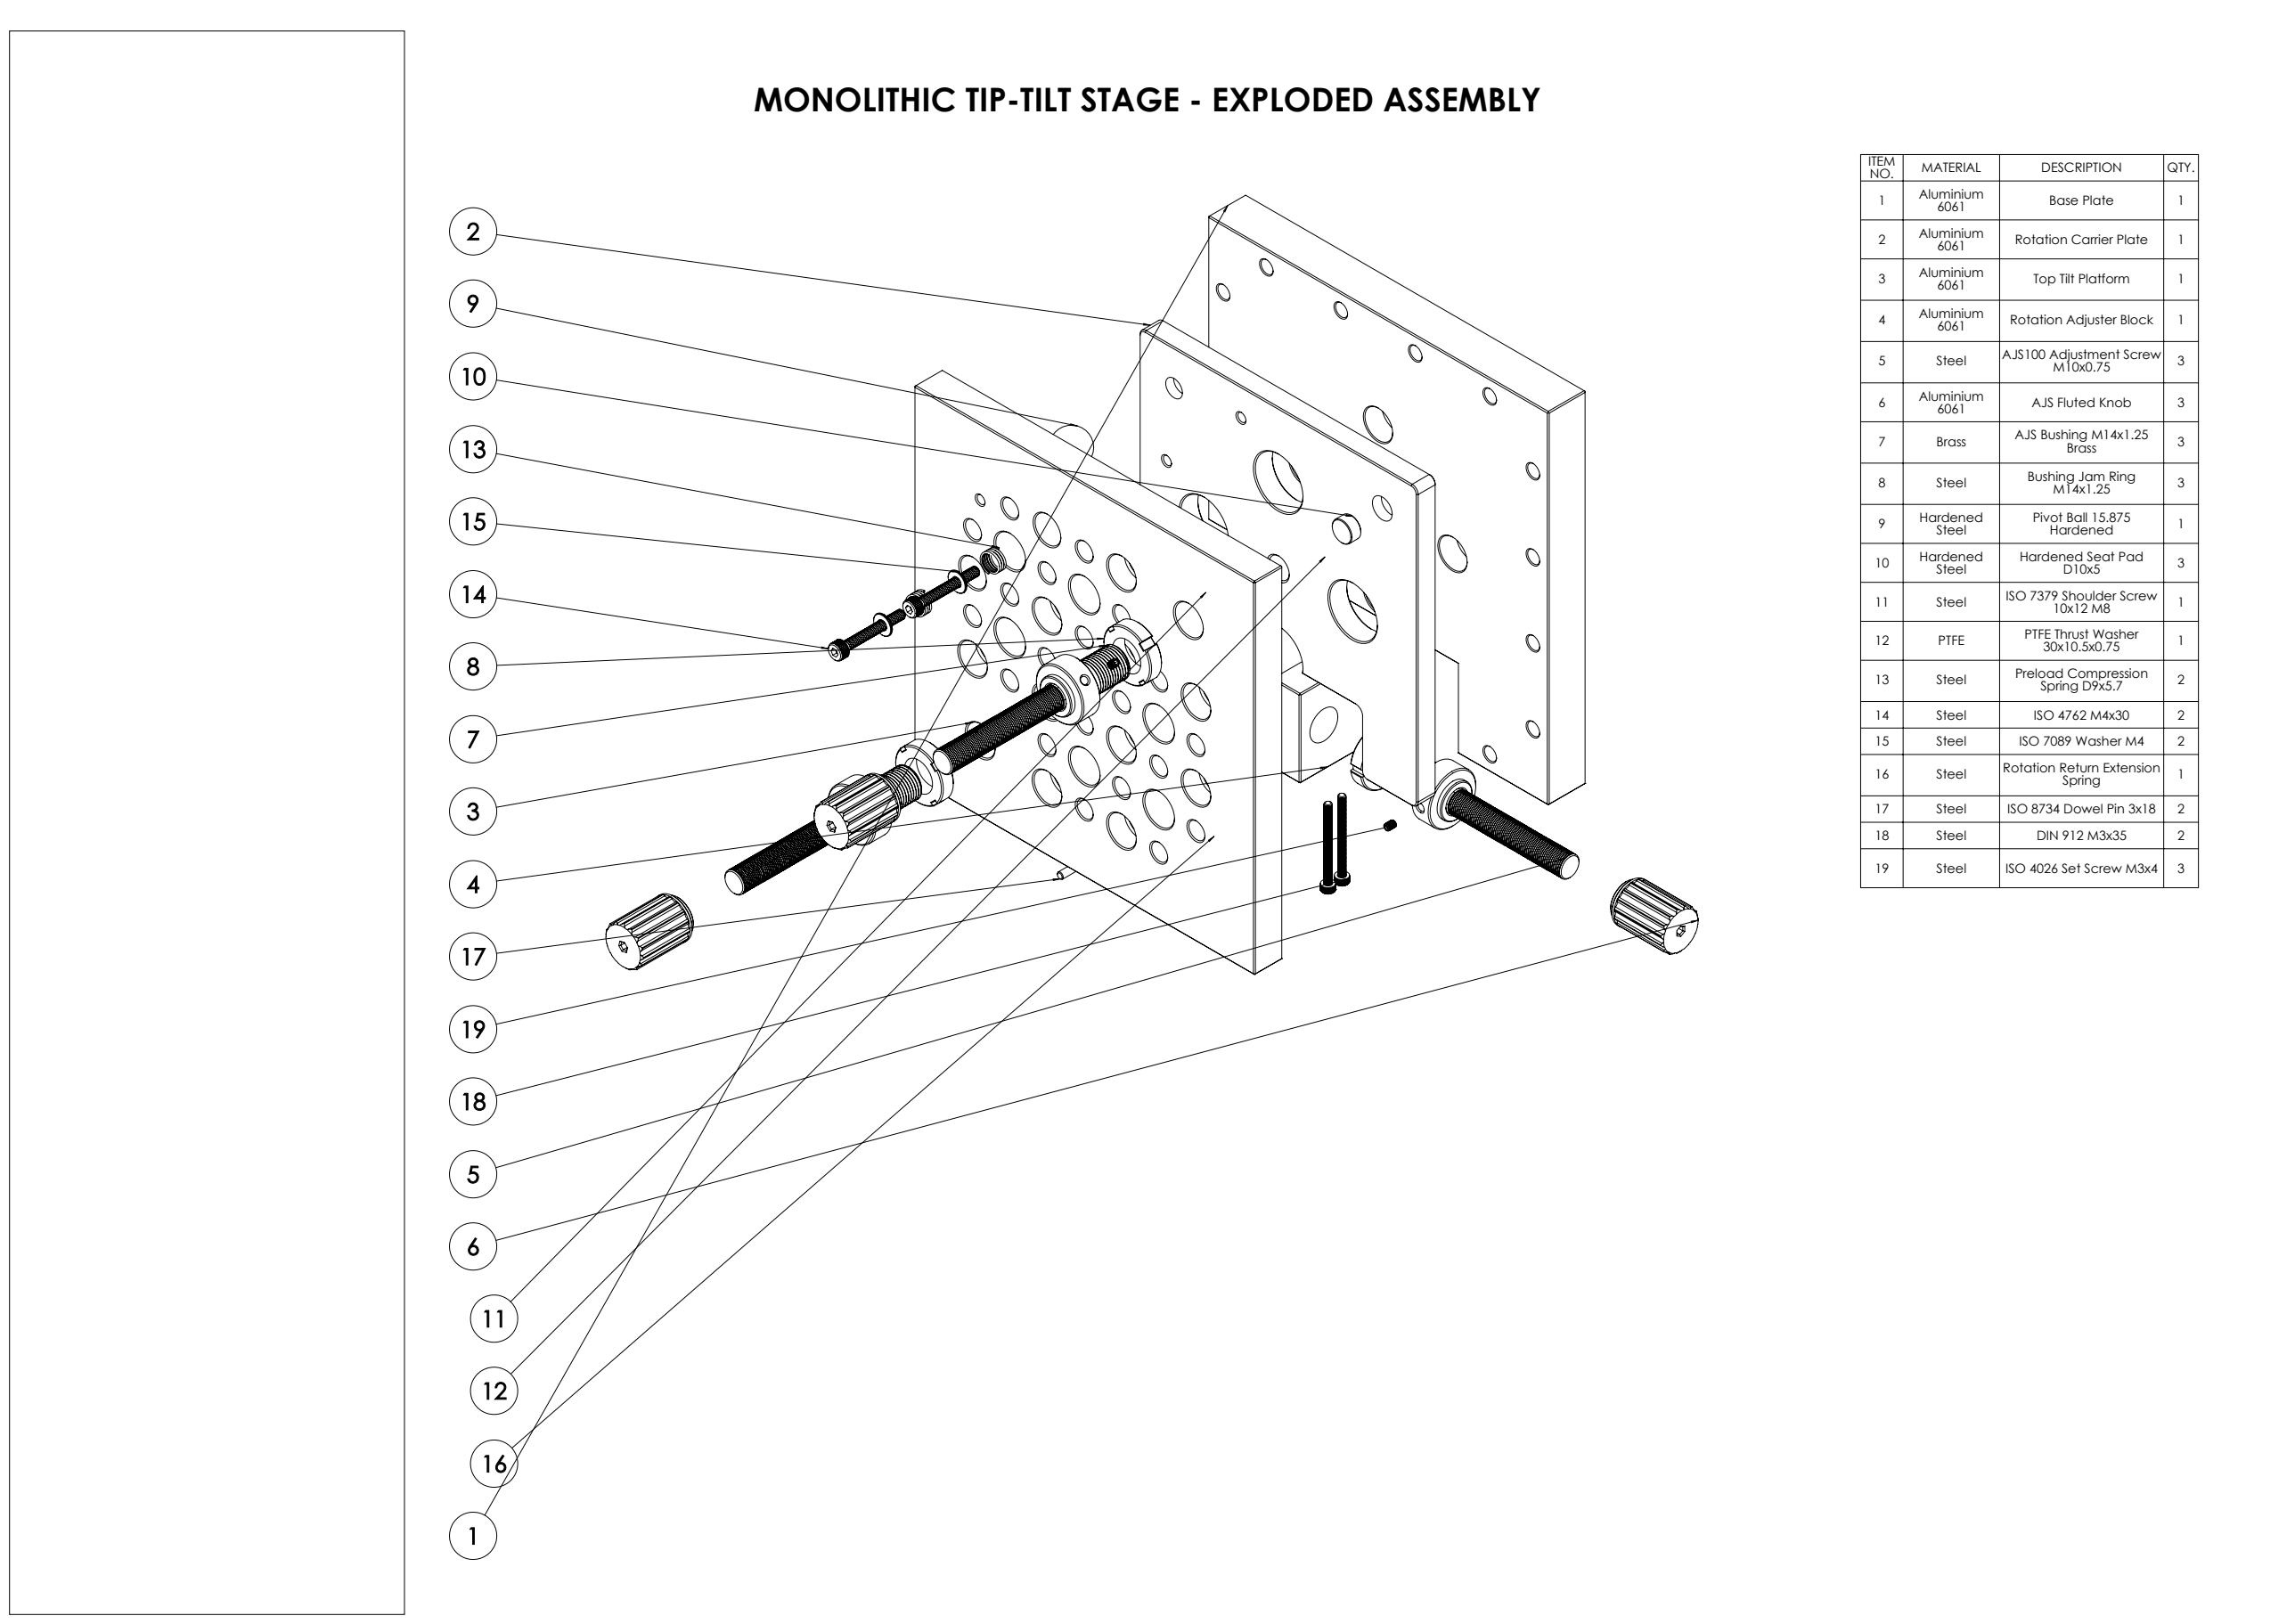
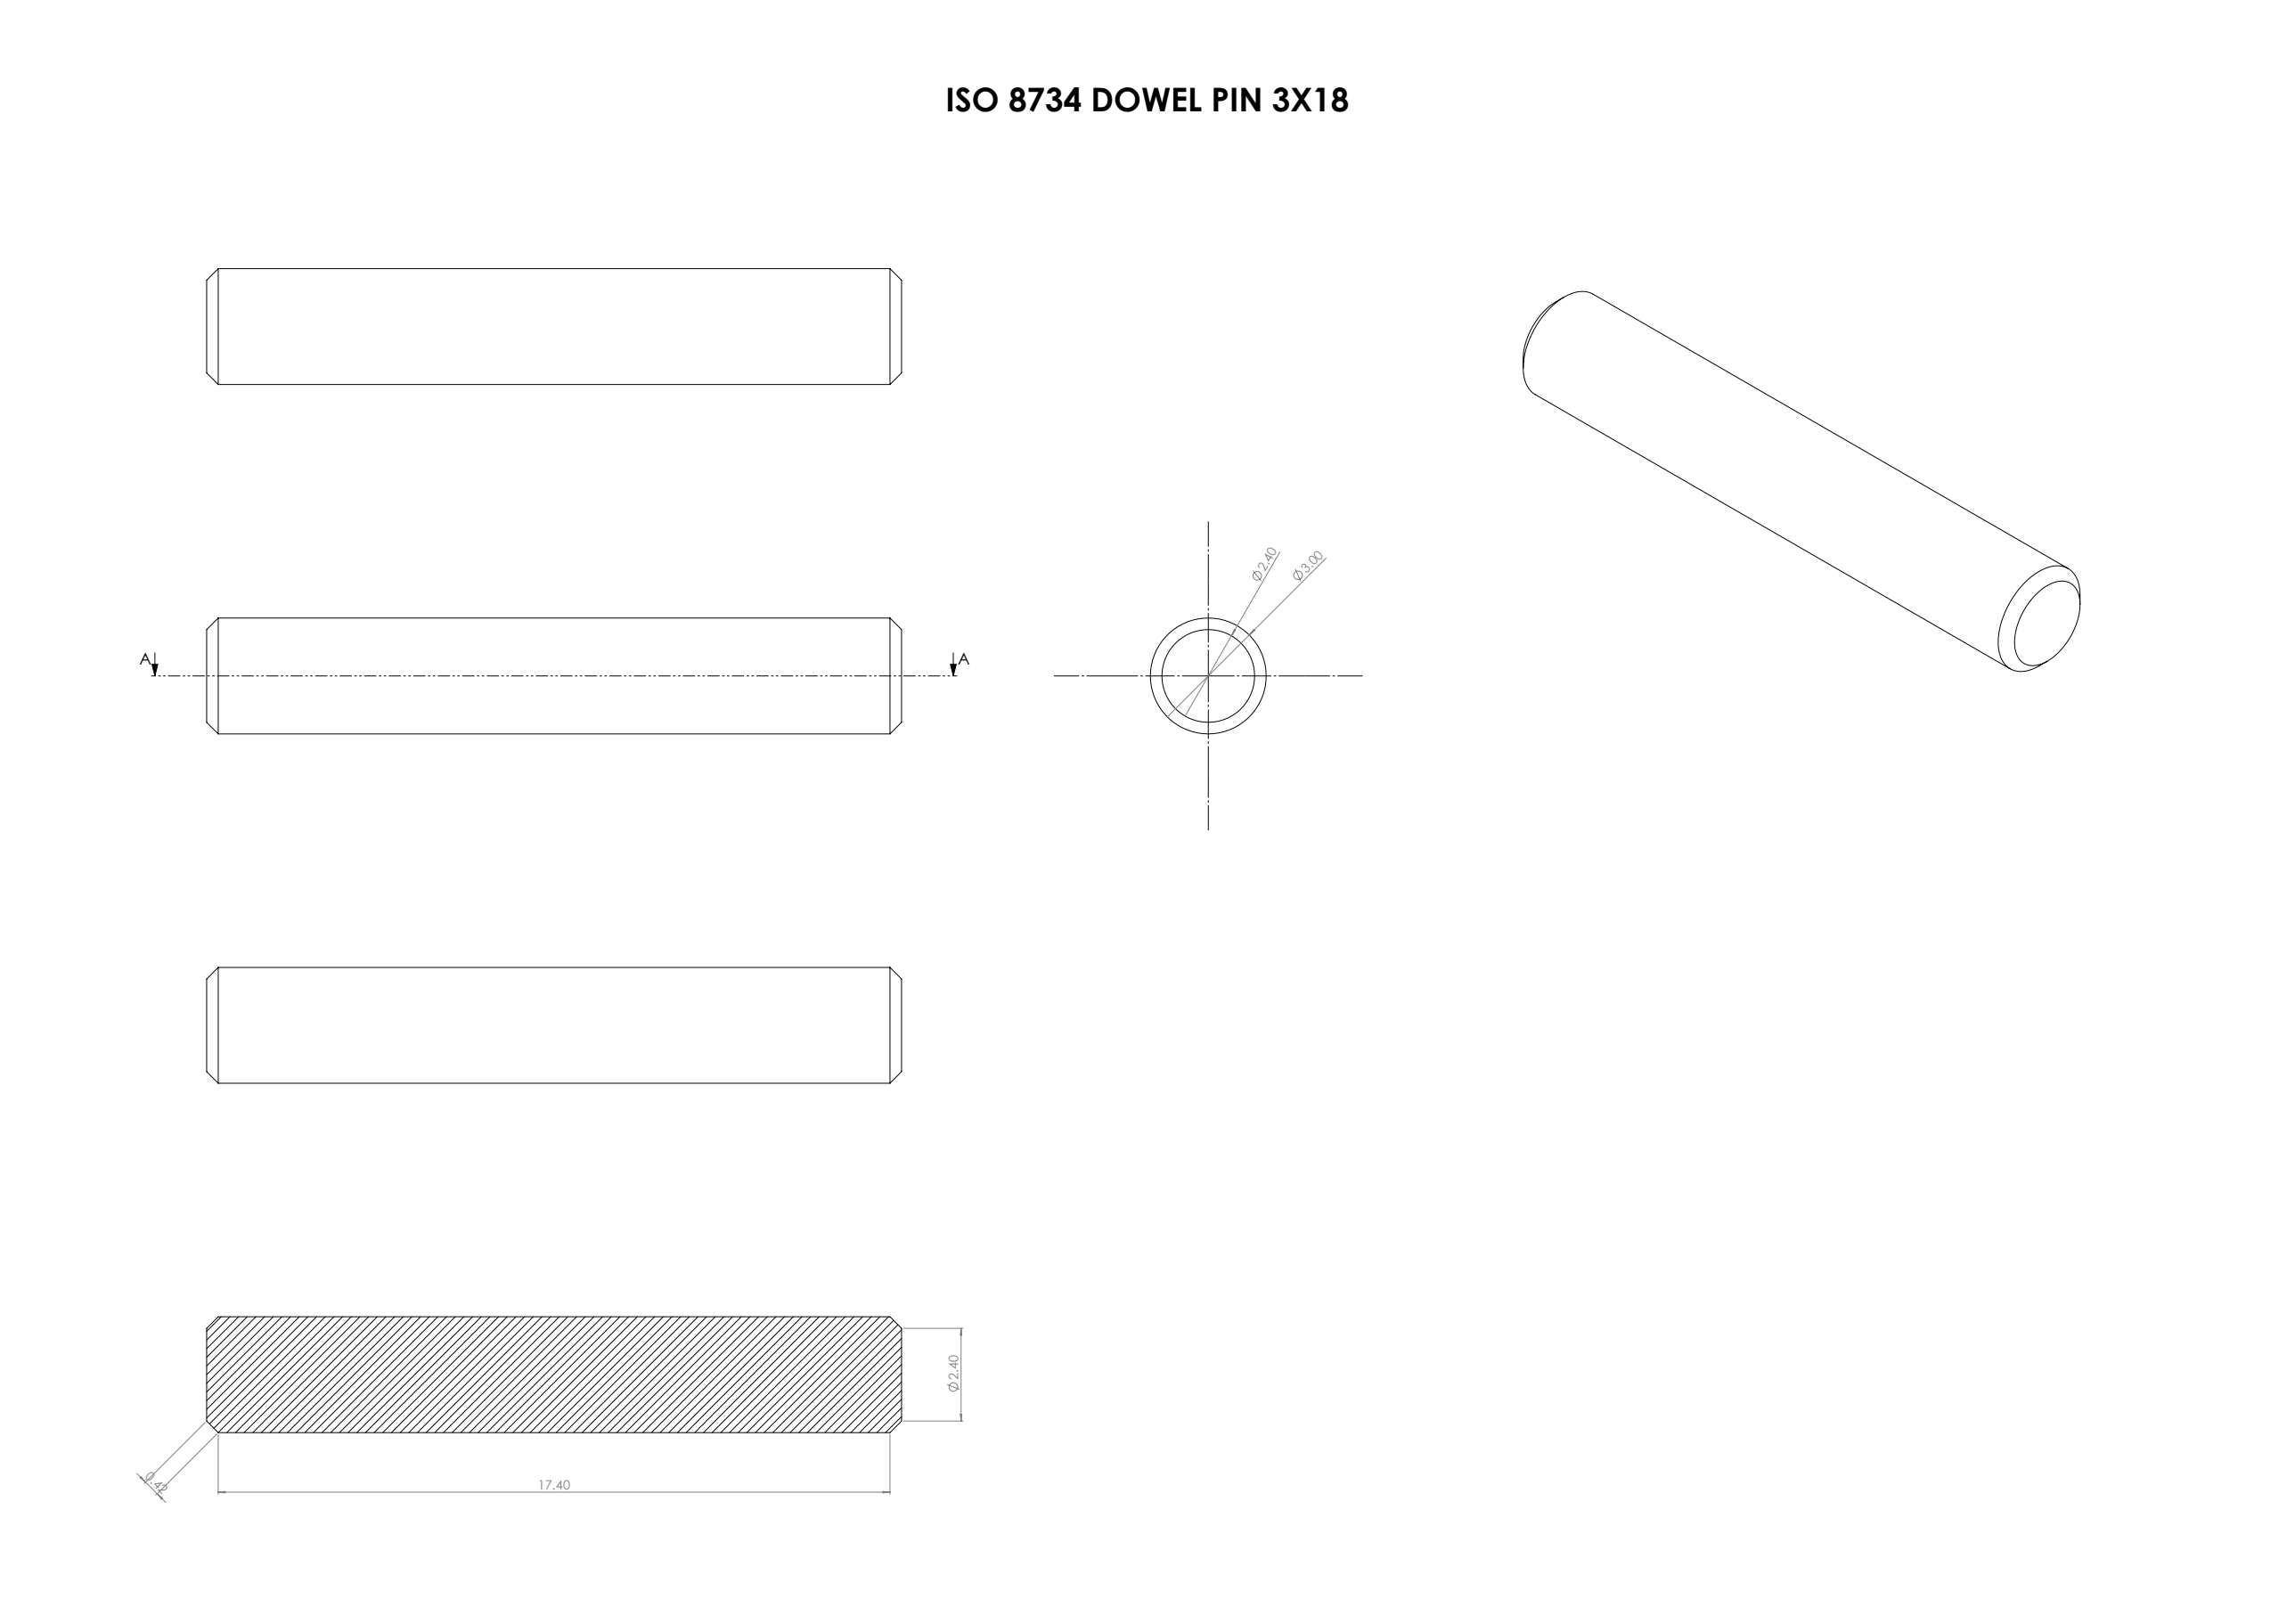
ISO-10303-21;
HEADER;
/* Generated by software containing ST-Developer
 * from STEP Tools, Inc. (www.steptools.com) 
 */

FILE_DESCRIPTION(
/* description */ (''),
/* implementation_level */ '2;1');

FILE_NAME(
/* name */ 'MAS-285',
/* time_stamp */ '2026-10-21T01:56:51-07:00',
/* author */ (''),
/* organization */ (''),
/* preprocessor_version */ 'ST-DEVELOPER v20.2',
/* originating_system */ 'Autodesk Translation Framework v15.15.0.0',
/* authorisation */ '');

FILE_SCHEMA (('AUTOMOTIVE_DESIGN { 1 0 10303 214 3 1 1 }'));
ENDSEC;

DATA;
#10=MECHANICAL_DESIGN_GEOMETRIC_PRESENTATION_REPRESENTATION('',(#270,#271,
#272,#273,#274,#275,#276,#277,#278,#279,#280,#281,#282,#283,#284,#285,#286,
#287,#288),#82384);
#11=ITEM_DEFINED_TRANSFORMATION($,$,#30891,#33377);
#12=ITEM_DEFINED_TRANSFORMATION($,$,#31122,#33378);
#13=ITEM_DEFINED_TRANSFORMATION($,$,#31321,#33379);
#14=ITEM_DEFINED_TRANSFORMATION($,$,#31710,#33380);
#15=ITEM_DEFINED_TRANSFORMATION($,$,#31766,#33381);
#16=ITEM_DEFINED_TRANSFORMATION($,$,#31784,#33382);
#17=ITEM_DEFINED_TRANSFORMATION($,$,#32066,#33383);
#18=ITEM_DEFINED_TRANSFORMATION($,$,#32075,#33384);
#19=ITEM_DEFINED_TRANSFORMATION($,$,#32078,#33385);
#20=ITEM_DEFINED_TRANSFORMATION($,$,#32078,#33386);
#21=ITEM_DEFINED_TRANSFORMATION($,$,#32078,#33387);
#22=ITEM_DEFINED_TRANSFORMATION($,$,#32088,#33388);
#23=ITEM_DEFINED_TRANSFORMATION($,$,#32093,#33389);
#24=ITEM_DEFINED_TRANSFORMATION($,$,#32107,#33390);
#25=ITEM_DEFINED_TRANSFORMATION($,$,#32088,#33391);
#26=ITEM_DEFINED_TRANSFORMATION($,$,#32093,#33392);
#27=ITEM_DEFINED_TRANSFORMATION($,$,#32107,#33393);
#28=ITEM_DEFINED_TRANSFORMATION($,$,#32444,#33394);
#29=ITEM_DEFINED_TRANSFORMATION($,$,#32444,#33395);
#30=ITEM_DEFINED_TRANSFORMATION($,$,#32454,#33396);
#31=ITEM_DEFINED_TRANSFORMATION($,$,#32454,#33397);
#32=ITEM_DEFINED_TRANSFORMATION($,$,#32845,#33398);
#33=ITEM_DEFINED_TRANSFORMATION($,$,#32907,#33399);
#34=ITEM_DEFINED_TRANSFORMATION($,$,#32982,#33400);
#35=ITEM_DEFINED_TRANSFORMATION($,$,#33154,#33401);
#36=ITEM_DEFINED_TRANSFORMATION($,$,#33338,#33402);
#37=ITEM_DEFINED_TRANSFORMATION($,$,#32845,#33403);
#38=ITEM_DEFINED_TRANSFORMATION($,$,#32907,#33404);
#39=ITEM_DEFINED_TRANSFORMATION($,$,#32982,#33405);
#40=ITEM_DEFINED_TRANSFORMATION($,$,#33154,#33406);
#41=ITEM_DEFINED_TRANSFORMATION($,$,#33338,#33407);
#42=ITEM_DEFINED_TRANSFORMATION($,$,#32845,#33408);
#43=ITEM_DEFINED_TRANSFORMATION($,$,#32907,#33409);
#44=ITEM_DEFINED_TRANSFORMATION($,$,#32982,#33410);
#45=ITEM_DEFINED_TRANSFORMATION($,$,#33154,#33411);
#46=ITEM_DEFINED_TRANSFORMATION($,$,#33338,#33412);
#47=(
REPRESENTATION_RELATIONSHIP($,$,#82466,#82465)
REPRESENTATION_RELATIONSHIP_WITH_TRANSFORMATION(#11)
SHAPE_REPRESENTATION_RELATIONSHIP()
);
#48=(
REPRESENTATION_RELATIONSHIP($,$,#82467,#82465)
REPRESENTATION_RELATIONSHIP_WITH_TRANSFORMATION(#12)
SHAPE_REPRESENTATION_RELATIONSHIP()
);
#49=(
REPRESENTATION_RELATIONSHIP($,$,#82468,#82465)
REPRESENTATION_RELATIONSHIP_WITH_TRANSFORMATION(#13)
SHAPE_REPRESENTATION_RELATIONSHIP()
);
#50=(
REPRESENTATION_RELATIONSHIP($,$,#82469,#82465)
REPRESENTATION_RELATIONSHIP_WITH_TRANSFORMATION(#14)
SHAPE_REPRESENTATION_RELATIONSHIP()
);
#51=(
REPRESENTATION_RELATIONSHIP($,$,#82470,#82465)
REPRESENTATION_RELATIONSHIP_WITH_TRANSFORMATION(#15)
SHAPE_REPRESENTATION_RELATIONSHIP()
);
#52=(
REPRESENTATION_RELATIONSHIP($,$,#82471,#82465)
REPRESENTATION_RELATIONSHIP_WITH_TRANSFORMATION(#16)
SHAPE_REPRESENTATION_RELATIONSHIP()
);
#53=(
REPRESENTATION_RELATIONSHIP($,$,#82472,#82465)
REPRESENTATION_RELATIONSHIP_WITH_TRANSFORMATION(#17)
SHAPE_REPRESENTATION_RELATIONSHIP()
);
#54=(
REPRESENTATION_RELATIONSHIP($,$,#82473,#82465)
REPRESENTATION_RELATIONSHIP_WITH_TRANSFORMATION(#18)
SHAPE_REPRESENTATION_RELATIONSHIP()
);
#55=(
REPRESENTATION_RELATIONSHIP($,$,#82474,#82465)
REPRESENTATION_RELATIONSHIP_WITH_TRANSFORMATION(#19)
SHAPE_REPRESENTATION_RELATIONSHIP()
);
#56=(
REPRESENTATION_RELATIONSHIP($,$,#82474,#82465)
REPRESENTATION_RELATIONSHIP_WITH_TRANSFORMATION(#20)
SHAPE_REPRESENTATION_RELATIONSHIP()
);
#57=(
REPRESENTATION_RELATIONSHIP($,$,#82474,#82465)
REPRESENTATION_RELATIONSHIP_WITH_TRANSFORMATION(#21)
SHAPE_REPRESENTATION_RELATIONSHIP()
);
#58=(
REPRESENTATION_RELATIONSHIP($,$,#82475,#82465)
REPRESENTATION_RELATIONSHIP_WITH_TRANSFORMATION(#22)
SHAPE_REPRESENTATION_RELATIONSHIP()
);
#59=(
REPRESENTATION_RELATIONSHIP($,$,#82476,#82465)
REPRESENTATION_RELATIONSHIP_WITH_TRANSFORMATION(#23)
SHAPE_REPRESENTATION_RELATIONSHIP()
);
#60=(
REPRESENTATION_RELATIONSHIP($,$,#82477,#82465)
REPRESENTATION_RELATIONSHIP_WITH_TRANSFORMATION(#24)
SHAPE_REPRESENTATION_RELATIONSHIP()
);
#61=(
REPRESENTATION_RELATIONSHIP($,$,#82475,#82465)
REPRESENTATION_RELATIONSHIP_WITH_TRANSFORMATION(#25)
SHAPE_REPRESENTATION_RELATIONSHIP()
);
#62=(
REPRESENTATION_RELATIONSHIP($,$,#82476,#82465)
REPRESENTATION_RELATIONSHIP_WITH_TRANSFORMATION(#26)
SHAPE_REPRESENTATION_RELATIONSHIP()
);
#63=(
REPRESENTATION_RELATIONSHIP($,$,#82477,#82465)
REPRESENTATION_RELATIONSHIP_WITH_TRANSFORMATION(#27)
SHAPE_REPRESENTATION_RELATIONSHIP()
);
#64=(
REPRESENTATION_RELATIONSHIP($,$,#82478,#82465)
REPRESENTATION_RELATIONSHIP_WITH_TRANSFORMATION(#28)
SHAPE_REPRESENTATION_RELATIONSHIP()
);
#65=(
REPRESENTATION_RELATIONSHIP($,$,#82478,#82465)
REPRESENTATION_RELATIONSHIP_WITH_TRANSFORMATION(#29)
SHAPE_REPRESENTATION_RELATIONSHIP()
);
#66=(
REPRESENTATION_RELATIONSHIP($,$,#82479,#82465)
REPRESENTATION_RELATIONSHIP_WITH_TRANSFORMATION(#30)
SHAPE_REPRESENTATION_RELATIONSHIP()
);
#67=(
REPRESENTATION_RELATIONSHIP($,$,#82479,#82465)
REPRESENTATION_RELATIONSHIP_WITH_TRANSFORMATION(#31)
SHAPE_REPRESENTATION_RELATIONSHIP()
);
#68=(
REPRESENTATION_RELATIONSHIP($,$,#82480,#82465)
REPRESENTATION_RELATIONSHIP_WITH_TRANSFORMATION(#32)
SHAPE_REPRESENTATION_RELATIONSHIP()
);
#69=(
REPRESENTATION_RELATIONSHIP($,$,#82481,#82465)
REPRESENTATION_RELATIONSHIP_WITH_TRANSFORMATION(#33)
SHAPE_REPRESENTATION_RELATIONSHIP()
);
#70=(
REPRESENTATION_RELATIONSHIP($,$,#82482,#82465)
REPRESENTATION_RELATIONSHIP_WITH_TRANSFORMATION(#34)
SHAPE_REPRESENTATION_RELATIONSHIP()
);
#71=(
REPRESENTATION_RELATIONSHIP($,$,#82483,#82465)
REPRESENTATION_RELATIONSHIP_WITH_TRANSFORMATION(#35)
SHAPE_REPRESENTATION_RELATIONSHIP()
);
#72=(
REPRESENTATION_RELATIONSHIP($,$,#82484,#82465)
REPRESENTATION_RELATIONSHIP_WITH_TRANSFORMATION(#36)
SHAPE_REPRESENTATION_RELATIONSHIP()
);
#73=(
REPRESENTATION_RELATIONSHIP($,$,#82480,#82465)
REPRESENTATION_RELATIONSHIP_WITH_TRANSFORMATION(#37)
SHAPE_REPRESENTATION_RELATIONSHIP()
);
#74=(
REPRESENTATION_RELATIONSHIP($,$,#82481,#82465)
REPRESENTATION_RELATIONSHIP_WITH_TRANSFORMATION(#38)
SHAPE_REPRESENTATION_RELATIONSHIP()
);
#75=(
REPRESENTATION_RELATIONSHIP($,$,#82482,#82465)
REPRESENTATION_RELATIONSHIP_WITH_TRANSFORMATION(#39)
SHAPE_REPRESENTATION_RELATIONSHIP()
);
#76=(
REPRESENTATION_RELATIONSHIP($,$,#82483,#82465)
REPRESENTATION_RELATIONSHIP_WITH_TRANSFORMATION(#40)
SHAPE_REPRESENTATION_RELATIONSHIP()
);
#77=(
REPRESENTATION_RELATIONSHIP($,$,#82484,#82465)
REPRESENTATION_RELATIONSHIP_WITH_TRANSFORMATION(#41)
SHAPE_REPRESENTATION_RELATIONSHIP()
);
#78=(
REPRESENTATION_RELATIONSHIP($,$,#82480,#82465)
REPRESENTATION_RELATIONSHIP_WITH_TRANSFORMATION(#42)
SHAPE_REPRESENTATION_RELATIONSHIP()
);
#79=(
REPRESENTATION_RELATIONSHIP($,$,#82481,#82465)
REPRESENTATION_RELATIONSHIP_WITH_TRANSFORMATION(#43)
SHAPE_REPRESENTATION_RELATIONSHIP()
);
#80=(
REPRESENTATION_RELATIONSHIP($,$,#82482,#82465)
REPRESENTATION_RELATIONSHIP_WITH_TRANSFORMATION(#44)
SHAPE_REPRESENTATION_RELATIONSHIP()
);
#81=(
REPRESENTATION_RELATIONSHIP($,$,#82483,#82465)
REPRESENTATION_RELATIONSHIP_WITH_TRANSFORMATION(#45)
SHAPE_REPRESENTATION_RELATIONSHIP()
);
#82=(
REPRESENTATION_RELATIONSHIP($,$,#82484,#82465)
REPRESENTATION_RELATIONSHIP_WITH_TRANSFORMATION(#46)
SHAPE_REPRESENTATION_RELATIONSHIP()
);
#83=CONTEXT_DEPENDENT_SHAPE_REPRESENTATION(#47,#82429);
#84=CONTEXT_DEPENDENT_SHAPE_REPRESENTATION(#48,#82430);
#85=CONTEXT_DEPENDENT_SHAPE_REPRESENTATION(#49,#82431);
#86=CONTEXT_DEPENDENT_SHAPE_REPRESENTATION(#50,#82432);
#87=CONTEXT_DEPENDENT_SHAPE_REPRESENTATION(#51,#82433);
#88=CONTEXT_DEPENDENT_SHAPE_REPRESENTATION(#52,#82434);
#89=CONTEXT_DEPENDENT_SHAPE_REPRESENTATION(#53,#82435);
#90=CONTEXT_DEPENDENT_SHAPE_REPRESENTATION(#54,#82436);
#91=CONTEXT_DEPENDENT_SHAPE_REPRESENTATION(#55,#82437);
#92=CONTEXT_DEPENDENT_SHAPE_REPRESENTATION(#56,#82438);
#93=CONTEXT_DEPENDENT_SHAPE_REPRESENTATION(#57,#82439);
#94=CONTEXT_DEPENDENT_SHAPE_REPRESENTATION(#58,#82440);
#95=CONTEXT_DEPENDENT_SHAPE_REPRESENTATION(#59,#82441);
#96=CONTEXT_DEPENDENT_SHAPE_REPRESENTATION(#60,#82442);
#97=CONTEXT_DEPENDENT_SHAPE_REPRESENTATION(#61,#82443);
#98=CONTEXT_DEPENDENT_SHAPE_REPRESENTATION(#62,#82444);
#99=CONTEXT_DEPENDENT_SHAPE_REPRESENTATION(#63,#82445);
#100=CONTEXT_DEPENDENT_SHAPE_REPRESENTATION(#64,#82446);
#101=CONTEXT_DEPENDENT_SHAPE_REPRESENTATION(#65,#82447);
#102=CONTEXT_DEPENDENT_SHAPE_REPRESENTATION(#66,#82448);
#103=CONTEXT_DEPENDENT_SHAPE_REPRESENTATION(#67,#82449);
#104=CONTEXT_DEPENDENT_SHAPE_REPRESENTATION(#68,#82450);
#105=CONTEXT_DEPENDENT_SHAPE_REPRESENTATION(#69,#82451);
#106=CONTEXT_DEPENDENT_SHAPE_REPRESENTATION(#70,#82452);
#107=CONTEXT_DEPENDENT_SHAPE_REPRESENTATION(#71,#82453);
#108=CONTEXT_DEPENDENT_SHAPE_REPRESENTATION(#72,#82454);
#109=CONTEXT_DEPENDENT_SHAPE_REPRESENTATION(#73,#82455);
#110=CONTEXT_DEPENDENT_SHAPE_REPRESENTATION(#74,#82456);
#111=CONTEXT_DEPENDENT_SHAPE_REPRESENTATION(#75,#82457);
#112=CONTEXT_DEPENDENT_SHAPE_REPRESENTATION(#76,#82458);
#113=CONTEXT_DEPENDENT_SHAPE_REPRESENTATION(#77,#82459);
#114=CONTEXT_DEPENDENT_SHAPE_REPRESENTATION(#78,#82460);
#115=CONTEXT_DEPENDENT_SHAPE_REPRESENTATION(#79,#82461);
#116=CONTEXT_DEPENDENT_SHAPE_REPRESENTATION(#80,#82462);
#117=CONTEXT_DEPENDENT_SHAPE_REPRESENTATION(#81,#82463);
#118=CONTEXT_DEPENDENT_SHAPE_REPRESENTATION(#82,#82464);
#119=NEXT_ASSEMBLY_USAGE_OCCURRENCE('01_Base_Plate:1','01_Base_Plate:1',
'01_Base_Plate:1',#82486,#82487,'01_Base_Plate:1');
#120=NEXT_ASSEMBLY_USAGE_OCCURRENCE('02_Rotation_Carrier_Plate:1',
'02_Rotation_Carrier_Plate:1','02_Rotation_Carrier_Plate:1',#82486,#82488,
'02_Rotation_Carrier_Plate:1');
#121=NEXT_ASSEMBLY_USAGE_OCCURRENCE('03_Top_Tilt_Platform:1',
'03_Top_Tilt_Platform:1','03_Top_Tilt_Platform:1',#82486,#82489,
'03_Top_Tilt_Platform:1');
#122=NEXT_ASSEMBLY_USAGE_OCCURRENCE('04_Rotation_Adjuster_Block:1',
'04_Rotation_Adjuster_Block:1','04_Rotation_Adjuster_Block:1',#82486,#82490,
'04_Rotation_Adjuster_Block:1');
#123=NEXT_ASSEMBLY_USAGE_OCCURRENCE(
'16_Rotation_Return_Extension_Spring:1',
'16_Rotation_Return_Extension_Spring:1',
'16_Rotation_Return_Extension_Spring:1',#82486,#82491,
'16_Rotation_Return_Extension_Spring:1');
#124=NEXT_ASSEMBLY_USAGE_OCCURRENCE(
'11_ISO_7379_Shoulder_Screw_10x12_M8:2',
'11_ISO_7379_Shoulder_Screw_10x12_M8:2',
'11_ISO_7379_Shoulder_Screw_10x12_M8:2',#82486,#82492,
'11_ISO_7379_Shoulder_Screw_10x12_M8:2');
#125=NEXT_ASSEMBLY_USAGE_OCCURRENCE(
'12_PTFE_Thrust_Washer_30x10.5x0.75:2',
'12_PTFE_Thrust_Washer_30x10.5x0.75:2',
'12_PTFE_Thrust_Washer_30x10.5x0.75:2',#82486,#82493,
'12_PTFE_Thrust_Washer_30x10.5x0.75:2');
#126=NEXT_ASSEMBLY_USAGE_OCCURRENCE('09_Pivot_Ball_15.875_Hardened:2',
'09_Pivot_Ball_15.875_Hardened:2','09_Pivot_Ball_15.875_Hardened:2',#82486,
#82494,'09_Pivot_Ball_15.875_Hardened:2');
#127=NEXT_ASSEMBLY_USAGE_OCCURRENCE('10_Hardened_Seat_Pad_D10x5:2',
'10_Hardened_Seat_Pad_D10x5:2','10_Hardened_Seat_Pad_D10x5:2',#82486,#82495,
'10_Hardened_Seat_Pad_D10x5:2');
#128=NEXT_ASSEMBLY_USAGE_OCCURRENCE('10_Hardened_Seat_Pad_D10x5:3',
'10_Hardened_Seat_Pad_D10x5:3','10_Hardened_Seat_Pad_D10x5:3',#82486,#82495,
'10_Hardened_Seat_Pad_D10x5:3');
#129=NEXT_ASSEMBLY_USAGE_OCCURRENCE('10_Hardened_Seat_Pad_D10x5:4',
'10_Hardened_Seat_Pad_D10x5:4','10_Hardened_Seat_Pad_D10x5:4',#82486,#82495,
'10_Hardened_Seat_Pad_D10x5:4');
#130=NEXT_ASSEMBLY_USAGE_OCCURRENCE(
'13_Preload_Compression_Spring_D9x5.7:2',
'13_Preload_Compression_Spring_D9x5.7:2',
'13_Preload_Compression_Spring_D9x5.7:2',#82486,#82496,
'13_Preload_Compression_Spring_D9x5.7:2');
#131=NEXT_ASSEMBLY_USAGE_OCCURRENCE('15_ISO_7089_Washer_M4:2',
'15_ISO_7089_Washer_M4:2','15_ISO_7089_Washer_M4:2',#82486,#82497,
'15_ISO_7089_Washer_M4:2');
#132=NEXT_ASSEMBLY_USAGE_OCCURRENCE('14_ISO_4762_M4x30:2',
'14_ISO_4762_M4x30:2','14_ISO_4762_M4x30:2',#82486,#82498,
'14_ISO_4762_M4x30:2');
#133=NEXT_ASSEMBLY_USAGE_OCCURRENCE(
'13_Preload_Compression_Spring_D9x5.7:3',
'13_Preload_Compression_Spring_D9x5.7:3',
'13_Preload_Compression_Spring_D9x5.7:3',#82486,#82496,
'13_Preload_Compression_Spring_D9x5.7:3');
#134=NEXT_ASSEMBLY_USAGE_OCCURRENCE('15_ISO_7089_Washer_M4:3',
'15_ISO_7089_Washer_M4:3','15_ISO_7089_Washer_M4:3',#82486,#82497,
'15_ISO_7089_Washer_M4:3');
#135=NEXT_ASSEMBLY_USAGE_OCCURRENCE('14_ISO_4762_M4x30:3',
'14_ISO_4762_M4x30:3','14_ISO_4762_M4x30:3',#82486,#82498,
'14_ISO_4762_M4x30:3');
#136=NEXT_ASSEMBLY_USAGE_OCCURRENCE('17_ISO_8734_Dowel_Pin_3x18:2',
'17_ISO_8734_Dowel_Pin_3x18:2','17_ISO_8734_Dowel_Pin_3x18:2',#82486,#82499,
'17_ISO_8734_Dowel_Pin_3x18:2');
#137=NEXT_ASSEMBLY_USAGE_OCCURRENCE('17_ISO_8734_Dowel_Pin_3x18:3',
'17_ISO_8734_Dowel_Pin_3x18:3','17_ISO_8734_Dowel_Pin_3x18:3',#82486,#82499,
'17_ISO_8734_Dowel_Pin_3x18:3');
#138=NEXT_ASSEMBLY_USAGE_OCCURRENCE('18_DIN_912_M3x35:2',
'18_DIN_912_M3x35:2','18_DIN_912_M3x35:2',#82486,#82500,
'18_DIN_912_M3x35:2');
#139=NEXT_ASSEMBLY_USAGE_OCCURRENCE('18_DIN_912_M3x35:3',
'18_DIN_912_M3x35:3','18_DIN_912_M3x35:3',#82486,#82500,
'18_DIN_912_M3x35:3');
#140=NEXT_ASSEMBLY_USAGE_OCCURRENCE('08_Bushing_Jam_Ring_M14x1.25:2',
'08_Bushing_Jam_Ring_M14x1.25:2','08_Bushing_Jam_Ring_M14x1.25:2',#82486,
#82501,'08_Bushing_Jam_Ring_M14x1.25:2');
#141=NEXT_ASSEMBLY_USAGE_OCCURRENCE('07_AJS_Bushing_M14x1.25_Brass:2',
'07_AJS_Bushing_M14x1.25_Brass:2','07_AJS_Bushing_M14x1.25_Brass:2',#82486,
#82502,'07_AJS_Bushing_M14x1.25_Brass:2');
#142=NEXT_ASSEMBLY_USAGE_OCCURRENCE(
'05_AJS100_Adjustment_Screw_M10x0.75:2',
'05_AJS100_Adjustment_Screw_M10x0.75:2',
'05_AJS100_Adjustment_Screw_M10x0.75:2',#82486,#82503,
'05_AJS100_Adjustment_Screw_M10x0.75:2');
#143=NEXT_ASSEMBLY_USAGE_OCCURRENCE('06_AJS_Fluted_Knob:2',
'06_AJS_Fluted_Knob:2','06_AJS_Fluted_Knob:2',#82486,#82504,
'06_AJS_Fluted_Knob:2');
#144=NEXT_ASSEMBLY_USAGE_OCCURRENCE('19_ISO_4026_Set_Screw_M3x4:2',
'19_ISO_4026_Set_Screw_M3x4:2','19_ISO_4026_Set_Screw_M3x4:2',#82486,#82505,
'19_ISO_4026_Set_Screw_M3x4:2');
#145=NEXT_ASSEMBLY_USAGE_OCCURRENCE('08_Bushing_Jam_Ring_M14x1.25:3',
'08_Bushing_Jam_Ring_M14x1.25:3','08_Bushing_Jam_Ring_M14x1.25:3',#82486,
#82501,'08_Bushing_Jam_Ring_M14x1.25:3');
#146=NEXT_ASSEMBLY_USAGE_OCCURRENCE('07_AJS_Bushing_M14x1.25_Brass:3',
'07_AJS_Bushing_M14x1.25_Brass:3','07_AJS_Bushing_M14x1.25_Brass:3',#82486,
#82502,'07_AJS_Bushing_M14x1.25_Brass:3');
#147=NEXT_ASSEMBLY_USAGE_OCCURRENCE(
'05_AJS100_Adjustment_Screw_M10x0.75:3',
'05_AJS100_Adjustment_Screw_M10x0.75:3',
'05_AJS100_Adjustment_Screw_M10x0.75:3',#82486,#82503,
'05_AJS100_Adjustment_Screw_M10x0.75:3');
#148=NEXT_ASSEMBLY_USAGE_OCCURRENCE('06_AJS_Fluted_Knob:3',
'06_AJS_Fluted_Knob:3','06_AJS_Fluted_Knob:3',#82486,#82504,
'06_AJS_Fluted_Knob:3');
#149=NEXT_ASSEMBLY_USAGE_OCCURRENCE('19_ISO_4026_Set_Screw_M3x4:3',
'19_ISO_4026_Set_Screw_M3x4:3','19_ISO_4026_Set_Screw_M3x4:3',#82486,#82505,
'19_ISO_4026_Set_Screw_M3x4:3');
#150=NEXT_ASSEMBLY_USAGE_OCCURRENCE('08_Bushing_Jam_Ring_M14x1.25:4',
'08_Bushing_Jam_Ring_M14x1.25:4','08_Bushing_Jam_Ring_M14x1.25:4',#82486,
#82501,'08_Bushing_Jam_Ring_M14x1.25:4');
#151=NEXT_ASSEMBLY_USAGE_OCCURRENCE('07_AJS_Bushing_M14x1.25_Brass:4',
'07_AJS_Bushing_M14x1.25_Brass:4','07_AJS_Bushing_M14x1.25_Brass:4',#82486,
#82502,'07_AJS_Bushing_M14x1.25_Brass:4');
#152=NEXT_ASSEMBLY_USAGE_OCCURRENCE(
'05_AJS100_Adjustment_Screw_M10x0.75:4',
'05_AJS100_Adjustment_Screw_M10x0.75:4',
'05_AJS100_Adjustment_Screw_M10x0.75:4',#82486,#82503,
'05_AJS100_Adjustment_Screw_M10x0.75:4');
#153=NEXT_ASSEMBLY_USAGE_OCCURRENCE('06_AJS_Fluted_Knob:4',
'06_AJS_Fluted_Knob:4','06_AJS_Fluted_Knob:4',#82486,#82504,
'06_AJS_Fluted_Knob:4');
#154=NEXT_ASSEMBLY_USAGE_OCCURRENCE('19_ISO_4026_Set_Screw_M3x4:4',
'19_ISO_4026_Set_Screw_M3x4:4','19_ISO_4026_Set_Screw_M3x4:4',#82486,#82505,
'19_ISO_4026_Set_Screw_M3x4:4');
#155=SPHERICAL_SURFACE('',#32076,7.9375);
#156=SPHERICAL_SURFACE('',#33152,3.00000000000001);
#157=TOROIDAL_SURFACE('',#31771,2.,0.4);
#158=TOROIDAL_SURFACE('',#31779,2.,0.4);
#159=TOROIDAL_SURFACE('',#32042,5.4,0.4);
#160=TOROIDAL_SURFACE('',#32201,2.154,0.2);
#161=TOROIDAL_SURFACE('',#32603,1.6635,0.2);
#162=(
BOUNDED_CURVE()
B_SPLINE_CURVE(2,(#43228,#43229,#43230),.UNSPECIFIED.,.F.,.F.)
B_SPLINE_CURVE_WITH_KNOTS((3,3),(0.0459620214738357,0.0928848613146929),
 .UNSPECIFIED.)
CURVE()
GEOMETRIC_REPRESENTATION_ITEM()
RATIONAL_B_SPLINE_CURVE((1.,1.,1.))
REPRESENTATION_ITEM('')
);
#163=(
BOUNDED_CURVE()
B_SPLINE_CURVE(2,(#43236,#43237,#43238),.UNSPECIFIED.,.F.,.F.)
B_SPLINE_CURVE_WITH_KNOTS((3,3),(0.,0.040804494448543),.UNSPECIFIED.)
CURVE()
GEOMETRIC_REPRESENTATION_ITEM()
RATIONAL_B_SPLINE_CURVE((1.,1.0001754834699,1.00017645997855))
REPRESENTATION_ITEM('')
);
#164=(
BOUNDED_CURVE()
B_SPLINE_CURVE(2,(#43242,#43243,#43244),.UNSPECIFIED.,.F.,.F.)
B_SPLINE_CURVE_WITH_KNOTS((3,3),(0.0412611632307347,0.0820656576920018),
 .UNSPECIFIED.)
CURVE()
GEOMETRIC_REPRESENTATION_ITEM()
RATIONAL_B_SPLINE_CURVE((1.00017645997855,1.00017548346996,1.))
REPRESENTATION_ITEM('')
);
#165=(
BOUNDED_CURVE()
B_SPLINE_CURVE(2,(#43257,#43258,#43259),.UNSPECIFIED.,.F.,.F.)
B_SPLINE_CURVE_WITH_KNOTS((3,3),(2.77288184399903,2.88132188410877),
 .UNSPECIFIED.)
CURVE()
GEOMETRIC_REPRESENTATION_ITEM()
RATIONAL_B_SPLINE_CURVE((1.00662865875794,1.0034439439933,1.))
REPRESENTATION_ITEM('')
);
#166=(
BOUNDED_CURVE()
B_SPLINE_CURVE(2,(#43294,#43295,#43296),.UNSPECIFIED.,.F.,.F.)
B_SPLINE_CURVE_WITH_KNOTS((3,3),(0.0225541082777549,0.04593400953422),
 .UNSPECIFIED.)
CURVE()
GEOMETRIC_REPRESENTATION_ITEM()
RATIONAL_B_SPLINE_CURVE((1.01228995969815,1.01859260314039,1.02475566063204))
REPRESENTATION_ITEM('')
);
#167=(
BOUNDED_CURVE()
B_SPLINE_CURVE(2,(#43300,#43301,#43302),.UNSPECIFIED.,.F.,.F.)
B_SPLINE_CURVE_WITH_KNOTS((3,3),(0.,0.0469228395759985),.UNSPECIFIED.)
CURVE()
GEOMETRIC_REPRESENTATION_ITEM()
RATIONAL_B_SPLINE_CURVE((1.,1.,1.))
REPRESENTATION_ITEM('')
);
#168=(
BOUNDED_CURVE()
B_SPLINE_CURVE(2,(#43425,#43426,#43427),.UNSPECIFIED.,.F.,.F.)
B_SPLINE_CURVE_WITH_KNOTS((3,3),(0.188460067452875,0.376920134905751),
 .UNSPECIFIED.)
CURVE()
GEOMETRIC_REPRESENTATION_ITEM()
RATIONAL_B_SPLINE_CURVE((1.,1.04083299973288,1.))
REPRESENTATION_ITEM('')
);
#169=(
BOUNDED_CURVE()
B_SPLINE_CURVE(2,(#44591,#44592,#44593),.UNSPECIFIED.,.F.,.F.)
B_SPLINE_CURVE_WITH_KNOTS((3,3),(0.,0.380788655293197),.UNSPECIFIED.)
CURVE()
GEOMETRIC_REPRESENTATION_ITEM()
RATIONAL_B_SPLINE_CURVE((1.,1.,1.))
REPRESENTATION_ITEM('')
);
#170=(
BOUNDED_CURVE()
B_SPLINE_CURVE(2,(#65757,#65758,#65759),.UNSPECIFIED.,.F.,.F.)
B_SPLINE_CURVE_WITH_KNOTS((3,3),(0.0445378083500862,0.0835095062261198),
 .UNSPECIFIED.)
CURVE()
GEOMETRIC_REPRESENTATION_ITEM()
RATIONAL_B_SPLINE_CURVE((1.00020174547405,1.00018913890855,1.))
REPRESENTATION_ITEM('')
);
#171=(
BOUNDED_CURVE()
B_SPLINE_CURVE(2,(#65763,#65764,#65765),.UNSPECIFIED.,.F.,.F.)
B_SPLINE_CURVE_WITH_KNOTS((3,3),(0.,0.0389716978752448),.UNSPECIFIED.)
CURVE()
GEOMETRIC_REPRESENTATION_ITEM()
RATIONAL_B_SPLINE_CURVE((1.,1.0001891389102,1.00020174547581))
REPRESENTATION_ITEM('')
);
#172=(
BOUNDED_CURVE()
B_SPLINE_CURVE(2,(#65775,#65776,#65777),.UNSPECIFIED.,.F.,.F.)
B_SPLINE_CURVE_WITH_KNOTS((3,3),(0.033425828127436,0.0710030761269733),
 .UNSPECIFIED.)
CURVE()
GEOMETRIC_REPRESENTATION_ITEM()
RATIONAL_B_SPLINE_CURVE((1.0001146955549,1.00012181803223,1.))
REPRESENTATION_ITEM('')
);
#173=(
BOUNDED_CURVE()
B_SPLINE_CURVE(2,(#65781,#65782,#65783),.UNSPECIFIED.,.F.,.F.)
B_SPLINE_CURVE_WITH_KNOTS((3,3),(0.,0.0375772479994726),.UNSPECIFIED.)
CURVE()
GEOMETRIC_REPRESENTATION_ITEM()
RATIONAL_B_SPLINE_CURVE((1.,1.00012181795416,1.0001146954814))
REPRESENTATION_ITEM('')
);
#174=(
BOUNDED_CURVE()
B_SPLINE_CURVE(2,(#65784,#65785,#65786),.UNSPECIFIED.,.F.,.F.)
B_SPLINE_CURVE_WITH_KNOTS((3,3),(0.,0.0389716978752398),.UNSPECIFIED.)
CURVE()
GEOMETRIC_REPRESENTATION_ITEM()
RATIONAL_B_SPLINE_CURVE((1.,1.00018913890916,1.0002017454747))
REPRESENTATION_ITEM('')
);
#175=(
BOUNDED_CURVE()
B_SPLINE_CURVE(2,(#65790,#65791,#65792),.UNSPECIFIED.,.F.,.F.)
B_SPLINE_CURVE_WITH_KNOTS((3,3),(0.0445378083500902,0.0835095062261194),
 .UNSPECIFIED.)
CURVE()
GEOMETRIC_REPRESENTATION_ITEM()
RATIONAL_B_SPLINE_CURVE((1.00020174547445,1.00018913890892,1.))
REPRESENTATION_ITEM('')
);
#176=(
BOUNDED_CURVE()
B_SPLINE_CURVE(2,(#65796,#65797,#65798),.UNSPECIFIED.,.F.,.F.)
B_SPLINE_CURVE_WITH_KNOTS((3,3),(0.,0.0389716978752542),.UNSPECIFIED.)
CURVE()
GEOMETRIC_REPRESENTATION_ITEM()
RATIONAL_B_SPLINE_CURVE((1.,1.00018913890855,1.00020174547405))
REPRESENTATION_ITEM('')
);
#177=(
BOUNDED_CURVE()
B_SPLINE_CURVE(2,(#65802,#65803,#65804),.UNSPECIFIED.,.F.,.F.)
B_SPLINE_CURVE_WITH_KNOTS((3,3),(0.,0.0375772479995372),.UNSPECIFIED.)
CURVE()
GEOMETRIC_REPRESENTATION_ITEM()
RATIONAL_B_SPLINE_CURVE((1.,1.00012181803223,1.0001146955549))
REPRESENTATION_ITEM('')
);
#178=(
BOUNDED_CURVE()
B_SPLINE_CURVE(2,(#65810,#65811,#65812),.UNSPECIFIED.,.F.,.F.)
B_SPLINE_CURVE_WITH_KNOTS((3,3),(0.0334258281258571,0.0710030761269732),
 .UNSPECIFIED.)
CURVE()
GEOMETRIC_REPRESENTATION_ITEM()
RATIONAL_B_SPLINE_CURVE((1.00011469550903,1.00012181798351,1.))
REPRESENTATION_ITEM('')
);
#179=(
BOUNDED_CURVE()
B_SPLINE_CURVE(2,(#65817,#65818,#65819),.UNSPECIFIED.,.F.,.F.)
B_SPLINE_CURVE_WITH_KNOTS((3,3),(0.044537808350094,0.0835095062261198),
 .UNSPECIFIED.)
CURVE()
GEOMETRIC_REPRESENTATION_ITEM()
RATIONAL_B_SPLINE_CURVE((1.00020174547469,1.00018913890915,1.))
REPRESENTATION_ITEM('')
);
#180=(
BOUNDED_CURVE()
B_SPLINE_CURVE(2,(#65821,#65822,#65823),.UNSPECIFIED.,.F.,.F.)
B_SPLINE_CURVE_WITH_KNOTS((3,3),(0.0334258281275199,0.0710030761269733),
 .UNSPECIFIED.)
CURVE()
GEOMETRIC_REPRESENTATION_ITEM()
RATIONAL_B_SPLINE_CURVE((1.00011469547359,1.00012181794587,1.))
REPRESENTATION_ITEM('')
);
#181=(
BOUNDED_CURVE()
B_SPLINE_CURVE(2,(#65844,#65845,#65846),.UNSPECIFIED.,.F.,.F.)
B_SPLINE_CURVE_WITH_KNOTS((3,3),(0.,0.0389716978752325),.UNSPECIFIED.)
CURVE()
GEOMETRIC_REPRESENTATION_ITEM()
RATIONAL_B_SPLINE_CURVE((1.,1.00018913890989,1.00020174547548))
REPRESENTATION_ITEM('')
);
#182=(
BOUNDED_CURVE()
B_SPLINE_CURVE(2,(#65850,#65851,#65852),.UNSPECIFIED.,.F.,.F.)
B_SPLINE_CURVE_WITH_KNOTS((3,3),(0.,0.0375772480011104),.UNSPECIFIED.)
CURVE()
GEOMETRIC_REPRESENTATION_ITEM()
RATIONAL_B_SPLINE_CURVE((1.,1.00012181798092,1.00011469550659))
REPRESENTATION_ITEM('')
);
#183=(
BOUNDED_CURVE()
B_SPLINE_CURVE(2,(#65860,#65861,#65862),.UNSPECIFIED.,.F.,.F.)
B_SPLINE_CURVE_WITH_KNOTS((3,3),(0.0445378083500976,0.0835095062261196),
 .UNSPECIFIED.)
CURVE()
GEOMETRIC_REPRESENTATION_ITEM()
RATIONAL_B_SPLINE_CURVE((1.0002017454746,1.00018913890906,1.))
REPRESENTATION_ITEM('')
);
#184=(
BOUNDED_CURVE()
B_SPLINE_CURVE(2,(#65866,#65867,#65868),.UNSPECIFIED.,.F.,.F.)
B_SPLINE_CURVE_WITH_KNOTS((3,3),(0.,0.0389716978752574),.UNSPECIFIED.)
CURVE()
GEOMETRIC_REPRESENTATION_ITEM()
RATIONAL_B_SPLINE_CURVE((1.,1.00018913890786,1.00020174547332))
REPRESENTATION_ITEM('')
);
#185=(
BOUNDED_CURVE()
B_SPLINE_CURVE(2,(#65878,#65879,#65880),.UNSPECIFIED.,.F.,.F.)
B_SPLINE_CURVE_WITH_KNOTS((3,3),(0.0334258281258531,0.0710030761269732),
 .UNSPECIFIED.)
CURVE()
GEOMETRIC_REPRESENTATION_ITEM()
RATIONAL_B_SPLINE_CURVE((1.00011469551065,1.00012181798524,1.))
REPRESENTATION_ITEM('')
);
#186=(
BOUNDED_CURVE()
B_SPLINE_CURVE(2,(#65884,#65885,#65886),.UNSPECIFIED.,.F.,.F.)
B_SPLINE_CURVE_WITH_KNOTS((3,3),(0.,0.0375772480011044),.UNSPECIFIED.)
CURVE()
GEOMETRIC_REPRESENTATION_ITEM()
RATIONAL_B_SPLINE_CURVE((1.,1.00012181797833,1.00011469550415))
REPRESENTATION_ITEM('')
);
#187=(
BOUNDED_CURVE()
B_SPLINE_CURVE(2,(#65887,#65888,#65889),.UNSPECIFIED.,.F.,.F.)
B_SPLINE_CURVE_WITH_KNOTS((3,3),(0.,0.0389716978752387),.UNSPECIFIED.)
CURVE()
GEOMETRIC_REPRESENTATION_ITEM()
RATIONAL_B_SPLINE_CURVE((1.,1.00018913890938,1.00020174547494))
REPRESENTATION_ITEM('')
);
#188=(
BOUNDED_CURVE()
B_SPLINE_CURVE(2,(#65907,#65908,#65909),.UNSPECIFIED.,.F.,.F.)
B_SPLINE_CURVE_WITH_KNOTS((3,3),(0.0445378083500854,0.0835095062261198),
 .UNSPECIFIED.)
CURVE()
GEOMETRIC_REPRESENTATION_ITEM()
RATIONAL_B_SPLINE_CURVE((1.00020174547577,1.00018913891016,1.))
REPRESENTATION_ITEM('')
);
#189=(
BOUNDED_CURVE()
B_SPLINE_CURVE(2,(#65913,#65914,#65915),.UNSPECIFIED.,.F.,.F.)
B_SPLINE_CURVE_WITH_KNOTS((3,3),(0.0334258281275259,0.0710030761269733),
 .UNSPECIFIED.)
CURVE()
GEOMETRIC_REPRESENTATION_ITEM()
RATIONAL_B_SPLINE_CURVE((1.00011469547113,1.00012181794325,1.))
REPRESENTATION_ITEM('')
);
#190=(
BOUNDED_CURVE()
B_SPLINE_CURVE(2,(#65918,#65919,#65920),.UNSPECIFIED.,.F.,.F.)
B_SPLINE_CURVE_WITH_KNOTS((3,3),(0.,0.0375772479994632),.UNSPECIFIED.)
CURVE()
GEOMETRIC_REPRESENTATION_ITEM()
RATIONAL_B_SPLINE_CURVE((1.,1.00012181795023,1.0001146954777))
REPRESENTATION_ITEM('')
);
#191=(
BOUNDED_CURVE()
B_SPLINE_CURVE(2,(#65929,#65930,#65931),.UNSPECIFIED.,.F.,.F.)
B_SPLINE_CURVE_WITH_KNOTS((3,3),(0.044537808350101,0.0835095062261195),
 .UNSPECIFIED.)
CURVE()
GEOMETRIC_REPRESENTATION_ITEM()
RATIONAL_B_SPLINE_CURVE((1.00020174547522,1.00018913890965,1.))
REPRESENTATION_ITEM('')
);
#192=(
BOUNDED_CURVE()
B_SPLINE_CURVE(2,(#65935,#65936,#65937),.UNSPECIFIED.,.F.,.F.)
B_SPLINE_CURVE_WITH_KNOTS((3,3),(0.,0.0389716978752438),.UNSPECIFIED.)
CURVE()
GEOMETRIC_REPRESENTATION_ITEM()
RATIONAL_B_SPLINE_CURVE((1.,1.00018913890923,1.00020174547478))
REPRESENTATION_ITEM('')
);
#193=(
BOUNDED_CURVE()
B_SPLINE_CURVE(2,(#65947,#65948,#65949),.UNSPECIFIED.,.F.,.F.)
B_SPLINE_CURVE_WITH_KNOTS((3,3),(0.0334258281258831,0.0710030761269732),
 .UNSPECIFIED.)
CURVE()
GEOMETRIC_REPRESENTATION_ITEM()
RATIONAL_B_SPLINE_CURVE((1.00011469550092,1.0001218179749,1.))
REPRESENTATION_ITEM('')
);
#194=(
BOUNDED_CURVE()
B_SPLINE_CURVE(2,(#65953,#65954,#65955),.UNSPECIFIED.,.F.,.F.)
B_SPLINE_CURVE_WITH_KNOTS((3,3),(0.,0.0375772480008883),.UNSPECIFIED.)
CURVE()
GEOMETRIC_REPRESENTATION_ITEM()
RATIONAL_B_SPLINE_CURVE((1.,1.0001218179815,1.00011469550713))
REPRESENTATION_ITEM('')
);
#195=(
BOUNDED_CURVE()
B_SPLINE_CURVE(2,(#65956,#65957,#65958),.UNSPECIFIED.,.F.,.F.)
B_SPLINE_CURVE_WITH_KNOTS((3,3),(0.,0.0389716978752413),.UNSPECIFIED.)
CURVE()
GEOMETRIC_REPRESENTATION_ITEM()
RATIONAL_B_SPLINE_CURVE((1.,1.00018913890951,1.00020174547507))
REPRESENTATION_ITEM('')
);
#196=(
BOUNDED_CURVE()
B_SPLINE_CURVE(2,(#65994,#65995,#65996),.UNSPECIFIED.,.F.,.F.)
B_SPLINE_CURVE_WITH_KNOTS((3,3),(0.0445378083501022,0.0835095062261196),
 .UNSPECIFIED.)
CURVE()
GEOMETRIC_REPRESENTATION_ITEM()
RATIONAL_B_SPLINE_CURVE((1.00020174547498,1.00018913890943,1.))
REPRESENTATION_ITEM('')
);
#197=(
BOUNDED_CURVE()
B_SPLINE_CURVE(2,(#66000,#66001,#66002),.UNSPECIFIED.,.F.,.F.)
B_SPLINE_CURVE_WITH_KNOTS((3,3),(0.0334258281258389,0.0710030761269732),
 .UNSPECIFIED.)
CURVE()
GEOMETRIC_REPRESENTATION_ITEM()
RATIONAL_B_SPLINE_CURVE((1.00011469551635,1.00012181799128,1.))
REPRESENTATION_ITEM('')
);
#198=(
BOUNDED_CURVE()
B_SPLINE_CURVE(2,(#66005,#66006,#66007),.UNSPECIFIED.,.F.,.F.)
B_SPLINE_CURVE_WITH_KNOTS((3,3),(0.,0.0375772480011161),.UNSPECIFIED.)
CURVE()
GEOMETRIC_REPRESENTATION_ITEM()
RATIONAL_B_SPLINE_CURVE((1.,1.00012181798351,1.00011469550903))
REPRESENTATION_ITEM('')
);
#199=(
BOUNDED_CURVE()
B_SPLINE_CURVE(2,(#66013,#66014,#66015),.UNSPECIFIED.,.F.,.F.)
B_SPLINE_CURVE_WITH_KNOTS((3,3),(0.0445378083500857,0.0835095062261197),
 .UNSPECIFIED.)
CURVE()
GEOMETRIC_REPRESENTATION_ITEM()
RATIONAL_B_SPLINE_CURVE((1.00020174547356,1.0001891389081,1.))
REPRESENTATION_ITEM('')
);
#200=(
BOUNDED_CURVE()
B_SPLINE_CURVE(2,(#66019,#66020,#66021),.UNSPECIFIED.,.F.,.F.)
B_SPLINE_CURVE_WITH_KNOTS((3,3),(0.03342582812753,0.0710030761269734),
 .UNSPECIFIED.)
CURVE()
GEOMETRIC_REPRESENTATION_ITEM()
RATIONAL_B_SPLINE_CURVE((1.00011469546948,1.0001218179415,1.))
REPRESENTATION_ITEM('')
);
#201=(
BOUNDED_CURVE()
B_SPLINE_CURVE(2,(#66024,#66025,#66026),.UNSPECIFIED.,.F.,.F.)
B_SPLINE_CURVE_WITH_KNOTS((3,3),(0.,0.0375772479994669),.UNSPECIFIED.)
CURVE()
GEOMETRIC_REPRESENTATION_ITEM()
RATIONAL_B_SPLINE_CURVE((1.,1.00012181795155,1.00011469547894))
REPRESENTATION_ITEM('')
);
#202=(
BOUNDED_CURVE()
B_SPLINE_CURVE(2,(#80282,#80283,#80284),.UNSPECIFIED.,.F.,.F.)
B_SPLINE_CURVE_WITH_KNOTS((3,3),(0.095709435566232,0.188213402372322),
 .UNSPECIFIED.)
CURVE()
GEOMETRIC_REPRESENTATION_ITEM()
RATIONAL_B_SPLINE_CURVE((1.00220608042206,1.00217204690889,1.00001144171476))
REPRESENTATION_ITEM('')
);
#203=(
BOUNDED_CURVE()
B_SPLINE_CURVE(2,(#80312,#80313,#80314),.UNSPECIFIED.,.F.,.F.)
B_SPLINE_CURVE_WITH_KNOTS((3,3),(0.000244613971281809,0.0927485807773717),
 .UNSPECIFIED.)
CURVE()
GEOMETRIC_REPRESENTATION_ITEM()
RATIONAL_B_SPLINE_CURVE((1.00001144171476,1.00217204690889,1.00220608042206))
REPRESENTATION_ITEM('')
);
#204=(
BOUNDED_CURVE()
B_SPLINE_CURVE(2,(#80322,#80323,#80324),.UNSPECIFIED.,.F.,.F.)
B_SPLINE_CURVE_WITH_KNOTS((3,3),(0.0957094355662357,0.188213402372324),
 .UNSPECIFIED.)
CURVE()
GEOMETRIC_REPRESENTATION_ITEM()
RATIONAL_B_SPLINE_CURVE((1.00220608042216,1.00217204690899,1.00001144171476))
REPRESENTATION_ITEM('')
);
#205=(
BOUNDED_CURVE()
B_SPLINE_CURVE(2,(#80469,#80470,#80471),.UNSPECIFIED.,.F.,.F.)
B_SPLINE_CURVE_WITH_KNOTS((3,3),(0.000244613971281676,0.0927485807773712),
 .UNSPECIFIED.)
CURVE()
GEOMETRIC_REPRESENTATION_ITEM()
RATIONAL_B_SPLINE_CURVE((1.00001144171476,1.00217204690889,1.00220608042206))
REPRESENTATION_ITEM('')
);
#206=(
BOUNDED_CURVE()
B_SPLINE_CURVE(2,(#80475,#80476,#80477),.UNSPECIFIED.,.F.,.F.)
B_SPLINE_CURVE_WITH_KNOTS((3,3),(0.0957094355662342,0.188213402372322),
 .UNSPECIFIED.)
CURVE()
GEOMETRIC_REPRESENTATION_ITEM()
RATIONAL_B_SPLINE_CURVE((1.00220608042205,1.00217204690887,1.00001144171476))
REPRESENTATION_ITEM('')
);
#207=(
BOUNDED_CURVE()
B_SPLINE_CURVE(2,(#80504,#80505,#80506),.UNSPECIFIED.,.F.,.F.)
B_SPLINE_CURVE_WITH_KNOTS((3,3),(0.000244613971281263,0.0927485807773676),
 .UNSPECIFIED.)
CURVE()
GEOMETRIC_REPRESENTATION_ITEM()
RATIONAL_B_SPLINE_CURVE((1.00001144171476,1.00217204690908,1.00220608042225))
REPRESENTATION_ITEM('')
);
#208=(
BOUNDED_CURVE()
B_SPLINE_CURVE(2,(#80510,#80511,#80512),.UNSPECIFIED.,.F.,.F.)
B_SPLINE_CURVE_WITH_KNOTS((3,3),(0.0957094355662345,0.188213402372322),
 .UNSPECIFIED.)
CURVE()
GEOMETRIC_REPRESENTATION_ITEM()
RATIONAL_B_SPLINE_CURVE((1.00220608042216,1.00217204690899,1.00001144171476))
REPRESENTATION_ITEM('')
);
#209=(
BOUNDED_CURVE()
B_SPLINE_CURVE(2,(#80539,#80540,#80541),.UNSPECIFIED.,.F.,.F.)
B_SPLINE_CURVE_WITH_KNOTS((3,3),(0.000244613971281759,0.0927485807773703),
 .UNSPECIFIED.)
CURVE()
GEOMETRIC_REPRESENTATION_ITEM()
RATIONAL_B_SPLINE_CURVE((1.00001144171476,1.00217204690897,1.00220608042214))
REPRESENTATION_ITEM('')
);
#210=(
BOUNDED_CURVE()
B_SPLINE_CURVE(2,(#80545,#80546,#80547),.UNSPECIFIED.,.F.,.F.)
B_SPLINE_CURVE_WITH_KNOTS((3,3),(0.0957094355662337,0.188213402372321),
 .UNSPECIFIED.)
CURVE()
GEOMETRIC_REPRESENTATION_ITEM()
RATIONAL_B_SPLINE_CURVE((1.00220608042215,1.00217204690897,1.00001144171476))
REPRESENTATION_ITEM('')
);
#211=(
BOUNDED_CURVE()
B_SPLINE_CURVE(2,(#80574,#80575,#80576),.UNSPECIFIED.,.F.,.F.)
B_SPLINE_CURVE_WITH_KNOTS((3,3),(0.000244613971281829,0.0927485807773718),
 .UNSPECIFIED.)
CURVE()
GEOMETRIC_REPRESENTATION_ITEM()
RATIONAL_B_SPLINE_CURVE((1.00001144171476,1.00217204690888,1.00220608042205))
REPRESENTATION_ITEM('')
);
#212=(
BOUNDED_CURVE()
B_SPLINE_CURVE(2,(#80580,#80581,#80582),.UNSPECIFIED.,.F.,.F.)
B_SPLINE_CURVE_WITH_KNOTS((3,3),(0.0957094355662314,0.188213402372321),
 .UNSPECIFIED.)
CURVE()
GEOMETRIC_REPRESENTATION_ITEM()
RATIONAL_B_SPLINE_CURVE((1.00220608042206,1.00217204690889,1.00001144171476))
REPRESENTATION_ITEM('')
);
#213=(
BOUNDED_CURVE()
B_SPLINE_CURVE(2,(#80609,#80610,#80611),.UNSPECIFIED.,.F.,.F.)
B_SPLINE_CURVE_WITH_KNOTS((3,3),(0.000244613971281268,0.0927485807773693),
 .UNSPECIFIED.)
CURVE()
GEOMETRIC_REPRESENTATION_ITEM()
RATIONAL_B_SPLINE_CURVE((1.00001144171476,1.00217204690897,1.00220608042215))
REPRESENTATION_ITEM('')
);
#214=(
BOUNDED_CURVE()
B_SPLINE_CURVE(2,(#80615,#80616,#80617),.UNSPECIFIED.,.F.,.F.)
B_SPLINE_CURVE_WITH_KNOTS((3,3),(0.0957094355662326,0.188213402372321),
 .UNSPECIFIED.)
CURVE()
GEOMETRIC_REPRESENTATION_ITEM()
RATIONAL_B_SPLINE_CURVE((1.00220608042217,1.002172046909,1.00001144171476))
REPRESENTATION_ITEM('')
);
#215=(
BOUNDED_CURVE()
B_SPLINE_CURVE(2,(#80644,#80645,#80646),.UNSPECIFIED.,.F.,.F.)
B_SPLINE_CURVE_WITH_KNOTS((3,3),(0.000244613971283097,0.0927485807773713),
 .UNSPECIFIED.)
CURVE()
GEOMETRIC_REPRESENTATION_ITEM()
RATIONAL_B_SPLINE_CURVE((1.00001144171476,1.002172046909,1.00220608042218))
REPRESENTATION_ITEM('')
);
#216=(
BOUNDED_CURVE()
B_SPLINE_CURVE(2,(#80650,#80651,#80652),.UNSPECIFIED.,.F.,.F.)
B_SPLINE_CURVE_WITH_KNOTS((3,3),(0.0957094355662316,0.188213402372321),
 .UNSPECIFIED.)
CURVE()
GEOMETRIC_REPRESENTATION_ITEM()
RATIONAL_B_SPLINE_CURVE((1.00220608042227,1.00217204690909,1.00001144171476))
REPRESENTATION_ITEM('')
);
#217=(
BOUNDED_CURVE()
B_SPLINE_CURVE(2,(#80679,#80680,#80681),.UNSPECIFIED.,.F.,.F.)
B_SPLINE_CURVE_WITH_KNOTS((3,3),(0.000244613971281759,0.09274858077737),
 .UNSPECIFIED.)
CURVE()
GEOMETRIC_REPRESENTATION_ITEM()
RATIONAL_B_SPLINE_CURVE((1.00001144171476,1.00217204690888,1.00220608042205))
REPRESENTATION_ITEM('')
);
#218=(
BOUNDED_CURVE()
B_SPLINE_CURVE(2,(#80685,#80686,#80687),.UNSPECIFIED.,.F.,.F.)
B_SPLINE_CURVE_WITH_KNOTS((3,3),(0.0957094355662316,0.18821340237232),
 .UNSPECIFIED.)
CURVE()
GEOMETRIC_REPRESENTATION_ITEM()
RATIONAL_B_SPLINE_CURVE((1.00220608042213,1.00217204690896,1.00001144171476))
REPRESENTATION_ITEM('')
);
#219=(
BOUNDED_CURVE()
B_SPLINE_CURVE(2,(#80714,#80715,#80716),.UNSPECIFIED.,.F.,.F.)
B_SPLINE_CURVE_WITH_KNOTS((3,3),(0.000244613971281648,0.0927485807773707),
 .UNSPECIFIED.)
CURVE()
GEOMETRIC_REPRESENTATION_ITEM()
RATIONAL_B_SPLINE_CURVE((1.00001144171476,1.00217204690889,1.00220608042206))
REPRESENTATION_ITEM('')
);
#220=(
BOUNDED_CURVE()
B_SPLINE_CURVE(2,(#80720,#80721,#80722),.UNSPECIFIED.,.F.,.F.)
B_SPLINE_CURVE_WITH_KNOTS((3,3),(0.0957094355662329,0.188213402372321),
 .UNSPECIFIED.)
CURVE()
GEOMETRIC_REPRESENTATION_ITEM()
RATIONAL_B_SPLINE_CURVE((1.00220608042214,1.00217204690897,1.00001144171476))
REPRESENTATION_ITEM('')
);
#221=(
BOUNDED_CURVE()
B_SPLINE_CURVE(2,(#80749,#80750,#80751),.UNSPECIFIED.,.F.,.F.)
B_SPLINE_CURVE_WITH_KNOTS((3,3),(0.000244613971281549,0.0927485807773708),
 .UNSPECIFIED.)
CURVE()
GEOMETRIC_REPRESENTATION_ITEM()
RATIONAL_B_SPLINE_CURVE((1.00001144171476,1.002172046909,1.00220608042218))
REPRESENTATION_ITEM('')
);
#222=(
BOUNDED_CURVE()
B_SPLINE_CURVE(2,(#80755,#80756,#80757),.UNSPECIFIED.,.F.,.F.)
B_SPLINE_CURVE_WITH_KNOTS((3,3),(0.0957094355662331,0.188213402372322),
 .UNSPECIFIED.)
CURVE()
GEOMETRIC_REPRESENTATION_ITEM()
RATIONAL_B_SPLINE_CURVE((1.00220608042225,1.00217204690908,1.00001144171476))
REPRESENTATION_ITEM('')
);
#223=(
BOUNDED_CURVE()
B_SPLINE_CURVE(2,(#80784,#80785,#80786),.UNSPECIFIED.,.F.,.F.)
B_SPLINE_CURVE_WITH_KNOTS((3,3),(0.000244613971281458,0.0927485807773696),
 .UNSPECIFIED.)
CURVE()
GEOMETRIC_REPRESENTATION_ITEM()
RATIONAL_B_SPLINE_CURVE((1.00001144171476,1.00217204690908,1.00220608042225))
REPRESENTATION_ITEM('')
);
#224=(
BOUNDED_CURVE()
B_SPLINE_CURVE(2,(#80790,#80791,#80792),.UNSPECIFIED.,.F.,.F.)
B_SPLINE_CURVE_WITH_KNOTS((3,3),(0.0957094355662337,0.188213402372322),
 .UNSPECIFIED.)
CURVE()
GEOMETRIC_REPRESENTATION_ITEM()
RATIONAL_B_SPLINE_CURVE((1.00220608042226,1.00217204690909,1.00001144171476))
REPRESENTATION_ITEM('')
);
#225=(
BOUNDED_CURVE()
B_SPLINE_CURVE(2,(#80819,#80820,#80821),.UNSPECIFIED.,.F.,.F.)
B_SPLINE_CURVE_WITH_KNOTS((3,3),(0.000244613971281769,0.0927485807773717),
 .UNSPECIFIED.)
CURVE()
GEOMETRIC_REPRESENTATION_ITEM()
RATIONAL_B_SPLINE_CURVE((1.00001144171476,1.00217204690888,1.00220608042205))
REPRESENTATION_ITEM('')
);
#226=(
BOUNDED_CURVE()
B_SPLINE_CURVE(2,(#80825,#80826,#80827),.UNSPECIFIED.,.F.,.F.)
B_SPLINE_CURVE_WITH_KNOTS((3,3),(0.0957094355662335,0.188213402372321),
 .UNSPECIFIED.)
CURVE()
GEOMETRIC_REPRESENTATION_ITEM()
RATIONAL_B_SPLINE_CURVE((1.00220608042207,1.0021720469089,1.00001144171476))
REPRESENTATION_ITEM('')
);
#227=(
BOUNDED_CURVE()
B_SPLINE_CURVE(2,(#80854,#80855,#80856),.UNSPECIFIED.,.F.,.F.)
B_SPLINE_CURVE_WITH_KNOTS((3,3),(0.00024461397128167,0.0927485807773707),
 .UNSPECIFIED.)
CURVE()
GEOMETRIC_REPRESENTATION_ITEM()
RATIONAL_B_SPLINE_CURVE((1.00001144171476,1.00217204690889,1.00220608042207))
REPRESENTATION_ITEM('')
);
#228=(
BOUNDED_CURVE()
B_SPLINE_CURVE(2,(#80860,#80861,#80862),.UNSPECIFIED.,.F.,.F.)
B_SPLINE_CURVE_WITH_KNOTS((3,3),(0.0957094355662347,0.188213402372323),
 .UNSPECIFIED.)
CURVE()
GEOMETRIC_REPRESENTATION_ITEM()
RATIONAL_B_SPLINE_CURVE((1.00220608042226,1.00217204690908,1.00001144171476))
REPRESENTATION_ITEM('')
);
#229=(
BOUNDED_CURVE()
B_SPLINE_CURVE(2,(#80889,#80890,#80891),.UNSPECIFIED.,.F.,.F.)
B_SPLINE_CURVE_WITH_KNOTS((3,3),(0.000244613971281467,0.0927485807773707),
 .UNSPECIFIED.)
CURVE()
GEOMETRIC_REPRESENTATION_ITEM()
RATIONAL_B_SPLINE_CURVE((1.00001144171476,1.00217204690889,1.00220608042206))
REPRESENTATION_ITEM('')
);
#230=(
BOUNDED_CURVE()
B_SPLINE_CURVE(2,(#80895,#80896,#80897),.UNSPECIFIED.,.F.,.F.)
B_SPLINE_CURVE_WITH_KNOTS((3,3),(0.0957094355662333,0.188213402372321),
 .UNSPECIFIED.)
CURVE()
GEOMETRIC_REPRESENTATION_ITEM()
RATIONAL_B_SPLINE_CURVE((1.00220608042207,1.00217204690889,1.00001144171476))
REPRESENTATION_ITEM('')
);
#231=(
BOUNDED_CURVE()
B_SPLINE_CURVE(2,(#80924,#80925,#80926),.UNSPECIFIED.,.F.,.F.)
B_SPLINE_CURVE_WITH_KNOTS((3,3),(0.000244613971281619,0.0927485807773719),
 .UNSPECIFIED.)
CURVE()
GEOMETRIC_REPRESENTATION_ITEM()
RATIONAL_B_SPLINE_CURVE((1.00001144171476,1.00217204690898,1.00220608042215))
REPRESENTATION_ITEM('')
);
#232=SHAPE_REPRESENTATION_RELATIONSHIP('SRR','None',#82466,#251);
#233=SHAPE_REPRESENTATION_RELATIONSHIP('SRR','None',#82467,#252);
#234=SHAPE_REPRESENTATION_RELATIONSHIP('SRR','None',#82468,#253);
#235=SHAPE_REPRESENTATION_RELATIONSHIP('SRR','None',#82469,#254);
#236=SHAPE_REPRESENTATION_RELATIONSHIP('SRR','None',#82470,#255);
#237=SHAPE_REPRESENTATION_RELATIONSHIP('SRR','None',#82471,#256);
#238=SHAPE_REPRESENTATION_RELATIONSHIP('SRR','None',#82472,#257);
#239=SHAPE_REPRESENTATION_RELATIONSHIP('SRR','None',#82473,#258);
#240=SHAPE_REPRESENTATION_RELATIONSHIP('SRR','None',#82474,#259);
#241=SHAPE_REPRESENTATION_RELATIONSHIP('SRR','None',#82475,#260);
#242=SHAPE_REPRESENTATION_RELATIONSHIP('SRR','None',#82476,#261);
#243=SHAPE_REPRESENTATION_RELATIONSHIP('SRR','None',#82477,#262);
#244=SHAPE_REPRESENTATION_RELATIONSHIP('SRR','None',#82478,#263);
#245=SHAPE_REPRESENTATION_RELATIONSHIP('SRR','None',#82479,#264);
#246=SHAPE_REPRESENTATION_RELATIONSHIP('SRR','None',#82480,#265);
#247=SHAPE_REPRESENTATION_RELATIONSHIP('SRR','None',#82481,#266);
#248=SHAPE_REPRESENTATION_RELATIONSHIP('SRR','None',#82482,#267);
#249=SHAPE_REPRESENTATION_RELATIONSHIP('SRR','None',#82483,#268);
#250=SHAPE_REPRESENTATION_RELATIONSHIP('SRR','None',#82484,#269);
#251=ADVANCED_BREP_SHAPE_REPRESENTATION('',(#289),#82365);
#252=ADVANCED_BREP_SHAPE_REPRESENTATION('',(#290),#82366);
#253=ADVANCED_BREP_SHAPE_REPRESENTATION('',(#291),#82367);
#254=ADVANCED_BREP_SHAPE_REPRESENTATION('',(#292),#82368);
#255=ADVANCED_BREP_SHAPE_REPRESENTATION('',(#293),#82369);
#256=ADVANCED_BREP_SHAPE_REPRESENTATION('',(#294),#82370);
#257=ADVANCED_BREP_SHAPE_REPRESENTATION('',(#295),#82371);
#258=ADVANCED_BREP_SHAPE_REPRESENTATION('',(#296),#82372);
#259=ADVANCED_BREP_SHAPE_REPRESENTATION('',(#297),#82373);
#260=ADVANCED_BREP_SHAPE_REPRESENTATION('',(#298),#82374);
#261=ADVANCED_BREP_SHAPE_REPRESENTATION('',(#299),#82375);
#262=ADVANCED_BREP_SHAPE_REPRESENTATION('',(#300),#82376);
#263=ADVANCED_BREP_SHAPE_REPRESENTATION('',(#301),#82377);
#264=ADVANCED_BREP_SHAPE_REPRESENTATION('',(#302),#82378);
#265=ADVANCED_BREP_SHAPE_REPRESENTATION('',(#303),#82379);
#266=ADVANCED_BREP_SHAPE_REPRESENTATION('',(#304),#82380);
#267=ADVANCED_BREP_SHAPE_REPRESENTATION('',(#305),#82381);
#268=ADVANCED_BREP_SHAPE_REPRESENTATION('',(#306),#82382);
#269=ADVANCED_BREP_SHAPE_REPRESENTATION('',(#307),#82383);
#270=STYLED_ITEM('',(#82610),#289);
#271=STYLED_ITEM('',(#82617),#290);
#272=STYLED_ITEM('',(#82645),#291);
#273=STYLED_ITEM('',(#82610),#292);
#274=STYLED_ITEM('',(#82631),#293);
#275=STYLED_ITEM('',(#82638),#294);
#276=STYLED_ITEM('',(#82638),#295);
#277=STYLED_ITEM('',(#82624),#296);
#278=STYLED_ITEM('',(#82617),#297);
#279=STYLED_ITEM('',(#82631),#298);
#280=STYLED_ITEM('',(#82638),#299);
#281=STYLED_ITEM('',(#82638),#300);
#282=STYLED_ITEM('',(#82631),#301);
#283=STYLED_ITEM('',(#82638),#302);
#284=STYLED_ITEM('',(#82645),#303);
#285=STYLED_ITEM('',(#82645),#304);
#286=STYLED_ITEM('',(#82638),#305);
#287=STYLED_ITEM('',(#82624),#306);
#288=STYLED_ITEM('',(#82638),#307);
#289=MANIFOLD_SOLID_BREP('Body1',#30661);
#290=MANIFOLD_SOLID_BREP('Body1',#30662);
#291=MANIFOLD_SOLID_BREP('Body1',#30663);
#292=MANIFOLD_SOLID_BREP('Body1',#30664);
#293=MANIFOLD_SOLID_BREP('Body1',#30665);
#294=MANIFOLD_SOLID_BREP('Body1',#30666);
#295=MANIFOLD_SOLID_BREP('Body1',#30667);
#296=MANIFOLD_SOLID_BREP('Body1',#30668);
#297=MANIFOLD_SOLID_BREP('Body1',#30669);
#298=MANIFOLD_SOLID_BREP('Body1',#30670);
#299=MANIFOLD_SOLID_BREP('Body1',#30671);
#300=MANIFOLD_SOLID_BREP('Body1',#30672);
#301=MANIFOLD_SOLID_BREP('Body1',#30673);
#302=MANIFOLD_SOLID_BREP('Body1',#30674);
#303=MANIFOLD_SOLID_BREP('Body1',#30675);
#304=MANIFOLD_SOLID_BREP('Body1',#30676);
#305=MANIFOLD_SOLID_BREP('Body1',#30677);
#306=MANIFOLD_SOLID_BREP('Body1',#30678);
#307=MANIFOLD_SOLID_BREP('Body1',#30679);
#308=B_SPLINE_SURFACE_WITH_KNOTS('',2,1,((#41609,#41610),(#41611,#41612),
(#41613,#41614)),.UNSPECIFIED.,.F.,.F.,.F.,(3,3),(2,2),(0.,1.),(0.,0.0299999999999994),
 .UNSPECIFIED.);
#309=B_SPLINE_SURFACE_WITH_KNOTS('',2,1,((#41620,#41621),(#41622,#41623),
(#41624,#41625)),.UNSPECIFIED.,.F.,.F.,.F.,(3,3),(2,2),(0.,1.),(0.,0.0299999999999994),
 .UNSPECIFIED.);
#310=B_SPLINE_SURFACE_WITH_KNOTS('',2,1,((#41631,#41632),(#41633,#41634),
(#41635,#41636)),.UNSPECIFIED.,.F.,.F.,.F.,(3,3),(2,2),(0.,1.),(0.,0.0299999999999994),
 .UNSPECIFIED.);
#311=B_SPLINE_SURFACE_WITH_KNOTS('',2,1,((#41642,#41643),(#41644,#41645),
(#41646,#41647)),.UNSPECIFIED.,.F.,.F.,.F.,(3,3),(2,2),(0.,1.),(0.,0.0299999999999994),
 .UNSPECIFIED.);
#312=B_SPLINE_SURFACE_WITH_KNOTS('',2,1,((#41665,#41666),(#41667,#41668),
(#41669,#41670)),.UNSPECIFIED.,.F.,.F.,.F.,(3,3),(2,2),(0.,1.),(0.,0.0299999999999994),
 .UNSPECIFIED.);
#313=B_SPLINE_SURFACE_WITH_KNOTS('',2,1,((#41676,#41677),(#41678,#41679),
(#41680,#41681)),.UNSPECIFIED.,.F.,.F.,.F.,(3,3),(2,2),(0.,1.),(0.,0.0299999999999994),
 .UNSPECIFIED.);
#314=B_SPLINE_SURFACE_WITH_KNOTS('',2,1,((#41687,#41688),(#41689,#41690),
(#41691,#41692)),.UNSPECIFIED.,.F.,.F.,.F.,(3,3),(2,2),(0.,1.),(0.,0.0299999999999994),
 .UNSPECIFIED.);
#315=B_SPLINE_SURFACE_WITH_KNOTS('',2,1,((#41698,#41699),(#41700,#41701),
(#41702,#41703)),.UNSPECIFIED.,.F.,.F.,.F.,(3,3),(2,2),(0.,1.),(0.,0.0299999999999994),
 .UNSPECIFIED.);
#316=B_SPLINE_SURFACE_WITH_KNOTS('',2,1,((#41709,#41710),(#41711,#41712),
(#41713,#41714)),.UNSPECIFIED.,.F.,.F.,.F.,(3,3),(2,2),(0.,1.),(0.,0.0299999999999994),
 .UNSPECIFIED.);
#317=B_SPLINE_SURFACE_WITH_KNOTS('',2,1,((#41720,#41721),(#41722,#41723),
(#41724,#41725)),.UNSPECIFIED.,.F.,.F.,.F.,(3,3),(2,2),(0.,1.),(0.,0.0299999999999994),
 .UNSPECIFIED.);
#318=B_SPLINE_SURFACE_WITH_KNOTS('',2,1,((#41731,#41732),(#41733,#41734),
(#41735,#41736)),.UNSPECIFIED.,.F.,.F.,.F.,(3,3),(2,2),(0.,1.),(0.,0.0299999999999994),
 .UNSPECIFIED.);
#319=B_SPLINE_SURFACE_WITH_KNOTS('',2,1,((#41806,#41807),(#41808,#41809),
(#41810,#41811)),.UNSPECIFIED.,.F.,.F.,.F.,(3,3),(2,2),(0.,1.),(0.,0.0299999999999994),
 .UNSPECIFIED.);
#320=B_SPLINE_SURFACE_WITH_KNOTS('',2,1,((#41819,#41820),(#41821,#41822),
(#41823,#41824)),.UNSPECIFIED.,.F.,.F.,.F.,(3,3),(2,2),(0.,1.),(0.,0.0299999999999994),
 .UNSPECIFIED.);
#321=B_SPLINE_SURFACE_WITH_KNOTS('',2,1,((#41834,#41835),(#41836,#41837),
(#41838,#41839)),.UNSPECIFIED.,.F.,.F.,.F.,(3,3),(2,2),(0.,1.),(0.,0.0299999999999994),
 .UNSPECIFIED.);
#322=B_SPLINE_SURFACE_WITH_KNOTS('',2,1,((#41845,#41846),(#41847,#41848),
(#41849,#41850)),.UNSPECIFIED.,.F.,.F.,.F.,(3,3),(2,2),(0.,1.),(0.,0.0299999999999994),
 .UNSPECIFIED.);
#323=B_SPLINE_SURFACE_WITH_KNOTS('',2,1,((#41856,#41857),(#41858,#41859),
(#41860,#41861)),.UNSPECIFIED.,.F.,.F.,.F.,(3,3),(2,2),(0.,1.),(0.,0.0299999999999994),
 .UNSPECIFIED.);
#324=B_SPLINE_SURFACE_WITH_KNOTS('',2,1,((#41883,#41884),(#41885,#41886),
(#41887,#41888)),.UNSPECIFIED.,.F.,.F.,.F.,(3,3),(2,2),(0.,1.),(0.,0.0299999999999994),
 .UNSPECIFIED.);
#325=B_SPLINE_SURFACE_WITH_KNOTS('',2,1,((#41893,#41894),(#41895,#41896),
(#41897,#41898)),.UNSPECIFIED.,.F.,.F.,.F.,(3,3),(2,2),(0.,1.),(0.,0.0299999999999994),
 .UNSPECIFIED.);
#326=B_SPLINE_SURFACE_WITH_KNOTS('',2,1,((#41906,#41907),(#41908,#41909),
(#41910,#41911)),.UNSPECIFIED.,.F.,.F.,.F.,(3,3),(2,2),(0.,1.),(0.,0.0299999999999994),
 .UNSPECIFIED.);
#327=B_SPLINE_SURFACE_WITH_KNOTS('',2,1,((#41917,#41918),(#41919,#41920),
(#41921,#41922)),.UNSPECIFIED.,.F.,.F.,.F.,(3,3),(2,2),(0.,1.),(0.,0.0299999999999994),
 .UNSPECIFIED.);
#328=B_SPLINE_SURFACE_WITH_KNOTS('',2,1,((#41928,#41929),(#41930,#41931),
(#41932,#41933)),.UNSPECIFIED.,.F.,.F.,.F.,(3,3),(2,2),(0.,1.),(0.,0.0299999999999994),
 .UNSPECIFIED.);
#329=B_SPLINE_SURFACE_WITH_KNOTS('',2,1,((#41939,#41940),(#41941,#41942),
(#41943,#41944)),.UNSPECIFIED.,.F.,.F.,.F.,(3,3),(2,2),(0.,1.),(0.,0.0299999999999994),
 .UNSPECIFIED.);
#330=B_SPLINE_SURFACE_WITH_KNOTS('',2,1,((#41950,#41951),(#41952,#41953),
(#41954,#41955)),.UNSPECIFIED.,.F.,.F.,.F.,(3,3),(2,2),(0.,1.),(0.,0.0299999999999994),
 .UNSPECIFIED.);
#331=B_SPLINE_SURFACE_WITH_KNOTS('',2,1,((#41961,#41962),(#41963,#41964),
(#41965,#41966)),.UNSPECIFIED.,.F.,.F.,.F.,(3,3),(2,2),(0.,1.),(0.,0.0299999999999994),
 .UNSPECIFIED.);
#332=B_SPLINE_SURFACE_WITH_KNOTS('',2,1,((#41972,#41973),(#41974,#41975),
(#41976,#41977)),.UNSPECIFIED.,.F.,.F.,.F.,(3,3),(2,2),(0.,1.),(0.,0.0299999999999994),
 .UNSPECIFIED.);
#333=B_SPLINE_SURFACE_WITH_KNOTS('',2,1,((#41983,#41984),(#41985,#41986),
(#41987,#41988)),.UNSPECIFIED.,.F.,.F.,.F.,(3,3),(2,2),(0.,1.),(0.,0.0299999999999994),
 .UNSPECIFIED.);
#334=B_SPLINE_SURFACE_WITH_KNOTS('',2,1,((#41994,#41995),(#41996,#41997),
(#41998,#41999)),.UNSPECIFIED.,.F.,.F.,.F.,(3,3),(2,2),(0.,1.),(0.,0.0299999999999994),
 .UNSPECIFIED.);
#335=B_SPLINE_SURFACE_WITH_KNOTS('',2,1,((#42005,#42006),(#42007,#42008),
(#42009,#42010)),.UNSPECIFIED.,.F.,.F.,.F.,(3,3),(2,2),(0.,1.),(0.,0.0299999999999994),
 .UNSPECIFIED.);
#336=B_SPLINE_SURFACE_WITH_KNOTS('',2,1,((#42016,#42017),(#42018,#42019),
(#42020,#42021)),.UNSPECIFIED.,.F.,.F.,.F.,(3,3),(2,2),(0.,1.),(0.,0.0299999999999994),
 .UNSPECIFIED.);
#337=B_SPLINE_SURFACE_WITH_KNOTS('',2,1,((#42027,#42028),(#42029,#42030),
(#42031,#42032)),.UNSPECIFIED.,.F.,.F.,.F.,(3,3),(2,2),(0.,1.),(0.,0.0299999999999994),
 .UNSPECIFIED.);
#338=B_SPLINE_SURFACE_WITH_KNOTS('',2,1,((#42042,#42043),(#42044,#42045),
(#42046,#42047)),.UNSPECIFIED.,.F.,.F.,.F.,(3,3),(2,2),(0.,1.),(0.,0.0299999999999994),
 .UNSPECIFIED.);
#339=B_SPLINE_SURFACE_WITH_KNOTS('',2,1,((#42053,#42054),(#42055,#42056),
(#42057,#42058)),.UNSPECIFIED.,.F.,.F.,.F.,(3,3),(2,2),(0.,1.),(0.,0.0299999999999994),
 .UNSPECIFIED.);
#340=B_SPLINE_SURFACE_WITH_KNOTS('',2,1,((#42064,#42065),(#42066,#42067),
(#42068,#42069)),.UNSPECIFIED.,.F.,.F.,.F.,(3,3),(2,2),(0.,1.),(0.,0.0299999999999994),
 .UNSPECIFIED.);
#341=B_SPLINE_SURFACE_WITH_KNOTS('',2,1,((#42075,#42076),(#42077,#42078),
(#42079,#42080)),.UNSPECIFIED.,.F.,.F.,.F.,(3,3),(2,2),(0.,1.),(0.,0.0299999999999994),
 .UNSPECIFIED.);
#342=B_SPLINE_SURFACE_WITH_KNOTS('',2,1,((#42086,#42087),(#42088,#42089),
(#42090,#42091)),.UNSPECIFIED.,.F.,.F.,.F.,(3,3),(2,2),(0.,1.),(0.,0.0299999999999994),
 .UNSPECIFIED.);
#343=B_SPLINE_SURFACE_WITH_KNOTS('',2,1,((#42097,#42098),(#42099,#42100),
(#42101,#42102)),.UNSPECIFIED.,.F.,.F.,.F.,(3,3),(2,2),(0.,1.),(0.,0.0299999999999994),
 .UNSPECIFIED.);
#344=B_SPLINE_SURFACE_WITH_KNOTS('',2,1,((#42108,#42109),(#42110,#42111),
(#42112,#42113)),.UNSPECIFIED.,.F.,.F.,.F.,(3,3),(2,2),(0.,1.),(0.,0.0299999999999994),
 .UNSPECIFIED.);
#345=B_SPLINE_SURFACE_WITH_KNOTS('',2,1,((#42119,#42120),(#42121,#42122),
(#42123,#42124)),.UNSPECIFIED.,.F.,.F.,.F.,(3,3),(2,2),(0.,1.),(0.,0.0299999999999994),
 .UNSPECIFIED.);
#346=B_SPLINE_SURFACE_WITH_KNOTS('',2,1,((#42130,#42131),(#42132,#42133),
(#42134,#42135)),.UNSPECIFIED.,.F.,.F.,.F.,(3,3),(2,2),(0.,1.),(0.,0.0299999999999994),
 .UNSPECIFIED.);
#347=B_SPLINE_SURFACE_WITH_KNOTS('',2,1,((#42141,#42142),(#42143,#42144),
(#42145,#42146)),.UNSPECIFIED.,.F.,.F.,.F.,(3,3),(2,2),(0.,1.),(0.,0.0299999999999994),
 .UNSPECIFIED.);
#348=B_SPLINE_SURFACE_WITH_KNOTS('',2,1,((#42152,#42153),(#42154,#42155),
(#42156,#42157)),.UNSPECIFIED.,.F.,.F.,.F.,(3,3),(2,2),(0.,1.),(0.,0.0299999999999994),
 .UNSPECIFIED.);
#349=B_SPLINE_SURFACE_WITH_KNOTS('',2,1,((#42163,#42164),(#42165,#42166),
(#42167,#42168)),.UNSPECIFIED.,.F.,.F.,.F.,(3,3),(2,2),(0.,1.),(0.,0.0299999999999994),
 .UNSPECIFIED.);
#350=B_SPLINE_SURFACE_WITH_KNOTS('',2,1,((#42174,#42175),(#42176,#42177),
(#42178,#42179)),.UNSPECIFIED.,.F.,.F.,.F.,(3,3),(2,2),(0.,1.),(0.,0.0299999999999994),
 .UNSPECIFIED.);
#351=B_SPLINE_SURFACE_WITH_KNOTS('',2,1,((#42185,#42186),(#42187,#42188),
(#42189,#42190)),.UNSPECIFIED.,.F.,.F.,.F.,(3,3),(2,2),(0.,1.),(0.,0.0299999999999994),
 .UNSPECIFIED.);
#352=B_SPLINE_SURFACE_WITH_KNOTS('',2,1,((#42196,#42197),(#42198,#42199),
(#42200,#42201)),.UNSPECIFIED.,.F.,.F.,.F.,(3,3),(2,2),(0.,1.),(0.,0.0299999999999994),
 .UNSPECIFIED.);
#353=B_SPLINE_SURFACE_WITH_KNOTS('',2,1,((#42207,#42208),(#42209,#42210),
(#42211,#42212)),.UNSPECIFIED.,.F.,.F.,.F.,(3,3),(2,2),(0.,1.),(0.,0.0299999999999994),
 .UNSPECIFIED.);
#354=B_SPLINE_SURFACE_WITH_KNOTS('',2,1,((#42218,#42219),(#42220,#42221),
(#42222,#42223)),.UNSPECIFIED.,.F.,.F.,.F.,(3,3),(2,2),(0.,1.),(0.,0.0299999999999994),
 .UNSPECIFIED.);
#355=B_SPLINE_SURFACE_WITH_KNOTS('',2,1,((#42229,#42230),(#42231,#42232),
(#42233,#42234)),.UNSPECIFIED.,.F.,.F.,.F.,(3,3),(2,2),(0.,1.),(0.,0.0299999999999994),
 .UNSPECIFIED.);
#356=B_SPLINE_SURFACE_WITH_KNOTS('',2,1,((#42244,#42245),(#42246,#42247),
(#42248,#42249)),.UNSPECIFIED.,.F.,.F.,.F.,(3,3),(2,2),(0.,1.),(0.,0.0299999999999994),
 .UNSPECIFIED.);
#357=B_SPLINE_SURFACE_WITH_KNOTS('',2,1,((#42255,#42256),(#42257,#42258),
(#42259,#42260)),.UNSPECIFIED.,.F.,.F.,.F.,(3,3),(2,2),(0.,1.),(0.,0.0299999999999994),
 .UNSPECIFIED.);
#358=B_SPLINE_SURFACE_WITH_KNOTS('',2,1,((#42265,#42266),(#42267,#42268),
(#42269,#42270)),.UNSPECIFIED.,.F.,.F.,.F.,(3,3),(2,2),(0.,1.),(0.,0.0299999999999994),
 .UNSPECIFIED.);
#359=B_SPLINE_SURFACE_WITH_KNOTS('',2,1,((#42278,#42279),(#42280,#42281),
(#42282,#42283)),.UNSPECIFIED.,.F.,.F.,.F.,(3,3),(2,2),(0.,1.),(0.,0.0299999999999994),
 .UNSPECIFIED.);
#360=B_SPLINE_SURFACE_WITH_KNOTS('',2,1,((#42289,#42290),(#42291,#42292),
(#42293,#42294)),.UNSPECIFIED.,.F.,.F.,.F.,(3,3),(2,2),(0.,1.),(0.,0.0299999999999994),
 .UNSPECIFIED.);
#361=B_SPLINE_SURFACE_WITH_KNOTS('',2,1,((#42300,#42301),(#42302,#42303),
(#42304,#42305)),.UNSPECIFIED.,.F.,.F.,.F.,(3,3),(2,2),(0.,1.),(0.,0.0299999999999994),
 .UNSPECIFIED.);
#362=B_SPLINE_SURFACE_WITH_KNOTS('',2,1,((#42311,#42312),(#42313,#42314),
(#42315,#42316)),.UNSPECIFIED.,.F.,.F.,.F.,(3,3),(2,2),(0.,1.),(0.,0.0299999999999994),
 .UNSPECIFIED.);
#363=B_SPLINE_SURFACE_WITH_KNOTS('',2,1,((#42322,#42323),(#42324,#42325),
(#42326,#42327)),.UNSPECIFIED.,.F.,.F.,.F.,(3,3),(2,2),(0.,1.),(0.,0.0299999999999994),
 .UNSPECIFIED.);
#364=B_SPLINE_SURFACE_WITH_KNOTS('',2,1,((#42333,#42334),(#42335,#42336),
(#42337,#42338)),.UNSPECIFIED.,.F.,.F.,.F.,(3,3),(2,2),(0.,1.),(0.,0.0299999999999994),
 .UNSPECIFIED.);
#365=B_SPLINE_SURFACE_WITH_KNOTS('',2,1,((#42344,#42345),(#42346,#42347),
(#42348,#42349)),.UNSPECIFIED.,.F.,.F.,.F.,(3,3),(2,2),(0.,1.),(0.,0.0299999999999994),
 .UNSPECIFIED.);
#366=B_SPLINE_SURFACE_WITH_KNOTS('',2,1,((#42355,#42356),(#42357,#42358),
(#42359,#42360)),.UNSPECIFIED.,.F.,.F.,.F.,(3,3),(2,2),(0.,1.),(0.,0.0299999999999994),
 .UNSPECIFIED.);
#367=B_SPLINE_SURFACE_WITH_KNOTS('',2,1,((#42366,#42367),(#42368,#42369),
(#42370,#42371)),.UNSPECIFIED.,.F.,.F.,.F.,(3,3),(2,2),(0.,1.),(0.,0.0299999999999994),
 .UNSPECIFIED.);
#368=B_SPLINE_SURFACE_WITH_KNOTS('',2,1,((#42377,#42378),(#42379,#42380),
(#42381,#42382)),.UNSPECIFIED.,.F.,.F.,.F.,(3,3),(2,2),(0.,1.),(0.,0.0299999999999994),
 .UNSPECIFIED.);
#369=B_SPLINE_SURFACE_WITH_KNOTS('',2,1,((#42392,#42393),(#42394,#42395),
(#42396,#42397)),.UNSPECIFIED.,.F.,.F.,.F.,(3,3),(2,2),(0.,1.),(0.,0.0299999999999994),
 .UNSPECIFIED.);
#370=B_SPLINE_SURFACE_WITH_KNOTS('',2,1,((#42403,#42404),(#42405,#42406),
(#42407,#42408)),.UNSPECIFIED.,.F.,.F.,.F.,(3,3),(2,2),(0.,1.),(0.,0.0299999999999994),
 .UNSPECIFIED.);
#371=B_SPLINE_SURFACE_WITH_KNOTS('',2,1,((#42414,#42415),(#42416,#42417),
(#42418,#42419)),.UNSPECIFIED.,.F.,.F.,.F.,(3,3),(2,2),(0.,1.),(0.,0.0299999999999994),
 .UNSPECIFIED.);
#372=B_SPLINE_SURFACE_WITH_KNOTS('',2,1,((#42425,#42426),(#42427,#42428),
(#42429,#42430)),.UNSPECIFIED.,.F.,.F.,.F.,(3,3),(2,2),(0.,1.),(0.,0.0299999999999994),
 .UNSPECIFIED.);
#373=B_SPLINE_SURFACE_WITH_KNOTS('',2,1,((#42436,#42437),(#42438,#42439),
(#42440,#42441)),.UNSPECIFIED.,.F.,.F.,.F.,(3,3),(2,2),(0.,1.),(0.,0.0299999999999994),
 .UNSPECIFIED.);
#374=B_SPLINE_SURFACE_WITH_KNOTS('',2,1,((#42447,#42448),(#42449,#42450),
(#42451,#42452)),.UNSPECIFIED.,.F.,.F.,.F.,(3,3),(2,2),(0.,1.),(0.,0.0299999999999994),
 .UNSPECIFIED.);
#375=B_SPLINE_SURFACE_WITH_KNOTS('',2,1,((#42458,#42459),(#42460,#42461),
(#42462,#42463)),.UNSPECIFIED.,.F.,.F.,.F.,(3,3),(2,2),(0.,1.),(0.,0.0299999999999994),
 .UNSPECIFIED.);
#376=B_SPLINE_SURFACE_WITH_KNOTS('',2,1,((#42473,#42474),(#42475,#42476),
(#42477,#42478)),.UNSPECIFIED.,.F.,.F.,.F.,(3,3),(2,2),(0.,1.),(0.,0.0299999999999994),
 .UNSPECIFIED.);
#377=B_SPLINE_SURFACE_WITH_KNOTS('',2,1,((#42484,#42485),(#42486,#42487),
(#42488,#42489)),.UNSPECIFIED.,.F.,.F.,.F.,(3,3),(2,2),(0.,1.),(0.,0.0299999999999994),
 .UNSPECIFIED.);
#378=B_SPLINE_SURFACE_WITH_KNOTS('',2,1,((#42495,#42496),(#42497,#42498),
(#42499,#42500)),.UNSPECIFIED.,.F.,.F.,.F.,(3,3),(2,2),(0.,1.),(0.,0.0299999999999994),
 .UNSPECIFIED.);
#379=B_SPLINE_SURFACE_WITH_KNOTS('',2,1,((#42506,#42507),(#42508,#42509),
(#42510,#42511)),.UNSPECIFIED.,.F.,.F.,.F.,(3,3),(2,2),(0.,1.),(0.,0.0299999999999994),
 .UNSPECIFIED.);
#380=B_SPLINE_SURFACE_WITH_KNOTS('',2,1,((#42517,#42518),(#42519,#42520),
(#42521,#42522)),.UNSPECIFIED.,.F.,.F.,.F.,(3,3),(2,2),(0.,1.),(0.,0.0299999999999994),
 .UNSPECIFIED.);
#381=B_SPLINE_SURFACE_WITH_KNOTS('',2,1,((#42528,#42529),(#42530,#42531),
(#42532,#42533)),.UNSPECIFIED.,.F.,.F.,.F.,(3,3),(2,2),(0.,1.),(0.,0.0299999999999994),
 .UNSPECIFIED.);
#382=B_SPLINE_SURFACE_WITH_KNOTS('',2,1,((#42539,#42540),(#42541,#42542),
(#42543,#42544)),.UNSPECIFIED.,.F.,.F.,.F.,(3,3),(2,2),(0.,1.),(0.,0.0299999999999994),
 .UNSPECIFIED.);
#383=B_SPLINE_SURFACE_WITH_KNOTS('',2,1,((#42554,#42555),(#42556,#42557),
(#42558,#42559)),.UNSPECIFIED.,.F.,.F.,.F.,(3,3),(2,2),(0.,1.),(0.,0.0299999999999994),
 .UNSPECIFIED.);
#384=B_SPLINE_SURFACE_WITH_KNOTS('',2,1,((#42565,#42566),(#42567,#42568),
(#42569,#42570)),.UNSPECIFIED.,.F.,.F.,.F.,(3,3),(2,2),(0.,1.),(0.,0.0299999999999994),
 .UNSPECIFIED.);
#385=B_SPLINE_SURFACE_WITH_KNOTS('',2,1,((#42592,#42593),(#42594,#42595),
(#42596,#42597)),.UNSPECIFIED.,.F.,.F.,.F.,(3,3),(2,2),(0.,1.),(0.,0.0299999999999994),
 .UNSPECIFIED.);
#386=B_SPLINE_SURFACE_WITH_KNOTS('',2,1,((#42605,#42606),(#42607,#42608),
(#42609,#42610)),.UNSPECIFIED.,.F.,.F.,.F.,(3,3),(2,2),(0.,1.),(0.,0.0299999999999994),
 .UNSPECIFIED.);
#387=B_SPLINE_SURFACE_WITH_KNOTS('',2,1,((#42616,#42617),(#42618,#42619),
(#42620,#42621)),.UNSPECIFIED.,.F.,.F.,.F.,(3,3),(2,2),(0.,1.),(0.,0.0299999999999994),
 .UNSPECIFIED.);
#388=B_SPLINE_SURFACE_WITH_KNOTS('',2,1,((#42627,#42628),(#42629,#42630),
(#42631,#42632)),.UNSPECIFIED.,.F.,.F.,.F.,(3,3),(2,2),(0.,1.),(0.,0.0299999999999994),
 .UNSPECIFIED.);
#389=B_SPLINE_SURFACE_WITH_KNOTS('',2,1,((#42638,#42639),(#42640,#42641),
(#42642,#42643)),.UNSPECIFIED.,.F.,.F.,.F.,(3,3),(2,2),(0.,1.),(0.,0.0299999999999994),
 .UNSPECIFIED.);
#390=B_SPLINE_SURFACE_WITH_KNOTS('',2,1,((#42649,#42650),(#42651,#42652),
(#42653,#42654)),.UNSPECIFIED.,.F.,.F.,.F.,(3,3),(2,2),(0.,1.),(0.,0.0299999999999994),
 .UNSPECIFIED.);
#391=B_SPLINE_SURFACE_WITH_KNOTS('',2,1,((#42660,#42661),(#42662,#42663),
(#42664,#42665)),.UNSPECIFIED.,.F.,.F.,.F.,(3,3),(2,2),(0.,1.),(0.,0.0299999999999994),
 .UNSPECIFIED.);
#392=B_SPLINE_SURFACE_WITH_KNOTS('',2,1,((#42671,#42672),(#42673,#42674),
(#42675,#42676)),.UNSPECIFIED.,.F.,.F.,.F.,(3,3),(2,2),(0.,1.),(0.,0.0299999999999994),
 .UNSPECIFIED.);
#393=B_SPLINE_SURFACE_WITH_KNOTS('',2,1,((#42682,#42683),(#42684,#42685),
(#42686,#42687)),.UNSPECIFIED.,.F.,.F.,.F.,(3,3),(2,2),(0.,1.),(0.,0.0299999999999994),
 .UNSPECIFIED.);
#394=B_SPLINE_SURFACE_WITH_KNOTS('',2,1,((#42693,#42694),(#42695,#42696),
(#42697,#42698)),.UNSPECIFIED.,.F.,.F.,.F.,(3,3),(2,2),(0.,1.),(0.,0.0299999999999994),
 .UNSPECIFIED.);
#395=B_SPLINE_SURFACE_WITH_KNOTS('',2,1,((#42704,#42705),(#42706,#42707),
(#42708,#42709)),.UNSPECIFIED.,.F.,.F.,.F.,(3,3),(2,2),(0.,1.),(0.,0.0299999999999994),
 .UNSPECIFIED.);
#396=B_SPLINE_SURFACE_WITH_KNOTS('',2,1,((#42715,#42716),(#42717,#42718),
(#42719,#42720)),.UNSPECIFIED.,.F.,.F.,.F.,(3,3),(2,2),(0.,1.),(0.,0.0299999999999994),
 .UNSPECIFIED.);
#397=B_SPLINE_SURFACE_WITH_KNOTS('',2,1,((#42726,#42727),(#42728,#42729),
(#42730,#42731)),.UNSPECIFIED.,.F.,.F.,.F.,(3,3),(2,2),(0.,1.),(0.,0.0299999999999994),
 .UNSPECIFIED.);
#398=B_SPLINE_SURFACE_WITH_KNOTS('',2,1,((#42741,#42742),(#42743,#42744),
(#42745,#42746)),.UNSPECIFIED.,.F.,.F.,.F.,(3,3),(2,2),(0.,1.),(0.,0.0299999999999994),
 .UNSPECIFIED.);
#399=B_SPLINE_SURFACE_WITH_KNOTS('',2,1,((#42752,#42753),(#42754,#42755),
(#42756,#42757)),.UNSPECIFIED.,.F.,.F.,.F.,(3,3),(2,2),(0.,1.),(0.,0.0299999999999994),
 .UNSPECIFIED.);
#400=B_SPLINE_SURFACE_WITH_KNOTS('',2,1,((#42763,#42764),(#42765,#42766),
(#42767,#42768)),.UNSPECIFIED.,.F.,.F.,.F.,(3,3),(2,2),(0.,1.),(0.,0.0299999999999994),
 .UNSPECIFIED.);
#401=B_SPLINE_SURFACE_WITH_KNOTS('',2,1,((#42774,#42775),(#42776,#42777),
(#42778,#42779)),.UNSPECIFIED.,.F.,.F.,.F.,(3,3),(2,2),(0.,1.),(0.,0.0299999999999994),
 .UNSPECIFIED.);
#402=B_SPLINE_SURFACE_WITH_KNOTS('',2,1,((#42785,#42786),(#42787,#42788),
(#42789,#42790)),.UNSPECIFIED.,.F.,.F.,.F.,(3,3),(2,2),(0.,1.),(0.,0.0299999999999994),
 .UNSPECIFIED.);
#403=B_SPLINE_SURFACE_WITH_KNOTS('',2,1,((#42796,#42797),(#42798,#42799),
(#42800,#42801)),.UNSPECIFIED.,.F.,.F.,.F.,(3,3),(2,2),(0.,1.),(0.,0.0299999999999994),
 .UNSPECIFIED.);
#404=B_SPLINE_SURFACE_WITH_KNOTS('',2,1,((#42807,#42808),(#42809,#42810),
(#42811,#42812)),.UNSPECIFIED.,.F.,.F.,.F.,(3,3),(2,2),(0.,1.),(0.,0.0299999999999994),
 .UNSPECIFIED.);
#405=B_SPLINE_SURFACE_WITH_KNOTS('',2,1,((#42818,#42819),(#42820,#42821),
(#42822,#42823)),.UNSPECIFIED.,.F.,.F.,.F.,(3,3),(2,2),(0.,1.),(0.,0.0299999999999994),
 .UNSPECIFIED.);
#406=B_SPLINE_SURFACE_WITH_KNOTS('',2,1,((#42829,#42830),(#42831,#42832),
(#42833,#42834)),.UNSPECIFIED.,.F.,.F.,.F.,(3,3),(2,2),(0.,1.),(0.,0.0299999999999994),
 .UNSPECIFIED.);
#407=B_SPLINE_SURFACE_WITH_KNOTS('',2,1,((#42840,#42841),(#42842,#42843),
(#42844,#42845)),.UNSPECIFIED.,.F.,.F.,.F.,(3,3),(2,2),(0.,1.),(0.,0.0299999999999994),
 .UNSPECIFIED.);
#408=B_SPLINE_SURFACE_WITH_KNOTS('',2,1,((#42851,#42852),(#42853,#42854),
(#42855,#42856)),.UNSPECIFIED.,.F.,.F.,.F.,(3,3),(2,2),(0.,1.),(0.,0.0299999999999994),
 .UNSPECIFIED.);
#409=B_SPLINE_SURFACE_WITH_KNOTS('',2,1,((#42862,#42863),(#42864,#42865),
(#42866,#42867)),.UNSPECIFIED.,.F.,.F.,.F.,(3,3),(2,2),(0.,1.),(0.,0.0299999999999994),
 .UNSPECIFIED.);
#410=B_SPLINE_SURFACE_WITH_KNOTS('',2,1,((#42873,#42874),(#42875,#42876),
(#42877,#42878)),.UNSPECIFIED.,.F.,.F.,.F.,(3,3),(2,2),(0.,1.),(0.,0.0299999999999994),
 .UNSPECIFIED.);
#411=B_SPLINE_SURFACE_WITH_KNOTS('',2,1,((#42884,#42885),(#42886,#42887),
(#42888,#42889)),.UNSPECIFIED.,.F.,.F.,.F.,(3,3),(2,2),(0.,1.),(0.,0.0299999999999994),
 .UNSPECIFIED.);
#412=B_SPLINE_SURFACE_WITH_KNOTS('',2,1,((#42895,#42896),(#42897,#42898),
(#42899,#42900)),.UNSPECIFIED.,.F.,.F.,.F.,(3,3),(2,2),(0.,1.),(0.,0.0299999999999994),
 .UNSPECIFIED.);
#413=B_SPLINE_SURFACE_WITH_KNOTS('',2,1,((#42906,#42907),(#42908,#42909),
(#42910,#42911)),.UNSPECIFIED.,.F.,.F.,.F.,(3,3),(2,2),(0.,1.),(0.,0.0299999999999994),
 .UNSPECIFIED.);
#414=B_SPLINE_SURFACE_WITH_KNOTS('',2,1,((#42917,#42918),(#42919,#42920),
(#42921,#42922)),.UNSPECIFIED.,.F.,.F.,.F.,(3,3),(2,2),(0.,1.),(0.,0.0299999999999994),
 .UNSPECIFIED.);
#415=B_SPLINE_SURFACE_WITH_KNOTS('',2,1,((#42928,#42929),(#42930,#42931),
(#42932,#42933)),.UNSPECIFIED.,.F.,.F.,.F.,(3,3),(2,2),(0.,1.),(0.,0.0299999999999994),
 .UNSPECIFIED.);
#416=B_SPLINE_SURFACE_WITH_KNOTS('',2,1,((#42943,#42944),(#42945,#42946),
(#42947,#42948)),.UNSPECIFIED.,.F.,.F.,.F.,(3,3),(2,2),(0.,1.),(0.,0.0299999999999994),
 .UNSPECIFIED.);
#417=B_SPLINE_SURFACE_WITH_KNOTS('',2,1,((#42954,#42955),(#42956,#42957),
(#42958,#42959)),.UNSPECIFIED.,.F.,.F.,.F.,(3,3),(2,2),(0.,1.),(0.,0.0299999999999994),
 .UNSPECIFIED.);
#418=B_SPLINE_SURFACE_WITH_KNOTS('',3,3,((#45016,#45017,#45018,#45019,#45020,
#45021,#45022,#45023,#45024,#45025,#45026,#45027,#45028,#45029,#45030,#45031,
#45032,#45033,#45034,#45035,#45036,#45037,#45038,#45039,#45040,#45041,#45042,
#45043,#45044,#45045,#45046,#45047,#45048,#45049,#45050,#45051,#45052,#45053,
#45054,#45055,#45056,#45057,#45058,#45059,#45060,#45061,#45062,#45063,#45064,
#45065,#45066,#45067,#45068,#45069,#45070,#45071,#45072,#45073,#45074,#45075,
#45076,#45077,#45078,#45079,#45080,#45081,#45082,#45083,#45084,#45085,#45086,
#45087,#45088,#45089,#45090,#45091,#45092,#45093,#45094,#45095,#45096,#45097,
#45098,#45099,#45100,#45101,#45102,#45103,#45104,#45105,#45106,#45107,#45108,
#45109,#45110,#45111,#45112,#45113,#45114,#45115,#45116,#45117,#45118,#45119,
#45120,#45121,#45122,#45123,#45124,#45125,#45126,#45127,#45128,#45129,#45130,
#45131,#45132,#45133,#45134,#45135,#45136,#45137,#45138,#45139,#45140,#45141,
#45142),(#45143,#45144,#45145,#45146,#45147,#45148,#45149,#45150,#45151,
#45152,#45153,#45154,#45155,#45156,#45157,#45158,#45159,#45160,#45161,#45162,
#45163,#45164,#45165,#45166,#45167,#45168,#45169,#45170,#45171,#45172,#45173,
#45174,#45175,#45176,#45177,#45178,#45179,#45180,#45181,#45182,#45183,#45184,
#45185,#45186,#45187,#45188,#45189,#45190,#45191,#45192,#45193,#45194,#45195,
#45196,#45197,#45198,#45199,#45200,#45201,#45202,#45203,#45204,#45205,#45206,
#45207,#45208,#45209,#45210,#45211,#45212,#45213,#45214,#45215,#45216,#45217,
#45218,#45219,#45220,#45221,#45222,#45223,#45224,#45225,#45226,#45227,#45228,
#45229,#45230,#45231,#45232,#45233,#45234,#45235,#45236,#45237,#45238,#45239,
#45240,#45241,#45242,#45243,#45244,#45245,#45246,#45247,#45248,#45249,#45250,
#45251,#45252,#45253,#45254,#45255,#45256,#45257,#45258,#45259,#45260,#45261,
#45262,#45263,#45264,#45265,#45266,#45267,#45268,#45269),(#45270,#45271,
#45272,#45273,#45274,#45275,#45276,#45277,#45278,#45279,#45280,#45281,#45282,
#45283,#45284,#45285,#45286,#45287,#45288,#45289,#45290,#45291,#45292,#45293,
#45294,#45295,#45296,#45297,#45298,#45299,#45300,#45301,#45302,#45303,#45304,
#45305,#45306,#45307,#45308,#45309,#45310,#45311,#45312,#45313,#45314,#45315,
#45316,#45317,#45318,#45319,#45320,#45321,#45322,#45323,#45324,#45325,#45326,
#45327,#45328,#45329,#45330,#45331,#45332,#45333,#45334,#45335,#45336,#45337,
#45338,#45339,#45340,#45341,#45342,#45343,#45344,#45345,#45346,#45347,#45348,
#45349,#45350,#45351,#45352,#45353,#45354,#45355,#45356,#45357,#45358,#45359,
#45360,#45361,#45362,#45363,#45364,#45365,#45366,#45367,#45368,#45369,#45370,
#45371,#45372,#45373,#45374,#45375,#45376,#45377,#45378,#45379,#45380,#45381,
#45382,#45383,#45384,#45385,#45386,#45387,#45388,#45389,#45390,#45391,#45392,
#45393,#45394,#45395,#45396),(#45397,#45398,#45399,#45400,#45401,#45402,
#45403,#45404,#45405,#45406,#45407,#45408,#45409,#45410,#45411,#45412,#45413,
#45414,#45415,#45416,#45417,#45418,#45419,#45420,#45421,#45422,#45423,#45424,
#45425,#45426,#45427,#45428,#45429,#45430,#45431,#45432,#45433,#45434,#45435,
#45436,#45437,#45438,#45439,#45440,#45441,#45442,#45443,#45444,#45445,#45446,
#45447,#45448,#45449,#45450,#45451,#45452,#45453,#45454,#45455,#45456,#45457,
#45458,#45459,#45460,#45461,#45462,#45463,#45464,#45465,#45466,#45467,#45468,
#45469,#45470,#45471,#45472,#45473,#45474,#45475,#45476,#45477,#45478,#45479,
#45480,#45481,#45482,#45483,#45484,#45485,#45486,#45487,#45488,#45489,#45490,
#45491,#45492,#45493,#45494,#45495,#45496,#45497,#45498,#45499,#45500,#45501,
#45502,#45503,#45504,#45505,#45506,#45507,#45508,#45509,#45510,#45511,#45512,
#45513,#45514,#45515,#45516,#45517,#45518,#45519,#45520,#45521,#45522,#45523),
(#45524,#45525,#45526,#45527,#45528,#45529,#45530,#45531,#45532,#45533,
#45534,#45535,#45536,#45537,#45538,#45539,#45540,#45541,#45542,#45543,#45544,
#45545,#45546,#45547,#45548,#45549,#45550,#45551,#45552,#45553,#45554,#45555,
#45556,#45557,#45558,#45559,#45560,#45561,#45562,#45563,#45564,#45565,#45566,
#45567,#45568,#45569,#45570,#45571,#45572,#45573,#45574,#45575,#45576,#45577,
#45578,#45579,#45580,#45581,#45582,#45583,#45584,#45585,#45586,#45587,#45588,
#45589,#45590,#45591,#45592,#45593,#45594,#45595,#45596,#45597,#45598,#45599,
#45600,#45601,#45602,#45603,#45604,#45605,#45606,#45607,#45608,#45609,#45610,
#45611,#45612,#45613,#45614,#45615,#45616,#45617,#45618,#45619,#45620,#45621,
#45622,#45623,#45624,#45625,#45626,#45627,#45628,#45629,#45630,#45631,#45632,
#45633,#45634,#45635,#45636,#45637,#45638,#45639,#45640,#45641,#45642,#45643,
#45644,#45645,#45646,#45647,#45648,#45649,#45650),(#45651,#45652,#45653,
#45654,#45655,#45656,#45657,#45658,#45659,#45660,#45661,#45662,#45663,#45664,
#45665,#45666,#45667,#45668,#45669,#45670,#45671,#45672,#45673,#45674,#45675,
#45676,#45677,#45678,#45679,#45680,#45681,#45682,#45683,#45684,#45685,#45686,
#45687,#45688,#45689,#45690,#45691,#45692,#45693,#45694,#45695,#45696,#45697,
#45698,#45699,#45700,#45701,#45702,#45703,#45704,#45705,#45706,#45707,#45708,
#45709,#45710,#45711,#45712,#45713,#45714,#45715,#45716,#45717,#45718,#45719,
#45720,#45721,#45722,#45723,#45724,#45725,#45726,#45727,#45728,#45729,#45730,
#45731,#45732,#45733,#45734,#45735,#45736,#45737,#45738,#45739,#45740,#45741,
#45742,#45743,#45744,#45745,#45746,#45747,#45748,#45749,#45750,#45751,#45752,
#45753,#45754,#45755,#45756,#45757,#45758,#45759,#45760,#45761,#45762,#45763,
#45764,#45765,#45766,#45767,#45768,#45769,#45770,#45771,#45772,#45773,#45774,
#45775,#45776,#45777),(#45778,#45779,#45780,#45781,#45782,#45783,#45784,
#45785,#45786,#45787,#45788,#45789,#45790,#45791,#45792,#45793,#45794,#45795,
#45796,#45797,#45798,#45799,#45800,#45801,#45802,#45803,#45804,#45805,#45806,
#45807,#45808,#45809,#45810,#45811,#45812,#45813,#45814,#45815,#45816,#45817,
#45818,#45819,#45820,#45821,#45822,#45823,#45824,#45825,#45826,#45827,#45828,
#45829,#45830,#45831,#45832,#45833,#45834,#45835,#45836,#45837,#45838,#45839,
#45840,#45841,#45842,#45843,#45844,#45845,#45846,#45847,#45848,#45849,#45850,
#45851,#45852,#45853,#45854,#45855,#45856,#45857,#45858,#45859,#45860,#45861,
#45862,#45863,#45864,#45865,#45866,#45867,#45868,#45869,#45870,#45871,#45872,
#45873,#45874,#45875,#45876,#45877,#45878,#45879,#45880,#45881,#45882,#45883,
#45884,#45885,#45886,#45887,#45888,#45889,#45890,#45891,#45892,#45893,#45894,
#45895,#45896,#45897,#45898,#45899,#45900,#45901,#45902,#45903,#45904),
(#45905,#45906,#45907,#45908,#45909,#45910,#45911,#45912,#45913,#45914,
#45915,#45916,#45917,#45918,#45919,#45920,#45921,#45922,#45923,#45924,#45925,
#45926,#45927,#45928,#45929,#45930,#45931,#45932,#45933,#45934,#45935,#45936,
#45937,#45938,#45939,#45940,#45941,#45942,#45943,#45944,#45945,#45946,#45947,
#45948,#45949,#45950,#45951,#45952,#45953,#45954,#45955,#45956,#45957,#45958,
#45959,#45960,#45961,#45962,#45963,#45964,#45965,#45966,#45967,#45968,#45969,
#45970,#45971,#45972,#45973,#45974,#45975,#45976,#45977,#45978,#45979,#45980,
#45981,#45982,#45983,#45984,#45985,#45986,#45987,#45988,#45989,#45990,#45991,
#45992,#45993,#45994,#45995,#45996,#45997,#45998,#45999,#46000,#46001,#46002,
#46003,#46004,#46005,#46006,#46007,#46008,#46009,#46010,#46011,#46012,#46013,
#46014,#46015,#46016,#46017,#46018,#46019,#46020,#46021,#46022,#46023,#46024,
#46025,#46026,#46027,#46028,#46029,#46030,#46031),(#46032,#46033,#46034,
#46035,#46036,#46037,#46038,#46039,#46040,#46041,#46042,#46043,#46044,#46045,
#46046,#46047,#46048,#46049,#46050,#46051,#46052,#46053,#46054,#46055,#46056,
#46057,#46058,#46059,#46060,#46061,#46062,#46063,#46064,#46065,#46066,#46067,
#46068,#46069,#46070,#46071,#46072,#46073,#46074,#46075,#46076,#46077,#46078,
#46079,#46080,#46081,#46082,#46083,#46084,#46085,#46086,#46087,#46088,#46089,
#46090,#46091,#46092,#46093,#46094,#46095,#46096,#46097,#46098,#46099,#46100,
#46101,#46102,#46103,#46104,#46105,#46106,#46107,#46108,#46109,#46110,#46111,
#46112,#46113,#46114,#46115,#46116,#46117,#46118,#46119,#46120,#46121,#46122,
#46123,#46124,#46125,#46126,#46127,#46128,#46129,#46130,#46131,#46132,#46133,
#46134,#46135,#46136,#46137,#46138,#46139,#46140,#46141,#46142,#46143,#46144,
#46145,#46146,#46147,#46148,#46149,#46150,#46151,#46152,#46153,#46154,#46155,
#46156,#46157,#46158),(#46159,#46160,#46161,#46162,#46163,#46164,#46165,
#46166,#46167,#46168,#46169,#46170,#46171,#46172,#46173,#46174,#46175,#46176,
#46177,#46178,#46179,#46180,#46181,#46182,#46183,#46184,#46185,#46186,#46187,
#46188,#46189,#46190,#46191,#46192,#46193,#46194,#46195,#46196,#46197,#46198,
#46199,#46200,#46201,#46202,#46203,#46204,#46205,#46206,#46207,#46208,#46209,
#46210,#46211,#46212,#46213,#46214,#46215,#46216,#46217,#46218,#46219,#46220,
#46221,#46222,#46223,#46224,#46225,#46226,#46227,#46228,#46229,#46230,#46231,
#46232,#46233,#46234,#46235,#46236,#46237,#46238,#46239,#46240,#46241,#46242,
#46243,#46244,#46245,#46246,#46247,#46248,#46249,#46250,#46251,#46252,#46253,
#46254,#46255,#46256,#46257,#46258,#46259,#46260,#46261,#46262,#46263,#46264,
#46265,#46266,#46267,#46268,#46269,#46270,#46271,#46272,#46273,#46274,#46275,
#46276,#46277,#46278,#46279,#46280,#46281,#46282,#46283,#46284,#46285)),
 .UNSPECIFIED.,.T.,.F.,.F.,(4,1,1,1,1,1,1,4),(4,1,1,1,1,1,1,1,1,1,1,1,1,
1,1,1,1,1,1,1,1,1,1,1,1,1,1,1,1,1,1,1,1,1,1,1,1,1,1,1,1,1,1,1,1,1,1,1,1,
1,1,1,1,1,1,1,1,1,1,1,1,1,1,1,1,1,1,1,1,1,1,1,1,1,1,1,1,1,1,1,1,1,1,1,1,
1,1,1,1,1,1,1,1,1,1,1,1,1,1,1,1,1,1,1,1,1,1,1,1,1,1,1,1,1,1,1,1,1,1,1,1,
1,1,1,4),(-3.14159265358979,-2.24399475256414,-1.34639685153848,-0.448798950512828,
0.448798950512828,1.34639685153848,2.24399475256414,3.14159265358979),(0.,
0.00446428571428571,0.00892857142857143,0.0178571428571429,0.0267857142857143,
0.0357142857142857,0.0446428571428571,0.0535714285714286,0.0625,0.0714285714285714,
0.0803571428571428,0.0892857142857143,0.0982142857142857,0.107142857142857,
0.116071428571429,0.125,0.129464285714286,0.133928571428571,0.138392857142857,
0.142857142857143,0.151785714285714,0.160714285714286,0.169642857142857,
0.178571428571429,0.1875,0.196428571428571,0.205357142857143,0.214285714285714,
0.223214285714286,0.232142857142857,0.241071428571429,0.25,0.258928571428571,
0.267857142857143,0.276785714285714,0.285714285714286,0.294642857142857,
0.303571428571429,0.3125,0.321428571428571,0.330357142857143,0.339285714285714,
0.348214285714286,0.357142857142857,0.366071428571428,0.375,0.383928571428571,
0.392857142857143,0.401785714285714,0.410714285714286,0.419642857142857,
0.428571428571429,0.4375,0.446428571428571,0.455357142857143,0.464285714285714,
0.473214285714286,0.482142857142857,0.494047619047619,0.5,0.504464285714286,
0.508928571428571,0.517857142857143,0.526785714285714,0.535714285714286,
0.544642857142857,0.553571428571429,0.5625,0.571428571428571,0.580357142857143,
0.589285714285714,0.598214285714286,0.607142857142857,0.616071428571429,
0.625,0.633928571428571,0.642857142857143,0.647321428571428,0.651785714285714,
0.660714285714286,0.666666666666667,0.678571428571428,0.6796875,0.680803571428571,
0.6875,0.696428571428571,0.705357142857143,0.714285714285714,0.726190476190476,
0.735119047619047,0.738095238095238,0.75,0.761904761904762,0.76984126984127,
0.777777777777778,0.785714285714286,0.793650793650794,0.801587301587302,
0.809523809523809,0.81547619047619,0.821428571428571,0.827380952380952,
0.830357142857143,0.833333333333333,0.839285714285714,0.845238095238095,
0.851190476190476,0.857142857142857,0.866071428571429,0.875,0.883928571428571,
0.892857142857143,0.901785714285714,0.910714285714286,0.919642857142857,
0.928571428571429,0.9375,0.946428571428571,0.955357142857143,0.964285714285714,
0.973214285714286,0.982142857142857,0.991071428571429,0.995535714285714,
1.),.UNSPECIFIED.);
#419=B_SPLINE_SURFACE_WITH_KNOTS('',3,3,((#47318,#47319,#47320,#47321,#47322,
#47323,#47324,#47325,#47326,#47327,#47328,#47329,#47330,#47331,#47332,#47333,
#47334,#47335,#47336,#47337,#47338,#47339,#47340,#47341,#47342,#47343,#47344,
#47345,#47346,#47347,#47348,#47349,#47350,#47351,#47352,#47353,#47354,#47355,
#47356,#47357,#47358,#47359,#47360,#47361,#47362,#47363,#47364,#47365,#47366,
#47367,#47368,#47369,#47370,#47371,#47372,#47373,#47374,#47375,#47376,#47377,
#47378,#47379,#47380,#47381,#47382,#47383,#47384),(#47385,#47386,#47387,
#47388,#47389,#47390,#47391,#47392,#47393,#47394,#47395,#47396,#47397,#47398,
#47399,#47400,#47401,#47402,#47403,#47404,#47405,#47406,#47407,#47408,#47409,
#47410,#47411,#47412,#47413,#47414,#47415,#47416,#47417,#47418,#47419,#47420,
#47421,#47422,#47423,#47424,#47425,#47426,#47427,#47428,#47429,#47430,#47431,
#47432,#47433,#47434,#47435,#47436,#47437,#47438,#47439,#47440,#47441,#47442,
#47443,#47444,#47445,#47446,#47447,#47448,#47449,#47450,#47451),(#47452,
#47453,#47454,#47455,#47456,#47457,#47458,#47459,#47460,#47461,#47462,#47463,
#47464,#47465,#47466,#47467,#47468,#47469,#47470,#47471,#47472,#47473,#47474,
#47475,#47476,#47477,#47478,#47479,#47480,#47481,#47482,#47483,#47484,#47485,
#47486,#47487,#47488,#47489,#47490,#47491,#47492,#47493,#47494,#47495,#47496,
#47497,#47498,#47499,#47500,#47501,#47502,#47503,#47504,#47505,#47506,#47507,
#47508,#47509,#47510,#47511,#47512,#47513,#47514,#47515,#47516,#47517,#47518),
(#47519,#47520,#47521,#47522,#47523,#47524,#47525,#47526,#47527,#47528,
#47529,#47530,#47531,#47532,#47533,#47534,#47535,#47536,#47537,#47538,#47539,
#47540,#47541,#47542,#47543,#47544,#47545,#47546,#47547,#47548,#47549,#47550,
#47551,#47552,#47553,#47554,#47555,#47556,#47557,#47558,#47559,#47560,#47561,
#47562,#47563,#47564,#47565,#47566,#47567,#47568,#47569,#47570,#47571,#47572,
#47573,#47574,#47575,#47576,#47577,#47578,#47579,#47580,#47581,#47582,#47583,
#47584,#47585)),.UNSPECIFIED.,.F.,.F.,.F.,(4,4),(4,1,1,1,1,1,1,1,1,1,1,
1,1,1,1,1,1,1,1,1,1,1,1,1,1,1,1,1,1,1,1,1,1,1,1,1,1,1,1,1,1,1,1,1,1,1,1,
1,1,1,1,1,1,1,1,1,1,1,1,1,1,1,1,1,4),(0.,0.0820126057383863),(8.31473274985803,
9.31389506365537,10.3130573774527,11.3122196912501,12.3113820050474,13.3105443188447,
14.3097066326421,15.3088689464394,16.3080312602368,17.3071935740341,18.3063558878314,
19.3055182016288,20.3046805154261,21.3038428292235,22.3030051430208,23.3021674568182,
24.3013297706155,25.3004920844128,26.2996543982102,27.2988167120075,28.2979790258049,
29.2971413396022,30.2963036533995,31.2954659671969,32.2946282809942,33.2937905947916,
34.2929529085889,35.2921152223863,36.2912775361836,37.2904398499809,38.2896021637783,
39.2887644775756,40.287926791373,41.2870891051703,42.2862514189677,43.285413732765,
44.2845760465623,45.2837383603597,46.282900674157,47.2820629879544,48.2812253017517,
49.280387615549,50.2795499293464,51.2787122431437,52.2778745569411,53.2770368707384,
54.2761991845358,55.2753614983331,56.2745238121304,57.2736861259278,58.2728484397251,
59.2720107535225,60.2711730673198,61.2703353811171,62.2694976949145,63.2686600087118,
64.2678223225092,65.2669846363065,66.2661469501039,67.2653092639012,68.2644715776985,
69.2636338914959,70.2627962052932,71.2619585190906,72.2611208328879),
 .UNSPECIFIED.);
#420=B_SPLINE_SURFACE_WITH_KNOTS('',3,3,((#47821,#47822,#47823,#47824,#47825,
#47826,#47827,#47828,#47829,#47830,#47831,#47832,#47833,#47834,#47835,#47836,
#47837,#47838,#47839,#47840,#47841,#47842,#47843,#47844,#47845,#47846,#47847,
#47848,#47849,#47850,#47851,#47852,#47853,#47854,#47855,#47856,#47857,#47858,
#47859,#47860,#47861,#47862,#47863,#47864,#47865,#47866,#47867,#47868,#47869,
#47870,#47871,#47872,#47873,#47874,#47875,#47876,#47877,#47878,#47879,#47880,
#47881,#47882,#47883,#47884,#47885,#47886,#47887),(#47888,#47889,#47890,
#47891,#47892,#47893,#47894,#47895,#47896,#47897,#47898,#47899,#47900,#47901,
#47902,#47903,#47904,#47905,#47906,#47907,#47908,#47909,#47910,#47911,#47912,
#47913,#47914,#47915,#47916,#47917,#47918,#47919,#47920,#47921,#47922,#47923,
#47924,#47925,#47926,#47927,#47928,#47929,#47930,#47931,#47932,#47933,#47934,
#47935,#47936,#47937,#47938,#47939,#47940,#47941,#47942,#47943,#47944,#47945,
#47946,#47947,#47948,#47949,#47950,#47951,#47952,#47953,#47954),(#47955,
#47956,#47957,#47958,#47959,#47960,#47961,#47962,#47963,#47964,#47965,#47966,
#47967,#47968,#47969,#47970,#47971,#47972,#47973,#47974,#47975,#47976,#47977,
#47978,#47979,#47980,#47981,#47982,#47983,#47984,#47985,#47986,#47987,#47988,
#47989,#47990,#47991,#47992,#47993,#47994,#47995,#47996,#47997,#47998,#47999,
#48000,#48001,#48002,#48003,#48004,#48005,#48006,#48007,#48008,#48009,#48010,
#48011,#48012,#48013,#48014,#48015,#48016,#48017,#48018,#48019,#48020,#48021),
(#48022,#48023,#48024,#48025,#48026,#48027,#48028,#48029,#48030,#48031,
#48032,#48033,#48034,#48035,#48036,#48037,#48038,#48039,#48040,#48041,#48042,
#48043,#48044,#48045,#48046,#48047,#48048,#48049,#48050,#48051,#48052,#48053,
#48054,#48055,#48056,#48057,#48058,#48059,#48060,#48061,#48062,#48063,#48064,
#48065,#48066,#48067,#48068,#48069,#48070,#48071,#48072,#48073,#48074,#48075,
#48076,#48077,#48078,#48079,#48080,#48081,#48082,#48083,#48084,#48085,#48086,
#48087,#48088)),.UNSPECIFIED.,.F.,.F.,.F.,(4,4),(4,1,1,1,1,1,1,1,1,1,1,
1,1,1,1,1,1,1,1,1,1,1,1,1,1,1,1,1,1,1,1,1,1,1,1,1,1,1,1,1,1,1,1,1,1,1,1,
1,1,1,1,1,1,1,1,1,1,1,1,1,1,1,1,1,4),(0.,0.0820126057383863),(11.6152142277547,
12.614376541552,13.6135388553494,14.6127011691467,15.6118634829441,16.6110257967414,
17.6101881105388,18.6093504243361,19.6085127381334,20.6076750519308,21.6068373657281,
22.6059996795255,23.6051619933228,24.6043243071202,25.6034866209175,26.6026489347148,
27.6018112485122,28.6009735623095,29.6001358761069,30.5992981899042,31.5984605037015,
32.5976228174989,33.5967851312962,34.5959474450936,35.5951097588909,36.5942720726883,
37.5934343864856,38.5925967002829,39.5917590140803,40.5909213278776,41.590083641675,
42.5892459554723,43.5884082692696,44.587570583067,45.5867328968643,46.5858952106617,
47.585057524459,48.5842198382564,49.5833821520537,50.582544465851,51.5817067796484,
52.5808690934457,53.5800314072431,54.5791937210404,55.5783560348378,56.5775183486351,
57.5766806624324,58.5758429762298,59.5750052900271,60.5741676038245,61.5733299176218,
62.5724922314191,63.5716545452165,64.5708168590138,65.5699791728112,66.5691414866085,
67.5683038004059,68.5674661142032,69.5666284280005,70.5657907417979,71.5649530555952,
72.5641153693926,73.5632776831899,74.5624399969873,75.5616023107846),
 .UNSPECIFIED.);
#421=B_SPLINE_SURFACE_WITH_KNOTS('',3,3,((#48911,#48912,#48913,#48914,#48915,
#48916,#48917,#48918,#48919,#48920,#48921,#48922,#48923,#48924,#48925,#48926,
#48927,#48928,#48929,#48930,#48931,#48932,#48933,#48934,#48935,#48936,#48937,
#48938,#48939,#48940,#48941,#48942,#48943,#48944,#48945,#48946,#48947,#48948,
#48949,#48950,#48951,#48952,#48953,#48954,#48955,#48956,#48957,#48958,#48959,
#48960,#48961,#48962,#48963,#48964,#48965,#48966,#48967),(#48968,#48969,
#48970,#48971,#48972,#48973,#48974,#48975,#48976,#48977,#48978,#48979,#48980,
#48981,#48982,#48983,#48984,#48985,#48986,#48987,#48988,#48989,#48990,#48991,
#48992,#48993,#48994,#48995,#48996,#48997,#48998,#48999,#49000,#49001,#49002,
#49003,#49004,#49005,#49006,#49007,#49008,#49009,#49010,#49011,#49012,#49013,
#49014,#49015,#49016,#49017,#49018,#49019,#49020,#49021,#49022,#49023,#49024),
(#49025,#49026,#49027,#49028,#49029,#49030,#49031,#49032,#49033,#49034,
#49035,#49036,#49037,#49038,#49039,#49040,#49041,#49042,#49043,#49044,#49045,
#49046,#49047,#49048,#49049,#49050,#49051,#49052,#49053,#49054,#49055,#49056,
#49057,#49058,#49059,#49060,#49061,#49062,#49063,#49064,#49065,#49066,#49067,
#49068,#49069,#49070,#49071,#49072,#49073,#49074,#49075,#49076,#49077,#49078,
#49079,#49080,#49081),(#49082,#49083,#49084,#49085,#49086,#49087,#49088,
#49089,#49090,#49091,#49092,#49093,#49094,#49095,#49096,#49097,#49098,#49099,
#49100,#49101,#49102,#49103,#49104,#49105,#49106,#49107,#49108,#49109,#49110,
#49111,#49112,#49113,#49114,#49115,#49116,#49117,#49118,#49119,#49120,#49121,
#49122,#49123,#49124,#49125,#49126,#49127,#49128,#49129,#49130,#49131,#49132,
#49133,#49134,#49135,#49136,#49137,#49138),(#49139,#49140,#49141,#49142,
#49143,#49144,#49145,#49146,#49147,#49148,#49149,#49150,#49151,#49152,#49153,
#49154,#49155,#49156,#49157,#49158,#49159,#49160,#49161,#49162,#49163,#49164,
#49165,#49166,#49167,#49168,#49169,#49170,#49171,#49172,#49173,#49174,#49175,
#49176,#49177,#49178,#49179,#49180,#49181,#49182,#49183,#49184,#49185,#49186,
#49187,#49188,#49189,#49190,#49191,#49192,#49193,#49194,#49195),(#49196,
#49197,#49198,#49199,#49200,#49201,#49202,#49203,#49204,#49205,#49206,#49207,
#49208,#49209,#49210,#49211,#49212,#49213,#49214,#49215,#49216,#49217,#49218,
#49219,#49220,#49221,#49222,#49223,#49224,#49225,#49226,#49227,#49228,#49229,
#49230,#49231,#49232,#49233,#49234,#49235,#49236,#49237,#49238,#49239,#49240,
#49241,#49242,#49243,#49244,#49245,#49246,#49247,#49248,#49249,#49250,#49251,
#49252),(#49253,#49254,#49255,#49256,#49257,#49258,#49259,#49260,#49261,
#49262,#49263,#49264,#49265,#49266,#49267,#49268,#49269,#49270,#49271,#49272,
#49273,#49274,#49275,#49276,#49277,#49278,#49279,#49280,#49281,#49282,#49283,
#49284,#49285,#49286,#49287,#49288,#49289,#49290,#49291,#49292,#49293,#49294,
#49295,#49296,#49297,#49298,#49299,#49300,#49301,#49302,#49303,#49304,#49305,
#49306,#49307,#49308,#49309),(#49310,#49311,#49312,#49313,#49314,#49315,
#49316,#49317,#49318,#49319,#49320,#49321,#49322,#49323,#49324,#49325,#49326,
#49327,#49328,#49329,#49330,#49331,#49332,#49333,#49334,#49335,#49336,#49337,
#49338,#49339,#49340,#49341,#49342,#49343,#49344,#49345,#49346,#49347,#49348,
#49349,#49350,#49351,#49352,#49353,#49354,#49355,#49356,#49357,#49358,#49359,
#49360,#49361,#49362,#49363,#49364,#49365,#49366),(#49367,#49368,#49369,
#49370,#49371,#49372,#49373,#49374,#49375,#49376,#49377,#49378,#49379,#49380,
#49381,#49382,#49383,#49384,#49385,#49386,#49387,#49388,#49389,#49390,#49391,
#49392,#49393,#49394,#49395,#49396,#49397,#49398,#49399,#49400,#49401,#49402,
#49403,#49404,#49405,#49406,#49407,#49408,#49409,#49410,#49411,#49412,#49413,
#49414,#49415,#49416,#49417,#49418,#49419,#49420,#49421,#49422,#49423),
(#49424,#49425,#49426,#49427,#49428,#49429,#49430,#49431,#49432,#49433,
#49434,#49435,#49436,#49437,#49438,#49439,#49440,#49441,#49442,#49443,#49444,
#49445,#49446,#49447,#49448,#49449,#49450,#49451,#49452,#49453,#49454,#49455,
#49456,#49457,#49458,#49459,#49460,#49461,#49462,#49463,#49464,#49465,#49466,
#49467,#49468,#49469,#49470,#49471,#49472,#49473,#49474,#49475,#49476,#49477,
#49478,#49479,#49480)),.UNSPECIFIED.,.T.,.F.,.F.,(4,1,1,1,1,1,1,4),(4,1,
1,1,1,1,1,1,1,1,1,1,1,1,1,1,1,1,1,1,1,1,1,1,1,1,1,1,1,1,1,1,1,1,1,1,1,1,
1,1,1,1,1,1,1,1,1,1,1,1,1,1,1,1,4),(-3.14159265358979,-2.24399475256414,
-1.34639685153848,-0.448798950512828,0.448798950512828,1.34639685153848,
2.24399475256414,3.14159265358979),(0.,0.00892857142857143,0.0178571428571429,
0.0357142857142857,0.0535714285714286,0.0714285714285714,0.0892857142857143,
0.107142857142857,0.125,0.142857142857143,0.166666666666667,0.19047619047619,
0.214285714285714,0.232142857142857,0.25,0.267857142857143,0.285714285714286,
0.303571428571429,0.321428571428571,0.339285714285714,0.357142857142857,
0.375,0.392857142857143,0.410714285714286,0.428571428571429,0.452380952380952,
0.476190476190476,0.5,0.523809523809524,0.547619047619048,0.571428571428571,
0.595238095238095,0.619047619047619,0.642857142857143,0.666666666666667,
0.682539682539682,0.698412698412698,0.714285714285714,0.73015873015873,
0.746031746031746,0.761904761904762,0.785714285714286,0.809523809523809,
0.833333333333333,0.857142857142857,0.866071428571429,0.875,0.892857142857143,
0.910714285714286,0.928571428571429,0.946428571428571,0.964285714285714,
0.982142857142857,0.991071428571429,1.),.UNSPECIFIED.);
#422=B_SPLINE_SURFACE_WITH_KNOTS('',3,3,((#52834,#52835,#52836,#52837,#52838,
#52839,#52840,#52841,#52842,#52843,#52844,#52845,#52846,#52847,#52848,#52849,
#52850,#52851,#52852,#52853,#52854,#52855,#52856,#52857,#52858,#52859,#52860,
#52861,#52862,#52863,#52864,#52865,#52866,#52867,#52868,#52869,#52870,#52871,
#52872,#52873,#52874,#52875,#52876,#52877,#52878,#52879,#52880,#52881,#52882,
#52883,#52884,#52885,#52886,#52887,#52888,#52889,#52890,#52891,#52892,#52893,
#52894,#52895,#52896,#52897,#52898,#52899,#52900,#52901,#52902,#52903,#52904,
#52905,#52906,#52907,#52908,#52909,#52910,#52911,#52912,#52913,#52914,#52915,
#52916,#52917,#52918,#52919,#52920,#52921,#52922,#52923,#52924,#52925,#52926,
#52927,#52928,#52929,#52930,#52931,#52932,#52933,#52934,#52935,#52936,#52937,
#52938,#52939,#52940,#52941,#52942,#52943,#52944,#52945,#52946,#52947,#52948,
#52949,#52950,#52951,#52952,#52953,#52954,#52955,#52956,#52957,#52958,#52959,
#52960,#52961,#52962,#52963,#52964,#52965,#52966,#52967,#52968,#52969,#52970,
#52971,#52972,#52973,#52974,#52975,#52976,#52977,#52978,#52979,#52980,#52981,
#52982,#52983,#52984,#52985,#52986,#52987,#52988,#52989,#52990,#52991,#52992,
#52993,#52994,#52995,#52996,#52997,#52998,#52999,#53000,#53001,#53002,#53003,
#53004,#53005,#53006,#53007,#53008,#53009,#53010,#53011,#53012,#53013,#53014,
#53015,#53016,#53017,#53018,#53019,#53020,#53021,#53022,#53023,#53024,#53025,
#53026,#53027,#53028,#53029,#53030,#53031,#53032,#53033,#53034,#53035,#53036,
#53037,#53038,#53039,#53040,#53041,#53042,#53043,#53044,#53045,#53046,#53047,
#53048,#53049,#53050,#53051,#53052,#53053,#53054,#53055,#53056,#53057,#53058,
#53059,#53060,#53061,#53062,#53063,#53064,#53065,#53066,#53067,#53068,#53069,
#53070,#53071,#53072,#53073,#53074,#53075,#53076,#53077,#53078,#53079,#53080,
#53081,#53082,#53083,#53084,#53085,#53086,#53087,#53088,#53089,#53090,#53091,
#53092,#53093,#53094,#53095,#53096,#53097,#53098,#53099,#53100,#53101,#53102,
#53103),(#53104,#53105,#53106,#53107,#53108,#53109,#53110,#53111,#53112,
#53113,#53114,#53115,#53116,#53117,#53118,#53119,#53120,#53121,#53122,#53123,
#53124,#53125,#53126,#53127,#53128,#53129,#53130,#53131,#53132,#53133,#53134,
#53135,#53136,#53137,#53138,#53139,#53140,#53141,#53142,#53143,#53144,#53145,
#53146,#53147,#53148,#53149,#53150,#53151,#53152,#53153,#53154,#53155,#53156,
#53157,#53158,#53159,#53160,#53161,#53162,#53163,#53164,#53165,#53166,#53167,
#53168,#53169,#53170,#53171,#53172,#53173,#53174,#53175,#53176,#53177,#53178,
#53179,#53180,#53181,#53182,#53183,#53184,#53185,#53186,#53187,#53188,#53189,
#53190,#53191,#53192,#53193,#53194,#53195,#53196,#53197,#53198,#53199,#53200,
#53201,#53202,#53203,#53204,#53205,#53206,#53207,#53208,#53209,#53210,#53211,
#53212,#53213,#53214,#53215,#53216,#53217,#53218,#53219,#53220,#53221,#53222,
#53223,#53224,#53225,#53226,#53227,#53228,#53229,#53230,#53231,#53232,#53233,
#53234,#53235,#53236,#53237,#53238,#53239,#53240,#53241,#53242,#53243,#53244,
#53245,#53246,#53247,#53248,#53249,#53250,#53251,#53252,#53253,#53254,#53255,
#53256,#53257,#53258,#53259,#53260,#53261,#53262,#53263,#53264,#53265,#53266,
#53267,#53268,#53269,#53270,#53271,#53272,#53273,#53274,#53275,#53276,#53277,
#53278,#53279,#53280,#53281,#53282,#53283,#53284,#53285,#53286,#53287,#53288,
#53289,#53290,#53291,#53292,#53293,#53294,#53295,#53296,#53297,#53298,#53299,
#53300,#53301,#53302,#53303,#53304,#53305,#53306,#53307,#53308,#53309,#53310,
#53311,#53312,#53313,#53314,#53315,#53316,#53317,#53318,#53319,#53320,#53321,
#53322,#53323,#53324,#53325,#53326,#53327,#53328,#53329,#53330,#53331,#53332,
#53333,#53334,#53335,#53336,#53337,#53338,#53339,#53340,#53341,#53342,#53343,
#53344,#53345,#53346,#53347,#53348,#53349,#53350,#53351,#53352,#53353,#53354,
#53355,#53356,#53357,#53358,#53359,#53360,#53361,#53362,#53363,#53364,#53365,
#53366,#53367,#53368,#53369,#53370,#53371,#53372,#53373),(#53374,#53375,
#53376,#53377,#53378,#53379,#53380,#53381,#53382,#53383,#53384,#53385,#53386,
#53387,#53388,#53389,#53390,#53391,#53392,#53393,#53394,#53395,#53396,#53397,
#53398,#53399,#53400,#53401,#53402,#53403,#53404,#53405,#53406,#53407,#53408,
#53409,#53410,#53411,#53412,#53413,#53414,#53415,#53416,#53417,#53418,#53419,
#53420,#53421,#53422,#53423,#53424,#53425,#53426,#53427,#53428,#53429,#53430,
#53431,#53432,#53433,#53434,#53435,#53436,#53437,#53438,#53439,#53440,#53441,
#53442,#53443,#53444,#53445,#53446,#53447,#53448,#53449,#53450,#53451,#53452,
#53453,#53454,#53455,#53456,#53457,#53458,#53459,#53460,#53461,#53462,#53463,
#53464,#53465,#53466,#53467,#53468,#53469,#53470,#53471,#53472,#53473,#53474,
#53475,#53476,#53477,#53478,#53479,#53480,#53481,#53482,#53483,#53484,#53485,
#53486,#53487,#53488,#53489,#53490,#53491,#53492,#53493,#53494,#53495,#53496,
#53497,#53498,#53499,#53500,#53501,#53502,#53503,#53504,#53505,#53506,#53507,
#53508,#53509,#53510,#53511,#53512,#53513,#53514,#53515,#53516,#53517,#53518,
#53519,#53520,#53521,#53522,#53523,#53524,#53525,#53526,#53527,#53528,#53529,
#53530,#53531,#53532,#53533,#53534,#53535,#53536,#53537,#53538,#53539,#53540,
#53541,#53542,#53543,#53544,#53545,#53546,#53547,#53548,#53549,#53550,#53551,
#53552,#53553,#53554,#53555,#53556,#53557,#53558,#53559,#53560,#53561,#53562,
#53563,#53564,#53565,#53566,#53567,#53568,#53569,#53570,#53571,#53572,#53573,
#53574,#53575,#53576,#53577,#53578,#53579,#53580,#53581,#53582,#53583,#53584,
#53585,#53586,#53587,#53588,#53589,#53590,#53591,#53592,#53593,#53594,#53595,
#53596,#53597,#53598,#53599,#53600,#53601,#53602,#53603,#53604,#53605,#53606,
#53607,#53608,#53609,#53610,#53611,#53612,#53613,#53614,#53615,#53616,#53617,
#53618,#53619,#53620,#53621,#53622,#53623,#53624,#53625,#53626,#53627,#53628,
#53629,#53630,#53631,#53632,#53633,#53634,#53635,#53636,#53637,#53638,#53639,
#53640,#53641,#53642,#53643),(#53644,#53645,#53646,#53647,#53648,#53649,
#53650,#53651,#53652,#53653,#53654,#53655,#53656,#53657,#53658,#53659,#53660,
#53661,#53662,#53663,#53664,#53665,#53666,#53667,#53668,#53669,#53670,#53671,
#53672,#53673,#53674,#53675,#53676,#53677,#53678,#53679,#53680,#53681,#53682,
#53683,#53684,#53685,#53686,#53687,#53688,#53689,#53690,#53691,#53692,#53693,
#53694,#53695,#53696,#53697,#53698,#53699,#53700,#53701,#53702,#53703,#53704,
#53705,#53706,#53707,#53708,#53709,#53710,#53711,#53712,#53713,#53714,#53715,
#53716,#53717,#53718,#53719,#53720,#53721,#53722,#53723,#53724,#53725,#53726,
#53727,#53728,#53729,#53730,#53731,#53732,#53733,#53734,#53735,#53736,#53737,
#53738,#53739,#53740,#53741,#53742,#53743,#53744,#53745,#53746,#53747,#53748,
#53749,#53750,#53751,#53752,#53753,#53754,#53755,#53756,#53757,#53758,#53759,
#53760,#53761,#53762,#53763,#53764,#53765,#53766,#53767,#53768,#53769,#53770,
#53771,#53772,#53773,#53774,#53775,#53776,#53777,#53778,#53779,#53780,#53781,
#53782,#53783,#53784,#53785,#53786,#53787,#53788,#53789,#53790,#53791,#53792,
#53793,#53794,#53795,#53796,#53797,#53798,#53799,#53800,#53801,#53802,#53803,
#53804,#53805,#53806,#53807,#53808,#53809,#53810,#53811,#53812,#53813,#53814,
#53815,#53816,#53817,#53818,#53819,#53820,#53821,#53822,#53823,#53824,#53825,
#53826,#53827,#53828,#53829,#53830,#53831,#53832,#53833,#53834,#53835,#53836,
#53837,#53838,#53839,#53840,#53841,#53842,#53843,#53844,#53845,#53846,#53847,
#53848,#53849,#53850,#53851,#53852,#53853,#53854,#53855,#53856,#53857,#53858,
#53859,#53860,#53861,#53862,#53863,#53864,#53865,#53866,#53867,#53868,#53869,
#53870,#53871,#53872,#53873,#53874,#53875,#53876,#53877,#53878,#53879,#53880,
#53881,#53882,#53883,#53884,#53885,#53886,#53887,#53888,#53889,#53890,#53891,
#53892,#53893,#53894,#53895,#53896,#53897,#53898,#53899,#53900,#53901,#53902,
#53903,#53904,#53905,#53906,#53907,#53908,#53909,#53910,#53911,#53912,#53913)),
 .UNSPECIFIED.,.F.,.F.,.F.,(4,4),(4,1,1,1,1,1,1,1,1,1,1,1,1,1,1,1,1,1,1,
1,1,1,1,1,1,1,1,1,1,1,1,1,1,1,1,1,1,1,1,1,1,1,1,1,1,1,1,1,1,1,1,1,1,1,1,
1,1,1,1,1,1,1,1,1,1,1,1,1,1,1,1,1,1,1,1,1,1,1,1,1,1,1,1,1,1,1,1,1,1,1,1,
1,1,1,1,1,1,1,1,1,1,1,1,1,1,1,1,1,1,1,1,1,1,1,1,1,1,1,1,1,1,1,1,1,1,1,1,
1,1,1,1,1,1,1,1,1,1,1,1,1,1,1,1,1,1,1,1,1,1,1,1,1,1,1,1,1,1,1,1,1,1,1,1,
1,1,1,1,1,1,1,1,1,1,1,1,1,1,1,1,1,1,1,1,1,1,1,1,1,1,1,1,1,1,1,1,1,1,1,1,
1,1,1,1,1,1,1,1,1,1,1,1,1,1,1,1,1,1,1,1,1,1,1,1,1,1,1,1,1,1,1,1,1,1,1,1,
1,1,1,1,1,1,1,1,1,1,1,1,1,1,1,1,1,1,1,1,1,1,1,1,1,1,1,1,1,1,1,1,4),(0.,
0.0460148164544131),(8.31058692274005,9.30823418142654,10.305881440113,
11.3035286987995,12.301175957486,13.2988232161725,14.296470474859,15.2941177335455,
16.291764992232,17.2894122509185,18.2870595096049,19.2847067682914,20.2823540269779,
21.2800012856644,22.2776485443509,23.2752958030374,24.2729430617239,25.2705903204104,
26.2682375790969,27.2658848377834,28.2635320964698,29.2611793551563,30.2588266138428,
31.2564738725293,32.2541211312158,33.2517683899023,34.2494156485888,35.2470629072753,
36.2447101659618,37.2423574246482,38.2400046833347,39.2376519420212,40.2352992007077,
41.2329464593942,42.2305937180807,43.2282409767672,44.2258882354537,45.2235354941402,
46.2211827528266,47.2188300115131,48.2164772701996,49.2141245288861,50.2117717875726,
51.2094190462591,52.2070663049456,53.2047135636321,54.2023608223186,55.2000080810051,
56.1976553396915,57.195302598378,58.1929498570645,59.190597115751,60.1882443744375,
61.185891633124,62.1835388918105,63.181186150497,64.1788334091835,65.17648066787,
66.1741279265564,67.1717751852429,68.1694224439294,69.1670697026159,70.1647169613024,
71.1623642199889,72.1600114786754,73.1576587373619,74.1553059960484,75.1529532547349,
76.1506005134213,77.1482477721078,78.1458950307943,79.1435422894808,80.1411895481673,
81.1388368068538,82.1364840655403,83.1341313242268,84.1317785829133,85.1294258415997,
86.1270731002862,87.1247203589727,88.1223676176592,89.1200148763457,90.1176621350322,
91.1153093937187,92.1129566524052,93.1106039110917,94.1082511697781,95.1058984284646,
96.1035456871511,97.1011929458376,98.0988402045241,99.0964874632106,100.094134721897,
101.091781980584,102.08942923927,103.087076497957,104.084723756643,105.08237101533,
106.080018274016,107.077665532703,108.075312791389,109.072960050075,110.070607308762,
111.068254567448,112.065901826135,113.063549084821,114.061196343508,115.058843602194,
116.056490860881,117.054138119567,118.051785378254,119.04943263694,120.047079895627,
121.044727154313,122.042374413,123.040021671686,124.037668930373,125.035316189059,
126.032963447746,127.030610706432,128.028257965119,129.025905223805,130.023552482492,
131.021199741178,132.018846999865,133.016494258551,134.014141517238,135.011788775924,
136.009436034611,137.007083293297,138.004730551984,139.00237781067,140.000025069357,
140.997672328043,141.99531958673,142.992966845416,143.990614104103,144.988261362789,
145.985908621476,146.983555880162,147.981203138849,148.978850397535,149.976497656222,
150.974144914908,151.971792173595,152.969439432281,153.967086690968,154.964733949654,
155.96238120834,156.960028467027,157.957675725713,158.9553229844,159.952970243086,
160.950617501773,161.948264760459,162.945912019146,163.943559277832,164.941206536519,
165.938853795205,166.936501053892,167.934148312578,168.931795571265,169.929442829951,
170.927090088638,171.924737347324,172.922384606011,173.920031864697,174.917679123384,
175.91532638207,176.912973640757,177.910620899443,178.90826815813,179.905915416816,
180.903562675503,181.901209934189,182.898857192876,183.896504451562,184.894151710249,
185.891798968935,186.889446227622,187.887093486308,188.884740744995,189.882388003681,
190.880035262368,191.877682521054,192.875329779741,193.872977038427,194.870624297114,
195.8682715558,196.865918814487,197.863566073173,198.86121333186,199.858860590546,
200.856507849232,201.854155107919,202.851802366605,203.849449625292,204.847096883978,
205.844744142665,206.842391401351,207.840038660038,208.837685918724,209.835333177411,
210.832980436097,211.830627694784,212.82827495347,213.825922212157,214.823569470843,
215.82121672953,216.818863988216,217.816511246903,218.814158505589,219.811805764276,
220.809453022962,221.807100281649,222.804747540335,223.802394799022,224.800042057708,
225.797689316395,226.795336575081,227.792983833768,228.790631092454,229.788278351141,
230.785925609827,231.783572868514,232.7812201272,233.778867385887,234.776514644573,
235.77416190326,236.771809161946,237.769456420633,238.767103679319,239.764750938006,
240.762398196692,241.760045455379,242.757692714065,243.755339972752,244.752987231438,
245.750634490125,246.748281748811,247.745929007497,248.743576266184,249.74122352487,
250.738870783557,251.736518042243,252.73416530093,253.731812559616,254.729459818303,
255.727107076989,256.724754335676,257.722401594362,258.720048853049,259.717696111735,
260.715343370422,261.712990629108,262.710637887795,263.708285146481,264.705932405168,
265.703579663854,266.701226922541,267.698874181227,268.696521439914,269.6941686986,
270.691815957287,271.689463215973,272.68711047466,273.684757733346,274.682404992033),
 .UNSPECIFIED.);
#423=B_SPLINE_SURFACE_WITH_KNOTS('',3,3,((#54128,#54129,#54130,#54131,#54132,
#54133,#54134,#54135,#54136,#54137,#54138,#54139,#54140,#54141,#54142,#54143,
#54144,#54145,#54146,#54147,#54148,#54149,#54150,#54151,#54152,#54153,#54154,
#54155,#54156,#54157,#54158,#54159,#54160,#54161,#54162,#54163,#54164,#54165,
#54166,#54167,#54168,#54169,#54170,#54171,#54172,#54173,#54174,#54175,#54176,
#54177,#54178,#54179,#54180,#54181,#54182,#54183,#54184,#54185,#54186,#54187,
#54188,#54189,#54190,#54191,#54192,#54193,#54194,#54195,#54196,#54197,#54198,
#54199,#54200,#54201,#54202,#54203,#54204,#54205,#54206,#54207,#54208,#54209,
#54210,#54211,#54212,#54213,#54214,#54215,#54216,#54217,#54218,#54219,#54220,
#54221,#54222,#54223,#54224,#54225,#54226,#54227,#54228,#54229,#54230,#54231,
#54232,#54233,#54234,#54235,#54236,#54237,#54238,#54239,#54240,#54241,#54242,
#54243,#54244,#54245,#54246,#54247,#54248,#54249,#54250,#54251,#54252,#54253,
#54254,#54255,#54256,#54257,#54258,#54259,#54260,#54261,#54262,#54263,#54264,
#54265,#54266,#54267,#54268,#54269,#54270,#54271,#54272,#54273,#54274,#54275,
#54276,#54277,#54278,#54279,#54280,#54281,#54282,#54283,#54284,#54285,#54286,
#54287,#54288,#54289,#54290,#54291,#54292,#54293,#54294,#54295,#54296,#54297,
#54298,#54299,#54300,#54301,#54302,#54303,#54304,#54305,#54306,#54307,#54308,
#54309,#54310,#54311,#54312,#54313,#54314,#54315,#54316,#54317,#54318,#54319,
#54320,#54321,#54322,#54323,#54324,#54325,#54326,#54327,#54328,#54329,#54330,
#54331,#54332,#54333,#54334,#54335,#54336,#54337,#54338,#54339,#54340,#54341,
#54342,#54343,#54344,#54345,#54346,#54347,#54348,#54349,#54350,#54351,#54352,
#54353,#54354,#54355,#54356,#54357,#54358,#54359,#54360,#54361,#54362,#54363,
#54364,#54365,#54366,#54367,#54368,#54369,#54370,#54371,#54372,#54373,#54374,
#54375,#54376,#54377,#54378,#54379,#54380,#54381,#54382,#54383,#54384,#54385,
#54386,#54387,#54388,#54389,#54390,#54391,#54392,#54393,#54394,#54395,#54396,
#54397),(#54398,#54399,#54400,#54401,#54402,#54403,#54404,#54405,#54406,
#54407,#54408,#54409,#54410,#54411,#54412,#54413,#54414,#54415,#54416,#54417,
#54418,#54419,#54420,#54421,#54422,#54423,#54424,#54425,#54426,#54427,#54428,
#54429,#54430,#54431,#54432,#54433,#54434,#54435,#54436,#54437,#54438,#54439,
#54440,#54441,#54442,#54443,#54444,#54445,#54446,#54447,#54448,#54449,#54450,
#54451,#54452,#54453,#54454,#54455,#54456,#54457,#54458,#54459,#54460,#54461,
#54462,#54463,#54464,#54465,#54466,#54467,#54468,#54469,#54470,#54471,#54472,
#54473,#54474,#54475,#54476,#54477,#54478,#54479,#54480,#54481,#54482,#54483,
#54484,#54485,#54486,#54487,#54488,#54489,#54490,#54491,#54492,#54493,#54494,
#54495,#54496,#54497,#54498,#54499,#54500,#54501,#54502,#54503,#54504,#54505,
#54506,#54507,#54508,#54509,#54510,#54511,#54512,#54513,#54514,#54515,#54516,
#54517,#54518,#54519,#54520,#54521,#54522,#54523,#54524,#54525,#54526,#54527,
#54528,#54529,#54530,#54531,#54532,#54533,#54534,#54535,#54536,#54537,#54538,
#54539,#54540,#54541,#54542,#54543,#54544,#54545,#54546,#54547,#54548,#54549,
#54550,#54551,#54552,#54553,#54554,#54555,#54556,#54557,#54558,#54559,#54560,
#54561,#54562,#54563,#54564,#54565,#54566,#54567,#54568,#54569,#54570,#54571,
#54572,#54573,#54574,#54575,#54576,#54577,#54578,#54579,#54580,#54581,#54582,
#54583,#54584,#54585,#54586,#54587,#54588,#54589,#54590,#54591,#54592,#54593,
#54594,#54595,#54596,#54597,#54598,#54599,#54600,#54601,#54602,#54603,#54604,
#54605,#54606,#54607,#54608,#54609,#54610,#54611,#54612,#54613,#54614,#54615,
#54616,#54617,#54618,#54619,#54620,#54621,#54622,#54623,#54624,#54625,#54626,
#54627,#54628,#54629,#54630,#54631,#54632,#54633,#54634,#54635,#54636,#54637,
#54638,#54639,#54640,#54641,#54642,#54643,#54644,#54645,#54646,#54647,#54648,
#54649,#54650,#54651,#54652,#54653,#54654,#54655,#54656,#54657,#54658,#54659,
#54660,#54661,#54662,#54663,#54664,#54665,#54666,#54667),(#54668,#54669,
#54670,#54671,#54672,#54673,#54674,#54675,#54676,#54677,#54678,#54679,#54680,
#54681,#54682,#54683,#54684,#54685,#54686,#54687,#54688,#54689,#54690,#54691,
#54692,#54693,#54694,#54695,#54696,#54697,#54698,#54699,#54700,#54701,#54702,
#54703,#54704,#54705,#54706,#54707,#54708,#54709,#54710,#54711,#54712,#54713,
#54714,#54715,#54716,#54717,#54718,#54719,#54720,#54721,#54722,#54723,#54724,
#54725,#54726,#54727,#54728,#54729,#54730,#54731,#54732,#54733,#54734,#54735,
#54736,#54737,#54738,#54739,#54740,#54741,#54742,#54743,#54744,#54745,#54746,
#54747,#54748,#54749,#54750,#54751,#54752,#54753,#54754,#54755,#54756,#54757,
#54758,#54759,#54760,#54761,#54762,#54763,#54764,#54765,#54766,#54767,#54768,
#54769,#54770,#54771,#54772,#54773,#54774,#54775,#54776,#54777,#54778,#54779,
#54780,#54781,#54782,#54783,#54784,#54785,#54786,#54787,#54788,#54789,#54790,
#54791,#54792,#54793,#54794,#54795,#54796,#54797,#54798,#54799,#54800,#54801,
#54802,#54803,#54804,#54805,#54806,#54807,#54808,#54809,#54810,#54811,#54812,
#54813,#54814,#54815,#54816,#54817,#54818,#54819,#54820,#54821,#54822,#54823,
#54824,#54825,#54826,#54827,#54828,#54829,#54830,#54831,#54832,#54833,#54834,
#54835,#54836,#54837,#54838,#54839,#54840,#54841,#54842,#54843,#54844,#54845,
#54846,#54847,#54848,#54849,#54850,#54851,#54852,#54853,#54854,#54855,#54856,
#54857,#54858,#54859,#54860,#54861,#54862,#54863,#54864,#54865,#54866,#54867,
#54868,#54869,#54870,#54871,#54872,#54873,#54874,#54875,#54876,#54877,#54878,
#54879,#54880,#54881,#54882,#54883,#54884,#54885,#54886,#54887,#54888,#54889,
#54890,#54891,#54892,#54893,#54894,#54895,#54896,#54897,#54898,#54899,#54900,
#54901,#54902,#54903,#54904,#54905,#54906,#54907,#54908,#54909,#54910,#54911,
#54912,#54913,#54914,#54915,#54916,#54917,#54918,#54919,#54920,#54921,#54922,
#54923,#54924,#54925,#54926,#54927,#54928,#54929,#54930,#54931,#54932,#54933,
#54934,#54935,#54936,#54937),(#54938,#54939,#54940,#54941,#54942,#54943,
#54944,#54945,#54946,#54947,#54948,#54949,#54950,#54951,#54952,#54953,#54954,
#54955,#54956,#54957,#54958,#54959,#54960,#54961,#54962,#54963,#54964,#54965,
#54966,#54967,#54968,#54969,#54970,#54971,#54972,#54973,#54974,#54975,#54976,
#54977,#54978,#54979,#54980,#54981,#54982,#54983,#54984,#54985,#54986,#54987,
#54988,#54989,#54990,#54991,#54992,#54993,#54994,#54995,#54996,#54997,#54998,
#54999,#55000,#55001,#55002,#55003,#55004,#55005,#55006,#55007,#55008,#55009,
#55010,#55011,#55012,#55013,#55014,#55015,#55016,#55017,#55018,#55019,#55020,
#55021,#55022,#55023,#55024,#55025,#55026,#55027,#55028,#55029,#55030,#55031,
#55032,#55033,#55034,#55035,#55036,#55037,#55038,#55039,#55040,#55041,#55042,
#55043,#55044,#55045,#55046,#55047,#55048,#55049,#55050,#55051,#55052,#55053,
#55054,#55055,#55056,#55057,#55058,#55059,#55060,#55061,#55062,#55063,#55064,
#55065,#55066,#55067,#55068,#55069,#55070,#55071,#55072,#55073,#55074,#55075,
#55076,#55077,#55078,#55079,#55080,#55081,#55082,#55083,#55084,#55085,#55086,
#55087,#55088,#55089,#55090,#55091,#55092,#55093,#55094,#55095,#55096,#55097,
#55098,#55099,#55100,#55101,#55102,#55103,#55104,#55105,#55106,#55107,#55108,
#55109,#55110,#55111,#55112,#55113,#55114,#55115,#55116,#55117,#55118,#55119,
#55120,#55121,#55122,#55123,#55124,#55125,#55126,#55127,#55128,#55129,#55130,
#55131,#55132,#55133,#55134,#55135,#55136,#55137,#55138,#55139,#55140,#55141,
#55142,#55143,#55144,#55145,#55146,#55147,#55148,#55149,#55150,#55151,#55152,
#55153,#55154,#55155,#55156,#55157,#55158,#55159,#55160,#55161,#55162,#55163,
#55164,#55165,#55166,#55167,#55168,#55169,#55170,#55171,#55172,#55173,#55174,
#55175,#55176,#55177,#55178,#55179,#55180,#55181,#55182,#55183,#55184,#55185,
#55186,#55187,#55188,#55189,#55190,#55191,#55192,#55193,#55194,#55195,#55196,
#55197,#55198,#55199,#55200,#55201,#55202,#55203,#55204,#55205,#55206,#55207)),
 .UNSPECIFIED.,.F.,.F.,.F.,(4,4),(4,1,1,1,1,1,1,1,1,1,1,1,1,1,1,1,1,1,1,
1,1,1,1,1,1,1,1,1,1,1,1,1,1,1,1,1,1,1,1,1,1,1,1,1,1,1,1,1,1,1,1,1,1,1,1,
1,1,1,1,1,1,1,1,1,1,1,1,1,1,1,1,1,1,1,1,1,1,1,1,1,1,1,1,1,1,1,1,1,1,1,1,
1,1,1,1,1,1,1,1,1,1,1,1,1,1,1,1,1,1,1,1,1,1,1,1,1,1,1,1,1,1,1,1,1,1,1,1,
1,1,1,1,1,1,1,1,1,1,1,1,1,1,1,1,1,1,1,1,1,1,1,1,1,1,1,1,1,1,1,1,1,1,1,1,
1,1,1,1,1,1,1,1,1,1,1,1,1,1,1,1,1,1,1,1,1,1,1,1,1,1,1,1,1,1,1,1,1,1,1,1,
1,1,1,1,1,1,1,1,1,1,1,1,1,1,1,1,1,1,1,1,1,1,1,1,1,1,1,1,1,1,1,1,1,1,1,1,
1,1,1,1,1,1,1,1,1,1,1,1,1,1,1,1,1,1,1,1,1,1,1,1,1,1,1,1,1,1,1,1,4),(0.,
0.0460148164544131),(11.615421519111,12.6130687777975,13.610716036484,14.6083632951705,
15.606010553857,16.6036578125435,17.60130507123,18.5989523299165,19.596599588603,
20.5942468472894,21.5918941059759,22.5895413646624,23.5871886233489,24.5848358820354,
25.5824831407219,26.5801303994084,27.5777776580949,28.5754249167814,29.5730721754678,
30.5707194341543,31.5683666928408,32.5660139515273,33.5636612102138,34.5613084689003,
35.5589557275868,36.5566029862733,37.5542502449598,38.5518975036462,39.5495447623327,
40.5471920210192,41.5448392797057,42.5424865383922,43.5401337970787,44.5377810557652,
45.5354283144517,46.5330755731381,47.5307228318246,48.5283700905111,49.5260173491976,
50.5236646078841,51.5213118665706,52.5189591252571,53.5166063839436,54.5142536426301,
55.5119009013166,56.509548160003,57.5071954186895,58.504842677376,59.5024899360625,
60.500137194749,61.4977844534355,62.495431712122,63.4930789708085,64.490726229495,
65.4883734881815,66.4860207468679,67.4836680055544,68.4813152642409,69.4789625229274,
70.4766097816139,71.4742570403004,72.4719042989869,73.4695515576734,74.4671988163598,
75.4648460750463,76.4624933337328,77.4601405924193,78.4577878511058,79.4554351097923,
80.4530823684788,81.4507296271653,82.4483768858518,83.4460241445382,84.4436714032247,
85.4413186619112,86.4389659205977,87.4366131792842,88.4342604379707,89.4319076966572,
90.4295549553437,91.4272022140302,92.4248494727166,93.4224967314031,94.4201439900896,
95.4177912487761,96.4154385074626,97.4130857661491,98.4107330248356,99.4083802835221,
100.406027542209,101.403674800895,102.401322059582,103.398969318268,104.396616576955,
105.394263835641,106.391911094327,107.389558353014,108.3872056117,109.384852870387,
110.382500129073,111.38014738776,112.377794646446,113.375441905133,114.373089163819,
115.370736422506,116.368383681192,117.366030939879,118.363678198565,119.361325457252,
120.358972715938,121.356619974625,122.354267233311,123.351914491998,124.349561750684,
125.347209009371,126.344856268057,127.342503526744,128.34015078543,129.337798044117,
130.335445302803,131.33309256149,132.330739820176,133.328387078863,134.326034337549,
135.323681596236,136.321328854922,137.318976113609,138.316623372295,139.314270630982,
140.311917889668,141.309565148355,142.307212407041,143.304859665728,144.302506924414,
145.300154183101,146.297801441787,147.295448700474,148.29309595916,149.290743217847,
150.288390476533,151.286037735219,152.283684993906,153.281332252592,154.278979511279,
155.276626769965,156.274274028652,157.271921287338,158.269568546025,159.267215804711,
160.264863063398,161.262510322084,162.260157580771,163.257804839457,164.255452098144,
165.25309935683,166.250746615517,167.248393874203,168.24604113289,169.243688391576,
170.241335650263,171.238982908949,172.236630167636,173.234277426322,174.231924685009,
175.229571943695,176.227219202382,177.224866461068,178.222513719755,179.220160978441,
180.217808237128,181.215455495814,182.213102754501,183.210750013187,184.208397271874,
185.20604453056,186.203691789247,187.201339047933,188.19898630662,189.196633565306,
190.194280823993,191.191928082679,192.189575341366,193.187222600052,194.184869858739,
195.182517117425,196.180164376111,197.177811634798,198.175458893484,199.173106152171,
200.170753410857,201.168400669544,202.16604792823,203.163695186917,204.161342445603,
205.15898970429,206.156636962976,207.154284221663,208.151931480349,209.149578739036,
210.147225997722,211.144873256409,212.142520515095,213.140167773782,214.137815032468,
215.135462291155,216.133109549841,217.130756808528,218.128404067214,219.126051325901,
220.123698584587,221.121345843274,222.11899310196,223.116640360647,224.114287619333,
225.11193487802,226.109582136706,227.107229395393,228.104876654079,229.102523912766,
230.100171171452,231.097818430139,232.095465688825,233.093112947512,234.090760206198,
235.088407464885,236.086054723571,237.083701982258,238.081349240944,239.078996499631,
240.076643758317,241.074291017004,242.07193827569,243.069585534376,244.067232793063,
245.064880051749,246.062527310436,247.060174569122,248.057821827809,249.055469086495,
250.053116345182,251.050763603868,252.048410862555,253.046058121241,254.043705379928,
255.041352638614,256.038999897301,257.036647155987,258.034294414674,259.03194167336,
260.029588932047,261.027236190733,262.02488344942,263.022530708106,264.020177966793,
265.017825225479,266.015472484166,267.013119742852,268.010767001539,269.008414260225,
270.006061518912,271.003708777598,272.001356036285,272.999003294971,273.996650553658,
274.994297812344,275.991945071031,276.989592329717,277.987239588404),
 .UNSPECIFIED.);
#424=B_SPLINE_SURFACE_WITH_KNOTS('',3,3,((#61259,#61260,#61261,#61262,#61263,
#61264,#61265,#61266,#61267,#61268,#61269,#61270,#61271,#61272,#61273,#61274,
#61275,#61276,#61277,#61278,#61279,#61280,#61281,#61282,#61283,#61284,#61285,
#61286,#61287,#61288,#61289,#61290,#61291,#61292,#61293,#61294,#61295,#61296,
#61297,#61298,#61299,#61300,#61301,#61302,#61303,#61304,#61305,#61306,#61307,
#61308,#61309,#61310,#61311,#61312,#61313,#61314,#61315,#61316,#61317,#61318,
#61319,#61320,#61321,#61322,#61323,#61324,#61325,#61326,#61327,#61328,#61329,
#61330,#61331,#61332,#61333,#61334,#61335,#61336,#61337,#61338,#61339,#61340,
#61341,#61342,#61343,#61344,#61345,#61346,#61347,#61348,#61349,#61350,#61351,
#61352,#61353,#61354,#61355,#61356,#61357,#61358,#61359,#61360,#61361,#61362,
#61363,#61364,#61365,#61366,#61367,#61368,#61369,#61370,#61371,#61372,#61373,
#61374,#61375,#61376,#61377,#61378,#61379,#61380,#61381,#61382,#61383,#61384,
#61385,#61386,#61387,#61388,#61389,#61390,#61391,#61392,#61393,#61394,#61395,
#61396,#61397,#61398,#61399,#61400,#61401,#61402,#61403,#61404,#61405,#61406,
#61407,#61408,#61409,#61410,#61411,#61412,#61413,#61414,#61415,#61416,#61417,
#61418,#61419,#61420,#61421,#61422,#61423,#61424,#61425,#61426,#61427,#61428,
#61429,#61430,#61431,#61432,#61433,#61434,#61435,#61436,#61437,#61438,#61439,
#61440,#61441,#61442,#61443,#61444,#61445,#61446,#61447,#61448,#61449,#61450,
#61451,#61452,#61453,#61454,#61455,#61456,#61457,#61458,#61459,#61460,#61461,
#61462,#61463,#61464,#61465,#61466,#61467,#61468,#61469,#61470,#61471,#61472,
#61473,#61474,#61475,#61476,#61477,#61478,#61479,#61480,#61481,#61482,#61483,
#61484,#61485,#61486,#61487,#61488,#61489,#61490,#61491,#61492,#61493,#61494,
#61495,#61496,#61497,#61498,#61499,#61500,#61501,#61502,#61503,#61504,#61505,
#61506,#61507,#61508,#61509,#61510,#61511,#61512,#61513,#61514,#61515,#61516,
#61517,#61518,#61519,#61520,#61521,#61522,#61523,#61524,#61525,#61526,#61527,
#61528,#61529,#61530,#61531,#61532,#61533,#61534,#61535,#61536,#61537,#61538,
#61539,#61540,#61541,#61542,#61543,#61544,#61545,#61546,#61547,#61548,#61549,
#61550,#61551,#61552,#61553,#61554,#61555,#61556,#61557,#61558,#61559,#61560,
#61561,#61562,#61563,#61564,#61565,#61566,#61567,#61568,#61569,#61570,#61571,
#61572,#61573,#61574,#61575,#61576,#61577,#61578,#61579,#61580,#61581,#61582,
#61583,#61584,#61585,#61586,#61587,#61588,#61589,#61590,#61591,#61592,#61593,
#61594,#61595,#61596,#61597,#61598,#61599,#61600,#61601,#61602,#61603,#61604,
#61605,#61606,#61607,#61608,#61609,#61610,#61611,#61612,#61613,#61614,#61615,
#61616,#61617,#61618,#61619,#61620,#61621,#61622,#61623,#61624,#61625,#61626,
#61627,#61628,#61629,#61630,#61631,#61632,#61633,#61634,#61635,#61636,#61637,
#61638,#61639,#61640,#61641,#61642,#61643,#61644,#61645,#61646,#61647,#61648,
#61649,#61650,#61651,#61652,#61653,#61654,#61655,#61656,#61657,#61658,#61659,
#61660,#61661,#61662,#61663,#61664,#61665,#61666,#61667,#61668,#61669,#61670,
#61671,#61672,#61673,#61674,#61675,#61676,#61677,#61678,#61679,#61680,#61681,
#61682,#61683,#61684,#61685,#61686,#61687,#61688,#61689,#61690,#61691,#61692,
#61693,#61694,#61695,#61696),(#61697,#61698,#61699,#61700,#61701,#61702,
#61703,#61704,#61705,#61706,#61707,#61708,#61709,#61710,#61711,#61712,#61713,
#61714,#61715,#61716,#61717,#61718,#61719,#61720,#61721,#61722,#61723,#61724,
#61725,#61726,#61727,#61728,#61729,#61730,#61731,#61732,#61733,#61734,#61735,
#61736,#61737,#61738,#61739,#61740,#61741,#61742,#61743,#61744,#61745,#61746,
#61747,#61748,#61749,#61750,#61751,#61752,#61753,#61754,#61755,#61756,#61757,
#61758,#61759,#61760,#61761,#61762,#61763,#61764,#61765,#61766,#61767,#61768,
#61769,#61770,#61771,#61772,#61773,#61774,#61775,#61776,#61777,#61778,#61779,
#61780,#61781,#61782,#61783,#61784,#61785,#61786,#61787,#61788,#61789,#61790,
#61791,#61792,#61793,#61794,#61795,#61796,#61797,#61798,#61799,#61800,#61801,
#61802,#61803,#61804,#61805,#61806,#61807,#61808,#61809,#61810,#61811,#61812,
#61813,#61814,#61815,#61816,#61817,#61818,#61819,#61820,#61821,#61822,#61823,
#61824,#61825,#61826,#61827,#61828,#61829,#61830,#61831,#61832,#61833,#61834,
#61835,#61836,#61837,#61838,#61839,#61840,#61841,#61842,#61843,#61844,#61845,
#61846,#61847,#61848,#61849,#61850,#61851,#61852,#61853,#61854,#61855,#61856,
#61857,#61858,#61859,#61860,#61861,#61862,#61863,#61864,#61865,#61866,#61867,
#61868,#61869,#61870,#61871,#61872,#61873,#61874,#61875,#61876,#61877,#61878,
#61879,#61880,#61881,#61882,#61883,#61884,#61885,#61886,#61887,#61888,#61889,
#61890,#61891,#61892,#61893,#61894,#61895,#61896,#61897,#61898,#61899,#61900,
#61901,#61902,#61903,#61904,#61905,#61906,#61907,#61908,#61909,#61910,#61911,
#61912,#61913,#61914,#61915,#61916,#61917,#61918,#61919,#61920,#61921,#61922,
#61923,#61924,#61925,#61926,#61927,#61928,#61929,#61930,#61931,#61932,#61933,
#61934,#61935,#61936,#61937,#61938,#61939,#61940,#61941,#61942,#61943,#61944,
#61945,#61946,#61947,#61948,#61949,#61950,#61951,#61952,#61953,#61954,#61955,
#61956,#61957,#61958,#61959,#61960,#61961,#61962,#61963,#61964,#61965,#61966,
#61967,#61968,#61969,#61970,#61971,#61972,#61973,#61974,#61975,#61976,#61977,
#61978,#61979,#61980,#61981,#61982,#61983,#61984,#61985,#61986,#61987,#61988,
#61989,#61990,#61991,#61992,#61993,#61994,#61995,#61996,#61997,#61998,#61999,
#62000,#62001,#62002,#62003,#62004,#62005,#62006,#62007,#62008,#62009,#62010,
#62011,#62012,#62013,#62014,#62015,#62016,#62017,#62018,#62019,#62020,#62021,
#62022,#62023,#62024,#62025,#62026,#62027,#62028,#62029,#62030,#62031,#62032,
#62033,#62034,#62035,#62036,#62037,#62038,#62039,#62040,#62041,#62042,#62043,
#62044,#62045,#62046,#62047,#62048,#62049,#62050,#62051,#62052,#62053,#62054,
#62055,#62056,#62057,#62058,#62059,#62060,#62061,#62062,#62063,#62064,#62065,
#62066,#62067,#62068,#62069,#62070,#62071,#62072,#62073,#62074,#62075,#62076,
#62077,#62078,#62079,#62080,#62081,#62082,#62083,#62084,#62085,#62086,#62087,
#62088,#62089,#62090,#62091,#62092,#62093,#62094,#62095,#62096,#62097,#62098,
#62099,#62100,#62101,#62102,#62103,#62104,#62105,#62106,#62107,#62108,#62109,
#62110,#62111,#62112,#62113,#62114,#62115,#62116,#62117,#62118,#62119,#62120,
#62121,#62122,#62123,#62124,#62125,#62126,#62127,#62128,#62129,#62130,#62131,
#62132,#62133,#62134),(#62135,#62136,#62137,#62138,#62139,#62140,#62141,
#62142,#62143,#62144,#62145,#62146,#62147,#62148,#62149,#62150,#62151,#62152,
#62153,#62154,#62155,#62156,#62157,#62158,#62159,#62160,#62161,#62162,#62163,
#62164,#62165,#62166,#62167,#62168,#62169,#62170,#62171,#62172,#62173,#62174,
#62175,#62176,#62177,#62178,#62179,#62180,#62181,#62182,#62183,#62184,#62185,
#62186,#62187,#62188,#62189,#62190,#62191,#62192,#62193,#62194,#62195,#62196,
#62197,#62198,#62199,#62200,#62201,#62202,#62203,#62204,#62205,#62206,#62207,
#62208,#62209,#62210,#62211,#62212,#62213,#62214,#62215,#62216,#62217,#62218,
#62219,#62220,#62221,#62222,#62223,#62224,#62225,#62226,#62227,#62228,#62229,
#62230,#62231,#62232,#62233,#62234,#62235,#62236,#62237,#62238,#62239,#62240,
#62241,#62242,#62243,#62244,#62245,#62246,#62247,#62248,#62249,#62250,#62251,
#62252,#62253,#62254,#62255,#62256,#62257,#62258,#62259,#62260,#62261,#62262,
#62263,#62264,#62265,#62266,#62267,#62268,#62269,#62270,#62271,#62272,#62273,
#62274,#62275,#62276,#62277,#62278,#62279,#62280,#62281,#62282,#62283,#62284,
#62285,#62286,#62287,#62288,#62289,#62290,#62291,#62292,#62293,#62294,#62295,
#62296,#62297,#62298,#62299,#62300,#62301,#62302,#62303,#62304,#62305,#62306,
#62307,#62308,#62309,#62310,#62311,#62312,#62313,#62314,#62315,#62316,#62317,
#62318,#62319,#62320,#62321,#62322,#62323,#62324,#62325,#62326,#62327,#62328,
#62329,#62330,#62331,#62332,#62333,#62334,#62335,#62336,#62337,#62338,#62339,
#62340,#62341,#62342,#62343,#62344,#62345,#62346,#62347,#62348,#62349,#62350,
#62351,#62352,#62353,#62354,#62355,#62356,#62357,#62358,#62359,#62360,#62361,
#62362,#62363,#62364,#62365,#62366,#62367,#62368,#62369,#62370,#62371,#62372,
#62373,#62374,#62375,#62376,#62377,#62378,#62379,#62380,#62381,#62382,#62383,
#62384,#62385,#62386,#62387,#62388,#62389,#62390,#62391,#62392,#62393,#62394,
#62395,#62396,#62397,#62398,#62399,#62400,#62401,#62402,#62403,#62404,#62405,
#62406,#62407,#62408,#62409,#62410,#62411,#62412,#62413,#62414,#62415,#62416,
#62417,#62418,#62419,#62420,#62421,#62422,#62423,#62424,#62425,#62426,#62427,
#62428,#62429,#62430,#62431,#62432,#62433,#62434,#62435,#62436,#62437,#62438,
#62439,#62440,#62441,#62442,#62443,#62444,#62445,#62446,#62447,#62448,#62449,
#62450,#62451,#62452,#62453,#62454,#62455,#62456,#62457,#62458,#62459,#62460,
#62461,#62462,#62463,#62464,#62465,#62466,#62467,#62468,#62469,#62470,#62471,
#62472,#62473,#62474,#62475,#62476,#62477,#62478,#62479,#62480,#62481,#62482,
#62483,#62484,#62485,#62486,#62487,#62488,#62489,#62490,#62491,#62492,#62493,
#62494,#62495,#62496,#62497,#62498,#62499,#62500,#62501,#62502,#62503,#62504,
#62505,#62506,#62507,#62508,#62509,#62510,#62511,#62512,#62513,#62514,#62515,
#62516,#62517,#62518,#62519,#62520,#62521,#62522,#62523,#62524,#62525,#62526,
#62527,#62528,#62529,#62530,#62531,#62532,#62533,#62534,#62535,#62536,#62537,
#62538,#62539,#62540,#62541,#62542,#62543,#62544,#62545,#62546,#62547,#62548,
#62549,#62550,#62551,#62552,#62553,#62554,#62555,#62556,#62557,#62558,#62559,
#62560,#62561,#62562,#62563,#62564,#62565,#62566,#62567,#62568,#62569,#62570,
#62571,#62572),(#62573,#62574,#62575,#62576,#62577,#62578,#62579,#62580,
#62581,#62582,#62583,#62584,#62585,#62586,#62587,#62588,#62589,#62590,#62591,
#62592,#62593,#62594,#62595,#62596,#62597,#62598,#62599,#62600,#62601,#62602,
#62603,#62604,#62605,#62606,#62607,#62608,#62609,#62610,#62611,#62612,#62613,
#62614,#62615,#62616,#62617,#62618,#62619,#62620,#62621,#62622,#62623,#62624,
#62625,#62626,#62627,#62628,#62629,#62630,#62631,#62632,#62633,#62634,#62635,
#62636,#62637,#62638,#62639,#62640,#62641,#62642,#62643,#62644,#62645,#62646,
#62647,#62648,#62649,#62650,#62651,#62652,#62653,#62654,#62655,#62656,#62657,
#62658,#62659,#62660,#62661,#62662,#62663,#62664,#62665,#62666,#62667,#62668,
#62669,#62670,#62671,#62672,#62673,#62674,#62675,#62676,#62677,#62678,#62679,
#62680,#62681,#62682,#62683,#62684,#62685,#62686,#62687,#62688,#62689,#62690,
#62691,#62692,#62693,#62694,#62695,#62696,#62697,#62698,#62699,#62700,#62701,
#62702,#62703,#62704,#62705,#62706,#62707,#62708,#62709,#62710,#62711,#62712,
#62713,#62714,#62715,#62716,#62717,#62718,#62719,#62720,#62721,#62722,#62723,
#62724,#62725,#62726,#62727,#62728,#62729,#62730,#62731,#62732,#62733,#62734,
#62735,#62736,#62737,#62738,#62739,#62740,#62741,#62742,#62743,#62744,#62745,
#62746,#62747,#62748,#62749,#62750,#62751,#62752,#62753,#62754,#62755,#62756,
#62757,#62758,#62759,#62760,#62761,#62762,#62763,#62764,#62765,#62766,#62767,
#62768,#62769,#62770,#62771,#62772,#62773,#62774,#62775,#62776,#62777,#62778,
#62779,#62780,#62781,#62782,#62783,#62784,#62785,#62786,#62787,#62788,#62789,
#62790,#62791,#62792,#62793,#62794,#62795,#62796,#62797,#62798,#62799,#62800,
#62801,#62802,#62803,#62804,#62805,#62806,#62807,#62808,#62809,#62810,#62811,
#62812,#62813,#62814,#62815,#62816,#62817,#62818,#62819,#62820,#62821,#62822,
#62823,#62824,#62825,#62826,#62827,#62828,#62829,#62830,#62831,#62832,#62833,
#62834,#62835,#62836,#62837,#62838,#62839,#62840,#62841,#62842,#62843,#62844,
#62845,#62846,#62847,#62848,#62849,#62850,#62851,#62852,#62853,#62854,#62855,
#62856,#62857,#62858,#62859,#62860,#62861,#62862,#62863,#62864,#62865,#62866,
#62867,#62868,#62869,#62870,#62871,#62872,#62873,#62874,#62875,#62876,#62877,
#62878,#62879,#62880,#62881,#62882,#62883,#62884,#62885,#62886,#62887,#62888,
#62889,#62890,#62891,#62892,#62893,#62894,#62895,#62896,#62897,#62898,#62899,
#62900,#62901,#62902,#62903,#62904,#62905,#62906,#62907,#62908,#62909,#62910,
#62911,#62912,#62913,#62914,#62915,#62916,#62917,#62918,#62919,#62920,#62921,
#62922,#62923,#62924,#62925,#62926,#62927,#62928,#62929,#62930,#62931,#62932,
#62933,#62934,#62935,#62936,#62937,#62938,#62939,#62940,#62941,#62942,#62943,
#62944,#62945,#62946,#62947,#62948,#62949,#62950,#62951,#62952,#62953,#62954,
#62955,#62956,#62957,#62958,#62959,#62960,#62961,#62962,#62963,#62964,#62965,
#62966,#62967,#62968,#62969,#62970,#62971,#62972,#62973,#62974,#62975,#62976,
#62977,#62978,#62979,#62980,#62981,#62982,#62983,#62984,#62985,#62986,#62987,
#62988,#62989,#62990,#62991,#62992,#62993,#62994,#62995,#62996,#62997,#62998,
#62999,#63000,#63001,#63002,#63003,#63004,#63005,#63006,#63007,#63008,#63009,
#63010)),.UNSPECIFIED.,.F.,.F.,.F.,(4,4),(4,1,1,1,1,1,1,1,1,1,1,1,1,1,1,
1,1,1,1,1,1,1,1,1,1,1,1,1,1,1,1,1,1,1,1,1,1,1,1,1,1,1,1,1,1,1,1,1,1,1,1,
1,1,1,1,1,1,1,1,1,1,1,1,1,1,1,1,1,1,1,1,1,1,1,1,1,1,1,1,1,1,1,1,1,1,1,1,
1,1,1,1,1,1,1,1,1,1,1,1,1,1,1,1,1,1,1,1,1,1,1,1,1,1,1,1,1,1,1,1,1,1,1,1,
1,1,1,1,1,1,1,1,1,1,1,1,1,1,1,1,1,1,1,1,1,1,1,1,1,1,1,1,1,1,1,1,1,1,1,1,
1,1,1,1,1,1,1,1,1,1,1,1,1,1,1,1,1,1,1,1,1,1,1,1,1,1,1,1,1,1,1,1,1,1,1,1,
1,1,1,1,1,1,1,1,1,1,1,1,1,1,1,1,1,1,1,1,1,1,1,1,1,1,1,1,1,1,1,1,1,1,1,1,
1,1,1,1,1,1,1,1,1,1,1,1,1,1,1,1,1,1,1,1,1,1,1,1,1,1,1,1,1,1,1,1,1,1,1,1,
1,1,1,1,1,1,1,1,1,1,1,1,1,1,1,1,1,1,1,1,1,1,1,1,1,1,1,1,1,1,1,1,1,1,1,1,
1,1,1,1,1,1,1,1,1,1,1,1,1,1,1,1,1,1,1,1,1,1,1,1,1,1,1,1,1,1,1,1,1,1,1,1,
1,1,1,1,1,1,1,1,1,1,1,1,1,1,1,1,1,1,1,1,1,1,1,1,1,1,1,1,1,1,1,1,1,1,1,1,
1,1,1,1,1,1,1,1,1,1,1,1,1,1,1,1,1,1,1,1,1,1,1,1,1,1,1,1,1,1,1,1,1,1,1,1,
1,1,1,1,1,1,1,1,1,1,1,1,1,1,1,1,1,1,1,1,1,1,1,1,4),(0.,0.0329955678841869),
(8.30203615430915,9.30161085392915,10.3011855535492,11.3007602531692,12.3003349527892,
13.2999096524091,14.2994843520291,15.2990590516491,16.2986337512691,17.2982084508891,
18.2977831505091,19.2973578501291,20.2969325497491,21.2965072493691,22.2960819489891,
23.2956566486091,24.2952313482291,25.2948060478491,26.2943807474691,27.2939554470891,
28.2935301467091,29.2931048463291,30.2926795459491,31.2922542455691,32.2918289451891,
33.2914036448091,34.2909783444291,35.2905530440491,36.2901277436691,37.2897024432891,
38.2892771429091,39.2888518425291,40.2884265421491,41.2880012417691,42.2875759413891,
43.2871506410091,44.2867253406291,45.2863000402491,46.2858747398691,47.2854494394891,
48.2850241391091,49.2845988387291,50.2841735383491,51.2837482379691,52.2833229375891,
53.2828976372091,54.2824723368291,55.2820470364491,56.2816217360691,57.2811964356891,
58.2807711353091,59.2803458349291,60.2799205345491,61.2794952341691,62.2790699337891,
63.2786446334091,64.2782193330291,65.2777940326491,66.2773687322691,67.2769434318891,
68.2765181315091,69.2760928311291,70.2756675307491,71.2752422303691,72.2748169299891,
73.2743916296091,74.2739663292291,75.2735410288491,76.2731157284691,77.2726904280891,
78.2722651277091,79.2718398273291,80.2714145269491,81.2709892265691,82.2705639261891,
83.2701386258091,84.2697133254291,85.2692880250491,86.2688627246691,87.2684374242891,
88.2680121239091,89.2675868235291,90.2671615231491,91.2667362227691,92.2663109223891,
93.2658856220091,94.265460321629,95.265035021249,96.264609720869,97.264184420489,
98.2637591201091,99.2633338197291,100.262908519349,101.262483218969,102.262057918589,
103.261632618209,104.261207317829,105.260782017449,106.260356717069,107.259931416689,
108.259506116309,109.259080815929,110.258655515549,111.258230215169,112.257804914789,
113.257379614409,114.256954314029,115.256529013649,116.256103713269,117.255678412889,
118.255253112509,119.254827812129,120.254402511749,121.253977211369,122.253551910989,
123.253126610609,124.252701310229,125.252276009849,126.251850709469,127.251425409089,
128.251000108709,129.250574808329,130.250149507949,131.249724207569,132.249298907189,
133.248873606809,134.248448306429,135.248023006049,136.247597705669,137.247172405289,
138.246747104909,139.246321804529,140.245896504149,141.245471203769,142.245045903389,
143.244620603009,144.244195302629,145.243770002249,146.243344701869,147.242919401489,
148.242494101109,149.242068800729,150.241643500349,151.241218199969,152.240792899589,
153.240367599209,154.239942298829,155.239516998449,156.239091698069,157.238666397689,
158.238241097309,159.237815796929,160.237390496549,161.236965196169,162.236539895789,
163.236114595409,164.235689295029,165.235263994649,166.234838694269,167.234413393889,
168.233988093509,169.233562793129,170.233137492749,171.232712192369,172.232286891989,
173.231861591609,174.231436291229,175.231010990849,176.230585690469,177.230160390089,
178.229735089709,179.229309789329,180.228884488949,181.228459188569,182.228033888189,
183.227608587809,184.227183287429,185.226757987049,186.226332686669,187.225907386289,
188.225482085909,189.225056785529,190.224631485149,191.224206184769,192.223780884389,
193.223355584009,194.222930283629,195.222504983249,196.222079682869,197.221654382489,
198.221229082109,199.220803781729,200.220378481349,201.219953180969,202.219527880589,
203.219102580209,204.218677279829,205.218251979449,206.217826679069,207.217401378689,
208.216976078309,209.216550777929,210.216125477549,211.215700177169,212.215274876789,
213.214849576409,214.214424276029,215.213998975649,216.213573675269,217.213148374889,
218.212723074509,219.212297774129,220.211872473749,221.211447173369,222.211021872989,
223.210596572609,224.210171272229,225.209745971849,226.209320671469,227.208895371089,
228.208470070709,229.208044770329,230.207619469949,231.207194169569,232.206768869189,
233.206343568809,234.205918268429,235.205492968049,236.205067667669,237.204642367289,
238.204217066909,239.203791766529,240.203366466149,241.202941165769,242.202515865389,
243.202090565009,244.201665264629,245.201239964249,246.200814663869,247.200389363489,
248.199964063109,249.199538762729,250.199113462349,251.198688161969,252.198262861589,
253.197837561209,254.197412260829,255.196986960449,256.196561660069,257.196136359689,
258.195711059309,259.195285758929,260.194860458549,261.194435158169,262.194009857789,
263.193584557409,264.193159257029,265.192733956649,266.192308656269,267.191883355889,
268.191458055509,269.191032755129,270.190607454749,271.190182154369,272.189756853989,
273.189331553609,274.188906253229,275.188480952849,276.188055652469,277.187630352089,
278.187205051709,279.186779751329,280.186354450949,281.185929150569,282.185503850189,
283.185078549809,284.184653249429,285.184227949049,286.183802648669,287.183377348289,
288.182952047909,289.182526747529,290.182101447149,291.181676146769,292.181250846389,
293.180825546009,294.180400245629,295.179974945249,296.179549644869,297.179124344489,
298.178699044109,299.178273743729,300.177848443349,301.177423142969,302.176997842589,
303.176572542209,304.176147241829,305.175721941449,306.175296641069,307.174871340689,
308.174446040309,309.174020739929,310.173595439549,311.173170139169,312.172744838789,
313.172319538409,314.171894238029,315.171468937649,316.171043637269,317.170618336889,
318.170193036509,319.169767736129,320.169342435749,321.168917135369,322.168491834989,
323.168066534609,324.167641234229,325.167215933849,326.166790633469,327.166365333089,
328.165940032709,329.165514732329,330.165089431949,331.164664131569,332.164238831189,
333.163813530809,334.163388230429,335.162962930049,336.162537629669,337.162112329289,
338.161687028909,339.161261728529,340.160836428149,341.160411127769,342.159985827389,
343.159560527009,344.159135226629,345.158709926249,346.158284625869,347.157859325489,
348.157434025109,349.157008724729,350.156583424349,351.156158123969,352.155732823589,
353.155307523209,354.154882222829,355.154456922449,356.154031622069,357.153606321689,
358.153181021309,359.152755720929,360.152330420549,361.151905120169,362.151479819789,
363.151054519409,364.150629219029,365.150203918649,366.149778618269,367.149353317889,
368.148928017509,369.148502717129,370.148077416749,371.147652116369,372.147226815989,
373.146801515609,374.146376215229,375.145950914849,376.145525614469,377.145100314089,
378.144675013709,379.144249713329,380.143824412949,381.143399112569,382.142973812189,
383.142548511809,384.142123211429,385.141697911049,386.141272610669,387.140847310289,
388.140422009909,389.139996709529,390.139571409149,391.139146108769,392.138720808389,
393.138295508009,394.137870207629,395.137444907249,396.137019606869,397.136594306489,
398.136169006109,399.135743705729,400.135318405349,401.134893104969,402.134467804589,
403.134042504209,404.133617203829,405.133191903449,406.132766603069,407.132341302689,
408.131916002309,409.131490701929,410.131065401549,411.130640101169,412.130214800789,
413.129789500409,414.129364200029,415.128938899649,416.128513599269,417.128088298889,
418.127662998509,419.127237698129,420.126812397749,421.126387097369,422.125961796989,
423.125536496609,424.125111196229,425.124685895849,426.124260595469,427.123835295089,
428.123409994709,429.122984694329,430.122559393949,431.122134093569,432.121708793189,
433.121283492809,434.120858192429,435.120432892049,436.120007591669,437.119582291289,
438.119156990909,439.118731690529,440.118306390149,441.117881089769,442.117455789389,
443.117030489009),.UNSPECIFIED.);
#425=B_SPLINE_SURFACE_WITH_KNOTS('',3,3,((#63219,#63220,#63221,#63222,#63223,
#63224,#63225,#63226,#63227,#63228,#63229,#63230,#63231,#63232,#63233,#63234,
#63235,#63236,#63237,#63238,#63239,#63240,#63241,#63242,#63243,#63244,#63245,
#63246,#63247,#63248,#63249,#63250,#63251,#63252,#63253,#63254,#63255,#63256,
#63257,#63258,#63259,#63260,#63261,#63262,#63263,#63264,#63265,#63266,#63267,
#63268,#63269,#63270,#63271,#63272,#63273,#63274,#63275,#63276,#63277,#63278,
#63279,#63280,#63281,#63282,#63283,#63284,#63285,#63286,#63287,#63288,#63289,
#63290,#63291,#63292,#63293,#63294,#63295,#63296,#63297,#63298,#63299,#63300,
#63301,#63302,#63303,#63304,#63305,#63306,#63307,#63308,#63309,#63310,#63311,
#63312,#63313,#63314,#63315,#63316,#63317,#63318,#63319,#63320,#63321,#63322,
#63323,#63324,#63325,#63326,#63327,#63328,#63329,#63330,#63331,#63332,#63333,
#63334,#63335,#63336,#63337,#63338,#63339,#63340,#63341,#63342,#63343,#63344,
#63345,#63346,#63347,#63348,#63349,#63350,#63351,#63352,#63353,#63354,#63355,
#63356,#63357,#63358,#63359,#63360,#63361,#63362,#63363,#63364,#63365,#63366,
#63367,#63368,#63369,#63370,#63371,#63372,#63373,#63374,#63375,#63376,#63377,
#63378,#63379,#63380,#63381,#63382,#63383,#63384,#63385,#63386,#63387,#63388,
#63389,#63390,#63391,#63392,#63393,#63394,#63395,#63396,#63397,#63398,#63399,
#63400,#63401,#63402,#63403,#63404,#63405,#63406,#63407,#63408,#63409,#63410,
#63411,#63412,#63413,#63414,#63415,#63416,#63417,#63418,#63419,#63420,#63421,
#63422,#63423,#63424,#63425,#63426,#63427,#63428,#63429,#63430,#63431,#63432,
#63433,#63434,#63435,#63436,#63437,#63438,#63439,#63440,#63441,#63442,#63443,
#63444,#63445,#63446,#63447,#63448,#63449,#63450,#63451,#63452,#63453,#63454,
#63455,#63456,#63457,#63458,#63459,#63460,#63461,#63462,#63463,#63464,#63465,
#63466,#63467,#63468,#63469,#63470,#63471,#63472,#63473,#63474,#63475,#63476,
#63477,#63478,#63479,#63480,#63481,#63482,#63483,#63484,#63485,#63486,#63487,
#63488,#63489,#63490,#63491,#63492,#63493,#63494,#63495,#63496,#63497,#63498,
#63499,#63500,#63501,#63502,#63503,#63504,#63505,#63506,#63507,#63508,#63509,
#63510,#63511,#63512,#63513,#63514,#63515,#63516,#63517,#63518,#63519,#63520,
#63521,#63522,#63523,#63524,#63525,#63526,#63527,#63528,#63529,#63530,#63531,
#63532,#63533,#63534,#63535,#63536,#63537,#63538,#63539,#63540,#63541,#63542,
#63543,#63544,#63545,#63546,#63547,#63548,#63549,#63550,#63551,#63552,#63553,
#63554,#63555,#63556,#63557,#63558,#63559,#63560,#63561,#63562,#63563,#63564,
#63565,#63566,#63567,#63568,#63569,#63570,#63571,#63572,#63573,#63574,#63575,
#63576,#63577,#63578,#63579,#63580,#63581,#63582,#63583,#63584,#63585,#63586,
#63587,#63588,#63589,#63590,#63591,#63592,#63593,#63594,#63595,#63596,#63597,
#63598,#63599,#63600,#63601,#63602,#63603,#63604,#63605,#63606,#63607,#63608,
#63609,#63610,#63611,#63612,#63613,#63614,#63615,#63616,#63617,#63618,#63619,
#63620,#63621,#63622,#63623,#63624,#63625,#63626,#63627,#63628,#63629,#63630,
#63631,#63632,#63633,#63634,#63635,#63636,#63637,#63638,#63639,#63640,#63641,
#63642,#63643,#63644,#63645,#63646,#63647,#63648,#63649,#63650,#63651,#63652,
#63653,#63654,#63655,#63656),(#63657,#63658,#63659,#63660,#63661,#63662,
#63663,#63664,#63665,#63666,#63667,#63668,#63669,#63670,#63671,#63672,#63673,
#63674,#63675,#63676,#63677,#63678,#63679,#63680,#63681,#63682,#63683,#63684,
#63685,#63686,#63687,#63688,#63689,#63690,#63691,#63692,#63693,#63694,#63695,
#63696,#63697,#63698,#63699,#63700,#63701,#63702,#63703,#63704,#63705,#63706,
#63707,#63708,#63709,#63710,#63711,#63712,#63713,#63714,#63715,#63716,#63717,
#63718,#63719,#63720,#63721,#63722,#63723,#63724,#63725,#63726,#63727,#63728,
#63729,#63730,#63731,#63732,#63733,#63734,#63735,#63736,#63737,#63738,#63739,
#63740,#63741,#63742,#63743,#63744,#63745,#63746,#63747,#63748,#63749,#63750,
#63751,#63752,#63753,#63754,#63755,#63756,#63757,#63758,#63759,#63760,#63761,
#63762,#63763,#63764,#63765,#63766,#63767,#63768,#63769,#63770,#63771,#63772,
#63773,#63774,#63775,#63776,#63777,#63778,#63779,#63780,#63781,#63782,#63783,
#63784,#63785,#63786,#63787,#63788,#63789,#63790,#63791,#63792,#63793,#63794,
#63795,#63796,#63797,#63798,#63799,#63800,#63801,#63802,#63803,#63804,#63805,
#63806,#63807,#63808,#63809,#63810,#63811,#63812,#63813,#63814,#63815,#63816,
#63817,#63818,#63819,#63820,#63821,#63822,#63823,#63824,#63825,#63826,#63827,
#63828,#63829,#63830,#63831,#63832,#63833,#63834,#63835,#63836,#63837,#63838,
#63839,#63840,#63841,#63842,#63843,#63844,#63845,#63846,#63847,#63848,#63849,
#63850,#63851,#63852,#63853,#63854,#63855,#63856,#63857,#63858,#63859,#63860,
#63861,#63862,#63863,#63864,#63865,#63866,#63867,#63868,#63869,#63870,#63871,
#63872,#63873,#63874,#63875,#63876,#63877,#63878,#63879,#63880,#63881,#63882,
#63883,#63884,#63885,#63886,#63887,#63888,#63889,#63890,#63891,#63892,#63893,
#63894,#63895,#63896,#63897,#63898,#63899,#63900,#63901,#63902,#63903,#63904,
#63905,#63906,#63907,#63908,#63909,#63910,#63911,#63912,#63913,#63914,#63915,
#63916,#63917,#63918,#63919,#63920,#63921,#63922,#63923,#63924,#63925,#63926,
#63927,#63928,#63929,#63930,#63931,#63932,#63933,#63934,#63935,#63936,#63937,
#63938,#63939,#63940,#63941,#63942,#63943,#63944,#63945,#63946,#63947,#63948,
#63949,#63950,#63951,#63952,#63953,#63954,#63955,#63956,#63957,#63958,#63959,
#63960,#63961,#63962,#63963,#63964,#63965,#63966,#63967,#63968,#63969,#63970,
#63971,#63972,#63973,#63974,#63975,#63976,#63977,#63978,#63979,#63980,#63981,
#63982,#63983,#63984,#63985,#63986,#63987,#63988,#63989,#63990,#63991,#63992,
#63993,#63994,#63995,#63996,#63997,#63998,#63999,#64000,#64001,#64002,#64003,
#64004,#64005,#64006,#64007,#64008,#64009,#64010,#64011,#64012,#64013,#64014,
#64015,#64016,#64017,#64018,#64019,#64020,#64021,#64022,#64023,#64024,#64025,
#64026,#64027,#64028,#64029,#64030,#64031,#64032,#64033,#64034,#64035,#64036,
#64037,#64038,#64039,#64040,#64041,#64042,#64043,#64044,#64045,#64046,#64047,
#64048,#64049,#64050,#64051,#64052,#64053,#64054,#64055,#64056,#64057,#64058,
#64059,#64060,#64061,#64062,#64063,#64064,#64065,#64066,#64067,#64068,#64069,
#64070,#64071,#64072,#64073,#64074,#64075,#64076,#64077,#64078,#64079,#64080,
#64081,#64082,#64083,#64084,#64085,#64086,#64087,#64088,#64089,#64090,#64091,
#64092,#64093,#64094),(#64095,#64096,#64097,#64098,#64099,#64100,#64101,
#64102,#64103,#64104,#64105,#64106,#64107,#64108,#64109,#64110,#64111,#64112,
#64113,#64114,#64115,#64116,#64117,#64118,#64119,#64120,#64121,#64122,#64123,
#64124,#64125,#64126,#64127,#64128,#64129,#64130,#64131,#64132,#64133,#64134,
#64135,#64136,#64137,#64138,#64139,#64140,#64141,#64142,#64143,#64144,#64145,
#64146,#64147,#64148,#64149,#64150,#64151,#64152,#64153,#64154,#64155,#64156,
#64157,#64158,#64159,#64160,#64161,#64162,#64163,#64164,#64165,#64166,#64167,
#64168,#64169,#64170,#64171,#64172,#64173,#64174,#64175,#64176,#64177,#64178,
#64179,#64180,#64181,#64182,#64183,#64184,#64185,#64186,#64187,#64188,#64189,
#64190,#64191,#64192,#64193,#64194,#64195,#64196,#64197,#64198,#64199,#64200,
#64201,#64202,#64203,#64204,#64205,#64206,#64207,#64208,#64209,#64210,#64211,
#64212,#64213,#64214,#64215,#64216,#64217,#64218,#64219,#64220,#64221,#64222,
#64223,#64224,#64225,#64226,#64227,#64228,#64229,#64230,#64231,#64232,#64233,
#64234,#64235,#64236,#64237,#64238,#64239,#64240,#64241,#64242,#64243,#64244,
#64245,#64246,#64247,#64248,#64249,#64250,#64251,#64252,#64253,#64254,#64255,
#64256,#64257,#64258,#64259,#64260,#64261,#64262,#64263,#64264,#64265,#64266,
#64267,#64268,#64269,#64270,#64271,#64272,#64273,#64274,#64275,#64276,#64277,
#64278,#64279,#64280,#64281,#64282,#64283,#64284,#64285,#64286,#64287,#64288,
#64289,#64290,#64291,#64292,#64293,#64294,#64295,#64296,#64297,#64298,#64299,
#64300,#64301,#64302,#64303,#64304,#64305,#64306,#64307,#64308,#64309,#64310,
#64311,#64312,#64313,#64314,#64315,#64316,#64317,#64318,#64319,#64320,#64321,
#64322,#64323,#64324,#64325,#64326,#64327,#64328,#64329,#64330,#64331,#64332,
#64333,#64334,#64335,#64336,#64337,#64338,#64339,#64340,#64341,#64342,#64343,
#64344,#64345,#64346,#64347,#64348,#64349,#64350,#64351,#64352,#64353,#64354,
#64355,#64356,#64357,#64358,#64359,#64360,#64361,#64362,#64363,#64364,#64365,
#64366,#64367,#64368,#64369,#64370,#64371,#64372,#64373,#64374,#64375,#64376,
#64377,#64378,#64379,#64380,#64381,#64382,#64383,#64384,#64385,#64386,#64387,
#64388,#64389,#64390,#64391,#64392,#64393,#64394,#64395,#64396,#64397,#64398,
#64399,#64400,#64401,#64402,#64403,#64404,#64405,#64406,#64407,#64408,#64409,
#64410,#64411,#64412,#64413,#64414,#64415,#64416,#64417,#64418,#64419,#64420,
#64421,#64422,#64423,#64424,#64425,#64426,#64427,#64428,#64429,#64430,#64431,
#64432,#64433,#64434,#64435,#64436,#64437,#64438,#64439,#64440,#64441,#64442,
#64443,#64444,#64445,#64446,#64447,#64448,#64449,#64450,#64451,#64452,#64453,
#64454,#64455,#64456,#64457,#64458,#64459,#64460,#64461,#64462,#64463,#64464,
#64465,#64466,#64467,#64468,#64469,#64470,#64471,#64472,#64473,#64474,#64475,
#64476,#64477,#64478,#64479,#64480,#64481,#64482,#64483,#64484,#64485,#64486,
#64487,#64488,#64489,#64490,#64491,#64492,#64493,#64494,#64495,#64496,#64497,
#64498,#64499,#64500,#64501,#64502,#64503,#64504,#64505,#64506,#64507,#64508,
#64509,#64510,#64511,#64512,#64513,#64514,#64515,#64516,#64517,#64518,#64519,
#64520,#64521,#64522,#64523,#64524,#64525,#64526,#64527,#64528,#64529,#64530,
#64531,#64532),(#64533,#64534,#64535,#64536,#64537,#64538,#64539,#64540,
#64541,#64542,#64543,#64544,#64545,#64546,#64547,#64548,#64549,#64550,#64551,
#64552,#64553,#64554,#64555,#64556,#64557,#64558,#64559,#64560,#64561,#64562,
#64563,#64564,#64565,#64566,#64567,#64568,#64569,#64570,#64571,#64572,#64573,
#64574,#64575,#64576,#64577,#64578,#64579,#64580,#64581,#64582,#64583,#64584,
#64585,#64586,#64587,#64588,#64589,#64590,#64591,#64592,#64593,#64594,#64595,
#64596,#64597,#64598,#64599,#64600,#64601,#64602,#64603,#64604,#64605,#64606,
#64607,#64608,#64609,#64610,#64611,#64612,#64613,#64614,#64615,#64616,#64617,
#64618,#64619,#64620,#64621,#64622,#64623,#64624,#64625,#64626,#64627,#64628,
#64629,#64630,#64631,#64632,#64633,#64634,#64635,#64636,#64637,#64638,#64639,
#64640,#64641,#64642,#64643,#64644,#64645,#64646,#64647,#64648,#64649,#64650,
#64651,#64652,#64653,#64654,#64655,#64656,#64657,#64658,#64659,#64660,#64661,
#64662,#64663,#64664,#64665,#64666,#64667,#64668,#64669,#64670,#64671,#64672,
#64673,#64674,#64675,#64676,#64677,#64678,#64679,#64680,#64681,#64682,#64683,
#64684,#64685,#64686,#64687,#64688,#64689,#64690,#64691,#64692,#64693,#64694,
#64695,#64696,#64697,#64698,#64699,#64700,#64701,#64702,#64703,#64704,#64705,
#64706,#64707,#64708,#64709,#64710,#64711,#64712,#64713,#64714,#64715,#64716,
#64717,#64718,#64719,#64720,#64721,#64722,#64723,#64724,#64725,#64726,#64727,
#64728,#64729,#64730,#64731,#64732,#64733,#64734,#64735,#64736,#64737,#64738,
#64739,#64740,#64741,#64742,#64743,#64744,#64745,#64746,#64747,#64748,#64749,
#64750,#64751,#64752,#64753,#64754,#64755,#64756,#64757,#64758,#64759,#64760,
#64761,#64762,#64763,#64764,#64765,#64766,#64767,#64768,#64769,#64770,#64771,
#64772,#64773,#64774,#64775,#64776,#64777,#64778,#64779,#64780,#64781,#64782,
#64783,#64784,#64785,#64786,#64787,#64788,#64789,#64790,#64791,#64792,#64793,
#64794,#64795,#64796,#64797,#64798,#64799,#64800,#64801,#64802,#64803,#64804,
#64805,#64806,#64807,#64808,#64809,#64810,#64811,#64812,#64813,#64814,#64815,
#64816,#64817,#64818,#64819,#64820,#64821,#64822,#64823,#64824,#64825,#64826,
#64827,#64828,#64829,#64830,#64831,#64832,#64833,#64834,#64835,#64836,#64837,
#64838,#64839,#64840,#64841,#64842,#64843,#64844,#64845,#64846,#64847,#64848,
#64849,#64850,#64851,#64852,#64853,#64854,#64855,#64856,#64857,#64858,#64859,
#64860,#64861,#64862,#64863,#64864,#64865,#64866,#64867,#64868,#64869,#64870,
#64871,#64872,#64873,#64874,#64875,#64876,#64877,#64878,#64879,#64880,#64881,
#64882,#64883,#64884,#64885,#64886,#64887,#64888,#64889,#64890,#64891,#64892,
#64893,#64894,#64895,#64896,#64897,#64898,#64899,#64900,#64901,#64902,#64903,
#64904,#64905,#64906,#64907,#64908,#64909,#64910,#64911,#64912,#64913,#64914,
#64915,#64916,#64917,#64918,#64919,#64920,#64921,#64922,#64923,#64924,#64925,
#64926,#64927,#64928,#64929,#64930,#64931,#64932,#64933,#64934,#64935,#64936,
#64937,#64938,#64939,#64940,#64941,#64942,#64943,#64944,#64945,#64946,#64947,
#64948,#64949,#64950,#64951,#64952,#64953,#64954,#64955,#64956,#64957,#64958,
#64959,#64960,#64961,#64962,#64963,#64964,#64965,#64966,#64967,#64968,#64969,
#64970)),.UNSPECIFIED.,.F.,.F.,.F.,(4,4),(4,1,1,1,1,1,1,1,1,1,1,1,1,1,1,
1,1,1,1,1,1,1,1,1,1,1,1,1,1,1,1,1,1,1,1,1,1,1,1,1,1,1,1,1,1,1,1,1,1,1,1,
1,1,1,1,1,1,1,1,1,1,1,1,1,1,1,1,1,1,1,1,1,1,1,1,1,1,1,1,1,1,1,1,1,1,1,1,
1,1,1,1,1,1,1,1,1,1,1,1,1,1,1,1,1,1,1,1,1,1,1,1,1,1,1,1,1,1,1,1,1,1,1,1,
1,1,1,1,1,1,1,1,1,1,1,1,1,1,1,1,1,1,1,1,1,1,1,1,1,1,1,1,1,1,1,1,1,1,1,1,
1,1,1,1,1,1,1,1,1,1,1,1,1,1,1,1,1,1,1,1,1,1,1,1,1,1,1,1,1,1,1,1,1,1,1,1,
1,1,1,1,1,1,1,1,1,1,1,1,1,1,1,1,1,1,1,1,1,1,1,1,1,1,1,1,1,1,1,1,1,1,1,1,
1,1,1,1,1,1,1,1,1,1,1,1,1,1,1,1,1,1,1,1,1,1,1,1,1,1,1,1,1,1,1,1,1,1,1,1,
1,1,1,1,1,1,1,1,1,1,1,1,1,1,1,1,1,1,1,1,1,1,1,1,1,1,1,1,1,1,1,1,1,1,1,1,
1,1,1,1,1,1,1,1,1,1,1,1,1,1,1,1,1,1,1,1,1,1,1,1,1,1,1,1,1,1,1,1,1,1,1,1,
1,1,1,1,1,1,1,1,1,1,1,1,1,1,1,1,1,1,1,1,1,1,1,1,1,1,1,1,1,1,1,1,1,1,1,1,
1,1,1,1,1,1,1,1,1,1,1,1,1,1,1,1,1,1,1,1,1,1,1,1,1,1,1,1,1,1,1,1,1,1,1,1,
1,1,1,1,1,1,1,1,1,1,1,1,1,1,1,1,1,1,1,1,1,1,1,1,4),(0.,0.0329955678841869),
(11.6159397475014,12.6155144471214,13.6150891467414,14.6146638463614,15.6142385459814,
16.6138132456014,17.6133879452214,18.6129626448414,19.6125373444614,20.6121120440814,
21.6116867437014,22.6112614433214,23.6108361429414,24.6104108425614,25.6099855421814,
26.6095602418014,27.6091349414214,28.6087096410414,29.6082843406614,30.6078590402814,
31.6074337399014,32.6070084395214,33.6065831391414,34.6061578387614,35.6057325383814,
36.6053072380014,37.6048819376214,38.6044566372414,39.6040313368614,40.6036060364814,
41.6031807361014,42.6027554357214,43.6023301353414,44.6019048349614,45.6014795345814,
46.6010542342014,47.6006289338214,48.6002036334414,49.5997783330614,50.5993530326813,
51.5989277323013,52.5985024319213,53.5980771315413,54.5976518311613,55.5972265307813,
56.5968012304013,57.5963759300213,58.5959506296413,59.5955253292613,60.5951000288813,
61.5946747285013,62.5942494281213,63.5938241277413,64.5933988273613,65.5929735269813,
66.5925482266013,67.5921229262213,68.5916976258413,69.5912723254613,70.5908470250813,
71.5904217247013,72.5899964243213,73.5895711239413,74.5891458235613,75.5887205231813,
76.5882952228013,77.5878699224213,78.5874446220413,79.5870193216613,80.5865940212813,
81.5861687209013,82.5857434205213,83.5853181201413,84.5848928197613,85.5844675193813,
86.5840422190013,87.5836169186213,88.5831916182413,89.5827663178613,90.5823410174813,
91.5819157171013,92.5814904167213,93.5810651163413,94.5806398159613,95.5802145155813,
96.5797892152013,97.5793639148213,98.5789386144413,99.5785133140613,100.578088013681,
101.577662713301,102.577237412921,103.576812112541,104.576386812161,105.575961511781,
106.575536211401,107.575110911021,108.574685610641,109.574260310261,110.573835009881,
111.573409709501,112.572984409121,113.572559108741,114.572133808361,115.571708507981,
116.571283207601,117.570857907221,118.570432606841,119.570007306461,120.569582006081,
121.569156705701,122.568731405321,123.568306104941,124.567880804561,125.567455504181,
126.567030203801,127.566604903421,128.566179603041,129.565754302661,130.565329002281,
131.564903701901,132.564478401521,133.564053101141,134.563627800761,135.563202500381,
136.562777200001,137.562351899621,138.561926599241,139.561501298861,140.561075998481,
141.560650698101,142.560225397721,143.559800097341,144.559374796961,145.558949496581,
146.558524196201,147.558098895821,148.557673595441,149.557248295061,150.556822994681,
151.556397694301,152.555972393921,153.555547093541,154.555121793161,155.554696492781,
156.554271192401,157.553845892021,158.553420591641,159.552995291261,160.552569990881,
161.552144690501,162.551719390121,163.551294089741,164.550868789361,165.550443488981,
166.550018188601,167.549592888221,168.549167587841,169.548742287461,170.548316987081,
171.547891686701,172.547466386321,173.547041085941,174.546615785561,175.546190485181,
176.545765184801,177.545339884421,178.544914584041,179.544489283661,180.544063983281,
181.543638682901,182.543213382521,183.542788082141,184.542362781761,185.541937481381,
186.541512181001,187.541086880621,188.540661580241,189.540236279861,190.539810979481,
191.539385679101,192.538960378721,193.538535078341,194.538109777961,195.537684477581,
196.537259177201,197.536833876821,198.536408576441,199.535983276061,200.535557975681,
201.535132675301,202.534707374921,203.534282074541,204.533856774161,205.533431473781,
206.533006173401,207.532580873021,208.532155572641,209.531730272261,210.531304971881,
211.530879671501,212.530454371121,213.530029070741,214.529603770361,215.529178469981,
216.528753169601,217.528327869221,218.527902568841,219.527477268461,220.527051968081,
221.526626667701,222.526201367321,223.525776066941,224.525350766561,225.524925466181,
226.524500165801,227.524074865421,228.523649565041,229.523224264661,230.522798964281,
231.522373663901,232.521948363521,233.521523063141,234.521097762761,235.520672462381,
236.520247162001,237.519821861621,238.519396561241,239.518971260861,240.518545960481,
241.518120660101,242.517695359721,243.517270059341,244.516844758961,245.516419458581,
246.515994158201,247.515568857821,248.515143557441,249.514718257061,250.514292956681,
251.513867656301,252.513442355921,253.513017055541,254.512591755161,255.512166454781,
256.511741154401,257.511315854021,258.510890553641,259.510465253261,260.510039952881,
261.509614652501,262.509189352121,263.508764051741,264.508338751361,265.507913450981,
266.507488150601,267.507062850221,268.506637549841,269.506212249461,270.505786949081,
271.505361648701,272.504936348321,273.504511047941,274.504085747561,275.503660447181,
276.503235146801,277.502809846421,278.502384546041,279.501959245661,280.501533945281,
281.501108644901,282.500683344521,283.500258044141,284.499832743761,285.499407443381,
286.498982143001,287.498556842621,288.498131542241,289.497706241861,290.497280941481,
291.496855641101,292.496430340721,293.496005040341,294.495579739961,295.495154439581,
296.494729139201,297.494303838821,298.493878538441,299.493453238061,300.493027937681,
301.492602637301,302.492177336921,303.491752036541,304.491326736161,305.490901435781,
306.490476135401,307.490050835021,308.489625534641,309.489200234261,310.488774933881,
311.488349633501,312.487924333121,313.487499032741,314.487073732361,315.486648431981,
316.486223131601,317.485797831221,318.485372530841,319.484947230461,320.484521930081,
321.484096629701,322.483671329321,323.483246028941,324.482820728561,325.482395428181,
326.481970127801,327.481544827421,328.481119527041,329.480694226661,330.480268926281,
331.479843625901,332.479418325521,333.478993025141,334.478567724761,335.478142424381,
336.477717124001,337.477291823621,338.476866523241,339.476441222861,340.476015922481,
341.475590622101,342.475165321721,343.474740021341,344.474314720961,345.473889420581,
346.473464120201,347.473038819821,348.472613519441,349.472188219061,350.471762918681,
351.471337618301,352.470912317921,353.470487017541,354.470061717161,355.469636416781,
356.469211116401,357.468785816021,358.468360515641,359.467935215261,360.467509914881,
361.467084614501,362.466659314121,363.466234013741,364.465808713361,365.465383412981,
366.464958112601,367.464532812221,368.464107511841,369.463682211461,370.463256911081,
371.462831610701,372.462406310321,373.461981009941,374.461555709561,375.461130409181,
376.460705108801,377.460279808421,378.459854508041,379.459429207661,380.459003907281,
381.458578606901,382.458153306521,383.457728006141,384.457302705761,385.456877405381,
386.456452105001,387.456026804621,388.455601504241,389.455176203861,390.454750903481,
391.454325603101,392.453900302721,393.453475002341,394.453049701961,395.452624401581,
396.452199101201,397.451773800821,398.451348500441,399.450923200061,400.450497899681,
401.450072599301,402.449647298921,403.449221998541,404.448796698161,405.448371397781,
406.447946097401,407.447520797021,408.447095496641,409.446670196261,410.446244895881,
411.445819595501,412.445394295121,413.444968994741,414.444543694361,415.444118393981,
416.443693093601,417.443267793221,418.442842492841,419.442417192461,420.441991892081,
421.441566591701,422.441141291321,423.440715990941,424.440290690561,425.439865390181,
426.439440089801,427.439014789421,428.438589489041,429.438164188661,430.437738888281,
431.437313587901,432.436888287521,433.436462987141,434.436037686761,435.435612386381,
436.435187086001,437.434761785621,438.434336485241,439.433911184861,440.433485884481,
441.433060584101,442.432635283721,443.432209983341,444.431784682961,445.431359382581,
446.430934082201),.UNSPECIFIED.);
#426=B_SPLINE_SURFACE_WITH_KNOTS('',3,3,((#68020,#68021,#68022,#68023,#68024,
#68025,#68026,#68027,#68028,#68029,#68030,#68031,#68032,#68033,#68034,#68035,
#68036,#68037,#68038,#68039,#68040,#68041,#68042,#68043,#68044,#68045,#68046),
(#68047,#68048,#68049,#68050,#68051,#68052,#68053,#68054,#68055,#68056,
#68057,#68058,#68059,#68060,#68061,#68062,#68063,#68064,#68065,#68066,#68067,
#68068,#68069,#68070,#68071,#68072,#68073),(#68074,#68075,#68076,#68077,
#68078,#68079,#68080,#68081,#68082,#68083,#68084,#68085,#68086,#68087,#68088,
#68089,#68090,#68091,#68092,#68093,#68094,#68095,#68096,#68097,#68098,#68099,
#68100),(#68101,#68102,#68103,#68104,#68105,#68106,#68107,#68108,#68109,
#68110,#68111,#68112,#68113,#68114,#68115,#68116,#68117,#68118,#68119,#68120,
#68121,#68122,#68123,#68124,#68125,#68126,#68127)),.UNSPECIFIED.,.F.,.T.,
 .F.,(4,4),(4,1,2,1,1,1,2,2,2,1,1,1,1,1,1,1,1,1,1,1,4),(0.,1.),(0.,0.0584568917522064,
0.116913783504413,0.175370117903373,0.233826452302333,0.263054619501813,
0.350739121100252,0.409196012852459,0.467652904604665,0.526109517680248,
0.569951977486936,0.584566130755832,0.672251050369206,0.686865203638102,
0.69417228027255,0.701479356906998,0.774550123251477,0.818392583058164,
0.847620889595956,0.876849196133747,0.93530580920933),.UNSPECIFIED.);
#427=B_SPLINE_SURFACE_WITH_KNOTS('',3,3,((#68199,#68200,#68201,#68202,#68203,
#68204,#68205,#68206,#68207,#68208,#68209,#68210,#68211,#68212,#68213,#68214,
#68215,#68216,#68217,#68218,#68219,#68220,#68221,#68222,#68223,#68224,#68225,
#68226,#68227,#68228,#68229,#68230,#68231,#68232,#68233,#68234,#68235,#68236,
#68237,#68238,#68239,#68240,#68241,#68242,#68243,#68244,#68245,#68246,#68247,
#68248,#68249,#68250,#68251,#68252,#68253,#68254,#68255,#68256,#68257,#68258,
#68259,#68260,#68261,#68262,#68263,#68264,#68265,#68266,#68267,#68268,#68269,
#68270,#68271,#68272,#68273,#68274,#68275,#68276,#68277,#68278,#68279,#68280,
#68281,#68282,#68283,#68284,#68285,#68286,#68287,#68288,#68289,#68290,#68291,
#68292,#68293,#68294,#68295,#68296,#68297,#68298,#68299,#68300,#68301,#68302,
#68303,#68304,#68305,#68306,#68307,#68308,#68309,#68310,#68311,#68312,#68313,
#68314,#68315,#68316,#68317,#68318,#68319,#68320,#68321,#68322,#68323,#68324,
#68325,#68326,#68327,#68328,#68329,#68330,#68331,#68332,#68333,#68334,#68335,
#68336,#68337,#68338,#68339,#68340,#68341,#68342,#68343,#68344,#68345,#68346,
#68347,#68348,#68349,#68350,#68351,#68352,#68353,#68354,#68355,#68356,#68357,
#68358,#68359,#68360,#68361,#68362,#68363,#68364,#68365,#68366,#68367,#68368,
#68369,#68370,#68371,#68372,#68373,#68374,#68375,#68376,#68377,#68378,#68379,
#68380,#68381,#68382,#68383,#68384,#68385,#68386,#68387,#68388,#68389,#68390,
#68391,#68392,#68393,#68394,#68395,#68396,#68397,#68398,#68399,#68400,#68401,
#68402,#68403),(#68404,#68405,#68406,#68407,#68408,#68409,#68410,#68411,
#68412,#68413,#68414,#68415,#68416,#68417,#68418,#68419,#68420,#68421,#68422,
#68423,#68424,#68425,#68426,#68427,#68428,#68429,#68430,#68431,#68432,#68433,
#68434,#68435,#68436,#68437,#68438,#68439,#68440,#68441,#68442,#68443,#68444,
#68445,#68446,#68447,#68448,#68449,#68450,#68451,#68452,#68453,#68454,#68455,
#68456,#68457,#68458,#68459,#68460,#68461,#68462,#68463,#68464,#68465,#68466,
#68467,#68468,#68469,#68470,#68471,#68472,#68473,#68474,#68475,#68476,#68477,
#68478,#68479,#68480,#68481,#68482,#68483,#68484,#68485,#68486,#68487,#68488,
#68489,#68490,#68491,#68492,#68493,#68494,#68495,#68496,#68497,#68498,#68499,
#68500,#68501,#68502,#68503,#68504,#68505,#68506,#68507,#68508,#68509,#68510,
#68511,#68512,#68513,#68514,#68515,#68516,#68517,#68518,#68519,#68520,#68521,
#68522,#68523,#68524,#68525,#68526,#68527,#68528,#68529,#68530,#68531,#68532,
#68533,#68534,#68535,#68536,#68537,#68538,#68539,#68540,#68541,#68542,#68543,
#68544,#68545,#68546,#68547,#68548,#68549,#68550,#68551,#68552,#68553,#68554,
#68555,#68556,#68557,#68558,#68559,#68560,#68561,#68562,#68563,#68564,#68565,
#68566,#68567,#68568,#68569,#68570,#68571,#68572,#68573,#68574,#68575,#68576,
#68577,#68578,#68579,#68580,#68581,#68582,#68583,#68584,#68585,#68586,#68587,
#68588,#68589,#68590,#68591,#68592,#68593,#68594,#68595,#68596,#68597,#68598,
#68599,#68600,#68601,#68602,#68603,#68604,#68605,#68606,#68607,#68608),
(#68609,#68610,#68611,#68612,#68613,#68614,#68615,#68616,#68617,#68618,
#68619,#68620,#68621,#68622,#68623,#68624,#68625,#68626,#68627,#68628,#68629,
#68630,#68631,#68632,#68633,#68634,#68635,#68636,#68637,#68638,#68639,#68640,
#68641,#68642,#68643,#68644,#68645,#68646,#68647,#68648,#68649,#68650,#68651,
#68652,#68653,#68654,#68655,#68656,#68657,#68658,#68659,#68660,#68661,#68662,
#68663,#68664,#68665,#68666,#68667,#68668,#68669,#68670,#68671,#68672,#68673,
#68674,#68675,#68676,#68677,#68678,#68679,#68680,#68681,#68682,#68683,#68684,
#68685,#68686,#68687,#68688,#68689,#68690,#68691,#68692,#68693,#68694,#68695,
#68696,#68697,#68698,#68699,#68700,#68701,#68702,#68703,#68704,#68705,#68706,
#68707,#68708,#68709,#68710,#68711,#68712,#68713,#68714,#68715,#68716,#68717,
#68718,#68719,#68720,#68721,#68722,#68723,#68724,#68725,#68726,#68727,#68728,
#68729,#68730,#68731,#68732,#68733,#68734,#68735,#68736,#68737,#68738,#68739,
#68740,#68741,#68742,#68743,#68744,#68745,#68746,#68747,#68748,#68749,#68750,
#68751,#68752,#68753,#68754,#68755,#68756,#68757,#68758,#68759,#68760,#68761,
#68762,#68763,#68764,#68765,#68766,#68767,#68768,#68769,#68770,#68771,#68772,
#68773,#68774,#68775,#68776,#68777,#68778,#68779,#68780,#68781,#68782,#68783,
#68784,#68785,#68786,#68787,#68788,#68789,#68790,#68791,#68792,#68793,#68794,
#68795,#68796,#68797,#68798,#68799,#68800,#68801,#68802,#68803,#68804,#68805,
#68806,#68807,#68808,#68809,#68810,#68811,#68812,#68813),(#68814,#68815,
#68816,#68817,#68818,#68819,#68820,#68821,#68822,#68823,#68824,#68825,#68826,
#68827,#68828,#68829,#68830,#68831,#68832,#68833,#68834,#68835,#68836,#68837,
#68838,#68839,#68840,#68841,#68842,#68843,#68844,#68845,#68846,#68847,#68848,
#68849,#68850,#68851,#68852,#68853,#68854,#68855,#68856,#68857,#68858,#68859,
#68860,#68861,#68862,#68863,#68864,#68865,#68866,#68867,#68868,#68869,#68870,
#68871,#68872,#68873,#68874,#68875,#68876,#68877,#68878,#68879,#68880,#68881,
#68882,#68883,#68884,#68885,#68886,#68887,#68888,#68889,#68890,#68891,#68892,
#68893,#68894,#68895,#68896,#68897,#68898,#68899,#68900,#68901,#68902,#68903,
#68904,#68905,#68906,#68907,#68908,#68909,#68910,#68911,#68912,#68913,#68914,
#68915,#68916,#68917,#68918,#68919,#68920,#68921,#68922,#68923,#68924,#68925,
#68926,#68927,#68928,#68929,#68930,#68931,#68932,#68933,#68934,#68935,#68936,
#68937,#68938,#68939,#68940,#68941,#68942,#68943,#68944,#68945,#68946,#68947,
#68948,#68949,#68950,#68951,#68952,#68953,#68954,#68955,#68956,#68957,#68958,
#68959,#68960,#68961,#68962,#68963,#68964,#68965,#68966,#68967,#68968,#68969,
#68970,#68971,#68972,#68973,#68974,#68975,#68976,#68977,#68978,#68979,#68980,
#68981,#68982,#68983,#68984,#68985,#68986,#68987,#68988,#68989,#68990,#68991,
#68992,#68993,#68994,#68995,#68996,#68997,#68998,#68999,#69000,#69001,#69002,
#69003,#69004,#69005,#69006,#69007,#69008,#69009,#69010,#69011,#69012,#69013,
#69014,#69015,#69016,#69017,#69018)),.UNSPECIFIED.,.F.,.F.,.F.,(4,4),(4,
1,1,1,1,1,1,1,1,1,1,1,1,1,1,1,1,1,1,1,1,1,1,1,1,1,1,1,1,1,1,1,1,1,1,1,1,
1,1,1,1,1,1,1,1,1,1,1,1,1,1,1,1,1,1,1,1,1,1,1,1,1,1,1,1,1,1,1,1,1,1,1,1,
1,1,1,1,1,1,1,1,1,1,1,1,1,1,1,1,1,1,1,1,1,1,1,1,1,1,1,1,1,1,1,1,1,1,1,1,
1,1,1,1,1,1,1,1,1,1,1,1,1,1,1,1,1,1,1,1,1,1,1,1,1,1,1,1,1,1,1,1,1,1,1,1,
1,1,1,1,1,1,1,1,1,1,1,1,1,1,1,1,1,1,1,1,1,1,1,1,1,1,1,1,1,1,1,1,1,1,1,1,
1,1,1,1,1,1,1,1,1,1,1,1,1,1,1,1,1,1,1,1,1,4),(0.,0.0824167509268191),(8.30472057736738,
8.80312233880653,9.30152410024569,9.79992586168484,10.298327623124,10.7967293845631,
11.2951311460023,11.7935329074415,12.2919346688806,12.7903364303198,13.2887381917589,
13.7871399531981,14.2855417146372,14.7839434760764,15.2823452375155,15.7807469989547,
16.2791487603938,16.777550521833,17.2759522832721,17.7743540447113,18.2727558061505,
18.7711575675896,19.2695593290288,19.7679610904679,20.2663628519071,20.7647646133462,
21.2631663747854,21.7615681362245,22.2599698976637,22.7583716591028,23.256773420542,
23.7551751819811,24.2535769434203,24.7519787048595,25.2503804662986,25.7487822277378,
26.2471839891769,26.7455857506161,27.2439875120552,27.7423892734944,28.2407910349335,
28.7391927963727,29.2375945578118,29.735996319251,30.2343980806901,30.7327998421293,
31.2312016035684,31.7296033650076,32.2280051264468,32.7264068878859,33.2248086493251,
33.7232104107642,34.2216121722034,34.7200139336425,35.2184156950817,35.7168174565208,
36.21521921796,36.7136209793991,37.2120227408383,37.7104245022774,38.2088262637166,
38.7072280251558,39.2056297865949,39.7040315480341,40.2024333094732,40.7008350709124,
41.1992368323515,41.6976385937907,42.1960403552298,42.694442116669,43.1928438781081,
43.6912456395473,44.1896474009864,44.6880491624256,45.1864509238648,45.6848526853039,
46.1832544467431,46.6816562081822,47.1800579696214,47.6784597310605,48.1768614924997,
48.6752632539388,49.173665015378,49.6720667768171,50.1704685382563,50.6688702996954,
51.1672720611346,51.6656738225738,52.1640755840129,52.6624773454521,53.1608791068912,
53.6592808683304,54.1576826297695,54.6560843912087,55.1544861526478,55.652887914087,
56.1512896755261,56.6496914369653,57.1480931984044,57.6464949598436,58.1448967212827,
58.6432984827219,59.1417002441611,59.6401020056002,60.1385037670394,60.6369055284785,
61.1353072899177,61.6337090513568,62.132110812796,62.6305125742351,63.1289143356743,
63.6273160971134,64.1257178585526,64.6241196199917,65.1225213814309,65.6209231428701,
66.1193249043092,66.6177266657484,67.1161284271875,67.6145301886267,68.1129319500658,
68.611333711505,69.1097354729441,69.6081372343833,70.1065389958224,70.6049407572616,
71.1033425187007,71.6017442801399,72.1001460415791,72.5985478030182,73.0969495644573,
73.5953513258965,74.0937530873357,74.5921548487748,75.090556610214,75.5889583716531,
76.0873601330923,76.5857618945314,77.0841636559706,77.5825654174097,78.0809671788489,
78.579368940288,79.0777707017272,79.5761724631663,80.0745742246055,80.5729759860447,
81.0713777474838,81.569779508923,82.0681812703621,82.5665830318013,83.0649847932404,
83.5633865546796,84.0617883161187,84.5601900775579,85.058591838997,85.5569936004362,
86.0553953618753,86.5537971233145,87.0521988847537,87.5506006461928,88.049002407632,
88.5474041690711,89.0458059305103,89.5442076919494,90.0426094533886,90.5410112148277,
91.0394129762669,91.537814737706,92.0362164991452,92.5346182605844,93.0330200220235,
93.5314217834626,94.0298235449018,94.528225306341,95.0266270677801,95.5250288292193,
96.0234305906584,96.5218323520976,97.0202341135367,97.5186358749759,98.017037636415,
98.5154393978542,99.0138411592933,99.5122429207325,100.010644682172,100.509046443611,
101.00744820505,101.505849966489,102.004251727928,102.502653489367,103.001055250807,
103.499457012246,103.997858773685,104.496260535124,104.994662296563,105.493064058002,
105.991465819441,106.489867580881,106.98826934232,107.486671103759,107.985072865198,
108.483474626637,108.981876388076),.UNSPECIFIED.);
#428=B_SPLINE_SURFACE_WITH_KNOTS('',3,3,((#69418,#69419,#69420,#69421,#69422,
#69423,#69424,#69425,#69426,#69427,#69428,#69429,#69430,#69431,#69432,#69433,
#69434,#69435,#69436,#69437,#69438,#69439,#69440,#69441,#69442,#69443,#69444,
#69445,#69446,#69447,#69448,#69449,#69450,#69451,#69452,#69453,#69454,#69455,
#69456,#69457,#69458,#69459,#69460,#69461,#69462,#69463,#69464,#69465,#69466,
#69467,#69468,#69469,#69470,#69471,#69472,#69473,#69474,#69475,#69476,#69477,
#69478,#69479,#69480,#69481,#69482,#69483,#69484,#69485,#69486,#69487,#69488,
#69489,#69490,#69491,#69492,#69493,#69494,#69495,#69496,#69497,#69498,#69499,
#69500,#69501,#69502,#69503,#69504,#69505,#69506,#69507,#69508,#69509,#69510,
#69511,#69512,#69513,#69514,#69515,#69516,#69517,#69518,#69519,#69520,#69521,
#69522,#69523,#69524,#69525,#69526,#69527,#69528,#69529,#69530,#69531,#69532,
#69533,#69534,#69535,#69536,#69537,#69538,#69539,#69540,#69541,#69542,#69543,
#69544,#69545,#69546,#69547,#69548,#69549,#69550,#69551,#69552,#69553,#69554,
#69555,#69556,#69557,#69558,#69559,#69560,#69561,#69562,#69563,#69564,#69565,
#69566,#69567,#69568,#69569,#69570,#69571,#69572,#69573,#69574,#69575,#69576,
#69577,#69578,#69579,#69580,#69581,#69582,#69583,#69584,#69585,#69586,#69587,
#69588,#69589,#69590,#69591,#69592,#69593,#69594,#69595,#69596,#69597,#69598,
#69599,#69600,#69601,#69602,#69603,#69604,#69605,#69606,#69607,#69608,#69609,
#69610,#69611,#69612,#69613,#69614,#69615,#69616,#69617,#69618,#69619,#69620,
#69621,#69622),(#69623,#69624,#69625,#69626,#69627,#69628,#69629,#69630,
#69631,#69632,#69633,#69634,#69635,#69636,#69637,#69638,#69639,#69640,#69641,
#69642,#69643,#69644,#69645,#69646,#69647,#69648,#69649,#69650,#69651,#69652,
#69653,#69654,#69655,#69656,#69657,#69658,#69659,#69660,#69661,#69662,#69663,
#69664,#69665,#69666,#69667,#69668,#69669,#69670,#69671,#69672,#69673,#69674,
#69675,#69676,#69677,#69678,#69679,#69680,#69681,#69682,#69683,#69684,#69685,
#69686,#69687,#69688,#69689,#69690,#69691,#69692,#69693,#69694,#69695,#69696,
#69697,#69698,#69699,#69700,#69701,#69702,#69703,#69704,#69705,#69706,#69707,
#69708,#69709,#69710,#69711,#69712,#69713,#69714,#69715,#69716,#69717,#69718,
#69719,#69720,#69721,#69722,#69723,#69724,#69725,#69726,#69727,#69728,#69729,
#69730,#69731,#69732,#69733,#69734,#69735,#69736,#69737,#69738,#69739,#69740,
#69741,#69742,#69743,#69744,#69745,#69746,#69747,#69748,#69749,#69750,#69751,
#69752,#69753,#69754,#69755,#69756,#69757,#69758,#69759,#69760,#69761,#69762,
#69763,#69764,#69765,#69766,#69767,#69768,#69769,#69770,#69771,#69772,#69773,
#69774,#69775,#69776,#69777,#69778,#69779,#69780,#69781,#69782,#69783,#69784,
#69785,#69786,#69787,#69788,#69789,#69790,#69791,#69792,#69793,#69794,#69795,
#69796,#69797,#69798,#69799,#69800,#69801,#69802,#69803,#69804,#69805,#69806,
#69807,#69808,#69809,#69810,#69811,#69812,#69813,#69814,#69815,#69816,#69817,
#69818,#69819,#69820,#69821,#69822,#69823,#69824,#69825,#69826,#69827),
(#69828,#69829,#69830,#69831,#69832,#69833,#69834,#69835,#69836,#69837,
#69838,#69839,#69840,#69841,#69842,#69843,#69844,#69845,#69846,#69847,#69848,
#69849,#69850,#69851,#69852,#69853,#69854,#69855,#69856,#69857,#69858,#69859,
#69860,#69861,#69862,#69863,#69864,#69865,#69866,#69867,#69868,#69869,#69870,
#69871,#69872,#69873,#69874,#69875,#69876,#69877,#69878,#69879,#69880,#69881,
#69882,#69883,#69884,#69885,#69886,#69887,#69888,#69889,#69890,#69891,#69892,
#69893,#69894,#69895,#69896,#69897,#69898,#69899,#69900,#69901,#69902,#69903,
#69904,#69905,#69906,#69907,#69908,#69909,#69910,#69911,#69912,#69913,#69914,
#69915,#69916,#69917,#69918,#69919,#69920,#69921,#69922,#69923,#69924,#69925,
#69926,#69927,#69928,#69929,#69930,#69931,#69932,#69933,#69934,#69935,#69936,
#69937,#69938,#69939,#69940,#69941,#69942,#69943,#69944,#69945,#69946,#69947,
#69948,#69949,#69950,#69951,#69952,#69953,#69954,#69955,#69956,#69957,#69958,
#69959,#69960,#69961,#69962,#69963,#69964,#69965,#69966,#69967,#69968,#69969,
#69970,#69971,#69972,#69973,#69974,#69975,#69976,#69977,#69978,#69979,#69980,
#69981,#69982,#69983,#69984,#69985,#69986,#69987,#69988,#69989,#69990,#69991,
#69992,#69993,#69994,#69995,#69996,#69997,#69998,#69999,#70000,#70001,#70002,
#70003,#70004,#70005,#70006,#70007,#70008,#70009,#70010,#70011,#70012,#70013,
#70014,#70015,#70016,#70017,#70018,#70019,#70020,#70021,#70022,#70023,#70024,
#70025,#70026,#70027,#70028,#70029,#70030,#70031,#70032),(#70033,#70034,
#70035,#70036,#70037,#70038,#70039,#70040,#70041,#70042,#70043,#70044,#70045,
#70046,#70047,#70048,#70049,#70050,#70051,#70052,#70053,#70054,#70055,#70056,
#70057,#70058,#70059,#70060,#70061,#70062,#70063,#70064,#70065,#70066,#70067,
#70068,#70069,#70070,#70071,#70072,#70073,#70074,#70075,#70076,#70077,#70078,
#70079,#70080,#70081,#70082,#70083,#70084,#70085,#70086,#70087,#70088,#70089,
#70090,#70091,#70092,#70093,#70094,#70095,#70096,#70097,#70098,#70099,#70100,
#70101,#70102,#70103,#70104,#70105,#70106,#70107,#70108,#70109,#70110,#70111,
#70112,#70113,#70114,#70115,#70116,#70117,#70118,#70119,#70120,#70121,#70122,
#70123,#70124,#70125,#70126,#70127,#70128,#70129,#70130,#70131,#70132,#70133,
#70134,#70135,#70136,#70137,#70138,#70139,#70140,#70141,#70142,#70143,#70144,
#70145,#70146,#70147,#70148,#70149,#70150,#70151,#70152,#70153,#70154,#70155,
#70156,#70157,#70158,#70159,#70160,#70161,#70162,#70163,#70164,#70165,#70166,
#70167,#70168,#70169,#70170,#70171,#70172,#70173,#70174,#70175,#70176,#70177,
#70178,#70179,#70180,#70181,#70182,#70183,#70184,#70185,#70186,#70187,#70188,
#70189,#70190,#70191,#70192,#70193,#70194,#70195,#70196,#70197,#70198,#70199,
#70200,#70201,#70202,#70203,#70204,#70205,#70206,#70207,#70208,#70209,#70210,
#70211,#70212,#70213,#70214,#70215,#70216,#70217,#70218,#70219,#70220,#70221,
#70222,#70223,#70224,#70225,#70226,#70227,#70228,#70229,#70230,#70231,#70232,
#70233,#70234,#70235,#70236,#70237)),.UNSPECIFIED.,.F.,.F.,.F.,(4,4),(4,
1,1,1,1,1,1,1,1,1,1,1,1,1,1,1,1,1,1,1,1,1,1,1,1,1,1,1,1,1,1,1,1,1,1,1,1,
1,1,1,1,1,1,1,1,1,1,1,1,1,1,1,1,1,1,1,1,1,1,1,1,1,1,1,1,1,1,1,1,1,1,1,1,
1,1,1,1,1,1,1,1,1,1,1,1,1,1,1,1,1,1,1,1,1,1,1,1,1,1,1,1,1,1,1,1,1,1,1,1,
1,1,1,1,1,1,1,1,1,1,1,1,1,1,1,1,1,1,1,1,1,1,1,1,1,1,1,1,1,1,1,1,1,1,1,1,
1,1,1,1,1,1,1,1,1,1,1,1,1,1,1,1,1,1,1,1,1,1,1,1,1,1,1,1,1,1,1,1,1,1,1,1,
1,1,1,1,1,1,1,1,1,1,1,1,1,1,1,1,1,1,1,1,1,4),(0.,0.0824167509268191),(11.6150691238055,
12.1134708852447,12.6118726466838,13.110274408123,13.6086761695621,14.1070779310013,
14.6054796924404,15.1038814538796,15.6022832153187,16.1006849767579,16.5990867381971,
17.0974884996362,17.5958902610754,18.0942920225145,18.5926937839537,19.0910955453928,
19.589497306832,20.0878990682711,20.5863008297103,21.0847025911494,21.5831043525886,
22.0815061140277,22.5799078754669,23.0783096369061,23.5767113983452,24.0751131597844,
24.5735149212235,25.0719166826627,25.5703184441018,26.068720205541,26.5671219669801,
27.0655237284193,27.5639254898584,28.0623272512976,28.5607290127367,29.0591307741759,
29.5575325356151,30.0559342970542,30.5543360584934,31.0527378199325,31.5511395813717,
32.0495413428108,32.54794310425,33.0463448656891,33.5447466271283,34.0431483885674,
34.5415501500066,35.0399519114457,35.5383536728849,36.036755434324,36.5351571957632,
37.0335589572024,37.5319607186415,38.0303624800807,38.5287642415198,39.027166002959,
39.5255677643981,40.0239695258373,40.5223712872764,41.0207730487156,41.5191748101547,
42.0175765715939,42.515978333033,43.0143800944722,43.5127818559113,44.0111836173505,
44.5095853787897,45.0079871402288,45.506388901668,46.0047906631071,46.5031924245463,
47.0015941859854,47.4999959474246,47.9983977088637,48.4967994703029,48.995201231742,
49.4936029931812,49.9920047546203,50.4904065160595,50.9888082774987,51.4872100389378,
51.985611800377,52.4840135618161,52.9824153232553,53.4808170846944,53.9792188461336,
54.4776206075727,54.9760223690119,55.474424130451,55.9728258918902,56.4712276533293,
56.9696294147685,57.4680311762077,57.9664329376468,58.464834699086,58.9632364605251,
59.4616382219643,59.9600399834034,60.4584417448426,60.9568435062817,61.4552452677209,
61.95364702916,62.4520487905992,62.9504505520383,63.4488523134775,63.9472540749166,
64.4456558363558,64.944057597795,65.4424593592341,65.9408611206733,66.4392628821124,
66.9376646435516,67.4360664049907,67.9344681664299,68.432869927869,68.9312716893082,
69.4296734507473,69.9280752121865,70.4264769736257,70.9248787350648,71.4232804965039,
71.9216822579431,72.4200840193823,72.9184857808214,73.4168875422606,73.9152893036997,
74.4136910651389,74.912092826578,75.4104945880172,75.9088963494563,76.4072981108955,
76.9056998723347,77.4041016337738,77.902503395213,78.4009051566521,78.8993069180913,
79.3977086795304,79.8961104409696,80.3945122024087,80.8929139638479,81.391315725287,
81.8897174867262,82.3881192481653,82.8865210096045,83.3849227710436,83.8833245324828,
84.381726293922,84.8801280553611,85.3785298168003,85.8769315782394,86.3753333396786,
86.8737351011177,87.3721368625569,87.870538623996,88.3689403854352,88.8673421468743,
89.3657439083135,89.8641456697526,90.3625474311918,90.860949192631,91.3593509540701,
91.8577527155093,92.3561544769484,92.8545562383876,93.3529579998267,93.8513597612659,
94.349761522705,94.8481632841442,95.3465650455833,95.8449668070225,96.3433685684616,
96.8417703299008,97.34017209134,97.8385738527791,98.3369756142182,98.8353773756574,
99.3337791370966,99.8321808985357,100.330582659975,100.828984421414,101.327386182853,
101.825787944292,102.324189705731,102.822591467171,103.32099322861,103.819394990049,
104.317796751488,104.816198512927,105.314600274366,105.813002035806,106.311403797245,
106.809805558684,107.308207320123,107.806609081562,108.305010843001,108.80341260444,
109.30181436588,109.800216127319,110.298617888758,110.797019650197,111.295421411636,
111.793823173075,112.292224934515),.UNSPECIFIED.);
#429=B_SPLINE_SURFACE_WITH_KNOTS('',3,3,((#76147,#76148,#76149,#76150,#76151,
#76152,#76153,#76154,#76155,#76156,#76157,#76158,#76159,#76160,#76161,#76162,
#76163,#76164,#76165,#76166,#76167,#76168,#76169,#76170,#76171,#76172,#76173,
#76174,#76175,#76176,#76177,#76178,#76179,#76180,#76181,#76182,#76183,#76184,
#76185,#76186,#76187,#76188,#76189,#76190,#76191,#76192,#76193,#76194,#76195,
#76196,#76197,#76198,#76199,#76200,#76201,#76202,#76203,#76204,#76205,#76206,
#76207,#76208,#76209,#76210,#76211,#76212,#76213,#76214,#76215,#76216,#76217,
#76218,#76219,#76220,#76221,#76222,#76223,#76224,#76225,#76226,#76227,#76228,
#76229,#76230,#76231,#76232,#76233,#76234,#76235,#76236,#76237,#76238,#76239,
#76240,#76241,#76242,#76243,#76244,#76245,#76246,#76247,#76248,#76249,#76250,
#76251,#76252,#76253,#76254,#76255,#76256,#76257,#76258,#76259,#76260,#76261,
#76262,#76263,#76264,#76265,#76266,#76267,#76268,#76269,#76270,#76271,#76272,
#76273,#76274,#76275,#76276,#76277,#76278,#76279,#76280,#76281,#76282,#76283,
#76284,#76285,#76286,#76287,#76288,#76289,#76290,#76291,#76292,#76293,#76294,
#76295,#76296,#76297,#76298,#76299,#76300,#76301,#76302,#76303,#76304,#76305,
#76306,#76307,#76308,#76309,#76310,#76311,#76312,#76313,#76314,#76315,#76316,
#76317,#76318,#76319,#76320,#76321,#76322,#76323,#76324,#76325,#76326,#76327,
#76328,#76329,#76330,#76331,#76332,#76333,#76334,#76335,#76336,#76337,#76338,
#76339,#76340,#76341,#76342,#76343,#76344,#76345,#76346,#76347,#76348,#76349,
#76350,#76351,#76352,#76353,#76354,#76355,#76356,#76357,#76358,#76359,#76360,
#76361,#76362,#76363,#76364,#76365,#76366,#76367,#76368,#76369,#76370,#76371,
#76372,#76373,#76374,#76375,#76376,#76377,#76378,#76379,#76380,#76381,#76382,
#76383,#76384,#76385,#76386,#76387,#76388,#76389,#76390,#76391,#76392,#76393,
#76394,#76395,#76396,#76397,#76398,#76399,#76400,#76401,#76402,#76403,#76404,
#76405,#76406,#76407,#76408,#76409,#76410,#76411,#76412,#76413,#76414,#76415,
#76416,#76417,#76418,#76419,#76420,#76421,#76422,#76423,#76424,#76425,#76426,
#76427,#76428,#76429,#76430,#76431,#76432,#76433,#76434,#76435,#76436,#76437,
#76438,#76439,#76440,#76441,#76442,#76443,#76444,#76445,#76446,#76447,#76448,
#76449,#76450,#76451,#76452,#76453,#76454,#76455,#76456,#76457,#76458,#76459,
#76460,#76461,#76462,#76463,#76464,#76465,#76466,#76467,#76468,#76469,#76470,
#76471,#76472,#76473,#76474,#76475,#76476,#76477,#76478,#76479,#76480,#76481,
#76482,#76483,#76484,#76485,#76486,#76487,#76488,#76489,#76490,#76491,#76492,
#76493,#76494,#76495,#76496,#76497,#76498,#76499,#76500,#76501,#76502,#76503,
#76504,#76505,#76506,#76507,#76508,#76509,#76510,#76511,#76512,#76513,#76514,
#76515,#76516,#76517,#76518,#76519,#76520,#76521,#76522,#76523,#76524,#76525,
#76526,#76527,#76528,#76529,#76530,#76531,#76532,#76533,#76534,#76535,#76536,
#76537,#76538,#76539,#76540,#76541,#76542,#76543,#76544,#76545,#76546,#76547,
#76548,#76549,#76550,#76551,#76552,#76553,#76554,#76555,#76556,#76557,#76558,
#76559,#76560,#76561,#76562,#76563,#76564,#76565,#76566,#76567,#76568,#76569,
#76570,#76571,#76572,#76573,#76574,#76575,#76576,#76577,#76578,#76579,#76580,
#76581,#76582,#76583,#76584,#76585,#76586,#76587,#76588,#76589,#76590,#76591,
#76592,#76593,#76594,#76595,#76596,#76597,#76598,#76599,#76600,#76601,#76602,
#76603,#76604,#76605,#76606,#76607,#76608,#76609,#76610,#76611,#76612,#76613,
#76614,#76615,#76616,#76617,#76618,#76619,#76620,#76621,#76622,#76623,#76624),
(#76625,#76626,#76627,#76628,#76629,#76630,#76631,#76632,#76633,#76634,
#76635,#76636,#76637,#76638,#76639,#76640,#76641,#76642,#76643,#76644,#76645,
#76646,#76647,#76648,#76649,#76650,#76651,#76652,#76653,#76654,#76655,#76656,
#76657,#76658,#76659,#76660,#76661,#76662,#76663,#76664,#76665,#76666,#76667,
#76668,#76669,#76670,#76671,#76672,#76673,#76674,#76675,#76676,#76677,#76678,
#76679,#76680,#76681,#76682,#76683,#76684,#76685,#76686,#76687,#76688,#76689,
#76690,#76691,#76692,#76693,#76694,#76695,#76696,#76697,#76698,#76699,#76700,
#76701,#76702,#76703,#76704,#76705,#76706,#76707,#76708,#76709,#76710,#76711,
#76712,#76713,#76714,#76715,#76716,#76717,#76718,#76719,#76720,#76721,#76722,
#76723,#76724,#76725,#76726,#76727,#76728,#76729,#76730,#76731,#76732,#76733,
#76734,#76735,#76736,#76737,#76738,#76739,#76740,#76741,#76742,#76743,#76744,
#76745,#76746,#76747,#76748,#76749,#76750,#76751,#76752,#76753,#76754,#76755,
#76756,#76757,#76758,#76759,#76760,#76761,#76762,#76763,#76764,#76765,#76766,
#76767,#76768,#76769,#76770,#76771,#76772,#76773,#76774,#76775,#76776,#76777,
#76778,#76779,#76780,#76781,#76782,#76783,#76784,#76785,#76786,#76787,#76788,
#76789,#76790,#76791,#76792,#76793,#76794,#76795,#76796,#76797,#76798,#76799,
#76800,#76801,#76802,#76803,#76804,#76805,#76806,#76807,#76808,#76809,#76810,
#76811,#76812,#76813,#76814,#76815,#76816,#76817,#76818,#76819,#76820,#76821,
#76822,#76823,#76824,#76825,#76826,#76827,#76828,#76829,#76830,#76831,#76832,
#76833,#76834,#76835,#76836,#76837,#76838,#76839,#76840,#76841,#76842,#76843,
#76844,#76845,#76846,#76847,#76848,#76849,#76850,#76851,#76852,#76853,#76854,
#76855,#76856,#76857,#76858,#76859,#76860,#76861,#76862,#76863,#76864,#76865,
#76866,#76867,#76868,#76869,#76870,#76871,#76872,#76873,#76874,#76875,#76876,
#76877,#76878,#76879,#76880,#76881,#76882,#76883,#76884,#76885,#76886,#76887,
#76888,#76889,#76890,#76891,#76892,#76893,#76894,#76895,#76896,#76897,#76898,
#76899,#76900,#76901,#76902,#76903,#76904,#76905,#76906,#76907,#76908,#76909,
#76910,#76911,#76912,#76913,#76914,#76915,#76916,#76917,#76918,#76919,#76920,
#76921,#76922,#76923,#76924,#76925,#76926,#76927,#76928,#76929,#76930,#76931,
#76932,#76933,#76934,#76935,#76936,#76937,#76938,#76939,#76940,#76941,#76942,
#76943,#76944,#76945,#76946,#76947,#76948,#76949,#76950,#76951,#76952,#76953,
#76954,#76955,#76956,#76957,#76958,#76959,#76960,#76961,#76962,#76963,#76964,
#76965,#76966,#76967,#76968,#76969,#76970,#76971,#76972,#76973,#76974,#76975,
#76976,#76977,#76978,#76979,#76980,#76981,#76982,#76983,#76984,#76985,#76986,
#76987,#76988,#76989,#76990,#76991,#76992,#76993,#76994,#76995,#76996,#76997,
#76998,#76999,#77000,#77001,#77002,#77003,#77004,#77005,#77006,#77007,#77008,
#77009,#77010,#77011,#77012,#77013,#77014,#77015,#77016,#77017,#77018,#77019,
#77020,#77021,#77022,#77023,#77024,#77025,#77026,#77027,#77028,#77029,#77030,
#77031,#77032,#77033,#77034,#77035,#77036,#77037,#77038,#77039,#77040,#77041,
#77042,#77043,#77044,#77045,#77046,#77047,#77048,#77049,#77050,#77051,#77052,
#77053,#77054,#77055,#77056,#77057,#77058,#77059,#77060,#77061,#77062,#77063,
#77064,#77065,#77066,#77067,#77068,#77069,#77070,#77071,#77072,#77073,#77074,
#77075,#77076,#77077,#77078,#77079,#77080,#77081,#77082,#77083,#77084,#77085,
#77086,#77087,#77088,#77089,#77090,#77091,#77092,#77093,#77094,#77095,#77096,
#77097,#77098,#77099,#77100,#77101,#77102),(#77103,#77104,#77105,#77106,
#77107,#77108,#77109,#77110,#77111,#77112,#77113,#77114,#77115,#77116,#77117,
#77118,#77119,#77120,#77121,#77122,#77123,#77124,#77125,#77126,#77127,#77128,
#77129,#77130,#77131,#77132,#77133,#77134,#77135,#77136,#77137,#77138,#77139,
#77140,#77141,#77142,#77143,#77144,#77145,#77146,#77147,#77148,#77149,#77150,
#77151,#77152,#77153,#77154,#77155,#77156,#77157,#77158,#77159,#77160,#77161,
#77162,#77163,#77164,#77165,#77166,#77167,#77168,#77169,#77170,#77171,#77172,
#77173,#77174,#77175,#77176,#77177,#77178,#77179,#77180,#77181,#77182,#77183,
#77184,#77185,#77186,#77187,#77188,#77189,#77190,#77191,#77192,#77193,#77194,
#77195,#77196,#77197,#77198,#77199,#77200,#77201,#77202,#77203,#77204,#77205,
#77206,#77207,#77208,#77209,#77210,#77211,#77212,#77213,#77214,#77215,#77216,
#77217,#77218,#77219,#77220,#77221,#77222,#77223,#77224,#77225,#77226,#77227,
#77228,#77229,#77230,#77231,#77232,#77233,#77234,#77235,#77236,#77237,#77238,
#77239,#77240,#77241,#77242,#77243,#77244,#77245,#77246,#77247,#77248,#77249,
#77250,#77251,#77252,#77253,#77254,#77255,#77256,#77257,#77258,#77259,#77260,
#77261,#77262,#77263,#77264,#77265,#77266,#77267,#77268,#77269,#77270,#77271,
#77272,#77273,#77274,#77275,#77276,#77277,#77278,#77279,#77280,#77281,#77282,
#77283,#77284,#77285,#77286,#77287,#77288,#77289,#77290,#77291,#77292,#77293,
#77294,#77295,#77296,#77297,#77298,#77299,#77300,#77301,#77302,#77303,#77304,
#77305,#77306,#77307,#77308,#77309,#77310,#77311,#77312,#77313,#77314,#77315,
#77316,#77317,#77318,#77319,#77320,#77321,#77322,#77323,#77324,#77325,#77326,
#77327,#77328,#77329,#77330,#77331,#77332,#77333,#77334,#77335,#77336,#77337,
#77338,#77339,#77340,#77341,#77342,#77343,#77344,#77345,#77346,#77347,#77348,
#77349,#77350,#77351,#77352,#77353,#77354,#77355,#77356,#77357,#77358,#77359,
#77360,#77361,#77362,#77363,#77364,#77365,#77366,#77367,#77368,#77369,#77370,
#77371,#77372,#77373,#77374,#77375,#77376,#77377,#77378,#77379,#77380,#77381,
#77382,#77383,#77384,#77385,#77386,#77387,#77388,#77389,#77390,#77391,#77392,
#77393,#77394,#77395,#77396,#77397,#77398,#77399,#77400,#77401,#77402,#77403,
#77404,#77405,#77406,#77407,#77408,#77409,#77410,#77411,#77412,#77413,#77414,
#77415,#77416,#77417,#77418,#77419,#77420,#77421,#77422,#77423,#77424,#77425,
#77426,#77427,#77428,#77429,#77430,#77431,#77432,#77433,#77434,#77435,#77436,
#77437,#77438,#77439,#77440,#77441,#77442,#77443,#77444,#77445,#77446,#77447,
#77448,#77449,#77450,#77451,#77452,#77453,#77454,#77455,#77456,#77457,#77458,
#77459,#77460,#77461,#77462,#77463,#77464,#77465,#77466,#77467,#77468,#77469,
#77470,#77471,#77472,#77473,#77474,#77475,#77476,#77477,#77478,#77479,#77480,
#77481,#77482,#77483,#77484,#77485,#77486,#77487,#77488,#77489,#77490,#77491,
#77492,#77493,#77494,#77495,#77496,#77497,#77498,#77499,#77500,#77501,#77502,
#77503,#77504,#77505,#77506,#77507,#77508,#77509,#77510,#77511,#77512,#77513,
#77514,#77515,#77516,#77517,#77518,#77519,#77520,#77521,#77522,#77523,#77524,
#77525,#77526,#77527,#77528,#77529,#77530,#77531,#77532,#77533,#77534,#77535,
#77536,#77537,#77538,#77539,#77540,#77541,#77542,#77543,#77544,#77545,#77546,
#77547,#77548,#77549,#77550,#77551,#77552,#77553,#77554,#77555,#77556,#77557,
#77558,#77559,#77560,#77561,#77562,#77563,#77564,#77565,#77566,#77567,#77568,
#77569,#77570,#77571,#77572,#77573,#77574,#77575,#77576,#77577,#77578,#77579,
#77580),(#77581,#77582,#77583,#77584,#77585,#77586,#77587,#77588,#77589,
#77590,#77591,#77592,#77593,#77594,#77595,#77596,#77597,#77598,#77599,#77600,
#77601,#77602,#77603,#77604,#77605,#77606,#77607,#77608,#77609,#77610,#77611,
#77612,#77613,#77614,#77615,#77616,#77617,#77618,#77619,#77620,#77621,#77622,
#77623,#77624,#77625,#77626,#77627,#77628,#77629,#77630,#77631,#77632,#77633,
#77634,#77635,#77636,#77637,#77638,#77639,#77640,#77641,#77642,#77643,#77644,
#77645,#77646,#77647,#77648,#77649,#77650,#77651,#77652,#77653,#77654,#77655,
#77656,#77657,#77658,#77659,#77660,#77661,#77662,#77663,#77664,#77665,#77666,
#77667,#77668,#77669,#77670,#77671,#77672,#77673,#77674,#77675,#77676,#77677,
#77678,#77679,#77680,#77681,#77682,#77683,#77684,#77685,#77686,#77687,#77688,
#77689,#77690,#77691,#77692,#77693,#77694,#77695,#77696,#77697,#77698,#77699,
#77700,#77701,#77702,#77703,#77704,#77705,#77706,#77707,#77708,#77709,#77710,
#77711,#77712,#77713,#77714,#77715,#77716,#77717,#77718,#77719,#77720,#77721,
#77722,#77723,#77724,#77725,#77726,#77727,#77728,#77729,#77730,#77731,#77732,
#77733,#77734,#77735,#77736,#77737,#77738,#77739,#77740,#77741,#77742,#77743,
#77744,#77745,#77746,#77747,#77748,#77749,#77750,#77751,#77752,#77753,#77754,
#77755,#77756,#77757,#77758,#77759,#77760,#77761,#77762,#77763,#77764,#77765,
#77766,#77767,#77768,#77769,#77770,#77771,#77772,#77773,#77774,#77775,#77776,
#77777,#77778,#77779,#77780,#77781,#77782,#77783,#77784,#77785,#77786,#77787,
#77788,#77789,#77790,#77791,#77792,#77793,#77794,#77795,#77796,#77797,#77798,
#77799,#77800,#77801,#77802,#77803,#77804,#77805,#77806,#77807,#77808,#77809,
#77810,#77811,#77812,#77813,#77814,#77815,#77816,#77817,#77818,#77819,#77820,
#77821,#77822,#77823,#77824,#77825,#77826,#77827,#77828,#77829,#77830,#77831,
#77832,#77833,#77834,#77835,#77836,#77837,#77838,#77839,#77840,#77841,#77842,
#77843,#77844,#77845,#77846,#77847,#77848,#77849,#77850,#77851,#77852,#77853,
#77854,#77855,#77856,#77857,#77858,#77859,#77860,#77861,#77862,#77863,#77864,
#77865,#77866,#77867,#77868,#77869,#77870,#77871,#77872,#77873,#77874,#77875,
#77876,#77877,#77878,#77879,#77880,#77881,#77882,#77883,#77884,#77885,#77886,
#77887,#77888,#77889,#77890,#77891,#77892,#77893,#77894,#77895,#77896,#77897,
#77898,#77899,#77900,#77901,#77902,#77903,#77904,#77905,#77906,#77907,#77908,
#77909,#77910,#77911,#77912,#77913,#77914,#77915,#77916,#77917,#77918,#77919,
#77920,#77921,#77922,#77923,#77924,#77925,#77926,#77927,#77928,#77929,#77930,
#77931,#77932,#77933,#77934,#77935,#77936,#77937,#77938,#77939,#77940,#77941,
#77942,#77943,#77944,#77945,#77946,#77947,#77948,#77949,#77950,#77951,#77952,
#77953,#77954,#77955,#77956,#77957,#77958,#77959,#77960,#77961,#77962,#77963,
#77964,#77965,#77966,#77967,#77968,#77969,#77970,#77971,#77972,#77973,#77974,
#77975,#77976,#77977,#77978,#77979,#77980,#77981,#77982,#77983,#77984,#77985,
#77986,#77987,#77988,#77989,#77990,#77991,#77992,#77993,#77994,#77995,#77996,
#77997,#77998,#77999,#78000,#78001,#78002,#78003,#78004,#78005,#78006,#78007,
#78008,#78009,#78010,#78011,#78012,#78013,#78014,#78015,#78016,#78017,#78018,
#78019,#78020,#78021,#78022,#78023,#78024,#78025,#78026,#78027,#78028,#78029,
#78030,#78031,#78032,#78033,#78034,#78035,#78036,#78037,#78038,#78039,#78040,
#78041,#78042,#78043,#78044,#78045,#78046,#78047,#78048,#78049,#78050,#78051,
#78052,#78053,#78054,#78055,#78056,#78057,#78058)),.UNSPECIFIED.,.F.,.F.,
 .F.,(4,4),(4,1,1,1,1,1,1,1,1,1,1,1,1,1,1,1,1,1,1,1,1,1,1,1,1,1,1,1,1,1,
1,1,1,1,1,1,1,1,1,1,1,1,1,1,1,1,1,1,1,1,1,1,1,1,1,1,1,1,1,1,1,1,1,1,1,1,
1,1,1,1,1,1,1,1,1,1,1,1,1,1,1,1,1,1,1,1,1,1,1,1,1,1,1,1,1,1,1,1,1,1,1,1,
1,1,1,1,1,1,1,1,1,1,1,1,1,1,1,1,1,1,1,1,1,1,1,1,1,1,1,1,1,1,1,1,1,1,1,1,
1,1,1,1,1,1,1,1,1,1,1,1,1,1,1,1,1,1,1,1,1,1,1,1,1,1,1,1,1,1,1,1,1,1,1,1,
1,1,1,1,1,1,1,1,1,1,1,1,1,1,1,1,1,1,1,1,1,1,1,1,1,1,1,1,1,1,1,1,1,1,1,1,
1,1,1,1,1,1,1,1,1,1,1,1,1,1,1,1,1,1,1,1,1,1,1,1,1,1,1,1,1,1,1,1,1,1,1,1,
1,1,1,1,1,1,1,1,1,1,1,1,1,1,1,1,1,1,1,1,1,1,1,1,1,1,1,1,1,1,1,1,1,1,1,1,
1,1,1,1,1,1,1,1,1,1,1,1,1,1,1,1,1,1,1,1,1,1,1,1,1,1,1,1,1,1,1,1,1,1,1,1,
1,1,1,1,1,1,1,1,1,1,1,1,1,1,1,1,1,1,1,1,1,1,1,1,1,1,1,1,1,1,1,1,1,1,1,1,
1,1,1,1,1,1,1,1,1,1,1,1,1,1,1,1,1,1,1,1,1,1,1,1,1,1,1,1,1,1,1,1,1,1,1,1,
1,1,1,1,1,1,1,1,1,1,1,1,1,1,1,1,1,1,1,1,1,1,1,1,1,1,1,1,1,1,1,1,1,1,1,1,
1,1,1,1,1,1,1,1,1,1,1,1,1,1,1,1,1,1,1,1,1,1,1,1,1,1,1,1,1,1,1,1,1,1,1,1,
1,1,1,1,1,1,1,1,1,1,1,1,1,4),(0.,0.0496809906637672),(8.29538555664048,
8.79496569366582,9.29454583069116,10.2937061047418,11.2928663787925,12.2920266528432,
13.2911869268939,14.2903472009446,15.2895074749953,16.288667749046,17.2878280230966,
18.2869882971473,19.286148571198,20.2853088452487,21.2844691192994,22.2836293933501,
23.2827896674008,24.2819499414514,25.2811102155021,26.2802704895528,27.2794307636035,
28.2785910376542,29.2777513117049,30.2769115857556,31.2760718598062,32.2752321338569,
33.2743924079076,34.2735526819583,35.272712956009,36.2718732300597,37.2710335041103,
38.270193778161,39.2693540522117,40.2685143262624,41.2676746003131,42.2668348743638,
43.2659951484145,44.2651554224651,45.2643156965158,46.2634759705665,47.2626362446172,
48.2617965186679,49.2609567927186,50.2601170667693,51.2592773408199,52.2584376148706,
53.2575978889213,54.256758162972,55.2559184370227,56.2550787110734,57.2542389851241,
58.2533992591747,59.2525595332254,60.2517198072761,61.2508800813268,62.2500403553775,
63.2492006294282,64.2483609034789,65.2475211775295,66.2466814515802,67.2458417256309,
68.2450019996816,69.2441622737323,70.243322547783,71.2424828218336,72.2416430958843,
73.240803369935,74.2399636439857,75.2391239180364,76.2382841920871,77.2374444661378,
78.2366047401885,79.2357650142391,80.2349252882898,81.2340855623405,82.2332458363912,
83.2324061104419,84.2315663844926,85.2307266585432,86.2298869325939,87.2290472066446,
88.2282074806953,89.227367754746,90.2265280287967,91.2256883028474,92.2248485768981,
93.2240088509487,94.2231691249994,95.2223293990501,96.2214896731008,97.2206499471515,
98.2198102212022,99.2189704952528,100.218130769304,101.217291043354,102.216451317405,
103.215611591456,104.214771865506,105.213932139557,106.213092413608,107.212252687658,
108.211412961709,109.21057323576,110.20973350981,111.208893783861,112.208054057912,
113.207214331962,114.206374606013,115.205534880064,116.204695154114,117.203855428165,
118.203015702216,119.202175976267,120.201336250317,121.200496524368,122.199656798419,
123.198817072469,124.19797734652,125.197137620571,126.196297894621,127.195458168672,
128.194618442723,129.193778716773,130.192938990824,131.192099264875,132.191259538925,
133.190419812976,134.189580087027,135.188740361078,136.187900635128,137.187060909179,
138.18622118323,139.18538145728,140.184541731331,141.183702005382,142.182862279432,
143.182022553483,144.181182827534,145.180343101584,146.179503375635,147.178663649686,
148.177823923736,149.176984197787,150.176144471838,151.175304745888,152.174465019939,
153.17362529399,154.172785568041,155.171945842091,156.171106116142,157.170266390193,
158.169426664243,159.168586938294,160.167747212345,161.166907486395,162.166067760446,
163.165228034497,164.164388308547,165.163548582598,166.162708856649,167.161869130699,
168.16102940475,169.160189678801,170.159349952851,171.158510226902,172.157670500953,
173.156830775004,174.155991049054,175.155151323105,176.154311597156,177.153471871206,
178.152632145257,179.151792419308,180.150952693358,181.150112967409,182.14927324146,
183.14843351551,184.147593789561,185.146754063612,186.145914337662,187.145074611713,
188.144234885764,189.143395159815,190.142555433865,191.141715707916,192.140875981967,
193.140036256017,194.139196530068,195.138356804119,196.137517078169,197.13667735222,
198.135837626271,199.134997900321,200.134158174372,201.133318448423,202.132478722473,
203.131638996524,204.130799270575,205.129959544625,206.129119818676,207.128280092727,
208.127440366778,209.126600640828,210.125760914879,211.12492118893,212.12408146298,
213.123241737031,214.122402011082,215.121562285132,216.120722559183,217.119882833234,
218.119043107284,219.118203381335,220.117363655386,221.116523929436,222.115684203487,
223.114844477538,224.114004751588,225.113165025639,226.11232529969,227.111485573741,
228.110645847791,229.109806121842,230.108966395893,231.108126669943,232.107286943994,
233.106447218045,234.105607492095,235.104767766146,236.103928040197,237.103088314247,
238.102248588298,239.101408862349,240.100569136399,241.09972941045,242.098889684501,
243.098049958552,244.097210232602,245.096370506653,246.095530780704,247.094691054754,
248.093851328805,249.093011602856,250.092171876906,251.091332150957,252.090492425008,
253.089652699058,254.088812973109,255.08797324716,256.08713352121,257.086293795261,
258.085454069312,259.084614343362,260.083774617413,261.082934891464,262.082095165515,
263.081255439565,264.080415713616,265.079575987667,266.078736261717,267.077896535768,
268.077056809819,269.076217083869,270.07537735792,271.074537631971,272.073697906021,
273.072858180072,274.072018454123,275.071178728173,276.070339002224,277.069499276275,
278.068659550326,279.067819824376,280.066980098427,281.066140372478,282.065300646528,
283.064460920579,284.06362119463,285.06278146868,286.061941742731,287.061102016782,
288.060262290832,289.059422564883,290.058582838934,291.057743112984,292.056903387035,
293.056063661086,294.055223935136,295.054384209187,296.053544483238,297.052704757289,
298.051865031339,299.05102530539,300.050185579441,301.049345853491,302.048506127542,
303.047666401593,304.046826675643,305.045986949694,306.045147223745,307.044307497795,
308.043467771846,309.042628045897,310.041788319947,311.040948593998,312.040108868049,
313.039269142099,314.03842941615,315.037589690201,316.036749964252,317.035910238302,
318.035070512353,319.034230786404,320.033391060454,321.032551334505,322.031711608556,
323.030871882606,324.030032156657,325.029192430708,326.028352704758,327.027512978809,
328.02667325286,329.025833526911,330.024993800961,331.024154075012,332.023314349063,
333.022474623113,334.021634897164,335.020795171215,336.019955445265,337.019115719316,
338.018275993367,339.017436267417,340.016596541468,341.015756815519,342.014917089569,
343.01407736362,344.013237637671,345.012397911721,346.011558185772,347.010718459823,
348.009878733874,349.009039007924,350.008199281975,351.007359556026,352.006519830076,
353.005680104127,354.004840378178,355.004000652228,356.003160926279,357.00232120033,
358.00148147438,359.000641748431,359.999802022482,360.998962296532,361.998122570583,
362.997282844634,363.996443118684,364.995603392735,365.994763666786,366.993923940837,
367.993084214887,368.992244488938,369.991404762989,370.990565037039,371.98972531109,
372.988885585141,373.988045859191,374.987206133242,375.986366407293,376.985526681343,
377.984686955394,378.983847229445,379.983007503495,380.982167777546,381.981328051597,
382.980488325648,383.979648599698,384.978808873749,385.9779691478,386.97712942185,
387.976289695901,388.975449969952,389.974610244002,390.973770518053,391.972930792104,
392.972091066154,393.971251340205,394.970411614256,395.969571888306,396.968732162357,
397.967892436408,398.967052710458,399.966212984509,400.96537325856,401.964533532611,
402.963693806661,403.962854080712,404.962014354763,405.961174628813,406.960334902864,
407.959495176915,408.958655450965,409.957815725016,410.956975999067,411.956136273117,
412.955296547168,413.954456821219,414.953617095269,415.95277736932,416.951937643371,
417.951097917421,418.950258191472,419.949418465523,420.948578739574,421.947739013624,
422.946899287675,423.946059561726,424.945219835776,425.944380109827,426.943540383878,
427.942700657928,428.941860931979,429.94102120603,430.94018148008,431.939341754131,
432.938502028182,433.937662302232,434.936822576283,435.935982850334,436.935143124384,
437.934303398435,438.933463672486,439.932623946537,440.931784220587,441.930944494638,
442.930104768689,443.929265042739,444.92842531679,445.927585590841,446.926745864891,
447.925906138942,448.925066412993,449.924226687043,450.923386961094,451.922547235145,
452.921707509195,453.920867783246,454.920028057297,455.919188331348,456.918348605398,
457.917508879449,458.9166691535,459.91582942755,460.914989701601,461.914149975652,
462.913310249702,463.912470523753,464.911630797804,465.910791071854,466.909951345905,
467.909111619956,468.908271894006,469.907432168057,470.906592442108,471.905752716158,
472.904912990209,473.90407326426,474.903233538311,475.902393812361,476.901554086412,
477.900714360463,478.899874634513,479.899034908564,480.398615045589,480.898195182615),
 .UNSPECIFIED.);
#430=B_SPLINE_SURFACE_WITH_KNOTS('',3,3,((#78316,#78317,#78318,#78319,#78320,
#78321,#78322,#78323,#78324,#78325,#78326,#78327,#78328,#78329,#78330,#78331,
#78332,#78333,#78334,#78335,#78336,#78337,#78338,#78339,#78340,#78341,#78342,
#78343,#78344,#78345,#78346,#78347,#78348,#78349,#78350,#78351,#78352,#78353,
#78354,#78355,#78356,#78357,#78358,#78359,#78360,#78361,#78362,#78363,#78364,
#78365,#78366,#78367,#78368,#78369,#78370,#78371,#78372,#78373,#78374,#78375,
#78376,#78377,#78378,#78379,#78380,#78381,#78382,#78383,#78384,#78385,#78386,
#78387,#78388,#78389,#78390,#78391,#78392,#78393,#78394,#78395,#78396,#78397,
#78398,#78399,#78400,#78401,#78402,#78403,#78404,#78405,#78406,#78407,#78408,
#78409,#78410,#78411,#78412,#78413,#78414,#78415,#78416,#78417,#78418,#78419,
#78420,#78421,#78422,#78423,#78424,#78425,#78426,#78427,#78428,#78429,#78430,
#78431,#78432,#78433,#78434,#78435,#78436,#78437,#78438,#78439,#78440,#78441,
#78442,#78443,#78444,#78445,#78446,#78447,#78448,#78449,#78450,#78451,#78452,
#78453,#78454,#78455,#78456,#78457,#78458,#78459,#78460,#78461,#78462,#78463,
#78464,#78465,#78466,#78467,#78468,#78469,#78470,#78471,#78472,#78473,#78474,
#78475,#78476,#78477,#78478,#78479,#78480,#78481,#78482,#78483,#78484,#78485,
#78486,#78487,#78488,#78489,#78490,#78491,#78492,#78493,#78494,#78495,#78496,
#78497,#78498,#78499,#78500,#78501,#78502,#78503,#78504,#78505,#78506,#78507,
#78508,#78509,#78510,#78511,#78512,#78513,#78514,#78515,#78516,#78517,#78518,
#78519,#78520,#78521,#78522,#78523,#78524,#78525,#78526,#78527,#78528,#78529,
#78530,#78531,#78532,#78533,#78534,#78535,#78536,#78537,#78538,#78539,#78540,
#78541,#78542,#78543,#78544,#78545,#78546,#78547,#78548,#78549,#78550,#78551,
#78552,#78553,#78554,#78555,#78556,#78557,#78558,#78559,#78560,#78561,#78562,
#78563,#78564,#78565,#78566,#78567,#78568,#78569,#78570,#78571,#78572,#78573,
#78574,#78575,#78576,#78577,#78578,#78579,#78580,#78581,#78582,#78583,#78584,
#78585,#78586,#78587,#78588,#78589,#78590,#78591,#78592,#78593,#78594,#78595,
#78596,#78597,#78598,#78599,#78600,#78601,#78602,#78603,#78604,#78605,#78606,
#78607,#78608,#78609,#78610,#78611,#78612,#78613,#78614,#78615,#78616,#78617,
#78618,#78619,#78620,#78621,#78622,#78623,#78624,#78625,#78626,#78627,#78628,
#78629,#78630,#78631,#78632,#78633,#78634,#78635,#78636,#78637,#78638,#78639,
#78640,#78641,#78642,#78643,#78644,#78645,#78646,#78647,#78648,#78649,#78650,
#78651,#78652,#78653,#78654,#78655,#78656,#78657,#78658,#78659,#78660,#78661,
#78662,#78663,#78664,#78665,#78666,#78667,#78668,#78669,#78670,#78671,#78672,
#78673,#78674,#78675,#78676,#78677,#78678,#78679,#78680,#78681,#78682,#78683,
#78684,#78685,#78686,#78687,#78688,#78689,#78690,#78691,#78692,#78693,#78694,
#78695,#78696,#78697,#78698,#78699,#78700,#78701,#78702,#78703,#78704,#78705,
#78706,#78707,#78708,#78709,#78710,#78711,#78712,#78713,#78714,#78715,#78716,
#78717,#78718,#78719,#78720,#78721,#78722,#78723,#78724,#78725,#78726,#78727,
#78728,#78729,#78730,#78731,#78732,#78733,#78734,#78735,#78736,#78737,#78738,
#78739,#78740,#78741,#78742,#78743,#78744,#78745,#78746,#78747,#78748,#78749,
#78750,#78751,#78752,#78753,#78754,#78755,#78756,#78757,#78758,#78759,#78760,
#78761,#78762,#78763,#78764,#78765,#78766,#78767,#78768,#78769,#78770,#78771,
#78772,#78773,#78774,#78775,#78776,#78777,#78778,#78779,#78780,#78781,#78782,
#78783,#78784,#78785,#78786,#78787,#78788,#78789,#78790,#78791,#78792,#78793),
(#78794,#78795,#78796,#78797,#78798,#78799,#78800,#78801,#78802,#78803,
#78804,#78805,#78806,#78807,#78808,#78809,#78810,#78811,#78812,#78813,#78814,
#78815,#78816,#78817,#78818,#78819,#78820,#78821,#78822,#78823,#78824,#78825,
#78826,#78827,#78828,#78829,#78830,#78831,#78832,#78833,#78834,#78835,#78836,
#78837,#78838,#78839,#78840,#78841,#78842,#78843,#78844,#78845,#78846,#78847,
#78848,#78849,#78850,#78851,#78852,#78853,#78854,#78855,#78856,#78857,#78858,
#78859,#78860,#78861,#78862,#78863,#78864,#78865,#78866,#78867,#78868,#78869,
#78870,#78871,#78872,#78873,#78874,#78875,#78876,#78877,#78878,#78879,#78880,
#78881,#78882,#78883,#78884,#78885,#78886,#78887,#78888,#78889,#78890,#78891,
#78892,#78893,#78894,#78895,#78896,#78897,#78898,#78899,#78900,#78901,#78902,
#78903,#78904,#78905,#78906,#78907,#78908,#78909,#78910,#78911,#78912,#78913,
#78914,#78915,#78916,#78917,#78918,#78919,#78920,#78921,#78922,#78923,#78924,
#78925,#78926,#78927,#78928,#78929,#78930,#78931,#78932,#78933,#78934,#78935,
#78936,#78937,#78938,#78939,#78940,#78941,#78942,#78943,#78944,#78945,#78946,
#78947,#78948,#78949,#78950,#78951,#78952,#78953,#78954,#78955,#78956,#78957,
#78958,#78959,#78960,#78961,#78962,#78963,#78964,#78965,#78966,#78967,#78968,
#78969,#78970,#78971,#78972,#78973,#78974,#78975,#78976,#78977,#78978,#78979,
#78980,#78981,#78982,#78983,#78984,#78985,#78986,#78987,#78988,#78989,#78990,
#78991,#78992,#78993,#78994,#78995,#78996,#78997,#78998,#78999,#79000,#79001,
#79002,#79003,#79004,#79005,#79006,#79007,#79008,#79009,#79010,#79011,#79012,
#79013,#79014,#79015,#79016,#79017,#79018,#79019,#79020,#79021,#79022,#79023,
#79024,#79025,#79026,#79027,#79028,#79029,#79030,#79031,#79032,#79033,#79034,
#79035,#79036,#79037,#79038,#79039,#79040,#79041,#79042,#79043,#79044,#79045,
#79046,#79047,#79048,#79049,#79050,#79051,#79052,#79053,#79054,#79055,#79056,
#79057,#79058,#79059,#79060,#79061,#79062,#79063,#79064,#79065,#79066,#79067,
#79068,#79069,#79070,#79071,#79072,#79073,#79074,#79075,#79076,#79077,#79078,
#79079,#79080,#79081,#79082,#79083,#79084,#79085,#79086,#79087,#79088,#79089,
#79090,#79091,#79092,#79093,#79094,#79095,#79096,#79097,#79098,#79099,#79100,
#79101,#79102,#79103,#79104,#79105,#79106,#79107,#79108,#79109,#79110,#79111,
#79112,#79113,#79114,#79115,#79116,#79117,#79118,#79119,#79120,#79121,#79122,
#79123,#79124,#79125,#79126,#79127,#79128,#79129,#79130,#79131,#79132,#79133,
#79134,#79135,#79136,#79137,#79138,#79139,#79140,#79141,#79142,#79143,#79144,
#79145,#79146,#79147,#79148,#79149,#79150,#79151,#79152,#79153,#79154,#79155,
#79156,#79157,#79158,#79159,#79160,#79161,#79162,#79163,#79164,#79165,#79166,
#79167,#79168,#79169,#79170,#79171,#79172,#79173,#79174,#79175,#79176,#79177,
#79178,#79179,#79180,#79181,#79182,#79183,#79184,#79185,#79186,#79187,#79188,
#79189,#79190,#79191,#79192,#79193,#79194,#79195,#79196,#79197,#79198,#79199,
#79200,#79201,#79202,#79203,#79204,#79205,#79206,#79207,#79208,#79209,#79210,
#79211,#79212,#79213,#79214,#79215,#79216,#79217,#79218,#79219,#79220,#79221,
#79222,#79223,#79224,#79225,#79226,#79227,#79228,#79229,#79230,#79231,#79232,
#79233,#79234,#79235,#79236,#79237,#79238,#79239,#79240,#79241,#79242,#79243,
#79244,#79245,#79246,#79247,#79248,#79249,#79250,#79251,#79252,#79253,#79254,
#79255,#79256,#79257,#79258,#79259,#79260,#79261,#79262,#79263,#79264,#79265,
#79266,#79267,#79268,#79269,#79270,#79271),(#79272,#79273,#79274,#79275,
#79276,#79277,#79278,#79279,#79280,#79281,#79282,#79283,#79284,#79285,#79286,
#79287,#79288,#79289,#79290,#79291,#79292,#79293,#79294,#79295,#79296,#79297,
#79298,#79299,#79300,#79301,#79302,#79303,#79304,#79305,#79306,#79307,#79308,
#79309,#79310,#79311,#79312,#79313,#79314,#79315,#79316,#79317,#79318,#79319,
#79320,#79321,#79322,#79323,#79324,#79325,#79326,#79327,#79328,#79329,#79330,
#79331,#79332,#79333,#79334,#79335,#79336,#79337,#79338,#79339,#79340,#79341,
#79342,#79343,#79344,#79345,#79346,#79347,#79348,#79349,#79350,#79351,#79352,
#79353,#79354,#79355,#79356,#79357,#79358,#79359,#79360,#79361,#79362,#79363,
#79364,#79365,#79366,#79367,#79368,#79369,#79370,#79371,#79372,#79373,#79374,
#79375,#79376,#79377,#79378,#79379,#79380,#79381,#79382,#79383,#79384,#79385,
#79386,#79387,#79388,#79389,#79390,#79391,#79392,#79393,#79394,#79395,#79396,
#79397,#79398,#79399,#79400,#79401,#79402,#79403,#79404,#79405,#79406,#79407,
#79408,#79409,#79410,#79411,#79412,#79413,#79414,#79415,#79416,#79417,#79418,
#79419,#79420,#79421,#79422,#79423,#79424,#79425,#79426,#79427,#79428,#79429,
#79430,#79431,#79432,#79433,#79434,#79435,#79436,#79437,#79438,#79439,#79440,
#79441,#79442,#79443,#79444,#79445,#79446,#79447,#79448,#79449,#79450,#79451,
#79452,#79453,#79454,#79455,#79456,#79457,#79458,#79459,#79460,#79461,#79462,
#79463,#79464,#79465,#79466,#79467,#79468,#79469,#79470,#79471,#79472,#79473,
#79474,#79475,#79476,#79477,#79478,#79479,#79480,#79481,#79482,#79483,#79484,
#79485,#79486,#79487,#79488,#79489,#79490,#79491,#79492,#79493,#79494,#79495,
#79496,#79497,#79498,#79499,#79500,#79501,#79502,#79503,#79504,#79505,#79506,
#79507,#79508,#79509,#79510,#79511,#79512,#79513,#79514,#79515,#79516,#79517,
#79518,#79519,#79520,#79521,#79522,#79523,#79524,#79525,#79526,#79527,#79528,
#79529,#79530,#79531,#79532,#79533,#79534,#79535,#79536,#79537,#79538,#79539,
#79540,#79541,#79542,#79543,#79544,#79545,#79546,#79547,#79548,#79549,#79550,
#79551,#79552,#79553,#79554,#79555,#79556,#79557,#79558,#79559,#79560,#79561,
#79562,#79563,#79564,#79565,#79566,#79567,#79568,#79569,#79570,#79571,#79572,
#79573,#79574,#79575,#79576,#79577,#79578,#79579,#79580,#79581,#79582,#79583,
#79584,#79585,#79586,#79587,#79588,#79589,#79590,#79591,#79592,#79593,#79594,
#79595,#79596,#79597,#79598,#79599,#79600,#79601,#79602,#79603,#79604,#79605,
#79606,#79607,#79608,#79609,#79610,#79611,#79612,#79613,#79614,#79615,#79616,
#79617,#79618,#79619,#79620,#79621,#79622,#79623,#79624,#79625,#79626,#79627,
#79628,#79629,#79630,#79631,#79632,#79633,#79634,#79635,#79636,#79637,#79638,
#79639,#79640,#79641,#79642,#79643,#79644,#79645,#79646,#79647,#79648,#79649,
#79650,#79651,#79652,#79653,#79654,#79655,#79656,#79657,#79658,#79659,#79660,
#79661,#79662,#79663,#79664,#79665,#79666,#79667,#79668,#79669,#79670,#79671,
#79672,#79673,#79674,#79675,#79676,#79677,#79678,#79679,#79680,#79681,#79682,
#79683,#79684,#79685,#79686,#79687,#79688,#79689,#79690,#79691,#79692,#79693,
#79694,#79695,#79696,#79697,#79698,#79699,#79700,#79701,#79702,#79703,#79704,
#79705,#79706,#79707,#79708,#79709,#79710,#79711,#79712,#79713,#79714,#79715,
#79716,#79717,#79718,#79719,#79720,#79721,#79722,#79723,#79724,#79725,#79726,
#79727,#79728,#79729,#79730,#79731,#79732,#79733,#79734,#79735,#79736,#79737,
#79738,#79739,#79740,#79741,#79742,#79743,#79744,#79745,#79746,#79747,#79748,
#79749),(#79750,#79751,#79752,#79753,#79754,#79755,#79756,#79757,#79758,
#79759,#79760,#79761,#79762,#79763,#79764,#79765,#79766,#79767,#79768,#79769,
#79770,#79771,#79772,#79773,#79774,#79775,#79776,#79777,#79778,#79779,#79780,
#79781,#79782,#79783,#79784,#79785,#79786,#79787,#79788,#79789,#79790,#79791,
#79792,#79793,#79794,#79795,#79796,#79797,#79798,#79799,#79800,#79801,#79802,
#79803,#79804,#79805,#79806,#79807,#79808,#79809,#79810,#79811,#79812,#79813,
#79814,#79815,#79816,#79817,#79818,#79819,#79820,#79821,#79822,#79823,#79824,
#79825,#79826,#79827,#79828,#79829,#79830,#79831,#79832,#79833,#79834,#79835,
#79836,#79837,#79838,#79839,#79840,#79841,#79842,#79843,#79844,#79845,#79846,
#79847,#79848,#79849,#79850,#79851,#79852,#79853,#79854,#79855,#79856,#79857,
#79858,#79859,#79860,#79861,#79862,#79863,#79864,#79865,#79866,#79867,#79868,
#79869,#79870,#79871,#79872,#79873,#79874,#79875,#79876,#79877,#79878,#79879,
#79880,#79881,#79882,#79883,#79884,#79885,#79886,#79887,#79888,#79889,#79890,
#79891,#79892,#79893,#79894,#79895,#79896,#79897,#79898,#79899,#79900,#79901,
#79902,#79903,#79904,#79905,#79906,#79907,#79908,#79909,#79910,#79911,#79912,
#79913,#79914,#79915,#79916,#79917,#79918,#79919,#79920,#79921,#79922,#79923,
#79924,#79925,#79926,#79927,#79928,#79929,#79930,#79931,#79932,#79933,#79934,
#79935,#79936,#79937,#79938,#79939,#79940,#79941,#79942,#79943,#79944,#79945,
#79946,#79947,#79948,#79949,#79950,#79951,#79952,#79953,#79954,#79955,#79956,
#79957,#79958,#79959,#79960,#79961,#79962,#79963,#79964,#79965,#79966,#79967,
#79968,#79969,#79970,#79971,#79972,#79973,#79974,#79975,#79976,#79977,#79978,
#79979,#79980,#79981,#79982,#79983,#79984,#79985,#79986,#79987,#79988,#79989,
#79990,#79991,#79992,#79993,#79994,#79995,#79996,#79997,#79998,#79999,#80000,
#80001,#80002,#80003,#80004,#80005,#80006,#80007,#80008,#80009,#80010,#80011,
#80012,#80013,#80014,#80015,#80016,#80017,#80018,#80019,#80020,#80021,#80022,
#80023,#80024,#80025,#80026,#80027,#80028,#80029,#80030,#80031,#80032,#80033,
#80034,#80035,#80036,#80037,#80038,#80039,#80040,#80041,#80042,#80043,#80044,
#80045,#80046,#80047,#80048,#80049,#80050,#80051,#80052,#80053,#80054,#80055,
#80056,#80057,#80058,#80059,#80060,#80061,#80062,#80063,#80064,#80065,#80066,
#80067,#80068,#80069,#80070,#80071,#80072,#80073,#80074,#80075,#80076,#80077,
#80078,#80079,#80080,#80081,#80082,#80083,#80084,#80085,#80086,#80087,#80088,
#80089,#80090,#80091,#80092,#80093,#80094,#80095,#80096,#80097,#80098,#80099,
#80100,#80101,#80102,#80103,#80104,#80105,#80106,#80107,#80108,#80109,#80110,
#80111,#80112,#80113,#80114,#80115,#80116,#80117,#80118,#80119,#80120,#80121,
#80122,#80123,#80124,#80125,#80126,#80127,#80128,#80129,#80130,#80131,#80132,
#80133,#80134,#80135,#80136,#80137,#80138,#80139,#80140,#80141,#80142,#80143,
#80144,#80145,#80146,#80147,#80148,#80149,#80150,#80151,#80152,#80153,#80154,
#80155,#80156,#80157,#80158,#80159,#80160,#80161,#80162,#80163,#80164,#80165,
#80166,#80167,#80168,#80169,#80170,#80171,#80172,#80173,#80174,#80175,#80176,
#80177,#80178,#80179,#80180,#80181,#80182,#80183,#80184,#80185,#80186,#80187,
#80188,#80189,#80190,#80191,#80192,#80193,#80194,#80195,#80196,#80197,#80198,
#80199,#80200,#80201,#80202,#80203,#80204,#80205,#80206,#80207,#80208,#80209,
#80210,#80211,#80212,#80213,#80214,#80215,#80216,#80217,#80218,#80219,#80220,
#80221,#80222,#80223,#80224,#80225,#80226,#80227)),.UNSPECIFIED.,.F.,.F.,
 .F.,(4,4),(4,1,1,1,1,1,1,1,1,1,1,1,1,1,1,1,1,1,1,1,1,1,1,1,1,1,1,1,1,1,
1,1,1,1,1,1,1,1,1,1,1,1,1,1,1,1,1,1,1,1,1,1,1,1,1,1,1,1,1,1,1,1,1,1,1,1,
1,1,1,1,1,1,1,1,1,1,1,1,1,1,1,1,1,1,1,1,1,1,1,1,1,1,1,1,1,1,1,1,1,1,1,1,
1,1,1,1,1,1,1,1,1,1,1,1,1,1,1,1,1,1,1,1,1,1,1,1,1,1,1,1,1,1,1,1,1,1,1,1,
1,1,1,1,1,1,1,1,1,1,1,1,1,1,1,1,1,1,1,1,1,1,1,1,1,1,1,1,1,1,1,1,1,1,1,1,
1,1,1,1,1,1,1,1,1,1,1,1,1,1,1,1,1,1,1,1,1,1,1,1,1,1,1,1,1,1,1,1,1,1,1,1,
1,1,1,1,1,1,1,1,1,1,1,1,1,1,1,1,1,1,1,1,1,1,1,1,1,1,1,1,1,1,1,1,1,1,1,1,
1,1,1,1,1,1,1,1,1,1,1,1,1,1,1,1,1,1,1,1,1,1,1,1,1,1,1,1,1,1,1,1,1,1,1,1,
1,1,1,1,1,1,1,1,1,1,1,1,1,1,1,1,1,1,1,1,1,1,1,1,1,1,1,1,1,1,1,1,1,1,1,1,
1,1,1,1,1,1,1,1,1,1,1,1,1,1,1,1,1,1,1,1,1,1,1,1,1,1,1,1,1,1,1,1,1,1,1,1,
1,1,1,1,1,1,1,1,1,1,1,1,1,1,1,1,1,1,1,1,1,1,1,1,1,1,1,1,1,1,1,1,1,1,1,1,
1,1,1,1,1,1,1,1,1,1,1,1,1,1,1,1,1,1,1,1,1,1,1,1,1,1,1,1,1,1,1,1,1,1,1,1,
1,1,1,1,1,1,1,1,1,1,1,1,1,1,1,1,1,1,1,1,1,1,1,1,1,1,1,1,1,1,1,1,1,1,1,1,
1,1,1,1,1,1,1,1,1,1,1,1,1,4),(0.,0.0496809906637672),(11.6147305479253,
12.1143106849507,12.613890821976,13.6130510960267,14.6122113700774,15.6113716441281,
16.6105319181787,17.6096921922294,18.6088524662801,19.6080127403308,20.6071730143815,
21.6063332884322,22.6054935624829,23.6046538365335,24.6038141105842,25.6029743846349,
26.6021346586856,27.6012949327363,28.600455206787,29.5996154808376,30.5987757548883,
31.597936028939,32.5970963029897,33.5962565770404,34.5954168510911,35.5945771251418,
36.5937373991924,37.5928976732431,38.5920579472938,39.5912182213445,40.5903784953952,
41.5895387694459,42.5886990434966,43.5878593175472,44.5870195915979,45.5861798656486,
46.5853401396993,47.58450041375,48.5836606878007,49.5828209618514,50.581981235902,
51.5811415099527,52.5803017840034,53.5794620580541,54.5786223321048,55.5777826061555,
56.5769428802061,57.5761031542568,58.5752634283075,59.5744237023582,60.5735839764089,
61.5727442504596,62.5719045245103,63.5710647985609,64.5702250726116,65.5693853466623,
66.568545620713,67.5677058947637,68.5668661688144,69.5660264428651,70.5651867169157,
71.5643469909664,72.5635072650171,73.5626675390678,74.5618278131185,75.5609880871692,
76.5601483612199,77.5593086352705,78.5584689093212,79.5576291833719,80.5567894574226,
81.5559497314733,82.555110005524,83.5542702795747,84.5534305536253,85.552590827676,
86.5517511017267,87.5509113757774,88.5500716498281,89.5492319238788,90.5483921979294,
91.5475524719801,92.5467127460308,93.5458730200815,94.5450332941322,95.5441935681829,
96.5433538422336,97.5425141162843,98.5416743903349,99.5408346643856,100.539994938436,
101.539155212487,102.538315486538,103.537475760588,104.536636034639,105.53579630869,
106.53495658274,107.534116856791,108.533277130842,109.532437404892,110.531597678943,
111.530757952994,112.529918227045,113.529078501095,114.528238775146,115.527399049197,
116.526559323247,117.525719597298,118.524879871349,119.524040145399,120.52320041945,
121.522360693501,122.521520967551,123.520681241602,124.519841515653,125.519001789703,
126.518162063754,127.517322337805,128.516482611855,129.515642885906,130.514803159957,
131.513963434008,132.513123708058,133.512283982109,134.51144425616,135.51060453021,
136.509764804261,137.508925078312,138.508085352362,139.507245626413,140.506405900464,
141.505566174514,142.504726448565,143.503886722616,144.503046996666,145.502207270717,
146.501367544768,147.500527818819,148.499688092869,149.49884836692,150.498008640971,
151.497168915021,152.496329189072,153.495489463123,154.494649737173,155.493810011224,
156.492970285275,157.492130559325,158.491290833376,159.490451107427,160.489611381477,
161.488771655528,162.487931929579,163.487092203629,164.48625247768,165.485412751731,
166.484573025782,167.483733299832,168.482893573883,169.482053847934,170.481214121984,
171.480374396035,172.479534670086,173.478694944136,174.477855218187,175.477015492238,
176.476175766288,177.475336040339,178.47449631439,179.47365658844,180.472816862491,
181.471977136542,182.471137410592,183.470297684643,184.469457958694,185.468618232745,
186.467778506795,187.466938780846,188.466099054897,189.465259328947,190.464419602998,
191.463579877049,192.462740151099,193.46190042515,194.461060699201,195.460220973251,
196.459381247302,197.458541521353,198.457701795403,199.456862069454,200.456022343505,
201.455182617555,202.454342891606,203.453503165657,204.452663439708,205.451823713758,
206.450983987809,207.45014426186,208.44930453591,209.448464809961,210.447625084012,
211.446785358062,212.445945632113,213.445105906164,214.444266180214,215.443426454265,
216.442586728316,217.441747002366,218.440907276417,219.440067550468,220.439227824519,
221.438388098569,222.43754837262,223.436708646671,224.435868920721,225.435029194772,
226.434189468823,227.433349742873,228.432510016924,229.431670290975,230.430830565025,
231.429990839076,232.429151113127,233.428311387177,234.427471661228,235.426631935279,
236.42579220933,237.42495248338,238.424112757431,239.423273031482,240.422433305532,
241.421593579583,242.420753853634,243.419914127684,244.419074401735,245.418234675786,
246.417394949836,247.416555223887,248.415715497938,249.414875771988,250.414036046039,
251.41319632009,252.41235659414,253.411516868191,254.410677142242,255.409837416293,
256.408997690343,257.408157964394,258.407318238445,259.406478512495,260.405638786546,
261.404799060597,262.403959334647,263.403119608698,264.402279882749,265.401440156799,
266.40060043085,267.399760704901,268.398920978951,269.398081253002,270.397241527053,
271.396401801103,272.395562075154,273.394722349205,274.393882623256,275.393042897306,
276.392203171357,277.391363445408,278.390523719458,279.389683993509,280.38884426756,
281.38800454161,282.387164815661,283.386325089712,284.385485363762,285.384645637813,
286.383805911864,287.382966185914,288.382126459965,289.381286734016,290.380447008066,
291.379607282117,292.378767556168,293.377927830219,294.377088104269,295.37624837832,
296.375408652371,297.374568926421,298.373729200472,299.372889474523,300.372049748573,
301.371210022624,302.370370296675,303.369530570725,304.368690844776,305.367851118827,
306.367011392877,307.366171666928,308.365331940979,309.364492215029,310.36365248908,
311.362812763131,312.361973037182,313.361133311232,314.360293585283,315.359453859334,
316.358614133384,317.357774407435,318.356934681486,319.356094955536,320.355255229587,
321.354415503638,322.353575777688,323.352736051739,324.35189632579,325.35105659984,
326.350216873891,327.349377147942,328.348537421993,329.347697696043,330.346857970094,
331.346018244145,332.345178518195,333.344338792246,334.343499066297,335.342659340347,
336.341819614398,337.340979888449,338.340140162499,339.33930043655,340.338460710601,
341.337620984651,342.336781258702,343.335941532753,344.335101806803,345.334262080854,
346.333422354905,347.332582628956,348.331742903006,349.330903177057,350.330063451108,
351.329223725158,352.328383999209,353.32754427326,354.32670454731,355.325864821361,
356.325025095412,357.324185369462,358.323345643513,359.322505917564,360.321666191614,
361.320826465665,362.319986739716,363.319147013766,364.318307287817,365.317467561868,
366.316627835919,367.315788109969,368.31494838402,369.314108658071,370.313268932121,
371.312429206172,372.311589480223,373.310749754273,374.309910028324,375.309070302375,
376.308230576425,377.307390850476,378.306551124527,379.305711398577,380.304871672628,
381.304031946679,382.303192220729,383.30235249478,384.301512768831,385.300673042882,
386.299833316932,387.298993590983,388.298153865034,389.297314139084,390.296474413135,
391.295634687186,392.294794961236,393.293955235287,394.293115509338,395.292275783388,
396.291436057439,397.29059633149,398.289756605541,399.288916879591,400.288077153642,
401.287237427693,402.286397701743,403.285557975794,404.284718249845,405.283878523895,
406.283038797946,407.282199071997,408.281359346047,409.280519620098,410.279679894149,
411.278840168199,412.27800044225,413.277160716301,414.276320990351,415.275481264402,
416.274641538453,417.273801812504,418.272962086554,419.272122360605,420.271282634656,
421.270442908706,422.269603182757,423.268763456808,424.267923730858,425.267084004909,
426.26624427896,427.26540455301,428.264564827061,429.263725101112,430.262885375162,
431.262045649213,432.261205923264,433.260366197314,434.259526471365,435.258686745416,
436.257847019467,437.257007293517,438.256167567568,439.255327841619,440.254488115669,
441.25364838972,442.252808663771,443.251968937821,444.251129211872,445.250289485923,
446.249449759973,447.248610034024,448.247770308075,449.246930582125,450.246090856176,
451.245251130227,452.244411404278,453.243571678328,454.242731952379,455.24189222643,
456.24105250048,457.240212774531,458.239373048582,459.238533322632,460.237693596683,
461.236853870734,462.236014144784,463.235174418835,464.234334692886,465.233494966936,
466.232655240987,467.231815515038,468.230975789088,469.230136063139,470.22929633719,
471.228456611241,472.227616885291,473.226777159342,474.225937433393,475.225097707443,
476.224257981494,477.223418255545,478.222578529595,479.221738803646,480.220899077697,
481.220059351747,482.219219625798,483.218379899849,483.717960036874,484.217540173899),
 .UNSPECIFIED.);
#431=B_SPLINE_SURFACE_WITH_KNOTS('',3,3,((#81664,#81665,#81666,#81667,#81668,
#81669,#81670,#81671,#81672,#81673,#81674,#81675,#81676,#81677,#81678,#81679,
#81680,#81681,#81682,#81683,#81684,#81685,#81686,#81687,#81688,#81689,#81690,
#81691,#81692,#81693,#81694,#81695,#81696,#81697,#81698,#81699,#81700,#81701,
#81702,#81703,#81704,#81705,#81706,#81707,#81708,#81709,#81710),(#81711,
#81712,#81713,#81714,#81715,#81716,#81717,#81718,#81719,#81720,#81721,#81722,
#81723,#81724,#81725,#81726,#81727,#81728,#81729,#81730,#81731,#81732,#81733,
#81734,#81735,#81736,#81737,#81738,#81739,#81740,#81741,#81742,#81743,#81744,
#81745,#81746,#81747,#81748,#81749,#81750,#81751,#81752,#81753,#81754,#81755,
#81756,#81757),(#81758,#81759,#81760,#81761,#81762,#81763,#81764,#81765,
#81766,#81767,#81768,#81769,#81770,#81771,#81772,#81773,#81774,#81775,#81776,
#81777,#81778,#81779,#81780,#81781,#81782,#81783,#81784,#81785,#81786,#81787,
#81788,#81789,#81790,#81791,#81792,#81793,#81794,#81795,#81796,#81797,#81798,
#81799,#81800,#81801,#81802,#81803,#81804),(#81805,#81806,#81807,#81808,
#81809,#81810,#81811,#81812,#81813,#81814,#81815,#81816,#81817,#81818,#81819,
#81820,#81821,#81822,#81823,#81824,#81825,#81826,#81827,#81828,#81829,#81830,
#81831,#81832,#81833,#81834,#81835,#81836,#81837,#81838,#81839,#81840,#81841,
#81842,#81843,#81844,#81845,#81846,#81847,#81848,#81849,#81850,#81851)),
 .UNSPECIFIED.,.F.,.F.,.F.,(4,4),(4,1,1,1,1,1,1,1,1,1,1,1,1,1,1,1,1,1,1,
1,1,1,1,1,1,1,1,1,1,1,1,1,1,1,1,1,1,1,1,1,1,1,1,1,4),(0.,0.0329955678841871),
(8.30203615430838,9.29820029578191,10.2943644372554,11.290528578729,12.2866927202025,
13.282856861676,14.2790210031496,15.2751851446231,16.2713492860966,17.2675134275701,
18.2636775690437,19.2598417105172,20.2560058519907,21.2521699934642,22.2483341349378,
23.2444982764113,24.2406624178848,25.2368265593584,26.2329907008319,27.2291548423054,
28.225318983779,29.2214831252525,30.217647266726,31.2138114081995,32.2099755496731,
33.2061396911466,34.2023038326201,35.1984679740937,36.1946321155672,37.1907962570407,
38.1869603985142,39.1831245399878,40.1792886814613,41.1754528229348,42.1716169644084,
43.1677811058819,44.1639452473554,45.1601093888289,46.1562735303025,47.152437671776,
48.1486018132495,49.1447659547231,50.1409300961966,51.1370942376701,52.1332583791436),
 .UNSPECIFIED.);
#432=B_SPLINE_SURFACE_WITH_KNOTS('',3,3,((#82060,#82061,#82062,#82063,#82064,
#82065,#82066,#82067,#82068,#82069,#82070,#82071,#82072,#82073,#82074,#82075,
#82076,#82077,#82078,#82079,#82080,#82081,#82082,#82083,#82084,#82085,#82086,
#82087,#82088,#82089,#82090,#82091,#82092,#82093,#82094,#82095,#82096,#82097,
#82098,#82099,#82100,#82101,#82102,#82103,#82104,#82105,#82106),(#82107,
#82108,#82109,#82110,#82111,#82112,#82113,#82114,#82115,#82116,#82117,#82118,
#82119,#82120,#82121,#82122,#82123,#82124,#82125,#82126,#82127,#82128,#82129,
#82130,#82131,#82132,#82133,#82134,#82135,#82136,#82137,#82138,#82139,#82140,
#82141,#82142,#82143,#82144,#82145,#82146,#82147,#82148,#82149,#82150,#82151,
#82152,#82153),(#82154,#82155,#82156,#82157,#82158,#82159,#82160,#82161,
#82162,#82163,#82164,#82165,#82166,#82167,#82168,#82169,#82170,#82171,#82172,
#82173,#82174,#82175,#82176,#82177,#82178,#82179,#82180,#82181,#82182,#82183,
#82184,#82185,#82186,#82187,#82188,#82189,#82190,#82191,#82192,#82193,#82194,
#82195,#82196,#82197,#82198,#82199,#82200),(#82201,#82202,#82203,#82204,
#82205,#82206,#82207,#82208,#82209,#82210,#82211,#82212,#82213,#82214,#82215,
#82216,#82217,#82218,#82219,#82220,#82221,#82222,#82223,#82224,#82225,#82226,
#82227,#82228,#82229,#82230,#82231,#82232,#82233,#82234,#82235,#82236,#82237,
#82238,#82239,#82240,#82241,#82242,#82243,#82244,#82245,#82246,#82247)),
 .UNSPECIFIED.,.F.,.F.,.F.,(4,4),(4,1,1,1,1,1,1,1,1,1,1,1,1,1,1,1,1,1,1,
1,1,1,1,1,1,1,1,1,1,1,1,1,1,1,1,1,1,1,1,1,1,1,1,1,4),(0.,0.0329955678841871),
(11.6159397475004,12.6121038889739,13.6082680304475,14.604432171921,15.6005963133945,
16.5967604548681,17.5929245963416,18.5890887378151,19.5852528792886,20.5814170207622,
21.5775811622357,22.5737453037092,23.5699094451828,24.5660735866563,25.5622377281298,
26.5584018696034,27.5545660110769,28.5507301525504,29.5468942940239,30.5430584354975,
31.539222576971,32.5353867184445,33.531550859918,34.5277150013916,35.5238791428651,
36.5200432843386,37.5162074258122,38.5123715672857,39.5085357087592,40.5046998502328,
41.5008639917063,42.4970281331798,43.4931922746533,44.4893564161269,45.4855205576004,
46.4816846990739,47.4778488405475,48.474012982021,49.4701771234945,50.466341264968,
51.4625054064416,52.4586695479151,53.4548336893886,54.4509978308621,55.4471619723357),
 .UNSPECIFIED.);
#433=CYLINDRICAL_SURFACE('',#30907,1.55);
#434=CYLINDRICAL_SURFACE('',#30911,1.55);
#435=CYLINDRICAL_SURFACE('',#30916,4.5);
#436=CYLINDRICAL_SURFACE('',#30923,4.5);
#437=CYLINDRICAL_SURFACE('',#30930,4.5);
#438=CYLINDRICAL_SURFACE('',#30937,4.5);
#439=CYLINDRICAL_SURFACE('',#31038,4.05);
#440=CYLINDRICAL_SURFACE('',#31042,3.05);
#441=CYLINDRICAL_SURFACE('',#31046,3.05);
#442=CYLINDRICAL_SURFACE('',#31050,3.05);
#443=CYLINDRICAL_SURFACE('',#31054,3.05000000000001);
#444=CYLINDRICAL_SURFACE('',#31058,3.05);
#445=CYLINDRICAL_SURFACE('',#31062,3.05000000000001);
#446=CYLINDRICAL_SURFACE('',#31066,3.05);
#447=CYLINDRICAL_SURFACE('',#31070,3.05);
#448=CYLINDRICAL_SURFACE('',#31074,3.05000000000001);
#449=CYLINDRICAL_SURFACE('',#31078,3.05);
#450=CYLINDRICAL_SURFACE('',#31082,3.05000000000001);
#451=CYLINDRICAL_SURFACE('',#31086,3.05);
#452=CYLINDRICAL_SURFACE('',#31090,7.);
#453=CYLINDRICAL_SURFACE('',#31093,7.);
#454=CYLINDRICAL_SURFACE('',#31096,7.);
#455=CYLINDRICAL_SURFACE('',#31099,7.);
#456=CYLINDRICAL_SURFACE('',#31118,5.5);
#457=CYLINDRICAL_SURFACE('',#31148,2.05);
#458=CYLINDRICAL_SURFACE('',#31152,2.05);
#459=CYLINDRICAL_SURFACE('',#31178,3.);
#460=CYLINDRICAL_SURFACE('',#31180,12.);
#461=CYLINDRICAL_SURFACE('',#31197,12.);
#462=CYLINDRICAL_SURFACE('',#31201,12.);
#463=CYLINDRICAL_SURFACE('',#31205,12.);
#464=CYLINDRICAL_SURFACE('',#31241,3.);
#465=CYLINDRICAL_SURFACE('',#31244,3.);
#466=CYLINDRICAL_SURFACE('',#31277,3.);
#467=CYLINDRICAL_SURFACE('',#31279,3.);
#468=CYLINDRICAL_SURFACE('',#31281,3.);
#469=CYLINDRICAL_SURFACE('',#31283,3.);
#470=CYLINDRICAL_SURFACE('',#31285,3.);
#471=CYLINDRICAL_SURFACE('',#31287,3.);
#472=CYLINDRICAL_SURFACE('',#31289,3.);
#473=CYLINDRICAL_SURFACE('',#31296,5.025);
#474=CYLINDRICAL_SURFACE('',#31297,1.5);
#475=CYLINDRICAL_SURFACE('',#31298,1.5);
#476=CYLINDRICAL_SURFACE('',#31301,4.5);
#477=CYLINDRICAL_SURFACE('',#31304,5.);
#478=CYLINDRICAL_SURFACE('',#31309,4.2379);
#479=CYLINDRICAL_SURFACE('',#31312,5.);
#480=CYLINDRICAL_SURFACE('',#31315,5.);
#481=CYLINDRICAL_SURFACE('',#31318,3.);
#482=CYLINDRICAL_SURFACE('',#31320,3.);
#483=CYLINDRICAL_SURFACE('',#31325,4.5);
#484=CYLINDRICAL_SURFACE('',#31332,4.5);
#485=CYLINDRICAL_SURFACE('',#31339,4.5);
#486=CYLINDRICAL_SURFACE('',#31346,4.5);
#487=CYLINDRICAL_SURFACE('',#31353,4.5);
#488=CYLINDRICAL_SURFACE('',#31360,4.5);
#489=CYLINDRICAL_SURFACE('',#31367,4.5);
#490=CYLINDRICAL_SURFACE('',#31374,4.5);
#491=CYLINDRICAL_SURFACE('',#31381,2.);
#492=CYLINDRICAL_SURFACE('',#31392,3.5);
#493=CYLINDRICAL_SURFACE('',#31399,3.5);
#494=CYLINDRICAL_SURFACE('',#31412,4.5);
#495=CYLINDRICAL_SURFACE('',#31419,4.5);
#496=CYLINDRICAL_SURFACE('',#31476,7.05);
#497=CYLINDRICAL_SURFACE('',#31480,7.05);
#498=CYLINDRICAL_SURFACE('',#31489,4.05);
#499=CYLINDRICAL_SURFACE('',#31493,4.05);
#500=CYLINDRICAL_SURFACE('',#31497,4.05);
#501=CYLINDRICAL_SURFACE('',#31501,4.05);
#502=CYLINDRICAL_SURFACE('',#31505,4.05);
#503=CYLINDRICAL_SURFACE('',#31509,4.05);
#504=CYLINDRICAL_SURFACE('',#31513,4.05);
#505=CYLINDRICAL_SURFACE('',#31517,4.05);
#506=CYLINDRICAL_SURFACE('',#31521,4.05);
#507=CYLINDRICAL_SURFACE('',#31525,4.05);
#508=CYLINDRICAL_SURFACE('',#31529,4.05);
#509=CYLINDRICAL_SURFACE('',#31533,4.05);
#510=CYLINDRICAL_SURFACE('',#31539,4.05);
#511=CYLINDRICAL_SURFACE('',#31543,4.05);
#512=CYLINDRICAL_SURFACE('',#31547,4.05);
#513=CYLINDRICAL_SURFACE('',#31551,4.05);
#514=CYLINDRICAL_SURFACE('',#31555,4.05);
#515=CYLINDRICAL_SURFACE('',#31559,4.05);
#516=CYLINDRICAL_SURFACE('',#31563,4.05);
#517=CYLINDRICAL_SURFACE('',#31567,4.05);
#518=CYLINDRICAL_SURFACE('',#31571,7.5);
#519=CYLINDRICAL_SURFACE('',#31575,7.5);
#520=CYLINDRICAL_SURFACE('',#31579,7.5);
#521=CYLINDRICAL_SURFACE('',#31583,7.5);
#522=CYLINDRICAL_SURFACE('',#31587,7.5);
#523=CYLINDRICAL_SURFACE('',#31591,7.5);
#524=CYLINDRICAL_SURFACE('',#31595,7.5);
#525=CYLINDRICAL_SURFACE('',#31652,7.);
#526=CYLINDRICAL_SURFACE('',#31655,7.);
#527=CYLINDRICAL_SURFACE('',#31658,7.);
#528=CYLINDRICAL_SURFACE('',#31661,7.);
#529=CYLINDRICAL_SURFACE('',#31664,7.);
#530=CYLINDRICAL_SURFACE('',#31667,7.);
#531=CYLINDRICAL_SURFACE('',#31670,7.);
#532=CYLINDRICAL_SURFACE('',#31673,7.);
#533=CYLINDRICAL_SURFACE('',#31676,7.);
#534=CYLINDRICAL_SURFACE('',#31679,7.);
#535=CYLINDRICAL_SURFACE('',#31704,6.5);
#536=CYLINDRICAL_SURFACE('',#31707,6.5);
#537=CYLINDRICAL_SURFACE('',#31708,4.2379);
#538=CYLINDRICAL_SURFACE('',#31720,3.25);
#539=CYLINDRICAL_SURFACE('',#31723,3.25);
#540=CYLINDRICAL_SURFACE('',#31755,1.7);
#541=CYLINDRICAL_SURFACE('',#31756,1.7);
#542=CYLINDRICAL_SURFACE('',#31757,1.5);
#543=CYLINDRICAL_SURFACE('',#31758,1.5);
#544=CYLINDRICAL_SURFACE('',#31761,4.5);
#545=CYLINDRICAL_SURFACE('',#31764,7.05);
#546=CYLINDRICAL_SURFACE('',#31767,0.4);
#547=CYLINDRICAL_SURFACE('',#31776,0.4);
#548=CYLINDRICAL_SURFACE('',#31785,3.933);
#549=CYLINDRICAL_SURFACE('',#31787,3.933);
#550=CYLINDRICAL_SURFACE('',#31788,3.933);
#551=CYLINDRICAL_SURFACE('',#31789,3.933);
#552=CYLINDRICAL_SURFACE('',#31790,3.933);
#553=CYLINDRICAL_SURFACE('',#31791,3.933);
#554=CYLINDRICAL_SURFACE('',#31792,3.933);
#555=CYLINDRICAL_SURFACE('',#31793,3.933);
#556=CYLINDRICAL_SURFACE('',#31794,3.933);
#557=CYLINDRICAL_SURFACE('',#31795,3.933);
#558=CYLINDRICAL_SURFACE('',#31796,3.22275);
#559=CYLINDRICAL_SURFACE('',#31798,3.22275);
#560=CYLINDRICAL_SURFACE('',#31799,3.22275);
#561=CYLINDRICAL_SURFACE('',#31800,3.22275);
#562=CYLINDRICAL_SURFACE('',#31801,3.22275);
#563=CYLINDRICAL_SURFACE('',#31802,3.22275);
#564=CYLINDRICAL_SURFACE('',#31803,3.22275);
#565=CYLINDRICAL_SURFACE('',#31804,3.22275);
#566=CYLINDRICAL_SURFACE('',#31805,3.22275);
#567=CYLINDRICAL_SURFACE('',#31806,3.22275);
#568=CYLINDRICAL_SURFACE('',#31814,3.22275);
#569=CYLINDRICAL_SURFACE('',#32047,5.);
#570=CYLINDRICAL_SURFACE('',#32054,3.933);
#571=CYLINDRICAL_SURFACE('',#32058,3.25);
#572=CYLINDRICAL_SURFACE('',#32061,8.);
#573=CYLINDRICAL_SURFACE('',#32067,5.25);
#574=CYLINDRICAL_SURFACE('',#32072,15.);
#575=CYLINDRICAL_SURFACE('',#32083,5.);
#576=CYLINDRICAL_SURFACE('',#32098,4.5);
#577=CYLINDRICAL_SURFACE('',#32102,2.225);
#578=CYLINDRICAL_SURFACE('',#32108,1.954);
#579=CYLINDRICAL_SURFACE('',#32110,1.954);
#580=CYLINDRICAL_SURFACE('',#32111,1.954);
#581=CYLINDRICAL_SURFACE('',#32112,1.954);
#582=CYLINDRICAL_SURFACE('',#32113,1.954);
#583=CYLINDRICAL_SURFACE('',#32114,1.954);
#584=CYLINDRICAL_SURFACE('',#32115,1.954);
#585=CYLINDRICAL_SURFACE('',#32116,1.954);
#586=CYLINDRICAL_SURFACE('',#32117,1.954);
#587=CYLINDRICAL_SURFACE('',#32118,1.954);
#588=CYLINDRICAL_SURFACE('',#32119,1.954);
#589=CYLINDRICAL_SURFACE('',#32120,1.954);
#590=CYLINDRICAL_SURFACE('',#32121,1.954);
#591=CYLINDRICAL_SURFACE('',#32122,1.954);
#592=CYLINDRICAL_SURFACE('',#32123,1.954);
#593=CYLINDRICAL_SURFACE('',#32124,1.954);
#594=CYLINDRICAL_SURFACE('',#32125,1.954);
#595=CYLINDRICAL_SURFACE('',#32126,1.954);
#596=CYLINDRICAL_SURFACE('',#32127,1.954);
#597=CYLINDRICAL_SURFACE('',#32128,1.954);
#598=CYLINDRICAL_SURFACE('',#32129,1.954);
#599=CYLINDRICAL_SURFACE('',#32130,1.954);
#600=CYLINDRICAL_SURFACE('',#32131,1.954);
#601=CYLINDRICAL_SURFACE('',#32132,1.954);
#602=CYLINDRICAL_SURFACE('',#32133,1.954);
#603=CYLINDRICAL_SURFACE('',#32134,1.954);
#604=CYLINDRICAL_SURFACE('',#32135,1.954);
#605=CYLINDRICAL_SURFACE('',#32136,1.954);
#606=CYLINDRICAL_SURFACE('',#32137,1.954);
#607=CYLINDRICAL_SURFACE('',#32138,1.954);
#608=CYLINDRICAL_SURFACE('',#32139,1.954);
#609=CYLINDRICAL_SURFACE('',#32140,1.954);
#610=CYLINDRICAL_SURFACE('',#32141,1.954);
#611=CYLINDRICAL_SURFACE('',#32142,1.954);
#612=CYLINDRICAL_SURFACE('',#32143,1.954);
#613=CYLINDRICAL_SURFACE('',#32144,1.954);
#614=CYLINDRICAL_SURFACE('',#32145,1.954);
#615=CYLINDRICAL_SURFACE('',#32146,1.954);
#616=CYLINDRICAL_SURFACE('',#32147,1.954);
#617=CYLINDRICAL_SURFACE('',#32148,1.954);
#618=CYLINDRICAL_SURFACE('',#32149,1.954);
#619=CYLINDRICAL_SURFACE('',#32150,1.954);
#620=CYLINDRICAL_SURFACE('',#32151,1.5555);
#621=CYLINDRICAL_SURFACE('',#32153,1.5555);
#622=CYLINDRICAL_SURFACE('',#32154,1.5555);
#623=CYLINDRICAL_SURFACE('',#32155,1.5555);
#624=CYLINDRICAL_SURFACE('',#32156,1.5555);
#625=CYLINDRICAL_SURFACE('',#32157,1.5555);
#626=CYLINDRICAL_SURFACE('',#32158,1.5555);
#627=CYLINDRICAL_SURFACE('',#32159,1.5555);
#628=CYLINDRICAL_SURFACE('',#32160,1.5555);
#629=CYLINDRICAL_SURFACE('',#32161,1.5555);
#630=CYLINDRICAL_SURFACE('',#32162,1.5555);
#631=CYLINDRICAL_SURFACE('',#32163,1.5555);
#632=CYLINDRICAL_SURFACE('',#32164,1.5555);
#633=CYLINDRICAL_SURFACE('',#32165,1.5555);
#634=CYLINDRICAL_SURFACE('',#32166,1.5555);
#635=CYLINDRICAL_SURFACE('',#32167,1.5555);
#636=CYLINDRICAL_SURFACE('',#32168,1.5555);
#637=CYLINDRICAL_SURFACE('',#32169,1.5555);
#638=CYLINDRICAL_SURFACE('',#32170,1.5555);
#639=CYLINDRICAL_SURFACE('',#32171,1.5555);
#640=CYLINDRICAL_SURFACE('',#32172,1.5555);
#641=CYLINDRICAL_SURFACE('',#32173,1.5555);
#642=CYLINDRICAL_SURFACE('',#32174,1.5555);
#643=CYLINDRICAL_SURFACE('',#32175,1.5555);
#644=CYLINDRICAL_SURFACE('',#32176,1.5555);
#645=CYLINDRICAL_SURFACE('',#32177,1.5555);
#646=CYLINDRICAL_SURFACE('',#32178,1.5555);
#647=CYLINDRICAL_SURFACE('',#32179,1.5555);
#648=CYLINDRICAL_SURFACE('',#32180,1.5555);
#649=CYLINDRICAL_SURFACE('',#32181,1.5555);
#650=CYLINDRICAL_SURFACE('',#32182,1.5555);
#651=CYLINDRICAL_SURFACE('',#32183,1.5555);
#652=CYLINDRICAL_SURFACE('',#32184,1.5555);
#653=CYLINDRICAL_SURFACE('',#32185,1.5555);
#654=CYLINDRICAL_SURFACE('',#32186,1.5555);
#655=CYLINDRICAL_SURFACE('',#32187,1.5555);
#656=CYLINDRICAL_SURFACE('',#32188,1.5555);
#657=CYLINDRICAL_SURFACE('',#32189,1.5555);
#658=CYLINDRICAL_SURFACE('',#32190,1.5555);
#659=CYLINDRICAL_SURFACE('',#32191,1.5555);
#660=CYLINDRICAL_SURFACE('',#32192,1.5555);
#661=CYLINDRICAL_SURFACE('',#32193,1.5555);
#662=CYLINDRICAL_SURFACE('',#32200,1.5555);
#663=CYLINDRICAL_SURFACE('',#32206,1.954);
#664=CYLINDRICAL_SURFACE('',#32439,3.5);
#665=CYLINDRICAL_SURFACE('',#32449,1.5);
#666=CYLINDRICAL_SURFACE('',#32455,1.4635);
#667=CYLINDRICAL_SURFACE('',#32457,1.4635);
#668=CYLINDRICAL_SURFACE('',#32458,1.4635);
#669=CYLINDRICAL_SURFACE('',#32459,1.4635);
#670=CYLINDRICAL_SURFACE('',#32460,1.4635);
#671=CYLINDRICAL_SURFACE('',#32461,1.4635);
#672=CYLINDRICAL_SURFACE('',#32462,1.4635);
#673=CYLINDRICAL_SURFACE('',#32463,1.4635);
#674=CYLINDRICAL_SURFACE('',#32464,1.4635);
#675=CYLINDRICAL_SURFACE('',#32465,1.4635);
#676=CYLINDRICAL_SURFACE('',#32466,1.4635);
#677=CYLINDRICAL_SURFACE('',#32467,1.4635);
#678=CYLINDRICAL_SURFACE('',#32468,1.4635);
#679=CYLINDRICAL_SURFACE('',#32469,1.4635);
#680=CYLINDRICAL_SURFACE('',#32470,1.4635);
#681=CYLINDRICAL_SURFACE('',#32471,1.4635);
#682=CYLINDRICAL_SURFACE('',#32472,1.4635);
#683=CYLINDRICAL_SURFACE('',#32473,1.4635);
#684=CYLINDRICAL_SURFACE('',#32474,1.4635);
#685=CYLINDRICAL_SURFACE('',#32475,1.4635);
#686=CYLINDRICAL_SURFACE('',#32476,1.4635);
#687=CYLINDRICAL_SURFACE('',#32477,1.4635);
#688=CYLINDRICAL_SURFACE('',#32478,1.4635);
#689=CYLINDRICAL_SURFACE('',#32479,1.4635);
#690=CYLINDRICAL_SURFACE('',#32480,1.4635);
#691=CYLINDRICAL_SURFACE('',#32481,1.4635);
#692=CYLINDRICAL_SURFACE('',#32482,1.4635);
#693=CYLINDRICAL_SURFACE('',#32483,1.4635);
#694=CYLINDRICAL_SURFACE('',#32484,1.4635);
#695=CYLINDRICAL_SURFACE('',#32485,1.4635);
#696=CYLINDRICAL_SURFACE('',#32486,1.4635);
#697=CYLINDRICAL_SURFACE('',#32487,1.4635);
#698=CYLINDRICAL_SURFACE('',#32488,1.4635);
#699=CYLINDRICAL_SURFACE('',#32489,1.4635);
#700=CYLINDRICAL_SURFACE('',#32490,1.4635);
#701=CYLINDRICAL_SURFACE('',#32491,1.4635);
#702=CYLINDRICAL_SURFACE('',#32492,1.4635);
#703=CYLINDRICAL_SURFACE('',#32493,1.4635);
#704=CYLINDRICAL_SURFACE('',#32494,1.4635);
#705=CYLINDRICAL_SURFACE('',#32495,1.4635);
#706=CYLINDRICAL_SURFACE('',#32496,1.4635);
#707=CYLINDRICAL_SURFACE('',#32497,1.4635);
#708=CYLINDRICAL_SURFACE('',#32498,1.4635);
#709=CYLINDRICAL_SURFACE('',#32499,1.4635);
#710=CYLINDRICAL_SURFACE('',#32500,1.4635);
#711=CYLINDRICAL_SURFACE('',#32501,1.4635);
#712=CYLINDRICAL_SURFACE('',#32502,1.4635);
#713=CYLINDRICAL_SURFACE('',#32503,1.4635);
#714=CYLINDRICAL_SURFACE('',#32504,1.4635);
#715=CYLINDRICAL_SURFACE('',#32505,1.4635);
#716=CYLINDRICAL_SURFACE('',#32506,1.4635);
#717=CYLINDRICAL_SURFACE('',#32507,1.4635);
#718=CYLINDRICAL_SURFACE('',#32508,1.4635);
#719=CYLINDRICAL_SURFACE('',#32509,1.4635);
#720=CYLINDRICAL_SURFACE('',#32510,1.4635);
#721=CYLINDRICAL_SURFACE('',#32511,1.4635);
#722=CYLINDRICAL_SURFACE('',#32512,1.4635);
#723=CYLINDRICAL_SURFACE('',#32513,1.4635);
#724=CYLINDRICAL_SURFACE('',#32514,1.4635);
#725=CYLINDRICAL_SURFACE('',#32515,1.4635);
#726=CYLINDRICAL_SURFACE('',#32516,1.4635);
#727=CYLINDRICAL_SURFACE('',#32517,1.4635);
#728=CYLINDRICAL_SURFACE('',#32518,1.4635);
#729=CYLINDRICAL_SURFACE('',#32519,1.4635);
#730=CYLINDRICAL_SURFACE('',#32520,1.4635);
#731=CYLINDRICAL_SURFACE('',#32521,1.4635);
#732=CYLINDRICAL_SURFACE('',#32522,1.4635);
#733=CYLINDRICAL_SURFACE('',#32523,1.4635);
#734=CYLINDRICAL_SURFACE('',#32524,1.4635);
#735=CYLINDRICAL_SURFACE('',#32525,1.17775);
#736=CYLINDRICAL_SURFACE('',#32527,1.17775);
#737=CYLINDRICAL_SURFACE('',#32528,1.17775);
#738=CYLINDRICAL_SURFACE('',#32529,1.17775);
#739=CYLINDRICAL_SURFACE('',#32530,1.17775);
#740=CYLINDRICAL_SURFACE('',#32531,1.17775);
#741=CYLINDRICAL_SURFACE('',#32532,1.17775);
#742=CYLINDRICAL_SURFACE('',#32533,1.17775);
#743=CYLINDRICAL_SURFACE('',#32534,1.17775);
#744=CYLINDRICAL_SURFACE('',#32535,1.17775);
#745=CYLINDRICAL_SURFACE('',#32536,1.17775);
#746=CYLINDRICAL_SURFACE('',#32537,1.17775);
#747=CYLINDRICAL_SURFACE('',#32538,1.17775);
#748=CYLINDRICAL_SURFACE('',#32539,1.17775);
#749=CYLINDRICAL_SURFACE('',#32540,1.17775);
#750=CYLINDRICAL_SURFACE('',#32541,1.17775);
#751=CYLINDRICAL_SURFACE('',#32542,1.17775);
#752=CYLINDRICAL_SURFACE('',#32543,1.17775);
#753=CYLINDRICAL_SURFACE('',#32544,1.17775);
#754=CYLINDRICAL_SURFACE('',#32545,1.17775);
#755=CYLINDRICAL_SURFACE('',#32546,1.17775);
#756=CYLINDRICAL_SURFACE('',#32547,1.17775);
#757=CYLINDRICAL_SURFACE('',#32548,1.17775);
#758=CYLINDRICAL_SURFACE('',#32549,1.17775);
#759=CYLINDRICAL_SURFACE('',#32550,1.17775);
#760=CYLINDRICAL_SURFACE('',#32551,1.17775);
#761=CYLINDRICAL_SURFACE('',#32552,1.17775);
#762=CYLINDRICAL_SURFACE('',#32553,1.17775);
#763=CYLINDRICAL_SURFACE('',#32554,1.17775);
#764=CYLINDRICAL_SURFACE('',#32555,1.17775);
#765=CYLINDRICAL_SURFACE('',#32556,1.17775);
#766=CYLINDRICAL_SURFACE('',#32557,1.17775);
#767=CYLINDRICAL_SURFACE('',#32558,1.17775);
#768=CYLINDRICAL_SURFACE('',#32559,1.17775);
#769=CYLINDRICAL_SURFACE('',#32560,1.17775);
#770=CYLINDRICAL_SURFACE('',#32561,1.17775);
#771=CYLINDRICAL_SURFACE('',#32562,1.17775);
#772=CYLINDRICAL_SURFACE('',#32563,1.17775);
#773=CYLINDRICAL_SURFACE('',#32564,1.17775);
#774=CYLINDRICAL_SURFACE('',#32565,1.17775);
#775=CYLINDRICAL_SURFACE('',#32566,1.17775);
#776=CYLINDRICAL_SURFACE('',#32567,1.17775);
#777=CYLINDRICAL_SURFACE('',#32568,1.17775);
#778=CYLINDRICAL_SURFACE('',#32569,1.17775);
#779=CYLINDRICAL_SURFACE('',#32570,1.17775);
#780=CYLINDRICAL_SURFACE('',#32571,1.17775);
#781=CYLINDRICAL_SURFACE('',#32572,1.17775);
#782=CYLINDRICAL_SURFACE('',#32573,1.17775);
#783=CYLINDRICAL_SURFACE('',#32574,1.17775);
#784=CYLINDRICAL_SURFACE('',#32575,1.17775);
#785=CYLINDRICAL_SURFACE('',#32576,1.17775);
#786=CYLINDRICAL_SURFACE('',#32577,1.17775);
#787=CYLINDRICAL_SURFACE('',#32578,1.17775);
#788=CYLINDRICAL_SURFACE('',#32579,1.17775);
#789=CYLINDRICAL_SURFACE('',#32580,1.17775);
#790=CYLINDRICAL_SURFACE('',#32581,1.17775);
#791=CYLINDRICAL_SURFACE('',#32582,1.17775);
#792=CYLINDRICAL_SURFACE('',#32583,1.17775);
#793=CYLINDRICAL_SURFACE('',#32584,1.17775);
#794=CYLINDRICAL_SURFACE('',#32585,1.17775);
#795=CYLINDRICAL_SURFACE('',#32586,1.17775);
#796=CYLINDRICAL_SURFACE('',#32587,1.17775);
#797=CYLINDRICAL_SURFACE('',#32588,1.17775);
#798=CYLINDRICAL_SURFACE('',#32589,1.17775);
#799=CYLINDRICAL_SURFACE('',#32590,1.17775);
#800=CYLINDRICAL_SURFACE('',#32591,1.17775);
#801=CYLINDRICAL_SURFACE('',#32592,1.17775);
#802=CYLINDRICAL_SURFACE('',#32593,1.17775);
#803=CYLINDRICAL_SURFACE('',#32594,1.17775);
#804=CYLINDRICAL_SURFACE('',#32602,1.17775);
#805=CYLINDRICAL_SURFACE('',#32607,1.4635);
#806=CYLINDRICAL_SURFACE('',#32840,2.75);
#807=CYLINDRICAL_SURFACE('',#32849,12.);
#808=CYLINDRICAL_SURFACE('',#32864,12.);
#809=CYLINDRICAL_SURFACE('',#32876,12.);
#810=CYLINDRICAL_SURFACE('',#32900,12.);
#811=CYLINDRICAL_SURFACE('',#32904,7.05);
#812=CYLINDRICAL_SURFACE('',#32908,6.933);
#813=CYLINDRICAL_SURFACE('',#32910,6.933);
#814=CYLINDRICAL_SURFACE('',#32911,6.933);
#815=CYLINDRICAL_SURFACE('',#32912,6.933);
#816=CYLINDRICAL_SURFACE('',#32913,6.933);
#817=CYLINDRICAL_SURFACE('',#32914,6.933);
#818=CYLINDRICAL_SURFACE('',#32915,6.933);
#819=CYLINDRICAL_SURFACE('',#32916,6.933);
#820=CYLINDRICAL_SURFACE('',#32917,6.933);
#821=CYLINDRICAL_SURFACE('',#32918,6.933);
#822=CYLINDRICAL_SURFACE('',#32919,6.933);
#823=CYLINDRICAL_SURFACE('',#32920,6.933);
#824=CYLINDRICAL_SURFACE('',#32921,6.933);
#825=CYLINDRICAL_SURFACE('',#32922,6.933);
#826=CYLINDRICAL_SURFACE('',#32923,6.933);
#827=CYLINDRICAL_SURFACE('',#32924,6.933);
#828=CYLINDRICAL_SURFACE('',#32925,6.21925);
#829=CYLINDRICAL_SURFACE('',#32927,6.21925);
#830=CYLINDRICAL_SURFACE('',#32929,6.21925);
#831=CYLINDRICAL_SURFACE('',#32930,6.21925);
#832=CYLINDRICAL_SURFACE('',#32931,6.21925);
#833=CYLINDRICAL_SURFACE('',#32932,6.21925);
#834=CYLINDRICAL_SURFACE('',#32933,6.21925);
#835=CYLINDRICAL_SURFACE('',#32934,6.21925);
#836=CYLINDRICAL_SURFACE('',#32935,6.21925);
#837=CYLINDRICAL_SURFACE('',#32936,6.21925);
#838=CYLINDRICAL_SURFACE('',#32937,6.21925);
#839=CYLINDRICAL_SURFACE('',#32938,6.21925);
#840=CYLINDRICAL_SURFACE('',#32939,6.21925);
#841=CYLINDRICAL_SURFACE('',#32940,6.21925);
#842=CYLINDRICAL_SURFACE('',#32941,6.21925);
#843=CYLINDRICAL_SURFACE('',#32942,6.21925);
#844=CYLINDRICAL_SURFACE('',#32947,5.05);
#845=CYLINDRICAL_SURFACE('',#32956,1.55);
#846=CYLINDRICAL_SURFACE('',#32959,12.);
#847=CYLINDRICAL_SURFACE('',#32966,6.21925);
#848=CYLINDRICAL_SURFACE('',#32970,6.933);
#849=CYLINDRICAL_SURFACE('',#32979,8.);
#850=CYLINDRICAL_SURFACE('',#32983,4.954);
#851=CYLINDRICAL_SURFACE('',#32985,4.954);
#852=CYLINDRICAL_SURFACE('',#32986,4.954);
#853=CYLINDRICAL_SURFACE('',#32987,4.954);
#854=CYLINDRICAL_SURFACE('',#32988,4.954);
#855=CYLINDRICAL_SURFACE('',#32989,4.954);
#856=CYLINDRICAL_SURFACE('',#32990,4.954);
#857=CYLINDRICAL_SURFACE('',#32991,4.954);
#858=CYLINDRICAL_SURFACE('',#32992,4.954);
#859=CYLINDRICAL_SURFACE('',#32993,4.954);
#860=CYLINDRICAL_SURFACE('',#32994,4.954);
#861=CYLINDRICAL_SURFACE('',#32995,4.954);
#862=CYLINDRICAL_SURFACE('',#32996,4.954);
#863=CYLINDRICAL_SURFACE('',#32997,4.954);
#864=CYLINDRICAL_SURFACE('',#32998,4.954);
#865=CYLINDRICAL_SURFACE('',#32999,4.954);
#866=CYLINDRICAL_SURFACE('',#33000,4.954);
#867=CYLINDRICAL_SURFACE('',#33001,4.954);
#868=CYLINDRICAL_SURFACE('',#33002,4.954);
#869=CYLINDRICAL_SURFACE('',#33003,4.954);
#870=CYLINDRICAL_SURFACE('',#33004,4.954);
#871=CYLINDRICAL_SURFACE('',#33005,4.954);
#872=CYLINDRICAL_SURFACE('',#33006,4.954);
#873=CYLINDRICAL_SURFACE('',#33007,4.954);
#874=CYLINDRICAL_SURFACE('',#33008,4.954);
#875=CYLINDRICAL_SURFACE('',#33009,4.954);
#876=CYLINDRICAL_SURFACE('',#33010,4.954);
#877=CYLINDRICAL_SURFACE('',#33011,4.954);
#878=CYLINDRICAL_SURFACE('',#33012,4.954);
#879=CYLINDRICAL_SURFACE('',#33013,4.954);
#880=CYLINDRICAL_SURFACE('',#33014,4.954);
#881=CYLINDRICAL_SURFACE('',#33015,4.954);
#882=CYLINDRICAL_SURFACE('',#33016,4.954);
#883=CYLINDRICAL_SURFACE('',#33017,4.954);
#884=CYLINDRICAL_SURFACE('',#33018,4.954);
#885=CYLINDRICAL_SURFACE('',#33019,4.954);
#886=CYLINDRICAL_SURFACE('',#33020,4.954);
#887=CYLINDRICAL_SURFACE('',#33021,4.954);
#888=CYLINDRICAL_SURFACE('',#33022,4.954);
#889=CYLINDRICAL_SURFACE('',#33023,4.954);
#890=CYLINDRICAL_SURFACE('',#33024,4.954);
#891=CYLINDRICAL_SURFACE('',#33025,4.954);
#892=CYLINDRICAL_SURFACE('',#33026,4.954);
#893=CYLINDRICAL_SURFACE('',#33027,4.954);
#894=CYLINDRICAL_SURFACE('',#33028,4.954);
#895=CYLINDRICAL_SURFACE('',#33029,4.954);
#896=CYLINDRICAL_SURFACE('',#33030,4.954);
#897=CYLINDRICAL_SURFACE('',#33031,4.954);
#898=CYLINDRICAL_SURFACE('',#33032,4.954);
#899=CYLINDRICAL_SURFACE('',#33033,4.954);
#900=CYLINDRICAL_SURFACE('',#33034,4.954);
#901=CYLINDRICAL_SURFACE('',#33035,4.954);
#902=CYLINDRICAL_SURFACE('',#33036,4.954);
#903=CYLINDRICAL_SURFACE('',#33037,4.954);
#904=CYLINDRICAL_SURFACE('',#33038,4.954);
#905=CYLINDRICAL_SURFACE('',#33039,4.954);
#906=CYLINDRICAL_SURFACE('',#33040,4.954);
#907=CYLINDRICAL_SURFACE('',#33041,4.954);
#908=CYLINDRICAL_SURFACE('',#33042,4.954);
#909=CYLINDRICAL_SURFACE('',#33043,4.954);
#910=CYLINDRICAL_SURFACE('',#33044,4.954);
#911=CYLINDRICAL_SURFACE('',#33045,4.954);
#912=CYLINDRICAL_SURFACE('',#33046,4.954);
#913=CYLINDRICAL_SURFACE('',#33047,4.954);
#914=CYLINDRICAL_SURFACE('',#33048,4.954);
#915=CYLINDRICAL_SURFACE('',#33049,4.954);
#916=CYLINDRICAL_SURFACE('',#33050,4.954);
#917=CYLINDRICAL_SURFACE('',#33051,4.954);
#918=CYLINDRICAL_SURFACE('',#33052,4.954);
#919=CYLINDRICAL_SURFACE('',#33053,4.954);
#920=CYLINDRICAL_SURFACE('',#33054,4.954);
#921=CYLINDRICAL_SURFACE('',#33055,4.954);
#922=CYLINDRICAL_SURFACE('',#33056,4.954);
#923=CYLINDRICAL_SURFACE('',#33057,4.954);
#924=CYLINDRICAL_SURFACE('',#33058,4.954);
#925=CYLINDRICAL_SURFACE('',#33059,4.52375);
#926=CYLINDRICAL_SURFACE('',#33061,4.52375);
#927=CYLINDRICAL_SURFACE('',#33062,4.52375);
#928=CYLINDRICAL_SURFACE('',#33063,4.52375);
#929=CYLINDRICAL_SURFACE('',#33064,4.52375);
#930=CYLINDRICAL_SURFACE('',#33065,4.52375);
#931=CYLINDRICAL_SURFACE('',#33066,4.52375);
#932=CYLINDRICAL_SURFACE('',#33067,4.52375);
#933=CYLINDRICAL_SURFACE('',#33068,4.52375);
#934=CYLINDRICAL_SURFACE('',#33069,4.52375);
#935=CYLINDRICAL_SURFACE('',#33070,4.52375);
#936=CYLINDRICAL_SURFACE('',#33071,4.52375);
#937=CYLINDRICAL_SURFACE('',#33072,4.52375);
#938=CYLINDRICAL_SURFACE('',#33073,4.52375);
#939=CYLINDRICAL_SURFACE('',#33074,4.52375);
#940=CYLINDRICAL_SURFACE('',#33075,4.52375);
#941=CYLINDRICAL_SURFACE('',#33076,4.52375);
#942=CYLINDRICAL_SURFACE('',#33077,4.52375);
#943=CYLINDRICAL_SURFACE('',#33078,4.52375);
#944=CYLINDRICAL_SURFACE('',#33079,4.52375);
#945=CYLINDRICAL_SURFACE('',#33080,4.52375);
#946=CYLINDRICAL_SURFACE('',#33081,4.52375);
#947=CYLINDRICAL_SURFACE('',#33082,4.52375);
#948=CYLINDRICAL_SURFACE('',#33083,4.52375);
#949=CYLINDRICAL_SURFACE('',#33084,4.52375);
#950=CYLINDRICAL_SURFACE('',#33085,4.52375);
#951=CYLINDRICAL_SURFACE('',#33086,4.52375);
#952=CYLINDRICAL_SURFACE('',#33087,4.52375);
#953=CYLINDRICAL_SURFACE('',#33088,4.52375);
#954=CYLINDRICAL_SURFACE('',#33089,4.52375);
#955=CYLINDRICAL_SURFACE('',#33090,4.52375);
#956=CYLINDRICAL_SURFACE('',#33091,4.52375);
#957=CYLINDRICAL_SURFACE('',#33092,4.52375);
#958=CYLINDRICAL_SURFACE('',#33093,4.52375);
#959=CYLINDRICAL_SURFACE('',#33094,4.52375);
#960=CYLINDRICAL_SURFACE('',#33095,4.52375);
#961=CYLINDRICAL_SURFACE('',#33096,4.52375);
#962=CYLINDRICAL_SURFACE('',#33097,4.52375);
#963=CYLINDRICAL_SURFACE('',#33098,4.52375);
#964=CYLINDRICAL_SURFACE('',#33099,4.52375);
#965=CYLINDRICAL_SURFACE('',#33100,4.52375);
#966=CYLINDRICAL_SURFACE('',#33101,4.52375);
#967=CYLINDRICAL_SURFACE('',#33102,4.52375);
#968=CYLINDRICAL_SURFACE('',#33103,4.52375);
#969=CYLINDRICAL_SURFACE('',#33104,4.52375);
#970=CYLINDRICAL_SURFACE('',#33105,4.52375);
#971=CYLINDRICAL_SURFACE('',#33106,4.52375);
#972=CYLINDRICAL_SURFACE('',#33107,4.52375);
#973=CYLINDRICAL_SURFACE('',#33108,4.52375);
#974=CYLINDRICAL_SURFACE('',#33109,4.52375);
#975=CYLINDRICAL_SURFACE('',#33110,4.52375);
#976=CYLINDRICAL_SURFACE('',#33111,4.52375);
#977=CYLINDRICAL_SURFACE('',#33112,4.52375);
#978=CYLINDRICAL_SURFACE('',#33113,4.52375);
#979=CYLINDRICAL_SURFACE('',#33114,4.52375);
#980=CYLINDRICAL_SURFACE('',#33115,4.52375);
#981=CYLINDRICAL_SURFACE('',#33116,4.52375);
#982=CYLINDRICAL_SURFACE('',#33117,4.52375);
#983=CYLINDRICAL_SURFACE('',#33118,4.52375);
#984=CYLINDRICAL_SURFACE('',#33119,4.52375);
#985=CYLINDRICAL_SURFACE('',#33120,4.52375);
#986=CYLINDRICAL_SURFACE('',#33121,4.52375);
#987=CYLINDRICAL_SURFACE('',#33122,4.52375);
#988=CYLINDRICAL_SURFACE('',#33123,4.52375);
#989=CYLINDRICAL_SURFACE('',#33124,4.52375);
#990=CYLINDRICAL_SURFACE('',#33125,4.52375);
#991=CYLINDRICAL_SURFACE('',#33126,4.52375);
#992=CYLINDRICAL_SURFACE('',#33127,4.52375);
#993=CYLINDRICAL_SURFACE('',#33128,4.52375);
#994=CYLINDRICAL_SURFACE('',#33129,4.52375);
#995=CYLINDRICAL_SURFACE('',#33130,4.52375);
#996=CYLINDRICAL_SURFACE('',#33131,4.52375);
#997=CYLINDRICAL_SURFACE('',#33132,4.52375);
#998=CYLINDRICAL_SURFACE('',#33133,4.52375);
#999=CYLINDRICAL_SURFACE('',#33134,4.52375);
#1000=CYLINDRICAL_SURFACE('',#33142,4.52375);
#1001=CYLINDRICAL_SURFACE('',#33143,2.5);
#1002=CYLINDRICAL_SURFACE('',#33147,4.954);
#1003=CYLINDRICAL_SURFACE('',#33159,5.05);
#1004=CYLINDRICAL_SURFACE('',#33164,1.5);
#1005=CYLINDRICAL_SURFACE('',#33171,9.5);
#1006=CYLINDRICAL_SURFACE('',#33204,1.5);
#1007=CYLINDRICAL_SURFACE('',#33211,1.5);
#1008=CYLINDRICAL_SURFACE('',#33218,1.5);
#1009=CYLINDRICAL_SURFACE('',#33225,1.5);
#1010=CYLINDRICAL_SURFACE('',#33232,1.5);
#1011=CYLINDRICAL_SURFACE('',#33239,1.5);
#1012=CYLINDRICAL_SURFACE('',#33246,1.5);
#1013=CYLINDRICAL_SURFACE('',#33253,1.5);
#1014=CYLINDRICAL_SURFACE('',#33260,1.5);
#1015=CYLINDRICAL_SURFACE('',#33267,1.5);
#1016=CYLINDRICAL_SURFACE('',#33274,1.5);
#1017=CYLINDRICAL_SURFACE('',#33281,1.5);
#1018=CYLINDRICAL_SURFACE('',#33288,1.5);
#1019=CYLINDRICAL_SURFACE('',#33295,1.5);
#1020=CYLINDRICAL_SURFACE('',#33332,8.);
#1021=CYLINDRICAL_SURFACE('',#33339,1.4635);
#1022=CYLINDRICAL_SURFACE('',#33341,1.4635);
#1023=CYLINDRICAL_SURFACE('',#33342,1.4635);
#1024=CYLINDRICAL_SURFACE('',#33343,1.4635);
#1025=CYLINDRICAL_SURFACE('',#33344,1.4635);
#1026=CYLINDRICAL_SURFACE('',#33345,1.4635);
#1027=CYLINDRICAL_SURFACE('',#33346,1.4635);
#1028=CYLINDRICAL_SURFACE('',#33347,1.17775);
#1029=CYLINDRICAL_SURFACE('',#33349,1.17775);
#1030=CYLINDRICAL_SURFACE('',#33350,1.17775);
#1031=CYLINDRICAL_SURFACE('',#33351,1.17775);
#1032=CYLINDRICAL_SURFACE('',#33352,1.17775);
#1033=CYLINDRICAL_SURFACE('',#33353,1.17775);
#1034=CYLINDRICAL_SURFACE('',#33361,1.17775);
#1035=CYLINDRICAL_SURFACE('',#33372,1.4635);
#1036=CIRCLE('',#30903,2.05);
#1037=CIRCLE('',#30904,1.55);
#1038=CIRCLE('',#30906,2.05);
#1039=CIRCLE('',#30908,1.55);
#1040=CIRCLE('',#30910,1.55);
#1041=CIRCLE('',#30912,1.55);
#1042=CIRCLE('',#30914,4.5);
#1043=CIRCLE('',#30915,5.);
#1044=CIRCLE('',#30917,4.5);
#1045=CIRCLE('',#30919,7.);
#1046=CIRCLE('',#30921,4.5);
#1047=CIRCLE('',#30922,5.);
#1048=CIRCLE('',#30924,4.5);
#1049=CIRCLE('',#30926,7.);
#1050=CIRCLE('',#30928,4.5);
#1051=CIRCLE('',#30929,5.);
#1052=CIRCLE('',#30931,4.5);
#1053=CIRCLE('',#30933,7.);
#1054=CIRCLE('',#30935,4.5);
#1055=CIRCLE('',#30936,5.);
#1056=CIRCLE('',#30938,4.5);
#1057=CIRCLE('',#30940,7.);
#1058=CIRCLE('',#30956,3.45);
#1059=CIRCLE('',#30957,3.45);
#1060=CIRCLE('',#30958,3.45);
#1061=CIRCLE('',#30959,3.45);
#1062=CIRCLE('',#30960,3.45);
#1063=CIRCLE('',#30961,3.45);
#1064=CIRCLE('',#30962,7.4);
#1065=CIRCLE('',#30963,7.4);
#1066=CIRCLE('',#30964,5.5);
#1067=CIRCLE('',#30965,7.4);
#1068=CIRCLE('',#30966,7.4);
#1069=CIRCLE('',#30967,3.45);
#1070=CIRCLE('',#30968,3.45);
#1071=CIRCLE('',#30969,3.45);
#1072=CIRCLE('',#30970,3.45);
#1073=CIRCLE('',#30971,3.45);
#1074=CIRCLE('',#30972,3.45);
#1075=CIRCLE('',#30975,4.45);
#1076=CIRCLE('',#30976,4.9);
#1077=CIRCLE('',#30977,4.9);
#1078=CIRCLE('',#30978,4.9);
#1079=CIRCLE('',#30979,4.9);
#1080=CIRCLE('',#31037,4.05);
#1081=CIRCLE('',#31039,4.05);
#1082=CIRCLE('',#31041,3.05);
#1083=CIRCLE('',#31043,3.05);
#1084=CIRCLE('',#31045,3.05);
#1085=CIRCLE('',#31047,3.05);
#1086=CIRCLE('',#31049,3.05);
#1087=CIRCLE('',#31051,3.05);
#1088=CIRCLE('',#31053,3.05000000000001);
#1089=CIRCLE('',#31055,3.05000000000001);
#1090=CIRCLE('',#31057,3.05);
#1091=CIRCLE('',#31059,3.05);
#1092=CIRCLE('',#31061,3.05000000000001);
#1093=CIRCLE('',#31063,3.05000000000001);
#1094=CIRCLE('',#31065,3.05);
#1095=CIRCLE('',#31067,3.05);
#1096=CIRCLE('',#31069,3.05);
#1097=CIRCLE('',#31071,3.05);
#1098=CIRCLE('',#31073,3.05000000000001);
#1099=CIRCLE('',#31075,3.05000000000001);
#1100=CIRCLE('',#31077,3.05);
#1101=CIRCLE('',#31079,3.05);
#1102=CIRCLE('',#31081,3.05000000000001);
#1103=CIRCLE('',#31083,3.05000000000001);
#1104=CIRCLE('',#31085,3.05);
#1105=CIRCLE('',#31087,3.05);
#1106=CIRCLE('',#31089,7.);
#1107=CIRCLE('',#31092,7.);
#1108=CIRCLE('',#31095,7.);
#1109=CIRCLE('',#31098,7.);
#1110=CIRCLE('',#31119,5.5);
#1111=CIRCLE('',#31124,2.55);
#1112=CIRCLE('',#31125,2.05);
#1113=CIRCLE('',#31127,2.5);
#1114=CIRCLE('',#31128,3.5);
#1115=CIRCLE('',#31129,12.5);
#1116=CIRCLE('',#31130,3.5);
#1117=CIRCLE('',#31131,2.5);
#1118=CIRCLE('',#31132,2.5);
#1119=CIRCLE('',#31133,2.5);
#1120=CIRCLE('',#31134,2.5);
#1121=CIRCLE('',#31135,3.5);
#1122=CIRCLE('',#31136,2.5);
#1123=CIRCLE('',#31137,2.5);
#1124=CIRCLE('',#31138,2.50000000000001);
#1125=CIRCLE('',#31139,2.55);
#1126=CIRCLE('',#31140,12.5);
#1127=CIRCLE('',#31141,12.5);
#1128=CIRCLE('',#31142,1.5);
#1129=CIRCLE('',#31143,5.);
#1130=CIRCLE('',#31144,5.);
#1131=CIRCLE('',#31145,4.2379);
#1132=CIRCLE('',#31146,5.625);
#1133=CIRCLE('',#31147,12.5);
#1134=CIRCLE('',#31149,2.05);
#1135=CIRCLE('',#31151,2.05);
#1136=CIRCLE('',#31153,2.05);
#1137=CIRCLE('',#31156,3.);
#1138=CIRCLE('',#31159,3.);
#1139=CIRCLE('',#31162,12.);
#1140=CIRCLE('',#31167,3.);
#1141=CIRCLE('',#31168,2.5);
#1142=CIRCLE('',#31171,3.);
#1143=CIRCLE('',#31172,3.5);
#1144=CIRCLE('',#31175,12.);
#1145=CIRCLE('',#31176,12.5);
#1146=CIRCLE('',#31184,12.5);
#1147=CIRCLE('',#31185,12.);
#1148=CIRCLE('',#31187,3.);
#1149=CIRCLE('',#31188,3.5);
#1150=CIRCLE('',#31189,2.5);
#1151=CIRCLE('',#31190,2.5);
#1152=CIRCLE('',#31191,2.5);
#1153=CIRCLE('',#31192,2.5);
#1154=CIRCLE('',#31193,3.5);
#1155=CIRCLE('',#31194,12.5);
#1156=CIRCLE('',#31195,5.025);
#1157=CIRCLE('',#31196,12.5);
#1158=CIRCLE('',#31198,12.);
#1159=CIRCLE('',#31200,12.);
#1160=CIRCLE('',#31202,12.);
#1161=CIRCLE('',#31204,12.);
#1162=CIRCLE('',#31206,12.);
#1163=CIRCLE('',#31208,3.);
#1164=CIRCLE('',#31211,3.);
#1165=CIRCLE('',#31214,3.);
#1166=CIRCLE('',#31217,3.);
#1167=CIRCLE('',#31220,3.);
#1168=CIRCLE('',#31223,3.);
#1169=CIRCLE('',#31227,3.);
#1170=CIRCLE('',#31228,2.5);
#1171=CIRCLE('',#31231,3.);
#1172=CIRCLE('',#31232,2.5);
#1173=CIRCLE('',#31235,3.);
#1174=CIRCLE('',#31236,2.5);
#1175=CIRCLE('',#31239,3.);
#1176=CIRCLE('',#31240,2.50000000000001);
#1177=CIRCLE('',#31242,3.);
#1178=CIRCLE('',#31245,3.);
#1179=CIRCLE('',#31247,4.5);
#1180=CIRCLE('',#31248,4.5);
#1181=CIRCLE('',#31249,5.);
#1182=CIRCLE('',#31252,3.);
#1183=CIRCLE('',#31255,3.);
#1184=CIRCLE('',#31258,3.);
#1185=CIRCLE('',#31261,3.);
#1186=CIRCLE('',#31264,3.);
#1187=CIRCLE('',#31267,3.);
#1188=CIRCLE('',#31270,3.);
#1189=CIRCLE('',#31295,5.025);
#1190=CIRCLE('',#31299,1.5);
#1191=CIRCLE('',#31302,4.5);
#1192=CIRCLE('',#31305,5.);
#1193=CIRCLE('',#31310,4.2379);
#1194=CIRCLE('',#31313,5.);
#1195=CIRCLE('',#31316,5.);
#1196=CIRCLE('',#31323,4.5);
#1197=CIRCLE('',#31324,5.);
#1198=CIRCLE('',#31326,4.5);
#1199=CIRCLE('',#31328,7.);
#1200=CIRCLE('',#31330,4.5);
#1201=CIRCLE('',#31331,5.);
#1202=CIRCLE('',#31333,4.5);
#1203=CIRCLE('',#31335,7.);
#1204=CIRCLE('',#31337,4.5);
#1205=CIRCLE('',#31338,5.);
#1206=CIRCLE('',#31340,4.5);
#1207=CIRCLE('',#31342,7.);
#1208=CIRCLE('',#31344,4.5);
#1209=CIRCLE('',#31345,5.);
#1210=CIRCLE('',#31347,4.5);
#1211=CIRCLE('',#31349,7.);
#1212=CIRCLE('',#31351,4.5);
#1213=CIRCLE('',#31352,5.);
#1214=CIRCLE('',#31354,4.5);
#1215=CIRCLE('',#31356,7.);
#1216=CIRCLE('',#31358,4.5);
#1217=CIRCLE('',#31359,5.);
#1218=CIRCLE('',#31361,4.5);
#1219=CIRCLE('',#31363,7.);
#1220=CIRCLE('',#31365,4.5);
#1221=CIRCLE('',#31366,5.);
#1222=CIRCLE('',#31368,4.5);
#1223=CIRCLE('',#31370,7.);
#1224=CIRCLE('',#31372,4.5);
#1225=CIRCLE('',#31373,5.);
#1226=CIRCLE('',#31375,4.5);
#1227=CIRCLE('',#31377,7.);
#1228=CIRCLE('',#31379,2.);
#1229=CIRCLE('',#31380,2.5);
#1230=CIRCLE('',#31382,2.);
#1231=CIRCLE('',#31384,4.2379);
#1232=CIRCLE('',#31390,3.5);
#1233=CIRCLE('',#31391,4.);
#1234=CIRCLE('',#31393,3.5);
#1235=CIRCLE('',#31395,6.5);
#1236=CIRCLE('',#31397,3.5);
#1237=CIRCLE('',#31398,3.99999999999999);
#1238=CIRCLE('',#31400,3.5);
#1239=CIRCLE('',#31402,6.5);
#1240=CIRCLE('',#31410,4.5);
#1241=CIRCLE('',#31411,5.);
#1242=CIRCLE('',#31413,4.5);
#1243=CIRCLE('',#31415,7.);
#1244=CIRCLE('',#31417,4.5);
#1245=CIRCLE('',#31418,5.);
#1246=CIRCLE('',#31420,4.5);
#1247=CIRCLE('',#31422,7.);
#1248=CIRCLE('',#31424,5.);
#1249=CIRCLE('',#31426,5.);
#1250=CIRCLE('',#31427,5.);
#1251=CIRCLE('',#31428,5.);
#1252=CIRCLE('',#31429,5.);
#1253=CIRCLE('',#31430,7.55);
#1254=CIRCLE('',#31431,5.);
#1255=CIRCLE('',#31432,4.55);
#1256=CIRCLE('',#31433,4.55);
#1257=CIRCLE('',#31434,4.55);
#1258=CIRCLE('',#31435,4.55);
#1259=CIRCLE('',#31436,4.55);
#1260=CIRCLE('',#31437,4.55);
#1261=CIRCLE('',#31438,3.99999999999999);
#1262=CIRCLE('',#31439,4.55);
#1263=CIRCLE('',#31440,4.55);
#1264=CIRCLE('',#31441,4.55);
#1265=CIRCLE('',#31442,4.55);
#1266=CIRCLE('',#31443,8.);
#1267=CIRCLE('',#31444,8.);
#1268=CIRCLE('',#31445,8.);
#1269=CIRCLE('',#31446,8.);
#1270=CIRCLE('',#31447,4.2379);
#1271=CIRCLE('',#31448,8.);
#1272=CIRCLE('',#31449,8.);
#1273=CIRCLE('',#31450,8.);
#1274=CIRCLE('',#31451,4.55);
#1275=CIRCLE('',#31452,4.55);
#1276=CIRCLE('',#31453,4.55);
#1277=CIRCLE('',#31454,4.55);
#1278=CIRCLE('',#31455,4.);
#1279=CIRCLE('',#31456,4.55);
#1280=CIRCLE('',#31457,4.55);
#1281=CIRCLE('',#31458,4.55);
#1282=CIRCLE('',#31459,4.55);
#1283=CIRCLE('',#31460,4.55);
#1284=CIRCLE('',#31461,4.55);
#1285=CIRCLE('',#31462,5.);
#1286=CIRCLE('',#31463,7.55);
#1287=CIRCLE('',#31464,5.);
#1288=CIRCLE('',#31465,5.);
#1289=CIRCLE('',#31466,5.);
#1290=CIRCLE('',#31475,7.05);
#1291=CIRCLE('',#31477,7.05);
#1292=CIRCLE('',#31479,7.05);
#1293=CIRCLE('',#31481,7.05);
#1294=CIRCLE('',#31488,4.05);
#1295=CIRCLE('',#31490,4.05);
#1296=CIRCLE('',#31492,4.05);
#1297=CIRCLE('',#31494,4.05);
#1298=CIRCLE('',#31496,4.05);
#1299=CIRCLE('',#31498,4.05);
#1300=CIRCLE('',#31500,4.05);
#1301=CIRCLE('',#31502,4.05);
#1302=CIRCLE('',#31504,4.05);
#1303=CIRCLE('',#31506,4.05);
#1304=CIRCLE('',#31508,4.05);
#1305=CIRCLE('',#31510,4.05);
#1306=CIRCLE('',#31512,4.05);
#1307=CIRCLE('',#31514,4.05);
#1308=CIRCLE('',#31516,4.05);
#1309=CIRCLE('',#31518,4.05);
#1310=CIRCLE('',#31520,4.05);
#1311=CIRCLE('',#31522,4.05);
#1312=CIRCLE('',#31524,4.05);
#1313=CIRCLE('',#31526,4.05);
#1314=CIRCLE('',#31528,4.05);
#1315=CIRCLE('',#31530,4.05);
#1316=CIRCLE('',#31532,4.05);
#1317=CIRCLE('',#31534,4.05);
#1318=CIRCLE('',#31538,4.05);
#1319=CIRCLE('',#31540,4.05);
#1320=CIRCLE('',#31542,4.05);
#1321=CIRCLE('',#31544,4.05);
#1322=CIRCLE('',#31546,4.05);
#1323=CIRCLE('',#31548,4.05);
#1324=CIRCLE('',#31550,4.05);
#1325=CIRCLE('',#31552,4.05);
#1326=CIRCLE('',#31554,4.05);
#1327=CIRCLE('',#31556,4.05);
#1328=CIRCLE('',#31558,4.05);
#1329=CIRCLE('',#31560,4.05);
#1330=CIRCLE('',#31562,4.05);
#1331=CIRCLE('',#31564,4.05);
#1332=CIRCLE('',#31566,4.05);
#1333=CIRCLE('',#31568,4.05);
#1334=CIRCLE('',#31570,7.5);
#1335=CIRCLE('',#31572,7.5);
#1336=CIRCLE('',#31574,7.5);
#1337=CIRCLE('',#31576,7.5);
#1338=CIRCLE('',#31578,7.5);
#1339=CIRCLE('',#31580,7.5);
#1340=CIRCLE('',#31582,7.5);
#1341=CIRCLE('',#31584,7.5);
#1342=CIRCLE('',#31586,7.5);
#1343=CIRCLE('',#31588,7.5);
#1344=CIRCLE('',#31590,7.5);
#1345=CIRCLE('',#31592,7.5);
#1346=CIRCLE('',#31594,7.5);
#1347=CIRCLE('',#31596,7.5);
#1348=CIRCLE('',#31600,2.5);
#1349=CIRCLE('',#31601,8.);
#1350=CIRCLE('',#31602,8.);
#1351=CIRCLE('',#31603,8.);
#1352=CIRCLE('',#31604,7.5);
#1353=CIRCLE('',#31605,7.5);
#1354=CIRCLE('',#31606,7.5);
#1355=CIRCLE('',#31607,7.5);
#1356=CIRCLE('',#31608,7.5);
#1357=CIRCLE('',#31609,4.55);
#1358=CIRCLE('',#31610,4.55);
#1359=CIRCLE('',#31611,4.55);
#1360=CIRCLE('',#31612,4.55);
#1361=CIRCLE('',#31613,4.55);
#1362=CIRCLE('',#31614,4.55);
#1363=CIRCLE('',#31615,4.55);
#1364=CIRCLE('',#31616,4.55);
#1365=CIRCLE('',#31617,4.55);
#1366=CIRCLE('',#31618,4.55);
#1367=CIRCLE('',#31619,7.55);
#1368=CIRCLE('',#31620,7.);
#1369=CIRCLE('',#31621,7.);
#1370=CIRCLE('',#31622,7.55);
#1371=CIRCLE('',#31623,4.55);
#1372=CIRCLE('',#31624,4.55);
#1373=CIRCLE('',#31625,4.55);
#1374=CIRCLE('',#31626,4.55);
#1375=CIRCLE('',#31627,4.55);
#1376=CIRCLE('',#31628,4.55);
#1377=CIRCLE('',#31629,4.55);
#1378=CIRCLE('',#31630,4.55);
#1379=CIRCLE('',#31631,4.55);
#1380=CIRCLE('',#31632,4.55);
#1381=CIRCLE('',#31633,7.5);
#1382=CIRCLE('',#31634,7.5);
#1383=CIRCLE('',#31635,7.5);
#1384=CIRCLE('',#31636,7.5);
#1385=CIRCLE('',#31637,7.5);
#1386=CIRCLE('',#31638,8.);
#1387=CIRCLE('',#31639,8.);
#1388=CIRCLE('',#31640,8.);
#1389=CIRCLE('',#31641,8.);
#1390=CIRCLE('',#31651,7.);
#1391=CIRCLE('',#31654,7.);
#1392=CIRCLE('',#31657,7.);
#1393=CIRCLE('',#31660,7.);
#1394=CIRCLE('',#31663,7.);
#1395=CIRCLE('',#31666,7.);
#1396=CIRCLE('',#31669,7.);
#1397=CIRCLE('',#31672,7.);
#1398=CIRCLE('',#31675,7.);
#1399=CIRCLE('',#31678,7.);
#1400=CIRCLE('',#31703,6.5);
#1401=CIRCLE('',#31706,6.5);
#1402=CIRCLE('',#31712,3.75);
#1403=CIRCLE('',#31713,3.25);
#1404=CIRCLE('',#31714,3.75);
#1405=CIRCLE('',#31716,3.75);
#1406=CIRCLE('',#31717,3.25);
#1407=CIRCLE('',#31718,3.75);
#1408=CIRCLE('',#31719,3.75);
#1409=CIRCLE('',#31721,3.25);
#1410=CIRCLE('',#31724,3.25);
#1411=CIRCLE('',#31735,1.7);
#1412=CIRCLE('',#31736,1.7);
#1413=CIRCLE('',#31738,7.05);
#1414=CIRCLE('',#31739,4.5);
#1415=CIRCLE('',#31748,7.05);
#1416=CIRCLE('',#31750,1.5);
#1417=CIRCLE('',#31752,1.7);
#1418=CIRCLE('',#31754,1.7);
#1419=CIRCLE('',#31759,1.5);
#1420=CIRCLE('',#31762,4.5);
#1421=CIRCLE('',#31768,0.4);
#1422=CIRCLE('',#31769,0.4);
#1423=CIRCLE('',#31772,0.4);
#1424=CIRCLE('',#31773,1.6);
#1425=CIRCLE('',#31775,0.4);
#1426=CIRCLE('',#31777,0.4);
#1427=CIRCLE('',#31780,0.4);
#1428=CIRCLE('',#31781,1.6);
#1429=CIRCLE('',#31783,0.4);
#1430=CIRCLE('',#31786,3.933);
#1431=CIRCLE('',#31797,3.22275);
#1432=CIRCLE('',#31808,3.933);
#1433=CIRCLE('',#31809,3.933);
#1434=CIRCLE('',#31811,3.933);
#1435=CIRCLE('',#31812,3.933);
#1436=CIRCLE('',#31813,3.22275);
#1437=CIRCLE('',#31817,8.);
#1438=CIRCLE('',#31820,8.);
#1439=CIRCLE('',#31823,8.);
#1440=CIRCLE('',#31826,8.);
#1441=CIRCLE('',#31829,8.);
#1442=CIRCLE('',#31832,8.);
#1443=CIRCLE('',#31835,8.);
#1444=CIRCLE('',#31838,8.);
#1445=CIRCLE('',#31841,8.);
#1446=CIRCLE('',#31844,8.);
#1447=CIRCLE('',#31847,8.);
#1448=CIRCLE('',#31850,8.);
#1449=CIRCLE('',#31853,8.);
#1450=CIRCLE('',#31856,8.);
#1451=CIRCLE('',#31859,8.);
#1452=CIRCLE('',#31862,8.);
#1453=CIRCLE('',#31865,8.);
#1454=CIRCLE('',#31868,8.);
#1455=CIRCLE('',#31871,8.);
#1456=CIRCLE('',#31874,8.);
#1457=CIRCLE('',#31877,8.);
#1458=CIRCLE('',#31880,8.);
#1459=CIRCLE('',#31883,8.);
#1460=CIRCLE('',#31886,8.);
#1461=CIRCLE('',#31889,8.);
#1462=CIRCLE('',#31892,8.);
#1463=CIRCLE('',#31895,8.);
#1464=CIRCLE('',#31898,8.);
#1465=CIRCLE('',#31901,8.);
#1466=CIRCLE('',#31904,8.);
#1467=CIRCLE('',#31907,8.);
#1468=CIRCLE('',#31910,8.);
#1469=CIRCLE('',#31913,8.);
#1470=CIRCLE('',#31916,8.);
#1471=CIRCLE('',#31919,8.);
#1472=CIRCLE('',#31920,8.);
#1473=CIRCLE('',#31923,8.);
#1474=CIRCLE('',#31924,8.);
#1475=CIRCLE('',#31927,8.);
#1476=CIRCLE('',#31930,8.);
#1477=CIRCLE('',#31933,8.);
#1478=CIRCLE('',#31936,8.);
#1479=CIRCLE('',#31939,8.);
#1480=CIRCLE('',#31942,8.);
#1481=CIRCLE('',#31945,8.);
#1482=CIRCLE('',#31948,8.);
#1483=CIRCLE('',#31951,8.);
#1484=CIRCLE('',#31954,8.);
#1485=CIRCLE('',#31957,8.);
#1486=CIRCLE('',#31960,8.);
#1487=CIRCLE('',#31963,8.);
#1488=CIRCLE('',#31966,8.);
#1489=CIRCLE('',#31969,8.);
#1490=CIRCLE('',#31972,8.);
#1491=CIRCLE('',#31975,8.);
#1492=CIRCLE('',#31978,8.);
#1493=CIRCLE('',#31981,8.);
#1494=CIRCLE('',#31984,8.);
#1495=CIRCLE('',#31987,8.);
#1496=CIRCLE('',#31990,8.);
#1497=CIRCLE('',#31993,8.);
#1498=CIRCLE('',#31996,8.);
#1499=CIRCLE('',#31999,8.);
#1500=CIRCLE('',#32002,8.);
#1501=CIRCLE('',#32005,8.);
#1502=CIRCLE('',#32008,8.);
#1503=CIRCLE('',#32011,8.);
#1504=CIRCLE('',#32014,8.);
#1505=CIRCLE('',#32017,8.);
#1506=CIRCLE('',#32020,8.);
#1507=CIRCLE('',#32023,8.);
#1508=CIRCLE('',#32026,8.);
#1509=CIRCLE('',#32029,8.);
#1510=CIRCLE('',#32032,8.);
#1511=CIRCLE('',#32034,2.48346726553949);
#1512=CIRCLE('',#32043,5.);
#1513=CIRCLE('',#32044,0.4);
#1514=CIRCLE('',#32045,5.4);
#1515=CIRCLE('',#32046,5.);
#1516=CIRCLE('',#32048,5.);
#1517=CIRCLE('',#32050,8.);
#1518=CIRCLE('',#32052,3.2);
#1519=CIRCLE('',#32055,3.933);
#1520=CIRCLE('',#32057,3.25);
#1521=CIRCLE('',#32059,3.25);
#1522=CIRCLE('',#32062,8.);
#1523=CIRCLE('',#32064,7.5);
#1524=CIRCLE('',#32068,5.25);
#1525=CIRCLE('',#32069,5.25);
#1526=CIRCLE('',#32071,15.);
#1527=CIRCLE('',#32073,15.);
#1528=CIRCLE('',#32077,7.9375);
#1529=CIRCLE('',#32080,4.7);
#1530=CIRCLE('',#32082,5.);
#1531=CIRCLE('',#32084,5.);
#1532=CIRCLE('',#32086,4.7);
#1533=CIRCLE('',#32089,0.4);
#1534=CIRCLE('',#32090,0.4);
#1535=CIRCLE('',#32095,4.3);
#1536=CIRCLE('',#32096,4.5);
#1537=CIRCLE('',#32097,4.5);
#1538=CIRCLE('',#32099,4.5);
#1539=CIRCLE('',#32101,2.225);
#1540=CIRCLE('',#32103,2.225);
#1541=CIRCLE('',#32105,4.35);
#1542=CIRCLE('',#32109,1.954);
#1543=CIRCLE('',#32152,1.5555);
#1544=CIRCLE('',#32195,1.954);
#1545=CIRCLE('',#32197,1.954);
#1546=CIRCLE('',#32198,1.954);
#1547=CIRCLE('',#32199,1.5555);
#1548=CIRCLE('',#32202,1.954);
#1549=CIRCLE('',#32203,0.2);
#1550=CIRCLE('',#32204,2.154);
#1551=CIRCLE('',#32205,1.954);
#1552=CIRCLE('',#32208,3.5);
#1553=CIRCLE('',#32211,3.5);
#1554=CIRCLE('',#32214,3.5);
#1555=CIRCLE('',#32217,3.5);
#1556=CIRCLE('',#32220,3.5);
#1557=CIRCLE('',#32223,3.5);
#1558=CIRCLE('',#32226,3.5);
#1559=CIRCLE('',#32229,3.5);
#1560=CIRCLE('',#32232,3.5);
#1561=CIRCLE('',#32235,3.5);
#1562=CIRCLE('',#32238,3.5);
#1563=CIRCLE('',#32241,3.5);
#1564=CIRCLE('',#32244,3.5);
#1565=CIRCLE('',#32247,3.5);
#1566=CIRCLE('',#32250,3.5);
#1567=CIRCLE('',#32253,3.5);
#1568=CIRCLE('',#32256,3.5);
#1569=CIRCLE('',#32259,3.5);
#1570=CIRCLE('',#32262,3.5);
#1571=CIRCLE('',#32265,3.5);
#1572=CIRCLE('',#32268,3.5);
#1573=CIRCLE('',#32271,3.5);
#1574=CIRCLE('',#32274,3.5);
#1575=CIRCLE('',#32277,3.5);
#1576=CIRCLE('',#32280,3.5);
#1577=CIRCLE('',#32283,3.5);
#1578=CIRCLE('',#32286,3.5);
#1579=CIRCLE('',#32289,3.5);
#1580=CIRCLE('',#32292,3.5);
#1581=CIRCLE('',#32295,3.5);
#1582=CIRCLE('',#32298,3.5);
#1583=CIRCLE('',#32301,3.5);
#1584=CIRCLE('',#32304,3.5);
#1585=CIRCLE('',#32307,3.5);
#1586=CIRCLE('',#32310,3.5);
#1587=CIRCLE('',#32313,3.5);
#1588=CIRCLE('',#32314,3.5);
#1589=CIRCLE('',#32317,3.5);
#1590=CIRCLE('',#32318,3.5);
#1591=CIRCLE('',#32321,3.5);
#1592=CIRCLE('',#32324,3.5);
#1593=CIRCLE('',#32327,3.5);
#1594=CIRCLE('',#32330,3.5);
#1595=CIRCLE('',#32333,3.5);
#1596=CIRCLE('',#32336,3.5);
#1597=CIRCLE('',#32339,3.5);
#1598=CIRCLE('',#32342,3.5);
#1599=CIRCLE('',#32345,3.5);
#1600=CIRCLE('',#32348,3.5);
#1601=CIRCLE('',#32351,3.5);
#1602=CIRCLE('',#32354,3.5);
#1603=CIRCLE('',#32357,3.5);
#1604=CIRCLE('',#32360,3.5);
#1605=CIRCLE('',#32363,3.5);
#1606=CIRCLE('',#32366,3.5);
#1607=CIRCLE('',#32369,3.5);
#1608=CIRCLE('',#32372,3.5);
#1609=CIRCLE('',#32375,3.5);
#1610=CIRCLE('',#32378,3.5);
#1611=CIRCLE('',#32381,3.5);
#1612=CIRCLE('',#32384,3.5);
#1613=CIRCLE('',#32387,3.5);
#1614=CIRCLE('',#32390,3.5);
#1615=CIRCLE('',#32393,3.5);
#1616=CIRCLE('',#32396,3.5);
#1617=CIRCLE('',#32399,3.5);
#1618=CIRCLE('',#32402,3.5);
#1619=CIRCLE('',#32405,3.5);
#1620=CIRCLE('',#32408,3.5);
#1621=CIRCLE('',#32411,3.5);
#1622=CIRCLE('',#32414,3.5);
#1623=CIRCLE('',#32417,3.5);
#1624=CIRCLE('',#32420,3.5);
#1625=CIRCLE('',#32423,3.5);
#1626=CIRCLE('',#32426,3.5);
#1627=CIRCLE('',#32428,1.483539833954);
#1628=CIRCLE('',#32437,1.6);
#1629=CIRCLE('',#32440,3.5);
#1630=CIRCLE('',#32442,3.1);
#1631=CIRCLE('',#32446,1.2);
#1632=CIRCLE('',#32448,1.5);
#1633=CIRCLE('',#32450,1.5);
#1634=CIRCLE('',#32452,1.2);
#1635=CIRCLE('',#32456,1.4635);
#1636=CIRCLE('',#32526,1.17775);
#1637=CIRCLE('',#32596,1.4635);
#1638=CIRCLE('',#32597,1.4635);
#1639=CIRCLE('',#32599,1.4635);
#1640=CIRCLE('',#32600,1.4635);
#1641=CIRCLE('',#32601,1.17775);
#1642=CIRCLE('',#32604,0.2);
#1643=CIRCLE('',#32605,1.6635);
#1644=CIRCLE('',#32606,1.4635);
#1645=CIRCLE('',#32609,2.75);
#1646=CIRCLE('',#32612,2.75);
#1647=CIRCLE('',#32615,2.75);
#1648=CIRCLE('',#32618,2.75);
#1649=CIRCLE('',#32621,2.75);
#1650=CIRCLE('',#32624,2.75);
#1651=CIRCLE('',#32627,2.75);
#1652=CIRCLE('',#32630,2.75);
#1653=CIRCLE('',#32633,2.75);
#1654=CIRCLE('',#32636,2.75);
#1655=CIRCLE('',#32639,2.75);
#1656=CIRCLE('',#32642,2.75);
#1657=CIRCLE('',#32645,2.75);
#1658=CIRCLE('',#32648,2.75);
#1659=CIRCLE('',#32651,2.75);
#1660=CIRCLE('',#32654,2.75);
#1661=CIRCLE('',#32657,2.75);
#1662=CIRCLE('',#32660,2.75);
#1663=CIRCLE('',#32663,2.75);
#1664=CIRCLE('',#32666,2.75);
#1665=CIRCLE('',#32669,2.75);
#1666=CIRCLE('',#32672,2.75);
#1667=CIRCLE('',#32675,2.75);
#1668=CIRCLE('',#32678,2.75);
#1669=CIRCLE('',#32681,2.75);
#1670=CIRCLE('',#32684,2.75);
#1671=CIRCLE('',#32687,2.75);
#1672=CIRCLE('',#32690,2.75);
#1673=CIRCLE('',#32693,2.75);
#1674=CIRCLE('',#32696,2.75);
#1675=CIRCLE('',#32699,2.75);
#1676=CIRCLE('',#32702,2.75);
#1677=CIRCLE('',#32705,2.75);
#1678=CIRCLE('',#32708,2.75);
#1679=CIRCLE('',#32711,2.75);
#1680=CIRCLE('',#32714,2.75);
#1681=CIRCLE('',#32715,2.75);
#1682=CIRCLE('',#32718,2.75);
#1683=CIRCLE('',#32719,2.75);
#1684=CIRCLE('',#32722,2.75);
#1685=CIRCLE('',#32725,2.75);
#1686=CIRCLE('',#32728,2.75);
#1687=CIRCLE('',#32731,2.75);
#1688=CIRCLE('',#32734,2.75);
#1689=CIRCLE('',#32737,2.75);
#1690=CIRCLE('',#32740,2.75);
#1691=CIRCLE('',#32743,2.75);
#1692=CIRCLE('',#32746,2.75);
#1693=CIRCLE('',#32749,2.75);
#1694=CIRCLE('',#32752,2.75);
#1695=CIRCLE('',#32755,2.75);
#1696=CIRCLE('',#32758,2.75);
#1697=CIRCLE('',#32761,2.75);
#1698=CIRCLE('',#32764,2.75);
#1699=CIRCLE('',#32767,2.75);
#1700=CIRCLE('',#32770,2.75);
#1701=CIRCLE('',#32773,2.75);
#1702=CIRCLE('',#32776,2.75);
#1703=CIRCLE('',#32779,2.75);
#1704=CIRCLE('',#32782,2.75);
#1705=CIRCLE('',#32785,2.75);
#1706=CIRCLE('',#32788,2.75);
#1707=CIRCLE('',#32791,2.75);
#1708=CIRCLE('',#32794,2.75);
#1709=CIRCLE('',#32797,2.75);
#1710=CIRCLE('',#32800,2.75);
#1711=CIRCLE('',#32803,2.75);
#1712=CIRCLE('',#32806,2.75);
#1713=CIRCLE('',#32809,2.75);
#1714=CIRCLE('',#32812,2.75);
#1715=CIRCLE('',#32815,2.75);
#1716=CIRCLE('',#32818,2.75);
#1717=CIRCLE('',#32821,2.75);
#1718=CIRCLE('',#32824,2.75);
#1719=CIRCLE('',#32827,2.75);
#1720=CIRCLE('',#32829,1.23357587978679);
#1721=CIRCLE('',#32838,1.1);
#1722=CIRCLE('',#32841,2.75);
#1723=CIRCLE('',#32843,2.45);
#1724=CIRCLE('',#32850,12.);
#1725=CIRCLE('',#32851,12.);
#1726=CIRCLE('',#32853,11.5);
#1727=CIRCLE('',#32857,12.);
#1728=CIRCLE('',#32858,11.5);
#1729=CIRCLE('',#32865,12.);
#1730=CIRCLE('',#32866,12.);
#1731=CIRCLE('',#32868,11.5);
#1732=CIRCLE('',#32873,11.5);
#1733=CIRCLE('',#32877,12.);
#1734=CIRCLE('',#32878,12.);
#1735=CIRCLE('',#32880,11.5);
#1736=CIRCLE('',#32889,11.5);
#1737=CIRCLE('',#32893,11.5);
#1738=CIRCLE('',#32896,11.5);
#1739=CIRCLE('',#32897,7.05);
#1740=CIRCLE('',#32901,12.);
#1741=CIRCLE('',#32905,7.05);
#1742=CIRCLE('',#32909,6.933);
#1743=CIRCLE('',#32926,6.21925);
#1744=CIRCLE('',#32928,6.21925);
#1745=CIRCLE('',#32944,5.55);
#1746=CIRCLE('',#32945,5.05);
#1747=CIRCLE('',#32946,5.05);
#1748=CIRCLE('',#32948,5.05);
#1749=CIRCLE('',#32949,5.05);
#1750=CIRCLE('',#32951,6.3);
#1751=CIRCLE('',#32953,5.55);
#1752=CIRCLE('',#32955,7.6);
#1753=CIRCLE('',#32957,1.55);
#1754=CIRCLE('',#32958,1.55);
#1755=CIRCLE('',#32960,12.);
#1756=CIRCLE('',#32961,12.);
#1757=CIRCLE('',#32963,6.933);
#1758=CIRCLE('',#32964,6.933);
#1759=CIRCLE('',#32965,6.21925);
#1760=CIRCLE('',#32971,6.933);
#1761=CIRCLE('',#32973,11.5);
#1762=CIRCLE('',#32976,11.5);
#1763=CIRCLE('',#32978,8.);
#1764=CIRCLE('',#32980,8.);
#1765=CIRCLE('',#32984,4.954);
#1766=CIRCLE('',#33060,4.52375);
#1767=CIRCLE('',#33136,4.954);
#1768=CIRCLE('',#33137,4.954);
#1769=CIRCLE('',#33139,4.954);
#1770=CIRCLE('',#33140,4.954);
#1771=CIRCLE('',#33141,4.52375);
#1772=CIRCLE('',#33144,2.5);
#1773=CIRCLE('',#33145,2.5);
#1774=CIRCLE('',#33148,4.954);
#1775=CIRCLE('',#33150,4.5);
#1776=CIRCLE('',#33153,3.00000000000001);
#1777=CIRCLE('',#33156,5.55);
#1778=CIRCLE('',#33157,5.05);
#1779=CIRCLE('',#33158,5.05);
#1780=CIRCLE('',#33160,5.05);
#1781=CIRCLE('',#33162,7.6);
#1782=CIRCLE('',#33165,1.5);
#1783=CIRCLE('',#33166,1.5);
#1784=CIRCLE('',#33169,9.5);
#1785=CIRCLE('',#33170,8.7);
#1786=CIRCLE('',#33172,9.5);
#1787=CIRCLE('',#33173,9.5);
#1788=CIRCLE('',#33174,9.5);
#1789=CIRCLE('',#33175,9.5);
#1790=CIRCLE('',#33176,9.5);
#1791=CIRCLE('',#33177,9.5);
#1792=CIRCLE('',#33178,9.5);
#1793=CIRCLE('',#33179,9.5);
#1794=CIRCLE('',#33180,9.5);
#1795=CIRCLE('',#33181,9.5);
#1796=CIRCLE('',#33182,9.5);
#1797=CIRCLE('',#33183,9.5);
#1798=CIRCLE('',#33184,9.5);
#1799=CIRCLE('',#33185,9.5);
#1800=CIRCLE('',#33186,9.5);
#1801=CIRCLE('',#33187,9.5);
#1802=CIRCLE('',#33188,9.5);
#1803=CIRCLE('',#33189,9.5);
#1804=CIRCLE('',#33190,9.5);
#1805=CIRCLE('',#33191,9.5);
#1806=CIRCLE('',#33192,9.5);
#1807=CIRCLE('',#33193,9.5);
#1808=CIRCLE('',#33194,9.5);
#1809=CIRCLE('',#33195,9.5);
#1810=CIRCLE('',#33196,9.5);
#1811=CIRCLE('',#33197,9.5);
#1812=CIRCLE('',#33198,9.5);
#1813=CIRCLE('',#33199,9.5);
#1814=CIRCLE('',#33200,9.5);
#1815=CIRCLE('',#33201,9.5);
#1816=CIRCLE('',#33202,9.5);
#1817=CIRCLE('',#33205,1.5);
#1818=CIRCLE('',#33206,1.5);
#1819=CIRCLE('',#33209,8.7);
#1820=CIRCLE('',#33212,1.5);
#1821=CIRCLE('',#33213,1.5);
#1822=CIRCLE('',#33216,8.7);
#1823=CIRCLE('',#33219,1.5);
#1824=CIRCLE('',#33220,1.5);
#1825=CIRCLE('',#33223,8.7);
#1826=CIRCLE('',#33226,1.5);
#1827=CIRCLE('',#33227,1.5);
#1828=CIRCLE('',#33230,8.7);
#1829=CIRCLE('',#33233,1.5);
#1830=CIRCLE('',#33234,1.5);
#1831=CIRCLE('',#33237,8.7);
#1832=CIRCLE('',#33240,1.5);
#1833=CIRCLE('',#33241,1.5);
#1834=CIRCLE('',#33244,8.7);
#1835=CIRCLE('',#33247,1.5);
#1836=CIRCLE('',#33248,1.5);
#1837=CIRCLE('',#33251,8.7);
#1838=CIRCLE('',#33254,1.5);
#1839=CIRCLE('',#33255,1.5);
#1840=CIRCLE('',#33258,8.7);
#1841=CIRCLE('',#33261,1.5);
#1842=CIRCLE('',#33262,1.5);
#1843=CIRCLE('',#33265,8.7);
#1844=CIRCLE('',#33268,1.5);
#1845=CIRCLE('',#33269,1.5);
#1846=CIRCLE('',#33272,8.7);
#1847=CIRCLE('',#33275,1.5);
#1848=CIRCLE('',#33276,1.5);
#1849=CIRCLE('',#33279,8.7);
#1850=CIRCLE('',#33282,1.5);
#1851=CIRCLE('',#33283,1.5);
#1852=CIRCLE('',#33286,8.7);
#1853=CIRCLE('',#33289,1.5);
#1854=CIRCLE('',#33290,1.5);
#1855=CIRCLE('',#33293,8.7);
#1856=CIRCLE('',#33296,1.5);
#1857=CIRCLE('',#33297,1.5);
#1858=CIRCLE('',#33309,8.7);
#1859=CIRCLE('',#33331,8.);
#1860=CIRCLE('',#33333,8.);
#1861=CIRCLE('',#33335,9.);
#1862=CIRCLE('',#33340,1.4635);
#1863=CIRCLE('',#33348,1.17775);
#1864=CIRCLE('',#33355,1.4635);
#1865=CIRCLE('',#33356,1.4635);
#1866=CIRCLE('',#33358,1.4635);
#1867=CIRCLE('',#33359,1.4635);
#1868=CIRCLE('',#33360,1.17775);
#1869=CIRCLE('',#33370,1.05);
#1870=CIRCLE('',#33373,1.4635);
#1871=CIRCLE('',#33375,1.2);
#1872=CONICAL_SURFACE('',#30902,1.8,0.785398163397448);
#1873=CONICAL_SURFACE('',#30909,1.8,0.785398163397448);
#1874=CONICAL_SURFACE('',#30913,4.75,0.785398163397448);
#1875=CONICAL_SURFACE('',#30920,4.75,0.785398163397446);
#1876=CONICAL_SURFACE('',#30927,4.75,0.785398163397446);
#1877=CONICAL_SURFACE('',#30934,4.75,0.785398163397448);
#1878=CONICAL_SURFACE('',#31036,4.25,0.785398163397448);
#1879=CONICAL_SURFACE('',#31040,3.25,0.785398163397448);
#1880=CONICAL_SURFACE('',#31044,3.25,0.785398163397448);
#1881=CONICAL_SURFACE('',#31048,3.25,0.785398163397448);
#1882=CONICAL_SURFACE('',#31052,3.25,0.785398163397437);
#1883=CONICAL_SURFACE('',#31056,3.25,0.785398163397448);
#1884=CONICAL_SURFACE('',#31060,3.25,0.785398163397437);
#1885=CONICAL_SURFACE('',#31064,3.25,0.785398163397448);
#1886=CONICAL_SURFACE('',#31068,3.25,0.785398163397448);
#1887=CONICAL_SURFACE('',#31072,3.25,0.785398163397437);
#1888=CONICAL_SURFACE('',#31076,3.25,0.785398163397448);
#1889=CONICAL_SURFACE('',#31080,3.25,0.785398163397437);
#1890=CONICAL_SURFACE('',#31084,3.25,0.785398163397448);
#1891=CONICAL_SURFACE('',#31088,7.2,0.785398163397448);
#1892=CONICAL_SURFACE('',#31091,7.2,0.785398163397448);
#1893=CONICAL_SURFACE('',#31094,7.2,0.785398163397448);
#1894=CONICAL_SURFACE('',#31097,7.2,0.785398163397448);
#1895=CONICAL_SURFACE('',#31100,4.7,0.785398163397448);
#1896=CONICAL_SURFACE('',#31101,4.7,0.785398163397448);
#1897=CONICAL_SURFACE('',#31102,4.7,0.785398163397448);
#1898=CONICAL_SURFACE('',#31103,4.7,0.785398163397448);
#1899=CONICAL_SURFACE('',#31123,2.3,0.785398163397448);
#1900=CONICAL_SURFACE('',#31150,2.3,0.785398163397451);
#1901=CONICAL_SURFACE('',#31155,2.75,0.785398163397449);
#1902=CONICAL_SURFACE('',#31158,3.25,0.785398163397449);
#1903=CONICAL_SURFACE('',#31161,12.25,0.785398163397448);
#1904=CONICAL_SURFACE('',#31166,2.75,0.785398163397449);
#1905=CONICAL_SURFACE('',#31170,3.25,0.785398163397449);
#1906=CONICAL_SURFACE('',#31174,12.25,0.785398163397455);
#1907=CONICAL_SURFACE('',#31183,12.25,0.785398163397451);
#1908=CONICAL_SURFACE('',#31199,12.25,0.785398163397448);
#1909=CONICAL_SURFACE('',#31203,12.25,0.785398163397448);
#1910=CONICAL_SURFACE('',#31207,3.25,0.785398163397448);
#1911=CONICAL_SURFACE('',#31210,2.75,0.785398163397449);
#1912=CONICAL_SURFACE('',#31213,2.75,0.785398163397449);
#1913=CONICAL_SURFACE('',#31216,2.75,0.785398163397449);
#1914=CONICAL_SURFACE('',#31219,2.75,0.785398163397449);
#1915=CONICAL_SURFACE('',#31222,3.25,0.785398163397448);
#1916=CONICAL_SURFACE('',#31226,2.75,0.785398163397448);
#1917=CONICAL_SURFACE('',#31230,2.75,0.785398163397447);
#1918=CONICAL_SURFACE('',#31234,2.75,0.785398163397447);
#1919=CONICAL_SURFACE('',#31238,2.75,0.785398163397443);
#1920=CONICAL_SURFACE('',#31251,3.25,0.785398163397448);
#1921=CONICAL_SURFACE('',#31254,2.75,0.785398163397449);
#1922=CONICAL_SURFACE('',#31257,2.75,0.785398163397449);
#1923=CONICAL_SURFACE('',#31260,2.75,0.785398163397449);
#1924=CONICAL_SURFACE('',#31263,2.75,0.785398163397449);
#1925=CONICAL_SURFACE('',#31266,3.25,0.785398163397448);
#1926=CONICAL_SURFACE('',#31269,2.75,0.785398163397449);
#1927=CONICAL_SURFACE('',#31272,2.75,0.785398163397449);
#1928=CONICAL_SURFACE('',#31274,2.75,0.785398163397443);
#1929=CONICAL_SURFACE('',#31291,12.25,0.785398163397448);
#1930=CONICAL_SURFACE('',#31292,12.25,0.785398163397448);
#1931=CONICAL_SURFACE('',#31293,12.25,0.785398163397451);
#1932=CONICAL_SURFACE('',#31294,5.325,0.785398163397447);
#1933=CONICAL_SURFACE('',#31322,4.75,0.785398163397448);
#1934=CONICAL_SURFACE('',#31329,4.75,0.785398163397448);
#1935=CONICAL_SURFACE('',#31336,4.75,0.785398163397451);
#1936=CONICAL_SURFACE('',#31343,4.75,0.785398163397451);
#1937=CONICAL_SURFACE('',#31350,4.75,0.785398163397451);
#1938=CONICAL_SURFACE('',#31357,4.75,0.785398163397448);
#1939=CONICAL_SURFACE('',#31364,4.75,0.785398163397448);
#1940=CONICAL_SURFACE('',#31371,4.75,0.785398163397448);
#1941=CONICAL_SURFACE('',#31378,2.25,0.785398163397448);
#1942=CONICAL_SURFACE('',#31389,3.75,0.785398163397451);
#1943=CONICAL_SURFACE('',#31396,3.75,0.785398163397448);
#1944=CONICAL_SURFACE('',#31409,4.75,0.785398163397448);
#1945=CONICAL_SURFACE('',#31416,4.75,0.785398163397448);
#1946=CONICAL_SURFACE('',#31423,4.75,0.785398163397448);
#1947=CONICAL_SURFACE('',#31467,4.75,0.785398163397448);
#1948=CONICAL_SURFACE('',#31468,4.75,0.785398163397451);
#1949=CONICAL_SURFACE('',#31469,4.75,0.785398163397451);
#1950=CONICAL_SURFACE('',#31470,4.75,0.785398163397451);
#1951=CONICAL_SURFACE('',#31471,4.75,0.785398163397448);
#1952=CONICAL_SURFACE('',#31472,4.75,0.785398163397448);
#1953=CONICAL_SURFACE('',#31473,4.75,0.785398163397448);
#1954=CONICAL_SURFACE('',#31474,7.3,0.785398163397448);
#1955=CONICAL_SURFACE('',#31478,7.3,0.785398163397448);
#1956=CONICAL_SURFACE('',#31482,4.75,0.785398163397448);
#1957=CONICAL_SURFACE('',#31483,4.75,0.785398163397448);
#1958=CONICAL_SURFACE('',#31487,4.3,0.785398163397448);
#1959=CONICAL_SURFACE('',#31491,4.3,0.785398163397448);
#1960=CONICAL_SURFACE('',#31495,4.3,0.785398163397448);
#1961=CONICAL_SURFACE('',#31499,4.3,0.785398163397448);
#1962=CONICAL_SURFACE('',#31503,4.3,0.785398163397451);
#1963=CONICAL_SURFACE('',#31507,4.3,0.785398163397451);
#1964=CONICAL_SURFACE('',#31511,4.3,0.78539816339745);
#1965=CONICAL_SURFACE('',#31515,4.3,0.78539816339745);
#1966=CONICAL_SURFACE('',#31519,4.3,0.785398163397448);
#1967=CONICAL_SURFACE('',#31523,4.3,0.785398163397448);
#1968=CONICAL_SURFACE('',#31527,4.3,0.785398163397448);
#1969=CONICAL_SURFACE('',#31531,4.3,0.785398163397448);
#1970=CONICAL_SURFACE('',#31535,3.75,0.785398163397448);
#1971=CONICAL_SURFACE('',#31536,3.75,0.785398163397451);
#1972=CONICAL_SURFACE('',#31537,4.3,0.785398163397451);
#1973=CONICAL_SURFACE('',#31541,4.3,0.78539816339745);
#1974=CONICAL_SURFACE('',#31545,4.3,0.785398163397448);
#1975=CONICAL_SURFACE('',#31549,4.3,0.78539816339745);
#1976=CONICAL_SURFACE('',#31553,4.3,0.785398163397448);
#1977=CONICAL_SURFACE('',#31557,4.3,0.785398163397448);
#1978=CONICAL_SURFACE('',#31561,4.3,0.785398163397448);
#1979=CONICAL_SURFACE('',#31565,4.3,0.785398163397448);
#1980=CONICAL_SURFACE('',#31569,7.75,0.785398163397448);
#1981=CONICAL_SURFACE('',#31573,7.75,0.785398163397448);
#1982=CONICAL_SURFACE('',#31577,7.75,0.785398163397451);
#1983=CONICAL_SURFACE('',#31581,7.75,0.785398163397448);
#1984=CONICAL_SURFACE('',#31585,7.75,0.785398163397451);
#1985=CONICAL_SURFACE('',#31589,7.75,0.785398163397451);
#1986=CONICAL_SURFACE('',#31593,7.75,0.785398163397448);
#1987=CONICAL_SURFACE('',#31642,2.25,0.785398163397448);
#1988=CONICAL_SURFACE('',#31643,7.75,0.785398163397448);
#1989=CONICAL_SURFACE('',#31644,7.75,0.785398163397451);
#1990=CONICAL_SURFACE('',#31645,7.75,0.785398163397451);
#1991=CONICAL_SURFACE('',#31646,7.75,0.785398163397448);
#1992=CONICAL_SURFACE('',#31647,7.75,0.785398163397451);
#1993=CONICAL_SURFACE('',#31648,7.75,0.785398163397448);
#1994=CONICAL_SURFACE('',#31649,7.75,0.785398163397448);
#1995=CONICAL_SURFACE('',#31650,7.25,0.785398163397448);
#1996=CONICAL_SURFACE('',#31653,7.25,0.785398163397448);
#1997=CONICAL_SURFACE('',#31656,7.25,0.785398163397448);
#1998=CONICAL_SURFACE('',#31659,7.25,0.785398163397448);
#1999=CONICAL_SURFACE('',#31662,7.25,0.785398163397451);
#2000=CONICAL_SURFACE('',#31665,7.25,0.785398163397451);
#2001=CONICAL_SURFACE('',#31668,7.25,0.785398163397451);
#2002=CONICAL_SURFACE('',#31671,7.25,0.785398163397448);
#2003=CONICAL_SURFACE('',#31674,7.25,0.785398163397448);
#2004=CONICAL_SURFACE('',#31677,7.25,0.785398163397448);
#2005=CONICAL_SURFACE('',#31680,4.3,0.785398163397448);
#2006=CONICAL_SURFACE('',#31681,4.3,0.785398163397448);
#2007=CONICAL_SURFACE('',#31682,4.3,0.785398163397448);
#2008=CONICAL_SURFACE('',#31683,4.3,0.785398163397448);
#2009=CONICAL_SURFACE('',#31684,4.3,0.78539816339745);
#2010=CONICAL_SURFACE('',#31685,4.3,0.785398163397448);
#2011=CONICAL_SURFACE('',#31686,4.3,0.78539816339745);
#2012=CONICAL_SURFACE('',#31687,4.3,0.785398163397451);
#2013=CONICAL_SURFACE('',#31688,4.3,0.785398163397448);
#2014=CONICAL_SURFACE('',#31689,4.3,0.785398163397448);
#2015=CONICAL_SURFACE('',#31690,4.3,0.785398163397448);
#2016=CONICAL_SURFACE('',#31691,4.3,0.785398163397448);
#2017=CONICAL_SURFACE('',#31692,4.3,0.785398163397451);
#2018=CONICAL_SURFACE('',#31693,4.3,0.785398163397451);
#2019=CONICAL_SURFACE('',#31694,4.3,0.78539816339745);
#2020=CONICAL_SURFACE('',#31695,4.3,0.78539816339745);
#2021=CONICAL_SURFACE('',#31696,4.3,0.785398163397448);
#2022=CONICAL_SURFACE('',#31697,4.3,0.785398163397448);
#2023=CONICAL_SURFACE('',#31698,4.3,0.785398163397448);
#2024=CONICAL_SURFACE('',#31699,4.3,0.785398163397448);
#2025=CONICAL_SURFACE('',#31700,7.3,0.785398163397448);
#2026=CONICAL_SURFACE('',#31701,7.3,0.785398163397448);
#2027=CONICAL_SURFACE('',#31702,6.75,0.785398163397448);
#2028=CONICAL_SURFACE('',#31705,6.75,0.785398163397451);
#2029=CONICAL_SURFACE('',#31711,3.5,0.785398163397442);
#2030=CONICAL_SURFACE('',#31715,3.5,0.785398163397442);
#2031=CONICAL_SURFACE('',#32033,1.25,1.02681050468488);
#2032=CONICAL_SURFACE('',#32053,3.6,0.785398163397448);
#2033=CONICAL_SURFACE('',#32056,3.625,0.982793723247331);
#2034=CONICAL_SURFACE('',#32063,7.75,0.78539816339745);
#2035=CONICAL_SURFACE('',#32081,4.85,0.785398163397448);
#2036=CONICAL_SURFACE('',#32085,4.85,0.785398163397448);
#2037=CONICAL_SURFACE('',#32094,4.4,0.785398163397449);
#2038=CONICAL_SURFACE('',#32106,4.425,0.785398163397451);
#2039=CONICAL_SURFACE('',#32427,0.75,1.02486043295185);
#2040=CONICAL_SURFACE('',#32438,1.8,0.785398163397448);
#2041=CONICAL_SURFACE('',#32441,3.3,0.785398163397448);
#2042=CONICAL_SURFACE('',#32447,1.35,0.785398163397448);
#2043=CONICAL_SURFACE('',#32451,1.35,0.785398163397448);
#2044=CONICAL_SURFACE('',#32828,0.625,1.02388712580674);
#2045=CONICAL_SURFACE('',#32839,1.3,0.785398163397448);
#2046=CONICAL_SURFACE('',#32842,2.6,0.785398163397449);
#2047=CONICAL_SURFACE('',#32852,11.75,0.78539816339745);
#2048=CONICAL_SURFACE('',#32856,11.75,0.78539816339745);
#2049=CONICAL_SURFACE('',#32867,11.75,0.785398163397449);
#2050=CONICAL_SURFACE('',#32872,11.75,0.78539816339745);
#2051=CONICAL_SURFACE('',#32879,11.75,0.785398163397449);
#2052=CONICAL_SURFACE('',#32888,11.75,0.785398163397449);
#2053=CONICAL_SURFACE('',#32892,11.75,0.78539816339745);
#2054=CONICAL_SURFACE('',#32902,11.75,0.785398163397449);
#2055=CONICAL_SURFACE('',#32943,5.3,0.785398163397448);
#2056=CONICAL_SURFACE('',#32952,5.3,0.785398163397448);
#2057=CONICAL_SURFACE('',#32969,6.65,0.785398163397447);
#2058=CONICAL_SURFACE('',#32974,11.75,0.785398163397448);
#2059=CONICAL_SURFACE('',#32975,11.75,0.785398163397448);
#2060=CONICAL_SURFACE('',#32981,7.8,0.785398163397451);
#2061=CONICAL_SURFACE('',#33146,3.75,1.19028994968253);
#2062=CONICAL_SURFACE('',#33149,4.75,0.78539816339745);
#2063=CONICAL_SURFACE('',#33155,5.3,0.785398163397451);
#2064=CONICAL_SURFACE('',#33168,9.1,0.785398163397454);
#2065=CONICAL_SURFACE('',#33208,9.1,0.785398163397454);
#2066=CONICAL_SURFACE('',#33215,9.1,0.785398163397454);
#2067=CONICAL_SURFACE('',#33222,9.1,0.785398163397454);
#2068=CONICAL_SURFACE('',#33229,9.1,0.785398163397454);
#2069=CONICAL_SURFACE('',#33236,9.1,0.785398163397454);
#2070=CONICAL_SURFACE('',#33243,9.1,0.785398163397454);
#2071=CONICAL_SURFACE('',#33250,9.1,0.785398163397454);
#2072=CONICAL_SURFACE('',#33257,9.1,0.785398163397454);
#2073=CONICAL_SURFACE('',#33264,9.1,0.785398163397454);
#2074=CONICAL_SURFACE('',#33271,9.1,0.785398163397454);
#2075=CONICAL_SURFACE('',#33278,9.1,0.785398163397454);
#2076=CONICAL_SURFACE('',#33285,9.1,0.785398163397454);
#2077=CONICAL_SURFACE('',#33292,9.1,0.785398163397454);
#2078=CONICAL_SURFACE('',#33329,9.1,0.785398163397454);
#2079=CONICAL_SURFACE('',#33330,7.8,0.785398163397454);
#2080=CONICAL_SURFACE('',#33336,9.25,0.785398163397445);
#2081=CONICAL_SURFACE('',#33371,1.275,0.785398163397448);
#2082=CONICAL_SURFACE('',#33374,1.35,0.785398163397448);
#2083=B_SPLINE_CURVE_WITH_KNOTS('',2,(#40862,#40863,#40864),
 .UNSPECIFIED.,.F.,.F.,(3,3),(0.,1.),.UNSPECIFIED.);
#2084=B_SPLINE_CURVE_WITH_KNOTS('',2,(#40866,#40867,#40868),
 .UNSPECIFIED.,.F.,.F.,(3,3),(0.,1.),.UNSPECIFIED.);
#2085=B_SPLINE_CURVE_WITH_KNOTS('',2,(#40870,#40871,#40872),
 .UNSPECIFIED.,.F.,.F.,(3,3),(0.,1.),.UNSPECIFIED.);
#2086=B_SPLINE_CURVE_WITH_KNOTS('',2,(#40874,#40875,#40876),
 .UNSPECIFIED.,.F.,.F.,(3,3),(0.,1.),.UNSPECIFIED.);
#2087=B_SPLINE_CURVE_WITH_KNOTS('',2,(#40878,#40879,#40880),
 .UNSPECIFIED.,.F.,.F.,(3,3),(0.,1.),.UNSPECIFIED.);
#2088=B_SPLINE_CURVE_WITH_KNOTS('',2,(#40882,#40883,#40884),
 .UNSPECIFIED.,.F.,.F.,(3,3),(0.,1.),.UNSPECIFIED.);
#2089=B_SPLINE_CURVE_WITH_KNOTS('',2,(#40886,#40887,#40888),
 .UNSPECIFIED.,.F.,.F.,(3,3),(0.,1.),.UNSPECIFIED.);
#2090=B_SPLINE_CURVE_WITH_KNOTS('',2,(#40896,#40897,#40898),
 .UNSPECIFIED.,.F.,.F.,(3,3),(0.,1.),.UNSPECIFIED.);
#2091=B_SPLINE_CURVE_WITH_KNOTS('',2,(#40900,#40901,#40902),
 .UNSPECIFIED.,.F.,.F.,(3,3),(0.,1.),.UNSPECIFIED.);
#2092=B_SPLINE_CURVE_WITH_KNOTS('',2,(#40904,#40905,#40906),
 .UNSPECIFIED.,.F.,.F.,(3,3),(0.,1.),.UNSPECIFIED.);
#2093=B_SPLINE_CURVE_WITH_KNOTS('',2,(#40907,#40908,#40909),
 .UNSPECIFIED.,.F.,.F.,(3,3),(0.,1.),.UNSPECIFIED.);
#2094=B_SPLINE_CURVE_WITH_KNOTS('',2,(#40936,#40937,#40938),
 .UNSPECIFIED.,.F.,.F.,(3,3),(0.,1.),.UNSPECIFIED.);
#2095=B_SPLINE_CURVE_WITH_KNOTS('',2,(#40940,#40941,#40942),
 .UNSPECIFIED.,.F.,.F.,(3,3),(0.,1.),.UNSPECIFIED.);
#2096=B_SPLINE_CURVE_WITH_KNOTS('',2,(#40952,#40953,#40954),
 .UNSPECIFIED.,.F.,.F.,(3,3),(0.,1.),.UNSPECIFIED.);
#2097=B_SPLINE_CURVE_WITH_KNOTS('',2,(#40956,#40957,#40958),
 .UNSPECIFIED.,.F.,.F.,(3,3),(0.,1.),.UNSPECIFIED.);
#2098=B_SPLINE_CURVE_WITH_KNOTS('',2,(#40960,#40961,#40962),
 .UNSPECIFIED.,.F.,.F.,(3,3),(0.,1.),.UNSPECIFIED.);
#2099=B_SPLINE_CURVE_WITH_KNOTS('',2,(#40965,#40966,#40967),
 .UNSPECIFIED.,.F.,.F.,(3,3),(0.,1.),.UNSPECIFIED.);
#2100=B_SPLINE_CURVE_WITH_KNOTS('',2,(#40970,#40971,#40972),
 .UNSPECIFIED.,.F.,.F.,(3,3),(0.,1.),.UNSPECIFIED.);
#2101=B_SPLINE_CURVE_WITH_KNOTS('',2,(#40974,#40975,#40976),
 .UNSPECIFIED.,.F.,.F.,(3,3),(0.,1.),.UNSPECIFIED.);
#2102=B_SPLINE_CURVE_WITH_KNOTS('',2,(#40978,#40979,#40980),
 .UNSPECIFIED.,.F.,.F.,(3,3),(0.,1.),.UNSPECIFIED.);
#2103=B_SPLINE_CURVE_WITH_KNOTS('',2,(#40984,#40985,#40986),
 .UNSPECIFIED.,.F.,.F.,(3,3),(0.,1.),.UNSPECIFIED.);
#2104=B_SPLINE_CURVE_WITH_KNOTS('',2,(#40988,#40989,#40990),
 .UNSPECIFIED.,.F.,.F.,(3,3),(0.,1.),.UNSPECIFIED.);
#2105=B_SPLINE_CURVE_WITH_KNOTS('',2,(#40992,#40993,#40994),
 .UNSPECIFIED.,.F.,.F.,(3,3),(0.,1.),.UNSPECIFIED.);
#2106=B_SPLINE_CURVE_WITH_KNOTS('',2,(#40996,#40997,#40998),
 .UNSPECIFIED.,.F.,.F.,(3,3),(0.,1.),.UNSPECIFIED.);
#2107=B_SPLINE_CURVE_WITH_KNOTS('',2,(#41000,#41001,#41002),
 .UNSPECIFIED.,.F.,.F.,(3,3),(0.,1.),.UNSPECIFIED.);
#2108=B_SPLINE_CURVE_WITH_KNOTS('',2,(#41004,#41005,#41006),
 .UNSPECIFIED.,.F.,.F.,(3,3),(0.,1.),.UNSPECIFIED.);
#2109=B_SPLINE_CURVE_WITH_KNOTS('',2,(#41008,#41009,#41010),
 .UNSPECIFIED.,.F.,.F.,(3,3),(0.,1.),.UNSPECIFIED.);
#2110=B_SPLINE_CURVE_WITH_KNOTS('',2,(#41012,#41013,#41014),
 .UNSPECIFIED.,.F.,.F.,(3,3),(0.,1.),.UNSPECIFIED.);
#2111=B_SPLINE_CURVE_WITH_KNOTS('',2,(#41016,#41017,#41018),
 .UNSPECIFIED.,.F.,.F.,(3,3),(0.,1.),.UNSPECIFIED.);
#2112=B_SPLINE_CURVE_WITH_KNOTS('',2,(#41020,#41021,#41022),
 .UNSPECIFIED.,.F.,.F.,(3,3),(0.,1.),.UNSPECIFIED.);
#2113=B_SPLINE_CURVE_WITH_KNOTS('',2,(#41024,#41025,#41026),
 .UNSPECIFIED.,.F.,.F.,(3,3),(0.,1.),.UNSPECIFIED.);
#2114=B_SPLINE_CURVE_WITH_KNOTS('',2,(#41028,#41029,#41030),
 .UNSPECIFIED.,.F.,.F.,(3,3),(0.,1.),.UNSPECIFIED.);
#2115=B_SPLINE_CURVE_WITH_KNOTS('',2,(#41032,#41033,#41034),
 .UNSPECIFIED.,.F.,.F.,(3,3),(0.,1.),.UNSPECIFIED.);
#2116=B_SPLINE_CURVE_WITH_KNOTS('',2,(#41036,#41037,#41038),
 .UNSPECIFIED.,.F.,.F.,(3,3),(0.,1.),.UNSPECIFIED.);
#2117=B_SPLINE_CURVE_WITH_KNOTS('',2,(#41040,#41041,#41042),
 .UNSPECIFIED.,.F.,.F.,(3,3),(0.,1.),.UNSPECIFIED.);
#2118=B_SPLINE_CURVE_WITH_KNOTS('',2,(#41044,#41045,#41046),
 .UNSPECIFIED.,.F.,.F.,(3,3),(0.,1.),.UNSPECIFIED.);
#2119=B_SPLINE_CURVE_WITH_KNOTS('',2,(#41048,#41049,#41050),
 .UNSPECIFIED.,.F.,.F.,(3,3),(0.,1.),.UNSPECIFIED.);
#2120=B_SPLINE_CURVE_WITH_KNOTS('',2,(#41052,#41053,#41054),
 .UNSPECIFIED.,.F.,.F.,(3,3),(0.,1.),.UNSPECIFIED.);
#2121=B_SPLINE_CURVE_WITH_KNOTS('',2,(#41058,#41059,#41060),
 .UNSPECIFIED.,.F.,.F.,(3,3),(0.,1.),.UNSPECIFIED.);
#2122=B_SPLINE_CURVE_WITH_KNOTS('',2,(#41062,#41063,#41064),
 .UNSPECIFIED.,.F.,.F.,(3,3),(0.,1.),.UNSPECIFIED.);
#2123=B_SPLINE_CURVE_WITH_KNOTS('',2,(#41066,#41067,#41068),
 .UNSPECIFIED.,.F.,.F.,(3,3),(0.,1.),.UNSPECIFIED.);
#2124=B_SPLINE_CURVE_WITH_KNOTS('',2,(#41070,#41071,#41072),
 .UNSPECIFIED.,.F.,.F.,(3,3),(0.,1.),.UNSPECIFIED.);
#2125=B_SPLINE_CURVE_WITH_KNOTS('',2,(#41074,#41075,#41076),
 .UNSPECIFIED.,.F.,.F.,(3,3),(0.,1.),.UNSPECIFIED.);
#2126=B_SPLINE_CURVE_WITH_KNOTS('',2,(#41078,#41079,#41080),
 .UNSPECIFIED.,.F.,.F.,(3,3),(0.,1.),.UNSPECIFIED.);
#2127=B_SPLINE_CURVE_WITH_KNOTS('',2,(#41082,#41083,#41084),
 .UNSPECIFIED.,.F.,.F.,(3,3),(0.,1.),.UNSPECIFIED.);
#2128=B_SPLINE_CURVE_WITH_KNOTS('',2,(#41086,#41087,#41088),
 .UNSPECIFIED.,.F.,.F.,(3,3),(0.,1.),.UNSPECIFIED.);
#2129=B_SPLINE_CURVE_WITH_KNOTS('',2,(#41090,#41091,#41092),
 .UNSPECIFIED.,.F.,.F.,(3,3),(0.,1.),.UNSPECIFIED.);
#2130=B_SPLINE_CURVE_WITH_KNOTS('',2,(#41094,#41095,#41096),
 .UNSPECIFIED.,.F.,.F.,(3,3),(0.,1.),.UNSPECIFIED.);
#2131=B_SPLINE_CURVE_WITH_KNOTS('',2,(#41098,#41099,#41100),
 .UNSPECIFIED.,.F.,.F.,(3,3),(0.,1.),.UNSPECIFIED.);
#2132=B_SPLINE_CURVE_WITH_KNOTS('',2,(#41101,#41102,#41103),
 .UNSPECIFIED.,.F.,.F.,(3,3),(0.,1.),.UNSPECIFIED.);
#2133=B_SPLINE_CURVE_WITH_KNOTS('',2,(#41106,#41107,#41108),
 .UNSPECIFIED.,.F.,.F.,(3,3),(0.,1.),.UNSPECIFIED.);
#2134=B_SPLINE_CURVE_WITH_KNOTS('',2,(#41110,#41111,#41112),
 .UNSPECIFIED.,.F.,.F.,(3,3),(0.,1.),.UNSPECIFIED.);
#2135=B_SPLINE_CURVE_WITH_KNOTS('',2,(#41114,#41115,#41116),
 .UNSPECIFIED.,.F.,.F.,(3,3),(0.,1.),.UNSPECIFIED.);
#2136=B_SPLINE_CURVE_WITH_KNOTS('',2,(#41120,#41121,#41122),
 .UNSPECIFIED.,.F.,.F.,(3,3),(0.,1.),.UNSPECIFIED.);
#2137=B_SPLINE_CURVE_WITH_KNOTS('',2,(#41124,#41125,#41126),
 .UNSPECIFIED.,.F.,.F.,(3,3),(0.,1.),.UNSPECIFIED.);
#2138=B_SPLINE_CURVE_WITH_KNOTS('',2,(#41128,#41129,#41130),
 .UNSPECIFIED.,.F.,.F.,(3,3),(0.,1.),.UNSPECIFIED.);
#2139=B_SPLINE_CURVE_WITH_KNOTS('',2,(#41132,#41133,#41134),
 .UNSPECIFIED.,.F.,.F.,(3,3),(0.,1.),.UNSPECIFIED.);
#2140=B_SPLINE_CURVE_WITH_KNOTS('',2,(#41136,#41137,#41138),
 .UNSPECIFIED.,.F.,.F.,(3,3),(0.,1.),.UNSPECIFIED.);
#2141=B_SPLINE_CURVE_WITH_KNOTS('',2,(#41140,#41141,#41142),
 .UNSPECIFIED.,.F.,.F.,(3,3),(0.,1.),.UNSPECIFIED.);
#2142=B_SPLINE_CURVE_WITH_KNOTS('',2,(#41144,#41145,#41146),
 .UNSPECIFIED.,.F.,.F.,(3,3),(0.,1.),.UNSPECIFIED.);
#2143=B_SPLINE_CURVE_WITH_KNOTS('',2,(#41150,#41151,#41152),
 .UNSPECIFIED.,.F.,.F.,(3,3),(0.,1.),.UNSPECIFIED.);
#2144=B_SPLINE_CURVE_WITH_KNOTS('',2,(#41154,#41155,#41156),
 .UNSPECIFIED.,.F.,.F.,(3,3),(0.,1.),.UNSPECIFIED.);
#2145=B_SPLINE_CURVE_WITH_KNOTS('',2,(#41158,#41159,#41160),
 .UNSPECIFIED.,.F.,.F.,(3,3),(0.,1.),.UNSPECIFIED.);
#2146=B_SPLINE_CURVE_WITH_KNOTS('',2,(#41162,#41163,#41164),
 .UNSPECIFIED.,.F.,.F.,(3,3),(0.,1.),.UNSPECIFIED.);
#2147=B_SPLINE_CURVE_WITH_KNOTS('',2,(#41166,#41167,#41168),
 .UNSPECIFIED.,.F.,.F.,(3,3),(0.,1.),.UNSPECIFIED.);
#2148=B_SPLINE_CURVE_WITH_KNOTS('',2,(#41170,#41171,#41172),
 .UNSPECIFIED.,.F.,.F.,(3,3),(0.,1.),.UNSPECIFIED.);
#2149=B_SPLINE_CURVE_WITH_KNOTS('',2,(#41174,#41175,#41176),
 .UNSPECIFIED.,.F.,.F.,(3,3),(0.,1.),.UNSPECIFIED.);
#2150=B_SPLINE_CURVE_WITH_KNOTS('',2,(#41180,#41181,#41182),
 .UNSPECIFIED.,.F.,.F.,(3,3),(0.,1.),.UNSPECIFIED.);
#2151=B_SPLINE_CURVE_WITH_KNOTS('',2,(#41184,#41185,#41186),
 .UNSPECIFIED.,.F.,.F.,(3,3),(0.,1.),.UNSPECIFIED.);
#2152=B_SPLINE_CURVE_WITH_KNOTS('',2,(#41188,#41189,#41190),
 .UNSPECIFIED.,.F.,.F.,(3,3),(0.,1.),.UNSPECIFIED.);
#2153=B_SPLINE_CURVE_WITH_KNOTS('',2,(#41192,#41193,#41194),
 .UNSPECIFIED.,.F.,.F.,(3,3),(0.,1.),.UNSPECIFIED.);
#2154=B_SPLINE_CURVE_WITH_KNOTS('',2,(#41196,#41197,#41198),
 .UNSPECIFIED.,.F.,.F.,(3,3),(0.,1.),.UNSPECIFIED.);
#2155=B_SPLINE_CURVE_WITH_KNOTS('',2,(#41200,#41201,#41202),
 .UNSPECIFIED.,.F.,.F.,(3,3),(0.,1.),.UNSPECIFIED.);
#2156=B_SPLINE_CURVE_WITH_KNOTS('',2,(#41204,#41205,#41206),
 .UNSPECIFIED.,.F.,.F.,(3,3),(0.,1.),.UNSPECIFIED.);
#2157=B_SPLINE_CURVE_WITH_KNOTS('',2,(#41208,#41209,#41210),
 .UNSPECIFIED.,.F.,.F.,(3,3),(0.,1.),.UNSPECIFIED.);
#2158=B_SPLINE_CURVE_WITH_KNOTS('',2,(#41212,#41213,#41214),
 .UNSPECIFIED.,.F.,.F.,(3,3),(0.,1.),.UNSPECIFIED.);
#2159=B_SPLINE_CURVE_WITH_KNOTS('',2,(#41215,#41216,#41217),
 .UNSPECIFIED.,.F.,.F.,(3,3),(0.,1.),.UNSPECIFIED.);
#2160=B_SPLINE_CURVE_WITH_KNOTS('',2,(#41228,#41229,#41230),
 .UNSPECIFIED.,.F.,.F.,(3,3),(0.,1.),.UNSPECIFIED.);
#2161=B_SPLINE_CURVE_WITH_KNOTS('',2,(#41232,#41233,#41234),
 .UNSPECIFIED.,.F.,.F.,(3,3),(0.,1.),.UNSPECIFIED.);
#2162=B_SPLINE_CURVE_WITH_KNOTS('',2,(#41236,#41237,#41238),
 .UNSPECIFIED.,.F.,.F.,(3,3),(0.,1.),.UNSPECIFIED.);
#2163=B_SPLINE_CURVE_WITH_KNOTS('',2,(#41242,#41243,#41244),
 .UNSPECIFIED.,.F.,.F.,(3,3),(0.,1.),.UNSPECIFIED.);
#2164=B_SPLINE_CURVE_WITH_KNOTS('',2,(#41246,#41247,#41248),
 .UNSPECIFIED.,.F.,.F.,(3,3),(0.,1.),.UNSPECIFIED.);
#2165=B_SPLINE_CURVE_WITH_KNOTS('',2,(#41250,#41251,#41252),
 .UNSPECIFIED.,.F.,.F.,(3,3),(0.,1.),.UNSPECIFIED.);
#2166=B_SPLINE_CURVE_WITH_KNOTS('',2,(#41254,#41255,#41256),
 .UNSPECIFIED.,.F.,.F.,(3,3),(0.,1.),.UNSPECIFIED.);
#2167=B_SPLINE_CURVE_WITH_KNOTS('',2,(#41258,#41259,#41260),
 .UNSPECIFIED.,.F.,.F.,(3,3),(0.,1.),.UNSPECIFIED.);
#2168=B_SPLINE_CURVE_WITH_KNOTS('',2,(#41262,#41263,#41264),
 .UNSPECIFIED.,.F.,.F.,(3,3),(0.,1.),.UNSPECIFIED.);
#2169=B_SPLINE_CURVE_WITH_KNOTS('',2,(#41266,#41267,#41268),
 .UNSPECIFIED.,.F.,.F.,(3,3),(0.,1.),.UNSPECIFIED.);
#2170=B_SPLINE_CURVE_WITH_KNOTS('',2,(#41270,#41271,#41272),
 .UNSPECIFIED.,.F.,.F.,(3,3),(0.,1.),.UNSPECIFIED.);
#2171=B_SPLINE_CURVE_WITH_KNOTS('',2,(#41274,#41275,#41276),
 .UNSPECIFIED.,.F.,.F.,(3,3),(0.,1.),.UNSPECIFIED.);
#2172=B_SPLINE_CURVE_WITH_KNOTS('',2,(#41278,#41279,#41280),
 .UNSPECIFIED.,.F.,.F.,(3,3),(0.,1.),.UNSPECIFIED.);
#2173=B_SPLINE_CURVE_WITH_KNOTS('',2,(#41282,#41283,#41284),
 .UNSPECIFIED.,.F.,.F.,(3,3),(0.,1.),.UNSPECIFIED.);
#2174=B_SPLINE_CURVE_WITH_KNOTS('',2,(#41286,#41287,#41288),
 .UNSPECIFIED.,.F.,.F.,(3,3),(0.,1.),.UNSPECIFIED.);
#2175=B_SPLINE_CURVE_WITH_KNOTS('',2,(#41290,#41291,#41292),
 .UNSPECIFIED.,.F.,.F.,(3,3),(0.,1.),.UNSPECIFIED.);
#2176=B_SPLINE_CURVE_WITH_KNOTS('',2,(#41294,#41295,#41296),
 .UNSPECIFIED.,.F.,.F.,(3,3),(0.,1.),.UNSPECIFIED.);
#2177=B_SPLINE_CURVE_WITH_KNOTS('',2,(#41298,#41299,#41300),
 .UNSPECIFIED.,.F.,.F.,(3,3),(0.,1.),.UNSPECIFIED.);
#2178=B_SPLINE_CURVE_WITH_KNOTS('',2,(#41302,#41303,#41304),
 .UNSPECIFIED.,.F.,.F.,(3,3),(0.,1.),.UNSPECIFIED.);
#2179=B_SPLINE_CURVE_WITH_KNOTS('',2,(#41306,#41307,#41308),
 .UNSPECIFIED.,.F.,.F.,(3,3),(0.,1.),.UNSPECIFIED.);
#2180=B_SPLINE_CURVE_WITH_KNOTS('',2,(#41310,#41311,#41312),
 .UNSPECIFIED.,.F.,.F.,(3,3),(0.,1.),.UNSPECIFIED.);
#2181=B_SPLINE_CURVE_WITH_KNOTS('',2,(#41316,#41317,#41318),
 .UNSPECIFIED.,.F.,.F.,(3,3),(0.,1.),.UNSPECIFIED.);
#2182=B_SPLINE_CURVE_WITH_KNOTS('',2,(#41320,#41321,#41322),
 .UNSPECIFIED.,.F.,.F.,(3,3),(0.,1.),.UNSPECIFIED.);
#2183=B_SPLINE_CURVE_WITH_KNOTS('',2,(#41324,#41325,#41326),
 .UNSPECIFIED.,.F.,.F.,(3,3),(0.,1.),.UNSPECIFIED.);
#2184=B_SPLINE_CURVE_WITH_KNOTS('',2,(#41328,#41329,#41330),
 .UNSPECIFIED.,.F.,.F.,(3,3),(0.,1.),.UNSPECIFIED.);
#2185=B_SPLINE_CURVE_WITH_KNOTS('',2,(#41332,#41333,#41334),
 .UNSPECIFIED.,.F.,.F.,(3,3),(0.,1.),.UNSPECIFIED.);
#2186=B_SPLINE_CURVE_WITH_KNOTS('',2,(#41336,#41337,#41338),
 .UNSPECIFIED.,.F.,.F.,(3,3),(0.,1.),.UNSPECIFIED.);
#2187=B_SPLINE_CURVE_WITH_KNOTS('',2,(#41340,#41341,#41342),
 .UNSPECIFIED.,.F.,.F.,(3,3),(0.,1.),.UNSPECIFIED.);
#2188=B_SPLINE_CURVE_WITH_KNOTS('',2,(#41344,#41345,#41346),
 .UNSPECIFIED.,.F.,.F.,(3,3),(0.,1.),.UNSPECIFIED.);
#2189=B_SPLINE_CURVE_WITH_KNOTS('',2,(#41348,#41349,#41350),
 .UNSPECIFIED.,.F.,.F.,(3,3),(0.,1.),.UNSPECIFIED.);
#2190=B_SPLINE_CURVE_WITH_KNOTS('',2,(#41352,#41353,#41354),
 .UNSPECIFIED.,.F.,.F.,(3,3),(0.,1.),.UNSPECIFIED.);
#2191=B_SPLINE_CURVE_WITH_KNOTS('',2,(#41356,#41357,#41358),
 .UNSPECIFIED.,.F.,.F.,(3,3),(0.,1.),.UNSPECIFIED.);
#2192=B_SPLINE_CURVE_WITH_KNOTS('',2,(#41359,#41360,#41361),
 .UNSPECIFIED.,.F.,.F.,(3,3),(0.,1.),.UNSPECIFIED.);
#2193=B_SPLINE_CURVE_WITH_KNOTS('',2,(#41617,#41618,#41619),
 .UNSPECIFIED.,.F.,.F.,(3,3),(0.,1.),.UNSPECIFIED.);
#2194=B_SPLINE_CURVE_WITH_KNOTS('',2,(#41628,#41629,#41630),
 .UNSPECIFIED.,.F.,.F.,(3,3),(0.,1.),.UNSPECIFIED.);
#2195=B_SPLINE_CURVE_WITH_KNOTS('',2,(#41639,#41640,#41641),
 .UNSPECIFIED.,.F.,.F.,(3,3),(0.,1.),.UNSPECIFIED.);
#2196=B_SPLINE_CURVE_WITH_KNOTS('',2,(#41650,#41651,#41652),
 .UNSPECIFIED.,.F.,.F.,(3,3),(0.,1.),.UNSPECIFIED.);
#2197=B_SPLINE_CURVE_WITH_KNOTS('',2,(#41673,#41674,#41675),
 .UNSPECIFIED.,.F.,.F.,(3,3),(0.,1.),.UNSPECIFIED.);
#2198=B_SPLINE_CURVE_WITH_KNOTS('',2,(#41684,#41685,#41686),
 .UNSPECIFIED.,.F.,.F.,(3,3),(0.,1.),.UNSPECIFIED.);
#2199=B_SPLINE_CURVE_WITH_KNOTS('',2,(#41695,#41696,#41697),
 .UNSPECIFIED.,.F.,.F.,(3,3),(0.,1.),.UNSPECIFIED.);
#2200=B_SPLINE_CURVE_WITH_KNOTS('',2,(#41706,#41707,#41708),
 .UNSPECIFIED.,.F.,.F.,(3,3),(0.,1.),.UNSPECIFIED.);
#2201=B_SPLINE_CURVE_WITH_KNOTS('',2,(#41717,#41718,#41719),
 .UNSPECIFIED.,.F.,.F.,(3,3),(0.,1.),.UNSPECIFIED.);
#2202=B_SPLINE_CURVE_WITH_KNOTS('',2,(#41728,#41729,#41730),
 .UNSPECIFIED.,.F.,.F.,(3,3),(0.,1.),.UNSPECIFIED.);
#2203=B_SPLINE_CURVE_WITH_KNOTS('',2,(#41739,#41740,#41741),
 .UNSPECIFIED.,.F.,.F.,(3,3),(0.,1.),.UNSPECIFIED.);
#2204=B_SPLINE_CURVE_WITH_KNOTS('',2,(#41815,#41816,#41817),
 .UNSPECIFIED.,.F.,.F.,(3,3),(0.,1.),.UNSPECIFIED.);
#2205=B_SPLINE_CURVE_WITH_KNOTS('',2,(#41827,#41828,#41829),
 .UNSPECIFIED.,.F.,.F.,(3,3),(0.,1.),.UNSPECIFIED.);
#2206=B_SPLINE_CURVE_WITH_KNOTS('',2,(#41842,#41843,#41844),
 .UNSPECIFIED.,.F.,.F.,(3,3),(0.,1.),.UNSPECIFIED.);
#2207=B_SPLINE_CURVE_WITH_KNOTS('',2,(#41853,#41854,#41855),
 .UNSPECIFIED.,.F.,.F.,(3,3),(0.,1.),.UNSPECIFIED.);
#2208=B_SPLINE_CURVE_WITH_KNOTS('',2,(#41864,#41865,#41866),
 .UNSPECIFIED.,.F.,.F.,(3,3),(0.,1.),.UNSPECIFIED.);
#2209=B_SPLINE_CURVE_WITH_KNOTS('',2,(#41889,#41890,#41891),
 .UNSPECIFIED.,.F.,.F.,(3,3),(0.,1.),.UNSPECIFIED.);
#2210=B_SPLINE_CURVE_WITH_KNOTS('',2,(#41902,#41903,#41904),
 .UNSPECIFIED.,.F.,.F.,(3,3),(0.,1.),.UNSPECIFIED.);
#2211=B_SPLINE_CURVE_WITH_KNOTS('',2,(#41914,#41915,#41916),
 .UNSPECIFIED.,.F.,.F.,(3,3),(0.,1.),.UNSPECIFIED.);
#2212=B_SPLINE_CURVE_WITH_KNOTS('',2,(#41925,#41926,#41927),
 .UNSPECIFIED.,.F.,.F.,(3,3),(0.,1.),.UNSPECIFIED.);
#2213=B_SPLINE_CURVE_WITH_KNOTS('',2,(#41936,#41937,#41938),
 .UNSPECIFIED.,.F.,.F.,(3,3),(0.,1.),.UNSPECIFIED.);
#2214=B_SPLINE_CURVE_WITH_KNOTS('',2,(#41947,#41948,#41949),
 .UNSPECIFIED.,.F.,.F.,(3,3),(0.,1.),.UNSPECIFIED.);
#2215=B_SPLINE_CURVE_WITH_KNOTS('',2,(#41958,#41959,#41960),
 .UNSPECIFIED.,.F.,.F.,(3,3),(0.,1.),.UNSPECIFIED.);
#2216=B_SPLINE_CURVE_WITH_KNOTS('',2,(#41969,#41970,#41971),
 .UNSPECIFIED.,.F.,.F.,(3,3),(0.,1.),.UNSPECIFIED.);
#2217=B_SPLINE_CURVE_WITH_KNOTS('',2,(#41980,#41981,#41982),
 .UNSPECIFIED.,.F.,.F.,(3,3),(0.,1.),.UNSPECIFIED.);
#2218=B_SPLINE_CURVE_WITH_KNOTS('',2,(#41991,#41992,#41993),
 .UNSPECIFIED.,.F.,.F.,(3,3),(0.,1.),.UNSPECIFIED.);
#2219=B_SPLINE_CURVE_WITH_KNOTS('',2,(#42002,#42003,#42004),
 .UNSPECIFIED.,.F.,.F.,(3,3),(0.,1.),.UNSPECIFIED.);
#2220=B_SPLINE_CURVE_WITH_KNOTS('',2,(#42013,#42014,#42015),
 .UNSPECIFIED.,.F.,.F.,(3,3),(0.,1.),.UNSPECIFIED.);
#2221=B_SPLINE_CURVE_WITH_KNOTS('',2,(#42024,#42025,#42026),
 .UNSPECIFIED.,.F.,.F.,(3,3),(0.,1.),.UNSPECIFIED.);
#2222=B_SPLINE_CURVE_WITH_KNOTS('',2,(#42035,#42036,#42037),
 .UNSPECIFIED.,.F.,.F.,(3,3),(0.,1.),.UNSPECIFIED.);
#2223=B_SPLINE_CURVE_WITH_KNOTS('',2,(#42050,#42051,#42052),
 .UNSPECIFIED.,.F.,.F.,(3,3),(0.,1.),.UNSPECIFIED.);
#2224=B_SPLINE_CURVE_WITH_KNOTS('',2,(#42061,#42062,#42063),
 .UNSPECIFIED.,.F.,.F.,(3,3),(0.,1.),.UNSPECIFIED.);
#2225=B_SPLINE_CURVE_WITH_KNOTS('',2,(#42072,#42073,#42074),
 .UNSPECIFIED.,.F.,.F.,(3,3),(0.,1.),.UNSPECIFIED.);
#2226=B_SPLINE_CURVE_WITH_KNOTS('',2,(#42083,#42084,#42085),
 .UNSPECIFIED.,.F.,.F.,(3,3),(0.,1.),.UNSPECIFIED.);
#2227=B_SPLINE_CURVE_WITH_KNOTS('',2,(#42094,#42095,#42096),
 .UNSPECIFIED.,.F.,.F.,(3,3),(0.,1.),.UNSPECIFIED.);
#2228=B_SPLINE_CURVE_WITH_KNOTS('',2,(#42105,#42106,#42107),
 .UNSPECIFIED.,.F.,.F.,(3,3),(0.,1.),.UNSPECIFIED.);
#2229=B_SPLINE_CURVE_WITH_KNOTS('',2,(#42116,#42117,#42118),
 .UNSPECIFIED.,.F.,.F.,(3,3),(0.,1.),.UNSPECIFIED.);
#2230=B_SPLINE_CURVE_WITH_KNOTS('',2,(#42127,#42128,#42129),
 .UNSPECIFIED.,.F.,.F.,(3,3),(0.,1.),.UNSPECIFIED.);
#2231=B_SPLINE_CURVE_WITH_KNOTS('',2,(#42138,#42139,#42140),
 .UNSPECIFIED.,.F.,.F.,(3,3),(0.,1.),.UNSPECIFIED.);
#2232=B_SPLINE_CURVE_WITH_KNOTS('',2,(#42149,#42150,#42151),
 .UNSPECIFIED.,.F.,.F.,(3,3),(0.,1.),.UNSPECIFIED.);
#2233=B_SPLINE_CURVE_WITH_KNOTS('',2,(#42160,#42161,#42162),
 .UNSPECIFIED.,.F.,.F.,(3,3),(0.,1.),.UNSPECIFIED.);
#2234=B_SPLINE_CURVE_WITH_KNOTS('',2,(#42171,#42172,#42173),
 .UNSPECIFIED.,.F.,.F.,(3,3),(0.,1.),.UNSPECIFIED.);
#2235=B_SPLINE_CURVE_WITH_KNOTS('',2,(#42182,#42183,#42184),
 .UNSPECIFIED.,.F.,.F.,(3,3),(0.,1.),.UNSPECIFIED.);
#2236=B_SPLINE_CURVE_WITH_KNOTS('',2,(#42193,#42194,#42195),
 .UNSPECIFIED.,.F.,.F.,(3,3),(0.,1.),.UNSPECIFIED.);
#2237=B_SPLINE_CURVE_WITH_KNOTS('',2,(#42204,#42205,#42206),
 .UNSPECIFIED.,.F.,.F.,(3,3),(0.,1.),.UNSPECIFIED.);
#2238=B_SPLINE_CURVE_WITH_KNOTS('',2,(#42215,#42216,#42217),
 .UNSPECIFIED.,.F.,.F.,(3,3),(0.,1.),.UNSPECIFIED.);
#2239=B_SPLINE_CURVE_WITH_KNOTS('',2,(#42226,#42227,#42228),
 .UNSPECIFIED.,.F.,.F.,(3,3),(0.,1.),.UNSPECIFIED.);
#2240=B_SPLINE_CURVE_WITH_KNOTS('',2,(#42237,#42238,#42239),
 .UNSPECIFIED.,.F.,.F.,(3,3),(0.,1.),.UNSPECIFIED.);
#2241=B_SPLINE_CURVE_WITH_KNOTS('',2,(#42252,#42253,#42254),
 .UNSPECIFIED.,.F.,.F.,(3,3),(0.,1.),.UNSPECIFIED.);
#2242=B_SPLINE_CURVE_WITH_KNOTS('',2,(#42261,#42262,#42263),
 .UNSPECIFIED.,.F.,.F.,(3,3),(0.,1.),.UNSPECIFIED.);
#2243=B_SPLINE_CURVE_WITH_KNOTS('',2,(#42274,#42275,#42276),
 .UNSPECIFIED.,.F.,.F.,(3,3),(0.,1.),.UNSPECIFIED.);
#2244=B_SPLINE_CURVE_WITH_KNOTS('',2,(#42286,#42287,#42288),
 .UNSPECIFIED.,.F.,.F.,(3,3),(0.,1.),.UNSPECIFIED.);
#2245=B_SPLINE_CURVE_WITH_KNOTS('',2,(#42297,#42298,#42299),
 .UNSPECIFIED.,.F.,.F.,(3,3),(0.,1.),.UNSPECIFIED.);
#2246=B_SPLINE_CURVE_WITH_KNOTS('',2,(#42308,#42309,#42310),
 .UNSPECIFIED.,.F.,.F.,(3,3),(0.,1.),.UNSPECIFIED.);
#2247=B_SPLINE_CURVE_WITH_KNOTS('',2,(#42319,#42320,#42321),
 .UNSPECIFIED.,.F.,.F.,(3,3),(0.,1.),.UNSPECIFIED.);
#2248=B_SPLINE_CURVE_WITH_KNOTS('',2,(#42330,#42331,#42332),
 .UNSPECIFIED.,.F.,.F.,(3,3),(0.,1.),.UNSPECIFIED.);
#2249=B_SPLINE_CURVE_WITH_KNOTS('',2,(#42341,#42342,#42343),
 .UNSPECIFIED.,.F.,.F.,(3,3),(0.,1.),.UNSPECIFIED.);
#2250=B_SPLINE_CURVE_WITH_KNOTS('',2,(#42352,#42353,#42354),
 .UNSPECIFIED.,.F.,.F.,(3,3),(0.,1.),.UNSPECIFIED.);
#2251=B_SPLINE_CURVE_WITH_KNOTS('',2,(#42363,#42364,#42365),
 .UNSPECIFIED.,.F.,.F.,(3,3),(0.,1.),.UNSPECIFIED.);
#2252=B_SPLINE_CURVE_WITH_KNOTS('',2,(#42374,#42375,#42376),
 .UNSPECIFIED.,.F.,.F.,(3,3),(0.,1.),.UNSPECIFIED.);
#2253=B_SPLINE_CURVE_WITH_KNOTS('',2,(#42385,#42386,#42387),
 .UNSPECIFIED.,.F.,.F.,(3,3),(0.,1.),.UNSPECIFIED.);
#2254=B_SPLINE_CURVE_WITH_KNOTS('',2,(#42400,#42401,#42402),
 .UNSPECIFIED.,.F.,.F.,(3,3),(0.,1.),.UNSPECIFIED.);
#2255=B_SPLINE_CURVE_WITH_KNOTS('',2,(#42411,#42412,#42413),
 .UNSPECIFIED.,.F.,.F.,(3,3),(0.,1.),.UNSPECIFIED.);
#2256=B_SPLINE_CURVE_WITH_KNOTS('',2,(#42422,#42423,#42424),
 .UNSPECIFIED.,.F.,.F.,(3,3),(0.,1.),.UNSPECIFIED.);
#2257=B_SPLINE_CURVE_WITH_KNOTS('',2,(#42433,#42434,#42435),
 .UNSPECIFIED.,.F.,.F.,(3,3),(0.,1.),.UNSPECIFIED.);
#2258=B_SPLINE_CURVE_WITH_KNOTS('',2,(#42444,#42445,#42446),
 .UNSPECIFIED.,.F.,.F.,(3,3),(0.,1.),.UNSPECIFIED.);
#2259=B_SPLINE_CURVE_WITH_KNOTS('',2,(#42455,#42456,#42457),
 .UNSPECIFIED.,.F.,.F.,(3,3),(0.,1.),.UNSPECIFIED.);
#2260=B_SPLINE_CURVE_WITH_KNOTS('',2,(#42466,#42467,#42468),
 .UNSPECIFIED.,.F.,.F.,(3,3),(0.,1.),.UNSPECIFIED.);
#2261=B_SPLINE_CURVE_WITH_KNOTS('',2,(#42481,#42482,#42483),
 .UNSPECIFIED.,.F.,.F.,(3,3),(0.,1.),.UNSPECIFIED.);
#2262=B_SPLINE_CURVE_WITH_KNOTS('',2,(#42492,#42493,#42494),
 .UNSPECIFIED.,.F.,.F.,(3,3),(0.,1.),.UNSPECIFIED.);
#2263=B_SPLINE_CURVE_WITH_KNOTS('',2,(#42503,#42504,#42505),
 .UNSPECIFIED.,.F.,.F.,(3,3),(0.,1.),.UNSPECIFIED.);
#2264=B_SPLINE_CURVE_WITH_KNOTS('',2,(#42514,#42515,#42516),
 .UNSPECIFIED.,.F.,.F.,(3,3),(0.,1.),.UNSPECIFIED.);
#2265=B_SPLINE_CURVE_WITH_KNOTS('',2,(#42525,#42526,#42527),
 .UNSPECIFIED.,.F.,.F.,(3,3),(0.,1.),.UNSPECIFIED.);
#2266=B_SPLINE_CURVE_WITH_KNOTS('',2,(#42536,#42537,#42538),
 .UNSPECIFIED.,.F.,.F.,(3,3),(0.,1.),.UNSPECIFIED.);
#2267=B_SPLINE_CURVE_WITH_KNOTS('',2,(#42547,#42548,#42549),
 .UNSPECIFIED.,.F.,.F.,(3,3),(0.,1.),.UNSPECIFIED.);
#2268=B_SPLINE_CURVE_WITH_KNOTS('',2,(#42562,#42563,#42564),
 .UNSPECIFIED.,.F.,.F.,(3,3),(0.,1.),.UNSPECIFIED.);
#2269=B_SPLINE_CURVE_WITH_KNOTS('',2,(#42571,#42572,#42573),
 .UNSPECIFIED.,.F.,.F.,(3,3),(0.,1.),.UNSPECIFIED.);
#2270=B_SPLINE_CURVE_WITH_KNOTS('',2,(#42601,#42602,#42603),
 .UNSPECIFIED.,.F.,.F.,(3,3),(0.,1.),.UNSPECIFIED.);
#2271=B_SPLINE_CURVE_WITH_KNOTS('',2,(#42613,#42614,#42615),
 .UNSPECIFIED.,.F.,.F.,(3,3),(0.,1.),.UNSPECIFIED.);
#2272=B_SPLINE_CURVE_WITH_KNOTS('',2,(#42624,#42625,#42626),
 .UNSPECIFIED.,.F.,.F.,(3,3),(0.,1.),.UNSPECIFIED.);
#2273=B_SPLINE_CURVE_WITH_KNOTS('',2,(#42635,#42636,#42637),
 .UNSPECIFIED.,.F.,.F.,(3,3),(0.,1.),.UNSPECIFIED.);
#2274=B_SPLINE_CURVE_WITH_KNOTS('',2,(#42646,#42647,#42648),
 .UNSPECIFIED.,.F.,.F.,(3,3),(0.,1.),.UNSPECIFIED.);
#2275=B_SPLINE_CURVE_WITH_KNOTS('',2,(#42657,#42658,#42659),
 .UNSPECIFIED.,.F.,.F.,(3,3),(0.,1.),.UNSPECIFIED.);
#2276=B_SPLINE_CURVE_WITH_KNOTS('',2,(#42668,#42669,#42670),
 .UNSPECIFIED.,.F.,.F.,(3,3),(0.,1.),.UNSPECIFIED.);
#2277=B_SPLINE_CURVE_WITH_KNOTS('',2,(#42679,#42680,#42681),
 .UNSPECIFIED.,.F.,.F.,(3,3),(0.,1.),.UNSPECIFIED.);
#2278=B_SPLINE_CURVE_WITH_KNOTS('',2,(#42690,#42691,#42692),
 .UNSPECIFIED.,.F.,.F.,(3,3),(0.,1.),.UNSPECIFIED.);
#2279=B_SPLINE_CURVE_WITH_KNOTS('',2,(#42701,#42702,#42703),
 .UNSPECIFIED.,.F.,.F.,(3,3),(0.,1.),.UNSPECIFIED.);
#2280=B_SPLINE_CURVE_WITH_KNOTS('',2,(#42712,#42713,#42714),
 .UNSPECIFIED.,.F.,.F.,(3,3),(0.,1.),.UNSPECIFIED.);
#2281=B_SPLINE_CURVE_WITH_KNOTS('',2,(#42723,#42724,#42725),
 .UNSPECIFIED.,.F.,.F.,(3,3),(0.,1.),.UNSPECIFIED.);
#2282=B_SPLINE_CURVE_WITH_KNOTS('',2,(#42734,#42735,#42736),
 .UNSPECIFIED.,.F.,.F.,(3,3),(0.,1.),.UNSPECIFIED.);
#2283=B_SPLINE_CURVE_WITH_KNOTS('',2,(#42749,#42750,#42751),
 .UNSPECIFIED.,.F.,.F.,(3,3),(0.,1.),.UNSPECIFIED.);
#2284=B_SPLINE_CURVE_WITH_KNOTS('',2,(#42760,#42761,#42762),
 .UNSPECIFIED.,.F.,.F.,(3,3),(0.,1.),.UNSPECIFIED.);
#2285=B_SPLINE_CURVE_WITH_KNOTS('',2,(#42771,#42772,#42773),
 .UNSPECIFIED.,.F.,.F.,(3,3),(0.,1.),.UNSPECIFIED.);
#2286=B_SPLINE_CURVE_WITH_KNOTS('',2,(#42782,#42783,#42784),
 .UNSPECIFIED.,.F.,.F.,(3,3),(0.,1.),.UNSPECIFIED.);
#2287=B_SPLINE_CURVE_WITH_KNOTS('',2,(#42793,#42794,#42795),
 .UNSPECIFIED.,.F.,.F.,(3,3),(0.,1.),.UNSPECIFIED.);
#2288=B_SPLINE_CURVE_WITH_KNOTS('',2,(#42804,#42805,#42806),
 .UNSPECIFIED.,.F.,.F.,(3,3),(0.,1.),.UNSPECIFIED.);
#2289=B_SPLINE_CURVE_WITH_KNOTS('',2,(#42815,#42816,#42817),
 .UNSPECIFIED.,.F.,.F.,(3,3),(0.,1.),.UNSPECIFIED.);
#2290=B_SPLINE_CURVE_WITH_KNOTS('',2,(#42826,#42827,#42828),
 .UNSPECIFIED.,.F.,.F.,(3,3),(0.,1.),.UNSPECIFIED.);
#2291=B_SPLINE_CURVE_WITH_KNOTS('',2,(#42837,#42838,#42839),
 .UNSPECIFIED.,.F.,.F.,(3,3),(0.,1.),.UNSPECIFIED.);
#2292=B_SPLINE_CURVE_WITH_KNOTS('',2,(#42848,#42849,#42850),
 .UNSPECIFIED.,.F.,.F.,(3,3),(0.,1.),.UNSPECIFIED.);
#2293=B_SPLINE_CURVE_WITH_KNOTS('',2,(#42859,#42860,#42861),
 .UNSPECIFIED.,.F.,.F.,(3,3),(0.,1.),.UNSPECIFIED.);
#2294=B_SPLINE_CURVE_WITH_KNOTS('',2,(#42870,#42871,#42872),
 .UNSPECIFIED.,.F.,.F.,(3,3),(0.,1.),.UNSPECIFIED.);
#2295=B_SPLINE_CURVE_WITH_KNOTS('',2,(#42881,#42882,#42883),
 .UNSPECIFIED.,.F.,.F.,(3,3),(0.,1.),.UNSPECIFIED.);
#2296=B_SPLINE_CURVE_WITH_KNOTS('',2,(#42892,#42893,#42894),
 .UNSPECIFIED.,.F.,.F.,(3,3),(0.,1.),.UNSPECIFIED.);
#2297=B_SPLINE_CURVE_WITH_KNOTS('',2,(#42903,#42904,#42905),
 .UNSPECIFIED.,.F.,.F.,(3,3),(0.,1.),.UNSPECIFIED.);
#2298=B_SPLINE_CURVE_WITH_KNOTS('',2,(#42914,#42915,#42916),
 .UNSPECIFIED.,.F.,.F.,(3,3),(0.,1.),.UNSPECIFIED.);
#2299=B_SPLINE_CURVE_WITH_KNOTS('',2,(#42925,#42926,#42927),
 .UNSPECIFIED.,.F.,.F.,(3,3),(0.,1.),.UNSPECIFIED.);
#2300=B_SPLINE_CURVE_WITH_KNOTS('',2,(#42936,#42937,#42938),
 .UNSPECIFIED.,.F.,.F.,(3,3),(0.,1.),.UNSPECIFIED.);
#2301=B_SPLINE_CURVE_WITH_KNOTS('',2,(#42951,#42952,#42953),
 .UNSPECIFIED.,.F.,.F.,(3,3),(0.,1.),.UNSPECIFIED.);
#2302=B_SPLINE_CURVE_WITH_KNOTS('',2,(#42960,#42961,#42962),
 .UNSPECIFIED.,.F.,.F.,(3,3),(0.,1.),.UNSPECIFIED.);
#2303=B_SPLINE_CURVE_WITH_KNOTS('',3,(#43245,#43246,#43247,#43248),
 .UNSPECIFIED.,.F.,.F.,(4,4),(0.,0.0472495496003301),.UNSPECIFIED.);
#2304=B_SPLINE_CURVE_WITH_KNOTS('',3,(#43495,#43496,#43497,#43498,#43499,
#43500,#43501,#43502,#43503,#43504),.UNSPECIFIED.,.F.,.F.,(4,2,2,2,4),(0.495600103897638,
0.617811944958686,0.790142329574639,0.962472714190591,1.08468455525164),
 .UNSPECIFIED.);
#2305=B_SPLINE_CURVE_WITH_KNOTS('',3,(#43626,#43627,#43628,#43629,#43630,
#43631,#43632,#43633,#43634,#43635,#43636,#43637,#43638,#43639,#43640,#43641,
#43642,#43643),.UNSPECIFIED.,.F.,.F.,(4,2,2,2,2,2,2,2,4),(0.227910044047723,
0.284874338888031,0.34183863372834,0.398829360911893,0.455820088095446,
0.512810815278999,0.569801542462552,0.626765837302861,0.683730132143169),
 .UNSPECIFIED.);
#2306=B_SPLINE_CURVE_WITH_KNOTS('',3,(#43645,#43646,#43647,#43648,#43649,
#43650,#43651,#43652,#43653,#43654),.UNSPECIFIED.,.F.,.F.,(4,2,2,2,4),(0.,
0.0569907271835534,0.113981454367107,0.170945749207415,0.227910044047723),
 .UNSPECIFIED.);
#2307=B_SPLINE_CURVE_WITH_KNOTS('',3,(#43655,#43656,#43657,#43658,#43659,
#43660,#43661,#43662,#43663,#43664),.UNSPECIFIED.,.F.,.F.,(4,2,2,2,4),(0.683730132143169,
0.740694426983477,0.797658721823785,0.854649449007338,0.911640176190892),
 .UNSPECIFIED.);
#2308=B_SPLINE_CURVE_WITH_KNOTS('',3,(#43668,#43669,#43670,#43671,#43672,
#43673,#43674,#43675,#43676,#43677),.UNSPECIFIED.,.F.,.F.,(4,2,2,2,4),(0.,
0.0569907271835534,0.113981454367107,0.170945749207415,0.227910044047723),
 .UNSPECIFIED.);
#2309=B_SPLINE_CURVE_WITH_KNOTS('',3,(#43678,#43679,#43680,#43681,#43682,
#43683,#43684,#43685,#43686,#43687,#43688,#43689,#43690,#43691,#43692,#43693,
#43694,#43695,#43696,#43697,#43698,#43699,#43700,#43701,#43702,#43703),
 .UNSPECIFIED.,.F.,.F.,(4,2,2,2,2,2,2,2,2,2,2,2,4),(0.227910044047723,0.284874338888031,
0.34183863372834,0.398829360911893,0.455820088095446,0.512810815278999,
0.569801542462552,0.626765837302861,0.683730132143169,0.740694426983477,
0.797658721823785,0.854649449007338,0.911640176190892),.UNSPECIFIED.);
#2310=B_SPLINE_CURVE_WITH_KNOTS('',3,(#44570,#44571,#44572,#44573,#44574,
#44575),.UNSPECIFIED.,.F.,.F.,(4,2,4),(1.60159343096041,1.75059102484718,
1.89958861873394),.UNSPECIFIED.);
#2311=B_SPLINE_CURVE_WITH_KNOTS('',3,(#44727,#44728,#44729,#44730,#44731,
#44732,#44733,#44734,#44735,#44736),.UNSPECIFIED.,.F.,.F.,(4,2,2,2,4),(0.,
0.056990727183553,0.113981454367106,0.170945749207414,0.227910044047722),
 .UNSPECIFIED.);
#2312=B_SPLINE_CURVE_WITH_KNOTS('',3,(#44738,#44739,#44740,#44741,#44742,
#44743,#44744,#44745,#44746,#44747),.UNSPECIFIED.,.F.,.F.,(4,2,2,2,4),(0.683730132143166,
0.740694426983474,0.797658721823782,0.854649449007335,0.911640176190888),
 .UNSPECIFIED.);
#2313=B_SPLINE_CURVE_WITH_KNOTS('',3,(#44748,#44749,#44750,#44751,#44752,
#44753,#44754,#44755,#44756,#44757,#44758,#44759,#44760,#44761,#44762,#44763,
#44764,#44765),.UNSPECIFIED.,.F.,.F.,(4,2,2,2,2,2,2,2,4),(0.227910044047722,
0.28487433888803,0.341838633728338,0.398829360911891,0.455820088095444,
0.512810815278997,0.56980154246255,0.626765837302858,0.683730132143166),
 .UNSPECIFIED.);
#2314=B_SPLINE_CURVE_WITH_KNOTS('',3,(#44769,#44770,#44771,#44772,#44773,
#44774,#44775,#44776,#44777,#44778,#44779,#44780,#44781,#44782,#44783,#44784,
#44785,#44786,#44787,#44788,#44789,#44790,#44791,#44792,#44793,#44794),
 .UNSPECIFIED.,.F.,.F.,(4,2,2,2,2,2,2,2,2,2,2,2,4),(0.,0.056990727183553,
0.113981454367106,0.170945749207414,0.227910044047722,0.28487433888803,
0.341838633728338,0.398829360911891,0.455820088095444,0.512810815278997,
0.56980154246255,0.626765837302858,0.683730132143166),.UNSPECIFIED.);
#2315=B_SPLINE_CURVE_WITH_KNOTS('',3,(#44795,#44796,#44797,#44798,#44799,
#44800,#44801,#44802,#44803,#44804),.UNSPECIFIED.,.F.,.F.,(4,2,2,2,4),(0.683730132143166,
0.740694426983474,0.797658721823782,0.854649449007335,0.911640176190888),
 .UNSPECIFIED.);
#2316=B_SPLINE_CURVE_WITH_KNOTS('',3,(#44822,#44823,#44824,#44825),
 .UNSPECIFIED.,.F.,.F.,(4,4),(-0.00278496917063749,0.000381985128916583),
 .UNSPECIFIED.);
#2317=B_SPLINE_CURVE_WITH_KNOTS('',3,(#44827,#44828,#44829,#44830,#44831,
#44832,#44833,#44834,#44835,#44836,#44837,#44838,#44839,#44840,#44841,#44842,
#44843,#44844,#44845,#44846,#44847,#44848),.UNSPECIFIED.,.F.,.F.,(4,2,2,
2,2,2,2,2,2,2,4),(-0.17876393636429,-0.178279109643944,-0.157081929142902,
-0.136547654157445,-0.114535014767487,-0.0983347050072544,-0.0847433634153561,
-0.0709327535553801,-0.0541499330631514,-0.0308889104943535,-0.00278496917063749),
 .UNSPECIFIED.);
#2318=B_SPLINE_CURVE_WITH_KNOTS('',3,(#44854,#44855,#44856,#44857,#44858,
#44859,#44860,#44861,#44862,#44863,#44864,#44865,#44866,#44867,#44868,#44869,
#44870,#44871,#44872,#44873,#44874,#44875,#44876,#44877,#44878,#44879),
 .UNSPECIFIED.,.F.,.F.,(4,2,2,2,2,2,2,2,2,2,2,2,4),(-0.149765769623311,
-0.149414895756082,-0.132671826505775,-0.114429386512108,-0.0992899556088679,
-0.0866980728560365,-0.074707447877953,-0.0627168228998696,-0.0501249401470389,
-0.0349855092437845,-0.0167430692500659,0.,0.000350873867280196),
 .UNSPECIFIED.);
#2319=B_SPLINE_CURVE_WITH_KNOTS('',3,(#44880,#44881,#44882,#44883,#44884,
#44885,#44886,#44887,#44888,#44889,#44890,#44891,#44892,#44893,#44894,#44895,
#44896,#44897,#44898,#44899,#44900,#44901,#44902,#44903,#44904,#44905),
 .UNSPECIFIED.,.F.,.F.,(4,2,2,2,2,2,2,2,2,2,2,2,4),(-0.149765769607808,
-0.149414895740571,-0.132671826492017,-0.114429386500231,-0.0992899555985793,
-0.086698072847082,-0.0747074478702766,-0.0627168228934715,-0.0501249401419783,
-0.0349855092403365,-0.0167430692485508,0.,0.000350873867236666),
 .UNSPECIFIED.);
#2320=B_SPLINE_CURVE_WITH_KNOTS('',3,(#44918,#44919,#44920,#44921,#44922,
#44923,#44924,#44925),.UNSPECIFIED.,.F.,.F.,(4,2,2,4),(-0.12173108833567,
-0.113308899129218,-0.097236345543046,-0.0881725331804662),
 .UNSPECIFIED.);
#2321=B_SPLINE_CURVE_WITH_KNOTS('',3,(#44927,#44928,#44929,#44930,#44931,
#44932,#44933,#44934,#44935,#44936),.UNSPECIFIED.,.F.,.F.,(4,2,2,2,4),(-0.177908635507065,
-0.177425299894269,-0.155806602995727,-0.134924086342148,-0.12173108833567),
 .UNSPECIFIED.);
#2322=B_SPLINE_CURVE_WITH_KNOTS('',3,(#44939,#44940,#44941,#44942,#44943,
#44944,#44945,#44946,#44947,#44948,#44949,#44950,#44951,#44952),
 .UNSPECIFIED.,.F.,.F.,(4,2,2,2,2,2,4),(-0.0881725331804662,-0.0836000761729691,
-0.069663721232867,-0.0537475177849022,-0.0307021203616524,0.,0.000380437960906122),
 .UNSPECIFIED.);
#2323=B_SPLINE_CURVE_WITH_KNOTS('',3,(#44956,#44957,#44958,#44959,#44960,
#44961,#44962,#44963,#44964,#44965,#44966,#44967,#44968,#44969,#44970,#44971,
#44972,#44973,#44974,#44975,#44976,#44977,#44978,#44979,#44980,#44981),
 .UNSPECIFIED.,.F.,.F.,(4,2,2,2,2,2,2,2,2,2,2,2,4),(-0.149766416121483,
-0.149416311689899,-0.132681110939406,-0.11446620080775,-0.0993072249168199,
-0.0867023299576758,-0.074708155848574,-0.0627139817394723,-0.0501090867803249,
-0.0349501108893815,-0.0167352007577163,0.,0.000350104430293171),
 .UNSPECIFIED.);
#2324=B_SPLINE_CURVE_WITH_KNOTS('',3,(#44982,#44983,#44984,#44985,#44986,
#44987,#44988,#44989,#44990,#44991,#44992,#44993,#44994,#44995,#44996,#44997,
#44998,#44999,#45000,#45001,#45002,#45003,#45004,#45005,#45006,#45007),
 .UNSPECIFIED.,.F.,.F.,(4,2,2,2,2,2,2,2,2,2,2,2,4),(-0.149766416599849,
-0.149416312168387,-0.132681111357522,-0.114466201167421,-0.0993072252278703,
-0.0867023302283183,-0.0747081560807638,-0.0627139819332097,-0.0501090869336602,
-0.0349501109941116,-0.0167352008040167,0.,0.000350104432701244),
 .UNSPECIFIED.);
#2325=B_SPLINE_CURVE_WITH_KNOTS('',3,(#46286,#46287,#46288,#46289,#46290,
#46291,#46292,#46293,#46294,#46295,#46296,#46297,#46298,#46299,#46300,#46301,
#46302,#46303,#46304,#46305,#46306,#46307,#46308,#46309,#46310,#46311,#46312,
#46313,#46314,#46315,#46316,#46317,#46318,#46319,#46320,#46321,#46322,#46323,
#46324,#46325,#46326,#46327,#46328,#46329,#46330,#46331,#46332,#46333,#46334,
#46335,#46336,#46337,#46338,#46339,#46340,#46341,#46342,#46343,#46344,#46345,
#46346,#46347,#46348,#46349,#46350,#46351,#46352,#46353,#46354,#46355,#46356,
#46357,#46358,#46359,#46360,#46361,#46362,#46363,#46364,#46365,#46366,#46367,
#46368,#46369,#46370,#46371,#46372,#46373,#46374,#46375,#46376,#46377,#46378,
#46379,#46380,#46381,#46382,#46383,#46384,#46385,#46386,#46387,#46388,#46389,
#46390,#46391,#46392,#46393,#46394,#46395,#46396,#46397,#46398,#46399,#46400,
#46401,#46402,#46403,#46404,#46405,#46406,#46407,#46408,#46409,#46410,#46411,
#46412),.UNSPECIFIED.,.F.,.F.,(4,1,1,1,1,1,1,1,1,1,1,1,1,1,1,1,1,1,1,1,
1,1,1,1,1,1,1,1,1,1,1,1,1,1,1,1,1,1,1,1,1,1,1,1,1,1,1,1,1,1,1,1,1,1,1,1,
1,1,1,1,1,1,1,1,1,1,1,1,1,1,1,1,1,1,1,1,1,1,1,1,1,1,1,1,1,1,1,1,1,1,1,1,
1,1,1,1,1,1,1,1,1,1,1,1,1,1,1,1,1,1,1,1,1,1,1,1,1,1,1,1,1,1,1,1,4),(0.00137832727077589,
0.00446428571428571,0.00892857142857143,0.0178571428571429,0.0267857142857143,
0.0357142857142857,0.0446428571428571,0.0535714285714286,0.0625,0.0714285714285714,
0.0803571428571428,0.0892857142857143,0.0982142857142857,0.107142857142857,
0.116071428571429,0.125,0.129464285714286,0.133928571428571,0.138392857142857,
0.142857142857143,0.151785714285714,0.160714285714286,0.169642857142857,
0.178571428571429,0.1875,0.196428571428571,0.205357142857143,0.214285714285714,
0.223214285714286,0.232142857142857,0.241071428571429,0.25,0.258928571428571,
0.267857142857143,0.276785714285714,0.285714285714286,0.294642857142857,
0.303571428571429,0.3125,0.321428571428571,0.330357142857143,0.339285714285714,
0.348214285714286,0.357142857142857,0.366071428571428,0.375,0.383928571428571,
0.392857142857143,0.401785714285714,0.410714285714286,0.419642857142857,
0.428571428571429,0.4375,0.446428571428571,0.455357142857143,0.464285714285714,
0.473214285714286,0.482142857142857,0.494047619047619,0.5,0.504464285714286,
0.508928571428571,0.517857142857143,0.526785714285714,0.535714285714286,
0.544642857142857,0.553571428571429,0.5625,0.571428571428571,0.580357142857143,
0.589285714285714,0.598214285714286,0.607142857142857,0.616071428571429,
0.625,0.633928571428571,0.642857142857143,0.647321428571428,0.651785714285714,
0.660714285714286,0.666666666666667,0.678571428571428,0.6796875,0.680803571428571,
0.6875,0.696428571428571,0.705357142857143,0.714285714285714,0.726190476190476,
0.735119047619047,0.738095238095238,0.75,0.761904761904762,0.76984126984127,
0.777777777777778,0.785714285714286,0.793650793650794,0.801587301587302,
0.809523809523809,0.81547619047619,0.821428571428571,0.827380952380952,
0.830357142857143,0.833333333333333,0.839285714285714,0.845238095238095,
0.851190476190476,0.857142857142857,0.866071428571429,0.875,0.883928571428571,
0.892857142857143,0.901785714285714,0.910714285714286,0.919642857142857,
0.928571428571429,0.9375,0.946428571428571,0.955357142857143,0.964285714285714,
0.973214285714286,0.982142857142857,0.991071428571429,0.995535714285714,
0.999890109193126),.UNSPECIFIED.);
#2326=B_SPLINE_CURVE_WITH_KNOTS('',3,(#46419,#46420,#46421,#46422,#46423,
#46424,#46425,#46426,#46427,#46428),.UNSPECIFIED.,.F.,.F.,(4,3,3,4),(-4.0927490401942,
-3.99664925518937,-2.99748694139203,-2.06120159751576),.UNSPECIFIED.);
#2327=B_SPLINE_CURVE_WITH_KNOTS('',3,(#46431,#46432,#46433,#46434,#46435,
#46436,#46437),.UNSPECIFIED.,.F.,.F.,(4,3,4),(0.,0.999162313797346,1.11004521091126),
 .UNSPECIFIED.);
#2328=B_SPLINE_CURVE_WITH_KNOTS('',3,(#46442,#46443,#46444,#46445,#46446,
#46447,#46448,#46449,#46450,#46451,#46452,#46453,#46454,#46455,#46456,#46457,
#46458,#46459,#46460,#46461,#46462,#46463),.UNSPECIFIED.,.F.,.F.,(4,3,3,
3,3,3,3,4),(-10.3759343473738,-9.99162313797342,-8.99246082417608,-7.99329851037874,
-6.9941361965814,-5.99497388278405,-4.99581156898671,-4.0927490401942),
 .UNSPECIFIED.);
#2329=B_SPLINE_CURVE_WITH_KNOTS('',3,(#46464,#46465,#46466,#46467,#46468,
#46469,#46470,#46471,#46472,#46473,#46474,#46475,#46476,#46477,#46478,#46479,
#46480,#46481,#46482,#46483,#46484,#46485),.UNSPECIFIED.,.F.,.F.,(4,3,3,
3,3,3,3,4),(1.11004521091126,1.99832462759469,2.99748694139203,3.99664925518937,
4.99581156898671,5.99497388278405,6.9941361965814,7.39323051809085),
 .UNSPECIFIED.);
#2330=B_SPLINE_CURVE_WITH_KNOTS('',3,(#46490,#46491,#46492,#46493,#46494,
#46495,#46496,#46497,#46498,#46499,#46500,#46501,#46502,#46503,#46504,#46505,
#46506,#46507,#46508,#46509,#46510,#46511),.UNSPECIFIED.,.F.,.F.,(4,3,3,
3,3,3,3,4),(-16.6591196545534,-15.9865970207575,-14.9874347069601,-13.9882723931628,
-12.9891100793654,-11.9899477655681,-10.9907854517708,-10.3759343473738),
 .UNSPECIFIED.);
#2331=B_SPLINE_CURVE_WITH_KNOTS('',3,(#46512,#46513,#46514,#46515,#46516,
#46517,#46518,#46519,#46520,#46521,#46522,#46523,#46524,#46525,#46526,#46527,
#46528,#46529,#46530,#46531,#46532,#46533),.UNSPECIFIED.,.F.,.F.,(4,3,3,
3,3,3,3,4),(7.39323051809085,7.99329851037874,8.99246082417608,9.99162313797342,
10.9907854517708,11.9899477655681,12.9891100793654,13.6764158252704),
 .UNSPECIFIED.);
#2332=B_SPLINE_CURVE_WITH_KNOTS('',3,(#46538,#46539,#46540,#46541,#46542,
#46543,#46544,#46545,#46546,#46547,#46548,#46549,#46550,#46551,#46552,#46553,
#46554,#46555,#46556,#46557,#46558,#46559),.UNSPECIFIED.,.F.,.F.,(4,3,3,
3,3,3,3,4),(-22.942304961733,-21.9815709035415,-20.9824085897442,-19.9832462759468,
-18.9840839621495,-17.9849216483522,-16.9857593345548,-16.6591196545534),
 .UNSPECIFIED.);
#2333=B_SPLINE_CURVE_WITH_KNOTS('',3,(#46560,#46561,#46562,#46563,#46564,
#46565,#46566,#46567,#46568,#46569,#46570,#46571,#46572,#46573,#46574,#46575,
#46576,#46577,#46578,#46579,#46580,#46581),.UNSPECIFIED.,.F.,.F.,(4,3,3,
3,3,3,3,4),(13.6764158252704,13.9882723931628,14.9874347069601,15.9865970207575,
16.9857593345548,17.9849216483522,18.9840839621495,19.95960113245),
 .UNSPECIFIED.);
#2334=B_SPLINE_CURVE_WITH_KNOTS('',3,(#46586,#46587,#46588,#46589,#46590,
#46591,#46592,#46593,#46594,#46595,#46596,#46597,#46598,#46599,#46600,#46601,
#46602,#46603,#46604,#46605,#46606,#46607,#46608,#46609,#46610),
 .UNSPECIFIED.,.F.,.F.,(4,3,3,3,3,3,3,3,4),(-29.2254902689126,-28.9757071001229,
-27.9765447863256,-26.9773824725282,-25.9782201587309,-24.9790578449336,
-23.9798955311362,-22.9807332173389,-22.942304961733),.UNSPECIFIED.);
#2335=B_SPLINE_CURVE_WITH_KNOTS('',3,(#46611,#46612,#46613,#46614,#46615,
#46616,#46617,#46618,#46619,#46620,#46621,#46622,#46623,#46624,#46625,#46626,
#46627,#46628,#46629,#46630,#46631,#46632,#46633,#46634,#46635),
 .UNSPECIFIED.,.F.,.F.,(4,3,3,3,3,3,3,3,4),(19.95960113245,19.9832462759468,
20.9824085897442,21.9815709035415,22.9807332173389,23.9798955311362,24.9790578449335,
25.9782201587309,26.2427864396296),.UNSPECIFIED.);
#2336=B_SPLINE_CURVE_WITH_KNOTS('',3,(#46640,#46641,#46642,#46643,#46644,
#46645,#46646,#46647,#46648,#46649,#46650,#46651,#46652,#46653,#46654,#46655,
#46656,#46657,#46658,#46659,#46660,#46661),.UNSPECIFIED.,.F.,.F.,(4,3,3,
3,3,3,3,4),(-35.5086755760921,-34.970680982907,-33.9715186691096,-32.9723563553123,
-31.9731940415149,-30.9740317277176,-29.9748694139203,-29.2254902689126),
 .UNSPECIFIED.);
#2337=B_SPLINE_CURVE_WITH_KNOTS('',3,(#46662,#46663,#46664,#46665,#46666,
#46667,#46668,#46669,#46670,#46671,#46672,#46673,#46674,#46675,#46676,#46677,
#46678,#46679,#46680,#46681,#46682,#46683),.UNSPECIFIED.,.F.,.F.,(4,3,3,
3,3,3,3,4),(26.2427864396296,26.9773824725282,27.9765447863256,28.9757071001229,
29.9748694139203,30.9740317277176,31.9731940415149,32.5259717468092),
 .UNSPECIFIED.);
#2338=B_SPLINE_CURVE_WITH_KNOTS('',3,(#46688,#46689,#46690,#46691,#46692,
#46693,#46694,#46695,#46696,#46697,#46698,#46699,#46700,#46701,#46702,#46703,
#46704,#46705,#46706,#46707,#46708,#46709),.UNSPECIFIED.,.F.,.F.,(4,3,3,
3,3,3,3,4),(-41.7918608832717,-40.965654865691,-39.9664925518937,-38.9673302380963,
-37.968167924299,-36.9690056105017,-35.9698432967043,-35.5086755760921),
 .UNSPECIFIED.);
#2339=B_SPLINE_CURVE_WITH_KNOTS('',3,(#46710,#46711,#46712,#46713,#46714,
#46715,#46716,#46717,#46718,#46719,#46720,#46721,#46722,#46723,#46724,#46725,
#46726,#46727,#46728,#46729,#46730,#46731),.UNSPECIFIED.,.F.,.F.,(4,3,3,
3,3,3,3,4),(32.5259717468092,32.9723563553123,33.9715186691096,34.970680982907,
35.9698432967043,36.9690056105017,37.968167924299,38.8091570539888),
 .UNSPECIFIED.);
#2340=B_SPLINE_CURVE_WITH_KNOTS('',3,(#46736,#46737,#46738,#46739,#46740,
#46741,#46742,#46743,#46744,#46745,#46746,#46747,#46748,#46749,#46750,#46751,
#46752,#46753,#46754,#46755,#46756,#46757,#46758,#46759,#46760),
 .UNSPECIFIED.,.F.,.F.,(4,3,3,3,3,3,3,3,4),(-48.0750461904513,-47.9597910622724,
-46.9606287484751,-45.9614664346777,-44.9623041208804,-43.9631418070831,
-42.9639794932857,-41.9648171794884,-41.7918608832717),.UNSPECIFIED.);
#2341=B_SPLINE_CURVE_WITH_KNOTS('',3,(#46761,#46762,#46763,#46764,#46765,
#46766,#46767,#46768,#46769,#46770,#46771,#46772,#46773,#46774,#46775,#46776,
#46777,#46778,#46779,#46780,#46781,#46782,#46783,#46784,#46785),
 .UNSPECIFIED.,.F.,.F.,(4,3,3,3,3,3,3,3,4),(38.8091570539888,38.9673302380963,
39.9664925518937,40.965654865691,41.9648171794884,42.9639794932857,43.963141807083,
44.9623041208804,45.0923423611684),.UNSPECIFIED.);
#2342=B_SPLINE_CURVE_WITH_KNOTS('',3,(#46790,#46791,#46792,#46793,#46794,
#46795,#46796,#46797,#46798,#46799,#46800,#46801,#46802,#46803,#46804,#46805,
#46806,#46807,#46808,#46809,#46810,#46811),.UNSPECIFIED.,.F.,.F.,(4,3,3,
3,3,3,3,4),(-54.3582314976309,-53.9547649450565,-52.9556026312591,-51.9564403174618,
-50.9572780036644,-49.9581156898671,-48.9589533760698,-48.0750461904513),
 .UNSPECIFIED.);
#2343=B_SPLINE_CURVE_WITH_KNOTS('',3,(#46812,#46813,#46814,#46815,#46816,
#46817,#46818,#46819,#46820,#46821,#46822,#46823,#46824,#46825,#46826,#46827,
#46828,#46829,#46830,#46831,#46832,#46833),.UNSPECIFIED.,.F.,.F.,(4,3,3,
3,3,3,3,4),(45.0923423611684,45.9614664346777,46.9606287484751,47.9597910622724,
48.9589533760698,49.9581156898671,50.9572780036644,51.375527668348),
 .UNSPECIFIED.);
#2344=B_SPLINE_CURVE_WITH_KNOTS('',3,(#46838,#46839,#46840,#46841,#46842,
#46843,#46844,#46845,#46846,#46847,#46848,#46849,#46850,#46851,#46852,#46853,
#46854,#46855,#46856,#46857,#46858,#46859),.UNSPECIFIED.,.F.,.F.,(4,3,3,
3,3,3,3,4),(-60.6414168048105,-59.9497388278405,-58.9505765140432,-57.9514142002458,
-56.9522518864485,-55.9530895726512,-54.9539272588538,-54.3582314976309),
 .UNSPECIFIED.);
#2345=B_SPLINE_CURVE_WITH_KNOTS('',3,(#46860,#46861,#46862,#46863,#46864,
#46865,#46866,#46867,#46868,#46869,#46870,#46871,#46872,#46873,#46874,#46875,
#46876,#46877,#46878,#46879,#46880,#46881),.UNSPECIFIED.,.F.,.F.,(4,3,3,
3,3,3,3,4),(51.375527668348,51.9564403174618,52.9556026312591,53.9547649450565,
54.9539272588538,55.9530895726512,56.9522518864485,57.6587129755276),
 .UNSPECIFIED.);
#2346=B_SPLINE_CURVE_WITH_KNOTS('',3,(#46887,#46888,#46889,#46890,#46891),
 .UNSPECIFIED.,.F.,.F.,(4,1,4),(72.2566310325653,72.5641153693926,73.5004007132688),
 .UNSPECIFIED.);
#2347=B_SPLINE_CURVE_WITH_KNOTS('',3,(#46894,#46895,#46896,#46897),
 .UNSPECIFIED.,.F.,.F.,(4,4),(72.2566310325652,72.2611208328879),
 .UNSPECIFIED.);
#2348=B_SPLINE_CURVE_WITH_KNOTS('',3,(#46902,#46903,#46904,#46905,#46906,
#46907,#46908,#46909,#46910,#46911),.UNSPECIFIED.,.F.,.F.,(4,1,1,1,1,1,
1,4),(65.9734457253856,66.5691414866085,67.5683038004059,68.5674661142032,
69.5666284280005,70.5657907417979,71.5649530555952,72.2566310325653),
 .UNSPECIFIED.);
#2349=B_SPLINE_CURVE_WITH_KNOTS('',3,(#46912,#46913,#46914,#46915,#46916,
#46917,#46918,#46919,#46920,#46921),.UNSPECIFIED.,.F.,.F.,(4,1,1,1,1,1,
1,4),(65.9734457253856,66.2661469501039,67.2653092639012,68.2644715776985,
69.2636338914959,70.2627962052932,71.2619585190906,72.2566310325652),
 .UNSPECIFIED.);
#2350=B_SPLINE_CURVE_WITH_KNOTS('',3,(#46926,#46927,#46928,#46929,#46930,
#46931,#46932,#46933,#46934,#46935),.UNSPECIFIED.,.F.,.F.,(4,1,1,1,1,1,
1,4),(59.6902604182061,60.5741676038245,61.5733299176218,62.5724922314191,
63.5716545452165,64.5708168590138,65.5699791728112,65.9734457253856),
 .UNSPECIFIED.);
#2351=B_SPLINE_CURVE_WITH_KNOTS('',3,(#46936,#46937,#46938,#46939,#46940,
#46941,#46942,#46943,#46944,#46945),.UNSPECIFIED.,.F.,.F.,(4,1,1,1,1,1,
1,4),(59.6902604182061,60.2711730673198,61.2703353811171,62.2694976949145,
63.2686600087118,64.2678223225092,65.2669846363065,65.9734457253856),
 .UNSPECIFIED.);
#2352=B_SPLINE_CURVE_WITH_KNOTS('',3,(#46950,#46951,#46952,#46953,#46954,
#46955,#46956,#46957,#46958,#46959,#46960),.UNSPECIFIED.,.F.,.F.,(4,1,1,
1,1,1,1,1,4),(53.4070751110265,53.5800314072431,54.5791937210404,55.5783560348378,
56.5775183486351,57.5766806624324,58.5758429762298,59.5750052900271,59.6902604182061),
 .UNSPECIFIED.);
#2353=B_SPLINE_CURVE_WITH_KNOTS('',3,(#46961,#46962,#46963,#46964,#46965,
#46966,#46967,#46968,#46969,#46970),.UNSPECIFIED.,.F.,.F.,(4,1,1,1,1,1,
1,4),(53.4070751110265,54.2761991845358,55.2753614983331,56.2745238121304,
57.2736861259278,58.2728484397251,59.2720107535225,59.6902604182061),
 .UNSPECIFIED.);
#2354=B_SPLINE_CURVE_WITH_KNOTS('',3,(#46975,#46976,#46977,#46978,#46979,
#46980,#46981,#46982,#46983,#46984),.UNSPECIFIED.,.F.,.F.,(4,1,1,1,1,1,
1,4),(47.1238898038469,47.585057524459,48.5842198382564,49.5833821520537,
50.582544465851,51.5817067796484,52.5808690934457,53.4070751110265),
 .UNSPECIFIED.);
#2355=B_SPLINE_CURVE_WITH_KNOTS('',3,(#46985,#46986,#46987,#46988,#46989,
#46990,#46991,#46992,#46993,#46994,#46995),.UNSPECIFIED.,.F.,.F.,(4,1,1,
1,1,1,1,1,4),(47.1238898038469,47.2820629879544,48.2812253017517,49.280387615549,
50.2795499293464,51.2787122431437,52.2778745569411,53.2770368707384,53.4070751110265),
 .UNSPECIFIED.);
#2356=B_SPLINE_CURVE_WITH_KNOTS('',3,(#47000,#47001,#47002,#47003,#47004,
#47005,#47006,#47007,#47008,#47009),.UNSPECIFIED.,.F.,.F.,(4,1,1,1,1,1,
1,4),(40.8407044966673,41.590083641675,42.5892459554723,43.5884082692696,
44.587570583067,45.5867328968643,46.5858952106617,47.1238898038469),
 .UNSPECIFIED.);
#2357=B_SPLINE_CURVE_WITH_KNOTS('',3,(#47010,#47011,#47012,#47013,#47014,
#47015,#47016,#47017,#47018,#47019),.UNSPECIFIED.,.F.,.F.,(4,1,1,1,1,1,
1,4),(40.8407044966673,41.2870891051703,42.2862514189677,43.285413732765,
44.2845760465623,45.2837383603597,46.282900674157,47.1238898038469),
 .UNSPECIFIED.);
#2358=B_SPLINE_CURVE_WITH_KNOTS('',3,(#47024,#47025,#47026,#47027,#47028,
#47029,#47030,#47031,#47032,#47033,#47034),.UNSPECIFIED.,.F.,.F.,(4,1,1,
1,1,1,1,1,4),(34.5575191894877,34.5959474450936,35.5951097588909,36.5942720726883,
37.5934343864856,38.5925967002829,39.5917590140803,40.5909213278776,40.8407044966673),
 .UNSPECIFIED.);
#2359=B_SPLINE_CURVE_WITH_KNOTS('',3,(#47035,#47036,#47037,#47038,#47039,
#47040,#47041,#47042,#47043,#47044),.UNSPECIFIED.,.F.,.F.,(4,1,1,1,1,1,
1,4),(34.5575191894877,35.2921152223863,36.2912775361836,37.2904398499809,
38.2896021637783,39.2887644775756,40.287926791373,40.8407044966673),
 .UNSPECIFIED.);
#2360=B_SPLINE_CURVE_WITH_KNOTS('',3,(#47049,#47050,#47051,#47052,#47053,
#47054,#47055,#47056,#47057,#47058),.UNSPECIFIED.,.F.,.F.,(4,1,1,1,1,1,
1,4),(28.2743338823081,28.6009735623095,29.6001358761069,30.5992981899042,
31.5984605037015,32.5976228174989,33.5967851312962,34.5575191894877),
 .UNSPECIFIED.);
#2361=B_SPLINE_CURVE_WITH_KNOTS('',3,(#47059,#47060,#47061,#47062,#47063,
#47064,#47065,#47066,#47067,#47068,#47069),.UNSPECIFIED.,.F.,.F.,(4,1,1,
1,1,1,1,1,4),(28.2743338823081,28.2979790258049,29.2971413396022,30.2963036533995,
31.2954659671969,32.2946282809942,33.2937905947916,34.2929529085889,34.5575191894877),
 .UNSPECIFIED.);
#2362=B_SPLINE_CURVE_WITH_KNOTS('',3,(#47074,#47075,#47076,#47077,#47078,
#47079,#47080,#47081,#47082,#47083),.UNSPECIFIED.,.F.,.F.,(4,1,1,1,1,1,
1,4),(21.9911485751285,22.6059996795255,23.6051619933228,24.6043243071202,
25.6034866209175,26.6026489347148,27.6018112485122,28.2743338823081),
 .UNSPECIFIED.);
#2363=B_SPLINE_CURVE_WITH_KNOTS('',3,(#47084,#47085,#47086,#47087,#47088,
#47089,#47090,#47091,#47092,#47093),.UNSPECIFIED.,.F.,.F.,(4,1,1,1,1,1,
1,4),(21.9911485751285,22.3030051430208,23.3021674568182,24.3013297706155,
25.3004920844128,26.2996543982102,27.2988167120075,28.2743338823081),
 .UNSPECIFIED.);
#2364=B_SPLINE_CURVE_WITH_KNOTS('',3,(#47098,#47099,#47100,#47101,#47102,
#47103,#47104,#47105,#47106,#47107),.UNSPECIFIED.,.F.,.F.,(4,1,1,1,1,1,
1,4),(15.7079632679489,16.6110257967414,17.6101881105388,18.6093504243361,
19.6085127381334,20.6076750519308,21.6068373657281,21.9911485751285),
 .UNSPECIFIED.);
#2365=B_SPLINE_CURVE_WITH_KNOTS('',3,(#47108,#47109,#47110,#47111,#47112,
#47113,#47114,#47115,#47116,#47117),.UNSPECIFIED.,.F.,.F.,(4,1,1,1,1,1,
1,4),(15.7079632679489,16.3080312602368,17.3071935740341,18.3063558878314,
19.3055182016288,20.3046805154261,21.3038428292235,21.9911485751285),
 .UNSPECIFIED.);
#2366=B_SPLINE_CURVE_WITH_KNOTS('',3,(#47120,#47121,#47122,#47123,#47124,
#47125,#47126,#47127,#47128,#47129,#47130,#47131,#47132,#47133,#47134,#47135,
#47136,#47137,#47138,#47139,#47140,#47141,#47142,#47143,#47144,#47145,#47146,
#47147,#47148,#47149,#47150,#47151,#47152,#47153,#47154,#47155,#47156,#47157,
#47158,#47159,#47160,#47161,#47162,#47163,#47164,#47165,#47166,#47167,#47168,
#47169,#47170,#47171,#47172,#47173,#47174,#47175,#47176,#47177,#47178,#47179,
#47180,#47181,#47182,#47183,#47184,#47185,#47186,#47187,#47188,#47189,#47190,
#47191,#47192,#47193,#47194,#47195,#47196,#47197,#47198,#47199,#47200,#47201,
#47202,#47203,#47204,#47205,#47206,#47207,#47208,#47209,#47210,#47211,#47212,
#47213,#47214,#47215,#47216),.UNSPECIFIED.,.F.,.F.,(4,3,3,3,3,3,3,3,3,3,
3,3,3,3,3,3,3,3,3,3,3,3,3,3,3,3,3,3,3,3,3,3,4),(-0.744397949170578,-0.723859366608779,
-0.692778390163693,-0.673163388835089,-0.66062832497008,-0.654997428133838,
-0.623000635306235,-0.592492852006209,-0.579145696812448,-0.572539965631915,
-0.567831580001411,-0.534463688691448,-0.50057067124518,-0.46675792585302,
-0.444803036616271,-0.438632777591669,-0.432866104431837,-0.397950947955525,
-0.378938368906026,-0.345225723678728,-0.310871405360981,-0.300047867503053,
-0.295192728302996,-0.260846341462991,-0.225369180435003,-0.189533834845717,
-0.165842105490003,-0.154268999879935,-0.147059086804718,-0.110294315103539,
-0.0734873168420825,-0.0367436584210412,0.),.UNSPECIFIED.);
#2367=B_SPLINE_CURVE_WITH_KNOTS('',3,(#47221,#47222,#47223,#47224,#47225,
#47226,#47227,#47228,#47229,#47230,#47231,#47232,#47233,#47234,#47235,#47236,
#47237,#47238,#47239,#47240,#47241,#47242,#47243,#47244,#47245,#47246,#47247,
#47248,#47249,#47250,#47251,#47252,#47253,#47254,#47255,#47256,#47257,#47258,
#47259,#47260,#47261,#47262,#47263,#47264,#47265,#47266,#47267,#47268,#47269,
#47270,#47271,#47272,#47273,#47274,#47275,#47276,#47277,#47278,#47279,#47280,
#47281,#47282,#47283,#47284,#47285,#47286,#47287,#47288,#47289,#47290,#47291,
#47292,#47293,#47294,#47295,#47296,#47297,#47298,#47299,#47300,#47301,#47302,
#47303,#47304,#47305,#47306,#47307,#47308,#47309,#47310,#47311,#47312,#47313,
#47314,#47315,#47316,#47317),.UNSPECIFIED.,.F.,.F.,(4,3,3,3,3,3,3,3,3,3,
3,3,3,3,3,3,3,3,3,3,3,3,3,3,3,3,3,3,3,3,3,3,4),(-0.741270768406328,-0.716584367599815,
-0.680056248148676,-0.658907114297353,-0.642813303176804,-0.636134709402922,
-0.599326634043495,-0.567119568103997,-0.553028976755466,-0.544366227927849,
-0.537678034880734,-0.502276348317679,-0.467136809341096,-0.43303532712436,
-0.410194021975148,-0.39912856359863,-0.394448100777585,-0.360831295807122,
-0.341670106527509,-0.307405657582616,-0.272989575876299,-0.262610092909626,
-0.257322277143721,-0.223891952452371,-0.190429464967423,-0.15737798688834,
-0.137705738527298,-0.128679290433546,-0.124522260753379,-0.0923095570632588,
-0.0605443501164106,-0.0297602312950581,0.),.UNSPECIFIED.);
#2368=B_SPLINE_CURVE_WITH_KNOTS('',3,(#47586,#47587,#47588,#47589,#47590,
#47591,#47592,#47593,#47594,#47595,#47596,#47597,#47598,#47599,#47600,#47601),
 .UNSPECIFIED.,.F.,.F.,(4,3,3,3,3,4),(57.6587129755276,57.9514142002458,
58.9505765140432,59.9497388278405,60.9489011416379,61.8851864855141),
 .UNSPECIFIED.);
#2369=B_SPLINE_CURVE_WITH_KNOTS('',3,(#47603,#47604,#47605,#47606,#47607,
#47608,#47609,#47610,#47611,#47612,#47613,#47614,#47615,#47616,#47617,#47618,
#47619,#47620,#47621,#47622,#47623,#47624,#47625,#47626,#47627,#47628,#47629,
#47630,#47631,#47632,#47633,#47634,#47635,#47636,#47637,#47638,#47639,#47640,
#47641,#47642,#47643,#47644,#47645,#47646,#47647,#47648,#47649,#47650,#47651,
#47652,#47653,#47654,#47655,#47656,#47657,#47658,#47659,#47660,#47661,#47662,
#47663,#47664,#47665,#47666,#47667,#47668,#47669,#47670,#47671,#47672,#47673,
#47674,#47675,#47676,#47677,#47678,#47679,#47680,#47681,#47682,#47683,#47684,
#47685,#47686,#47687,#47688,#47689,#47690,#47691,#47692,#47693,#47694,#47695,
#47696,#47697,#47698,#47699),.UNSPECIFIED.,.F.,.F.,(4,3,3,3,3,3,3,3,3,3,
3,3,3,3,3,3,3,3,3,3,3,3,3,3,3,3,3,3,3,3,3,3,4),(-0.744397949170611,-0.723859366608811,
-0.692778425140133,-0.673163421625501,-0.66062836032772,-0.654997464717496,
-0.623000702910192,-0.592492911159671,-0.579145752268819,-0.572540185113237,
-0.567831953655538,-0.53446408683659,-0.50057107660485,-0.466758326635226,
-0.444803337202926,-0.438637144898971,-0.432867617692046,-0.397952458797699,
-0.378938368906029,-0.345225738440821,-0.310871437714059,-0.300047912343567,
-0.295192811934132,-0.260846440789055,-0.225369298521846,-0.189533961517898,
-0.16584221632816,-0.154269162505787,-0.147059061291272,-0.110294295968454,
-0.0734872911176007,-0.0367436455588004,0.),.UNSPECIFIED.);
#2370=B_SPLINE_CURVE_WITH_KNOTS('',3,(#47700,#47701,#47702,#47703,#47704,
#47705,#47706,#47707,#47708),.UNSPECIFIED.,.F.,.F.,(4,1,1,1,1,1,4),(10.3759343473738,
11.3122196912501,12.3113820050474,13.3105443188447,14.3097066326421,15.3088689464394,
15.7079632679489),.UNSPECIFIED.);
#2371=B_SPLINE_CURVE_WITH_KNOTS('',3,(#47714,#47715,#47716,#47717,#47718,
#47719,#47720,#47721,#47722,#47723,#47724,#47725,#47726,#47727,#47728,#47729,
#47730,#47731,#47732,#47733,#47734,#47735,#47736,#47737,#47738,#47739,#47740,
#47741,#47742,#47743,#47744,#47745,#47746,#47747,#47748,#47749,#47750,#47751,
#47752,#47753,#47754,#47755,#47756,#47757,#47758,#47759,#47760,#47761,#47762,
#47763,#47764,#47765,#47766,#47767,#47768,#47769,#47770,#47771,#47772,#47773,
#47774,#47775,#47776,#47777,#47778,#47779,#47780,#47781,#47782,#47783,#47784,
#47785,#47786,#47787,#47788,#47789,#47790,#47791,#47792,#47793,#47794,#47795,
#47796,#47797,#47798,#47799,#47800,#47801,#47802,#47803,#47804,#47805,#47806,
#47807,#47808,#47809,#47810),.UNSPECIFIED.,.F.,.F.,(4,3,3,3,3,3,3,3,3,3,
3,3,3,3,3,3,3,3,3,3,3,3,3,3,3,3,3,3,3,3,3,3,4),(-0.741270768406356,-0.716584367599843,
-0.680056245830011,-0.658907112123604,-0.642813301702322,-0.636134706984057,
-0.599326631926989,-0.567119566252054,-0.55302897501927,-0.54436621135304,
-0.537678029406459,-0.502276340484753,-0.467136787004678,-0.433035266636814,
-0.410193976609488,-0.399128488173405,-0.394447934771061,-0.360831102765067,
-0.341670106527508,-0.307405637245107,-0.272989559930472,-0.262610069828679,
-0.257322284490531,-0.223891948269394,-0.190429473282791,-0.157378031219309,
-0.137705777316896,-0.128679430637047,-0.124522456571441,-0.0923097812005346,
-0.0605446165933425,-0.0297605544881402,0.),.UNSPECIFIED.);
#2372=B_SPLINE_CURVE_WITH_KNOTS('',3,(#47813,#47814,#47815,#47816,#47817,
#47818,#47819,#47820),.UNSPECIFIED.,.F.,.F.,(4,1,1,1,1,4),(11.6152142277547,
12.614376541552,13.6135388553494,14.6127011691467,15.6118634829441,15.7079632679489),
 .UNSPECIFIED.);
#2373=B_SPLINE_CURVE_WITH_KNOTS('',3,(#48089,#48090,#48091,#48092,#48093,
#48094,#48095,#48096,#48097,#48098,#48099,#48100,#48101),.UNSPECIFIED.,
 .F.,.F.,(4,3,3,3,4),(-63.9463880830299,-62.9472257692326,-61.9480634554352,
-60.9489011416379,-60.6414168048105),.UNSPECIFIED.);
#2374=B_SPLINE_CURVE_WITH_KNOTS('',3,(#49484,#49485,#49486,#49487,#49488,
#49489,#49490,#49491,#49492,#49493,#49494,#49495,#49496,#49497,#49498,#49499,
#49500,#49501,#49502,#49503,#49504,#49505,#49506,#49507,#49508,#49509,#49510,
#49511,#49512,#49513,#49514,#49515,#49516,#49517,#49518,#49519,#49520,#49521,
#49522,#49523,#49524,#49525,#49526,#49527,#49528,#49529,#49530,#49531,#49532,
#49533,#49534,#49535,#49536,#49537,#49538,#49539,#49540),.UNSPECIFIED.,
 .F.,.F.,(4,1,1,1,1,1,1,1,1,1,1,1,1,1,1,1,1,1,1,1,1,1,1,1,1,1,1,1,1,1,1,
1,1,1,1,1,1,1,1,1,1,1,1,1,1,1,1,1,1,1,1,1,1,1,4),(0.,0.00892857142857143,
0.0178571428571429,0.0357142857142857,0.0535714285714286,0.0714285714285714,
0.0892857142857143,0.107142857142857,0.125,0.142857142857143,0.166666666666667,
0.19047619047619,0.214285714285714,0.232142857142857,0.25,0.267857142857143,
0.285714285714286,0.303571428571429,0.321428571428571,0.339285714285714,
0.357142857142857,0.375,0.392857142857143,0.410714285714286,0.428571428571429,
0.452380952380952,0.476190476190476,0.5,0.523809523809524,0.547619047619048,
0.571428571428571,0.595238095238095,0.619047619047619,0.642857142857143,
0.666666666666667,0.682539682539682,0.698412698412698,0.714285714285714,
0.73015873015873,0.746031746031746,0.761904761904762,0.785714285714286,
0.809523809523809,0.833333333333333,0.857142857142857,0.866071428571429,
0.875,0.892857142857143,0.910714285714286,0.928571428571429,0.946428571428571,
0.964285714285714,0.982142857142857,0.991071428571429,1.),.UNSPECIFIED.);
#2375=B_SPLINE_CURVE_WITH_KNOTS('',3,(#49575,#49576,#49577,#49578,#49579,
#49580,#49581,#49582,#49583,#49584),.UNSPECIFIED.,.F.,.F.,(4,3,3,4),(-4.09254174883831,
-3.99058903474596,-2.99294177605947,-2.06514013327809),.UNSPECIFIED.);
#2376=B_SPLINE_CURVE_WITH_KNOTS('',3,(#49587,#49588,#49589,#49590,#49591,
#49592,#49593),.UNSPECIFIED.,.F.,.F.,(4,3,4),(0.,0.997647258686503,1.11419103803015),
 .UNSPECIFIED.);
#2377=B_SPLINE_CURVE_WITH_KNOTS('',3,(#49598,#49599,#49600,#49601,#49602,
#49603,#49604,#49605,#49606,#49607,#49608,#49609,#49610,#49611,#49612,#49613,
#49614,#49615,#49616,#49617,#49618,#49619),.UNSPECIFIED.,.F.,.F.,(4,3,3,
3,3,3,3,4),(-10.3757270560179,-9.97647258686489,-8.9788253281784,-7.98117806949191,
-6.98353081080542,-5.98588355211893,-4.98823629343245,-4.09254174883831),
 .UNSPECIFIED.);
#2378=B_SPLINE_CURVE_WITH_KNOTS('',3,(#49620,#49621,#49622,#49623,#49624,
#49625,#49626,#49627,#49628,#49629,#49630,#49631,#49632,#49633,#49634,#49635,
#49636,#49637,#49638,#49639,#49640,#49641),.UNSPECIFIED.,.F.,.F.,(4,3,3,
3,3,3,3,4),(1.11419103803015,1.99529451737299,2.99294177605948,3.99058903474597,
4.98823629343246,5.98588355211895,6.98353081080544,7.39737634520972),
 .UNSPECIFIED.);
#2379=B_SPLINE_CURVE_WITH_KNOTS('',3,(#49646,#49647,#49648,#49649,#49650,
#49651,#49652,#49653,#49654,#49655,#49656,#49657,#49658,#49659,#49660,#49661,
#49662,#49663,#49664,#49665,#49666,#49667),.UNSPECIFIED.,.F.,.F.,(4,3,3,
3,3,3,3,4),(-16.6589123631975,-15.9623561389838,-14.9647088802973,-13.9670616216108,
-12.9694143629244,-11.9717671042379,-10.9741198455514,-10.3757270560179),
 .UNSPECIFIED.);
#2380=B_SPLINE_CURVE_WITH_KNOTS('',3,(#49668,#49669,#49670,#49671,#49672,
#49673,#49674,#49675,#49676,#49677,#49678,#49679,#49680,#49681,#49682,#49683,
#49684,#49685,#49686,#49687,#49688,#49689),.UNSPECIFIED.,.F.,.F.,(4,3,3,
3,3,3,3,4),(7.39737634520972,7.98117806949192,8.97882532817841,9.97647258686489,
10.9741198455514,11.9717671042379,12.9694143629243,13.6805616523893),
 .UNSPECIFIED.);
#2381=B_SPLINE_CURVE_WITH_KNOTS('',3,(#49694,#49695,#49696,#49697,#49698,
#49699,#49700,#49701,#49702,#49703,#49704,#49705,#49706,#49707,#49708,#49709,
#49710,#49711,#49712,#49713,#49714,#49715),.UNSPECIFIED.,.F.,.F.,(4,3,3,
3,3,3,3,4),(-22.9420976703771,-21.9482396911028,-20.9505924324163,-19.9529451737298,
-18.9552979150433,-17.9576506563568,-16.9600033976703,-16.6589123631975),
 .UNSPECIFIED.);
#2382=B_SPLINE_CURVE_WITH_KNOTS('',3,(#49716,#49717,#49718,#49719,#49720,
#49721,#49722,#49723,#49724,#49725,#49726,#49727,#49728,#49729,#49730,#49731,
#49732,#49733,#49734,#49735,#49736,#49737,#49738,#49739,#49740),
 .UNSPECIFIED.,.F.,.F.,(4,3,3,3,3,3,3,3,4),(13.6805616523893,13.9670616216108,
14.9647088802973,15.9623561389838,16.9600033976703,17.9576506563568,18.9552979150433,
19.9529451737298,19.9637469595689),.UNSPECIFIED.);
#2383=B_SPLINE_CURVE_WITH_KNOTS('',3,(#49745,#49746,#49747,#49748,#49749,
#49750,#49751,#49752,#49753,#49754,#49755,#49756,#49757,#49758,#49759,#49760,
#49761,#49762,#49763,#49764,#49765,#49766,#49767,#49768,#49769),
 .UNSPECIFIED.,.F.,.F.,(4,3,3,3,3,3,3,3,4),(-29.2252829775566,-28.9317705019082,
-27.9341232432217,-26.9364759845352,-25.9388287258487,-24.9411814671622,
-23.9435342084757,-22.9458869497892,-22.9420976703771),.UNSPECIFIED.);
#2384=B_SPLINE_CURVE_WITH_KNOTS('',3,(#49770,#49771,#49772,#49773,#49774,
#49775,#49776,#49777,#49778,#49779,#49780,#49781,#49782,#49783,#49784,#49785,
#49786,#49787,#49788,#49789,#49790,#49791),.UNSPECIFIED.,.F.,.F.,(4,3,3,
3,3,3,3,4),(19.9637469595689,20.9505924324163,21.9482396911028,22.9458869497892,
23.9435342084757,24.9411814671622,25.9388287258487,26.2469322667485),
 .UNSPECIFIED.);
#2385=B_SPLINE_CURVE_WITH_KNOTS('',3,(#49796,#49797,#49798,#49799,#49800,
#49801,#49802,#49803,#49804,#49805,#49806,#49807,#49808,#49809,#49810,#49811,
#49812,#49813,#49814,#49815,#49816,#49817),.UNSPECIFIED.,.F.,.F.,(4,3,3,
3,3,3,3,4),(-35.5084682847363,-34.9176540540271,-33.9200067953406,-32.9223595366541,
-31.9247122779677,-30.9270650192812,-29.9294177605947,-29.2252829775566),
 .UNSPECIFIED.);
#2386=B_SPLINE_CURVE_WITH_KNOTS('',3,(#49818,#49819,#49820,#49821,#49822,
#49823,#49824,#49825,#49826,#49827,#49828,#49829,#49830,#49831,#49832,#49833,
#49834,#49835,#49836,#49837,#49838,#49839),.UNSPECIFIED.,.F.,.F.,(4,3,3,
3,3,3,3,4),(26.2469322667485,26.9364759845352,27.9341232432217,28.9317705019082,
29.9294177605947,30.9270650192812,31.9247122779677,32.5301175739281),
 .UNSPECIFIED.);
#2387=B_SPLINE_CURVE_WITH_KNOTS('',3,(#49844,#49845,#49846,#49847,#49848,
#49849,#49850,#49851,#49852,#49853,#49854,#49855,#49856,#49857,#49858,#49859,
#49860,#49861,#49862,#49863,#49864,#49865),.UNSPECIFIED.,.F.,.F.,(4,3,3,
3,3,3,3,4),(-41.7916535919158,-40.903537606146,-39.9058903474596,-38.9082430887731,
-37.9105958300866,-36.9129485714001,-35.9153013127136,-35.5084682847363),
 .UNSPECIFIED.);
#2388=B_SPLINE_CURVE_WITH_KNOTS('',3,(#49866,#49867,#49868,#49869,#49870,
#49871,#49872,#49873,#49874,#49875,#49876,#49877,#49878,#49879,#49880,#49881,
#49882,#49883,#49884,#49885,#49886,#49887),.UNSPECIFIED.,.F.,.F.,(4,3,3,
3,3,3,3,4),(32.5301175739281,32.9223595366541,33.9200067953406,34.9176540540271,
35.9153013127136,36.9129485714001,37.9105958300866,38.8133028811077),
 .UNSPECIFIED.);
#2389=B_SPLINE_CURVE_WITH_KNOTS('',3,(#49892,#49893,#49894,#49895,#49896,
#49897,#49898,#49899,#49900,#49901,#49902,#49903,#49904,#49905,#49906,#49907,
#49908,#49909,#49910,#49911,#49912,#49913,#49914,#49915,#49916),
 .UNSPECIFIED.,.F.,.F.,(4,3,3,3,3,3,3,3,4),(-48.0748388990954,-47.8870684169515,
-46.889421158265,-45.8917738995785,-44.894126640892,-43.8964793822055,-42.898832123519,
-41.9011848648325,-41.7916535919158),.UNSPECIFIED.);
#2390=B_SPLINE_CURVE_WITH_KNOTS('',3,(#49917,#49918,#49919,#49920,#49921,
#49922,#49923,#49924,#49925,#49926,#49927,#49928,#49929,#49930,#49931,#49932,
#49933,#49934,#49935,#49936,#49937,#49938,#49939,#49940,#49941),
 .UNSPECIFIED.,.F.,.F.,(4,3,3,3,3,3,3,3,4),(38.8133028811077,38.9082430887731,
39.9058903474596,40.9035376061461,41.9011848648326,42.898832123519,43.8964793822055,
44.894126640892,45.0964881882873),.UNSPECIFIED.);
#2391=B_SPLINE_CURVE_WITH_KNOTS('',3,(#49946,#49947,#49948,#49949,#49950,
#49951,#49952,#49953,#49954,#49955,#49956,#49957,#49958,#49959,#49960,#49961,
#49962,#49963,#49964,#49965,#49966,#49967),.UNSPECIFIED.,.F.,.F.,(4,3,3,
3,3,3,3,4),(-54.358024206275,-53.8729519690704,-52.8753047103839,-51.8776574516974,
-50.8800101930109,-49.8823629343244,-48.884715675638,-48.0748388990954),
 .UNSPECIFIED.);
#2392=B_SPLINE_CURVE_WITH_KNOTS('',3,(#49968,#49969,#49970,#49971,#49972,
#49973,#49974,#49975,#49976,#49977,#49978,#49979,#49980,#49981,#49982,#49983,
#49984,#49985,#49986,#49987,#49988,#49989),.UNSPECIFIED.,.F.,.F.,(4,3,3,
3,3,3,3,4),(45.0964881882873,45.8917738995785,46.889421158265,47.8870684169515,
48.884715675638,49.8823629343245,50.880010193011,51.3796734954669),
 .UNSPECIFIED.);
#2393=B_SPLINE_CURVE_WITH_KNOTS('',3,(#49994,#49995,#49996,#49997,#49998,
#49999,#50000,#50001,#50002,#50003,#50004,#50005,#50006,#50007,#50008,#50009,
#50010,#50011,#50012,#50013,#50014,#50015),.UNSPECIFIED.,.F.,.F.,(4,3,3,
3,3,3,3,4),(-60.6412095134546,-59.8588355211893,-58.8611882625028,-57.8635410038164,
-56.8658937451299,-55.8682464864434,-54.8705992277569,-54.358024206275),
 .UNSPECIFIED.);
#2394=B_SPLINE_CURVE_WITH_KNOTS('',3,(#50016,#50017,#50018,#50019,#50020,
#50021,#50022,#50023,#50024,#50025,#50026,#50027,#50028,#50029,#50030,#50031,
#50032,#50033,#50034,#50035,#50036,#50037),.UNSPECIFIED.,.F.,.F.,(4,3,3,
3,3,3,3,4),(51.3796734954669,51.8776574516975,52.8753047103839,53.8729519690704,
54.8705992277569,55.8682464864434,56.8658937451299,57.6628588026465),
 .UNSPECIFIED.);
#2395=B_SPLINE_CURVE_WITH_KNOTS('',3,(#50042,#50043,#50044,#50045,#50046,
#50047,#50048,#50049,#50050,#50051,#50052,#50053,#50054,#50055,#50056,#50057,
#50058,#50059,#50060,#50061,#50062,#50063,#50064,#50065,#50066),
 .UNSPECIFIED.,.F.,.F.,(4,3,3,3,3,3,3,3,4),(-66.9243948206342,-66.8423663319947,
-65.8447190733083,-64.8470718146218,-63.8494245559353,-62.8517772972488,
-61.8541300385623,-60.8564827798758,-60.6412095134546),.UNSPECIFIED.);
#2396=B_SPLINE_CURVE_WITH_KNOTS('',3,(#50067,#50068,#50069,#50070,#50071,
#50072,#50073,#50074,#50075,#50076,#50077,#50078,#50079,#50080,#50081,#50082,
#50083,#50084,#50085,#50086,#50087,#50088,#50089,#50090,#50091),
 .UNSPECIFIED.,.F.,.F.,(4,3,3,3,3,3,3,3,4),(57.6628588026465,57.8635410038164,
58.8611882625029,59.8588355211894,60.8564827798759,61.8541300385624,62.8517772972489,
63.8494245559354,63.946044109826),.UNSPECIFIED.);
#2397=B_SPLINE_CURVE_WITH_KNOTS('',3,(#50096,#50097,#50098,#50099,#50100,
#50101,#50102,#50103,#50104,#50105,#50106,#50107,#50108,#50109,#50110,#50111,
#50112,#50113,#50114,#50115,#50116,#50117),.UNSPECIFIED.,.F.,.F.,(4,3,3,
3,3,3,3,4),(-73.2075801278138,-72.8282498841137,-71.8306026254272,-70.8329553667407,
-69.8353081080542,-68.8376608493677,-67.8400135906812,-66.9243948206342),
 .UNSPECIFIED.);
#2398=B_SPLINE_CURVE_WITH_KNOTS('',3,(#50118,#50119,#50120,#50121,#50122,
#50123,#50124,#50125,#50126,#50127,#50128,#50129,#50130,#50131,#50132,#50133,
#50134,#50135,#50136,#50137,#50138,#50139),.UNSPECIFIED.,.F.,.F.,(4,3,3,
3,3,3,3,4),(63.946044109826,64.8470718146218,65.8447190733083,66.8423663319948,
67.8400135906813,68.8376608493678,69.8353081080543,70.2292294170057),
 .UNSPECIFIED.);
#2399=B_SPLINE_CURVE_WITH_KNOTS('',3,(#50144,#50145,#50146,#50147,#50148,
#50149,#50150,#50151,#50152,#50153,#50154,#50155,#50156,#50157,#50158,#50159,
#50160,#50161,#50162,#50163,#50164,#50165),.UNSPECIFIED.,.F.,.F.,(4,3,3,
3,3,3,3,4),(-79.4907654349934,-78.8141334362326,-77.8164861775462,-76.8188389188597,
-75.8211916601732,-74.8235444014867,-73.8258971428002,-73.2075801278138),
 .UNSPECIFIED.);
#2400=B_SPLINE_CURVE_WITH_KNOTS('',3,(#50166,#50167,#50168,#50169,#50170,
#50171,#50172,#50173,#50174,#50175,#50176,#50177,#50178,#50179,#50180,#50181,
#50182,#50183,#50184,#50185,#50186,#50187),.UNSPECIFIED.,.F.,.F.,(4,3,3,
3,3,3,3,4),(70.2292294170057,70.8329553667407,71.8306026254272,72.8282498841137,
73.8258971428002,74.8235444014867,75.8211916601732,76.5124147241852),
 .UNSPECIFIED.);
#2401=B_SPLINE_CURVE_WITH_KNOTS('',3,(#50192,#50193,#50194,#50195,#50196,
#50197,#50198,#50199,#50200,#50201,#50202,#50203,#50204,#50205,#50206,#50207,
#50208,#50209,#50210,#50211,#50212,#50213),.UNSPECIFIED.,.F.,.F.,(4,3,3,
3,3,3,3,4),(-85.773950742173,-84.8000169883516,-83.8023697296651,-82.8047224709786,
-81.8070752122921,-80.8094279536056,-79.8117806949191,-79.4907654349934),
 .UNSPECIFIED.);
#2402=B_SPLINE_CURVE_WITH_KNOTS('',3,(#50214,#50215,#50216,#50217,#50218,
#50219,#50220,#50221,#50222,#50223,#50224,#50225,#50226,#50227,#50228,#50229,
#50230,#50231,#50232,#50233,#50234,#50235),.UNSPECIFIED.,.F.,.F.,(4,3,3,
3,3,3,3,4),(76.5124147241852,76.8188389188597,77.8164861775462,78.8141334362327,
79.8117806949192,80.8094279536056,81.8070752122921,82.7956000313648),
 .UNSPECIFIED.);
#2403=B_SPLINE_CURVE_WITH_KNOTS('',3,(#50240,#50241,#50242,#50243,#50244,
#50245,#50246,#50247,#50248,#50249,#50250,#50251,#50252,#50253,#50254,#50255,
#50256,#50257,#50258,#50259,#50260,#50261,#50262,#50263,#50264),
 .UNSPECIFIED.,.F.,.F.,(4,3,3,3,3,3,3,3,4),(-92.0571360493526,-91.783547799157,
-90.7859005404705,-89.788253281784,-88.7906060230975,-87.792958764411,-86.7953115057246,
-85.7976642470381,-85.773950742173),.UNSPECIFIED.);
#2404=B_SPLINE_CURVE_WITH_KNOTS('',3,(#50265,#50266,#50267,#50268,#50269,
#50270,#50271,#50272,#50273,#50274,#50275,#50276,#50277,#50278,#50279,#50280,
#50281,#50282,#50283,#50284,#50285,#50286,#50287,#50288,#50289),
 .UNSPECIFIED.,.F.,.F.,(4,3,3,3,3,3,3,3,4),(82.7956000313648,82.8047224709786,
83.8023697296651,84.8000169883516,85.7976642470381,86.7953115057246,87.7929587644111,
88.7906060230976,89.0787853385444),.UNSPECIFIED.);
#2405=B_SPLINE_CURVE_WITH_KNOTS('',3,(#50294,#50295,#50296,#50297,#50298,
#50299,#50300,#50301,#50302,#50303,#50304,#50305,#50306,#50307,#50308,#50309,
#50310,#50311,#50312,#50313,#50314,#50315),.UNSPECIFIED.,.F.,.F.,(4,3,3,
3,3,3,3,4),(-98.3403213565322,-97.7694313512759,-96.7717840925894,-95.774136833903,
-94.7764895752164,-93.77884231653,-92.7811950578435,-92.0571360493526),
 .UNSPECIFIED.);
#2406=B_SPLINE_CURVE_WITH_KNOTS('',3,(#50316,#50317,#50318,#50319,#50320,
#50321,#50322,#50323,#50324,#50325,#50326,#50327,#50328,#50329,#50330,#50331,
#50332,#50333,#50334,#50335,#50336,#50337),.UNSPECIFIED.,.F.,.F.,(4,3,3,
3,3,3,3,4),(89.0787853385444,89.7882532817841,90.7859005404705,91.783547799157,
92.7811950578435,93.77884231653,94.7764895752165,95.361970645724),
 .UNSPECIFIED.);
#2407=B_SPLINE_CURVE_WITH_KNOTS('',3,(#50342,#50343,#50344,#50345,#50346,
#50347,#50348,#50349,#50350,#50351,#50352,#50353,#50354,#50355,#50356,#50357,
#50358,#50359,#50360,#50361,#50362,#50363),.UNSPECIFIED.,.F.,.F.,(4,3,3,
3,3,3,3,4),(-104.623506663712,-103.755314903395,-102.757667644708,-101.760020386022,
-100.762373127335,-99.7647258686489,-98.7670786099624,-98.3403213565322),
 .UNSPECIFIED.);
#2408=B_SPLINE_CURVE_WITH_KNOTS('',3,(#50364,#50365,#50366,#50367,#50368,
#50369,#50370,#50371,#50372,#50373,#50374,#50375,#50376,#50377,#50378,#50379,
#50380,#50381,#50382,#50383,#50384,#50385),.UNSPECIFIED.,.F.,.F.,(4,3,3,
3,3,3,3,4),(95.361970645724,95.774136833903,96.7717840925895,97.769431351276,
98.7670786099625,99.7647258686489,100.762373127335,101.645155952904),
 .UNSPECIFIED.);
#2409=B_SPLINE_CURVE_WITH_KNOTS('',3,(#50390,#50391,#50392,#50393,#50394,
#50395,#50396,#50397,#50398,#50399,#50400,#50401,#50402,#50403,#50404,#50405,
#50406,#50407,#50408,#50409,#50410,#50411,#50412,#50413,#50414),
 .UNSPECIFIED.,.F.,.F.,(4,3,3,3,3,3,3,3,4),(-110.906691970891,-110.7388457142,
-109.741198455514,-108.743551196827,-107.745903938141,-106.748256679454,
-105.750609420768,-104.752962162081,-104.623506663712),.UNSPECIFIED.);
#2410=B_SPLINE_CURVE_WITH_KNOTS('',3,(#50415,#50416,#50417,#50418,#50419,
#50420,#50421,#50422,#50423,#50424,#50425,#50426,#50427,#50428,#50429,#50430,
#50431,#50432,#50433,#50434,#50435,#50436,#50437,#50438,#50439),
 .UNSPECIFIED.,.F.,.F.,(4,3,3,3,3,3,3,3,4),(101.645155952904,101.760020386022,
102.757667644708,103.755314903395,104.752962162081,105.750609420768,106.748256679454,
107.745903938141,107.928341260083),.UNSPECIFIED.);
#2411=B_SPLINE_CURVE_WITH_KNOTS('',3,(#50444,#50445,#50446,#50447,#50448,
#50449,#50450,#50451,#50452,#50453,#50454,#50455,#50456,#50457,#50458,#50459,
#50460,#50461,#50462,#50463,#50464,#50465),.UNSPECIFIED.,.F.,.F.,(4,3,3,
3,3,3,3,4),(-117.189877278071,-116.724729266319,-115.727082007633,-114.729434748946,
-113.73178749026,-112.734140231573,-111.736492972887,-110.906691970891),
 .UNSPECIFIED.);
#2412=B_SPLINE_CURVE_WITH_KNOTS('',3,(#50466,#50467,#50468,#50469,#50470,
#50471,#50472,#50473,#50474,#50475,#50476,#50477,#50478,#50479,#50480,#50481,
#50482,#50483,#50484,#50485,#50486,#50487),.UNSPECIFIED.,.F.,.F.,(4,3,3,
3,3,3,3,4),(107.928341260083,108.743551196827,109.741198455514,110.7388457142,
111.736492972887,112.734140231573,113.73178749026,114.211526567263),
 .UNSPECIFIED.);
#2413=B_SPLINE_CURVE_WITH_KNOTS('',3,(#50492,#50493,#50494,#50495,#50496,
#50497,#50498,#50499,#50500,#50501,#50502,#50503,#50504,#50505,#50506,#50507,
#50508,#50509,#50510,#50511,#50512,#50513),.UNSPECIFIED.,.F.,.F.,(4,3,3,
3,3,3,3,4),(-123.473062585251,-122.710612818438,-121.712965559752,-120.715318301065,
-119.717671042379,-118.720023783692,-117.722376525006,-117.189877278071),
 .UNSPECIFIED.);
#2414=B_SPLINE_CURVE_WITH_KNOTS('',3,(#50514,#50515,#50516,#50517,#50518,
#50519,#50520,#50521,#50522,#50523,#50524,#50525,#50526,#50527,#50528,#50529,
#50530,#50531,#50532,#50533,#50534,#50535),.UNSPECIFIED.,.F.,.F.,(4,3,3,
3,3,3,3,4),(114.211526567263,114.729434748946,115.727082007633,116.724729266319,
117.722376525006,118.720023783692,119.717671042379,120.494711874442),
 .UNSPECIFIED.);
#2415=B_SPLINE_CURVE_WITH_KNOTS('',3,(#50540,#50541,#50542,#50543,#50544,
#50545,#50546,#50547,#50548,#50549,#50550,#50551,#50552,#50553,#50554,#50555,
#50556,#50557,#50558,#50559,#50560,#50561,#50562,#50563,#50564),
 .UNSPECIFIED.,.F.,.F.,(4,3,3,3,3,3,3,3,4),(-129.75624789243,-129.694143629244,
-128.696496370557,-127.698849111871,-126.701201853184,-125.703554594498,
-124.705907335811,-123.708260077125,-123.473062585251),.UNSPECIFIED.);
#2416=B_SPLINE_CURVE_WITH_KNOTS('',3,(#50565,#50566,#50567,#50568,#50569,
#50570,#50571,#50572,#50573,#50574,#50575,#50576,#50577,#50578,#50579,#50580,
#50581,#50582,#50583,#50584,#50585,#50586,#50587,#50588,#50589),
 .UNSPECIFIED.,.F.,.F.,(4,3,3,3,3,3,3,3,4),(120.494711874442,120.715318301065,
121.712965559752,122.710612818438,123.708260077125,124.705907335811,125.703554594498,
126.701201853184,126.777897181622),.UNSPECIFIED.);
#2417=B_SPLINE_CURVE_WITH_KNOTS('',3,(#50594,#50595,#50596,#50597,#50598,
#50599,#50600,#50601,#50602,#50603,#50604,#50605,#50606,#50607,#50608,#50609,
#50610,#50611,#50612,#50613,#50614,#50615),.UNSPECIFIED.,.F.,.F.,(4,3,3,
3,3,3,3,4),(-136.03943319961,-135.680027181363,-134.682379922676,-133.68473266399,
-132.687085405303,-131.689438146617,-130.69179088793,-129.75624789243),
 .UNSPECIFIED.);
#2418=B_SPLINE_CURVE_WITH_KNOTS('',3,(#50616,#50617,#50618,#50619,#50620,
#50621,#50622,#50623,#50624,#50625,#50626,#50627,#50628,#50629,#50630,#50631,
#50632,#50633,#50634,#50635,#50636,#50637),.UNSPECIFIED.,.F.,.F.,(4,3,3,
3,3,3,3,4),(126.777897181622,127.698849111871,128.696496370557,129.694143629244,
130.69179088793,131.689438146617,132.687085405303,133.061082488802),
 .UNSPECIFIED.);
#2419=B_SPLINE_CURVE_WITH_KNOTS('',3,(#50642,#50643,#50644,#50645,#50646,
#50647,#50648,#50649,#50650,#50651,#50652,#50653,#50654,#50655,#50656,#50657,
#50658,#50659,#50660,#50661,#50662,#50663),.UNSPECIFIED.,.F.,.F.,(4,3,3,
3,3,3,3,4),(-142.322618506789,-141.665910733481,-140.668263474795,-139.670616216108,
-138.672968957422,-137.675321698735,-136.677674440049,-136.03943319961),
 .UNSPECIFIED.);
#2420=B_SPLINE_CURVE_WITH_KNOTS('',3,(#50664,#50665,#50666,#50667,#50668,
#50669,#50670,#50671,#50672,#50673,#50674,#50675,#50676,#50677,#50678,#50679,
#50680,#50681,#50682,#50683,#50684,#50685),.UNSPECIFIED.,.F.,.F.,(4,3,3,
3,3,3,3,4),(133.061082488802,133.68473266399,134.682379922676,135.680027181363,
136.677674440049,137.675321698736,138.672968957422,139.344267795981),
 .UNSPECIFIED.);
#2421=B_SPLINE_CURVE_WITH_KNOTS('',3,(#50690,#50691,#50692,#50693,#50694,
#50695,#50696,#50697,#50698,#50699,#50700,#50701,#50702,#50703,#50704,#50705,
#50706,#50707,#50708,#50709,#50710,#50711),.UNSPECIFIED.,.F.,.F.,(4,3,3,
3,3,3,3,4),(-148.605803813969,-147.6517942856,-146.654147026914,-145.656499768227,
-144.658852509541,-143.661205250854,-142.663557992168,-142.322618506789),
 .UNSPECIFIED.);
#2422=B_SPLINE_CURVE_WITH_KNOTS('',3,(#50712,#50713,#50714,#50715,#50716,
#50717,#50718,#50719,#50720,#50721,#50722,#50723,#50724,#50725,#50726,#50727,
#50728,#50729,#50730,#50731,#50732,#50733),.UNSPECIFIED.,.F.,.F.,(4,3,3,
3,3,3,3,4),(139.344267795981,139.670616216109,140.668263474795,141.665910733481,
142.663557992168,143.661205250854,144.658852509541,145.627453103161),
 .UNSPECIFIED.);
#2423=B_SPLINE_CURVE_WITH_KNOTS('',3,(#50738,#50739,#50740,#50741,#50742,
#50743,#50744,#50745,#50746,#50747,#50748,#50749,#50750,#50751,#50752,#50753,
#50754,#50755,#50756,#50757,#50758,#50759,#50760,#50761,#50762),
 .UNSPECIFIED.,.F.,.F.,(4,3,3,3,3,3,3,3,4),(-154.888989121148,-154.635325096406,
-153.637677837719,-152.640030579033,-151.642383320346,-150.64473606166,
-149.647088802973,-148.649441544287,-148.605803813969),.UNSPECIFIED.);
#2424=B_SPLINE_CURVE_WITH_KNOTS('',3,(#50763,#50764,#50765,#50766,#50767,
#50768,#50769,#50770,#50771,#50772,#50773,#50774,#50775,#50776,#50777,#50778,
#50779,#50780,#50781,#50782,#50783,#50784,#50785,#50786,#50787),
 .UNSPECIFIED.,.F.,.F.,(4,3,3,3,3,3,3,3,4),(145.627453103161,145.656499768227,
146.654147026914,147.6517942856,148.649441544287,149.647088802973,150.64473606166,
151.642383320346,151.91063841034),.UNSPECIFIED.);
#2425=B_SPLINE_CURVE_WITH_KNOTS('',3,(#50792,#50793,#50794,#50795,#50796,
#50797,#50798,#50799,#50800,#50801,#50802,#50803,#50804,#50805,#50806,#50807,
#50808,#50809,#50810,#50811,#50812,#50813),.UNSPECIFIED.,.F.,.F.,(4,3,3,
3,3,3,3,4),(-161.172174428328,-160.621208648525,-159.623561389838,-158.625914131152,
-157.628266872465,-156.630619613779,-155.632972355092,-154.888989121148),
 .UNSPECIFIED.);
#2426=B_SPLINE_CURVE_WITH_KNOTS('',3,(#50814,#50815,#50816,#50817,#50818,
#50819,#50820,#50821,#50822,#50823,#50824,#50825,#50826,#50827,#50828,#50829,
#50830,#50831,#50832,#50833,#50834,#50835),.UNSPECIFIED.,.F.,.F.,(4,3,3,
3,3,3,3,4),(151.91063841034,152.640030579033,153.637677837719,154.635325096406,
155.632972355092,156.630619613779,157.628266872465,158.19382371752),
 .UNSPECIFIED.);
#2427=B_SPLINE_CURVE_WITH_KNOTS('',3,(#50840,#50841,#50842,#50843,#50844,
#50845,#50846,#50847,#50848,#50849,#50850,#50851,#50852,#50853,#50854,#50855,
#50856,#50857,#50858,#50859,#50860,#50861),.UNSPECIFIED.,.F.,.F.,(4,3,3,
3,3,3,3,4),(-167.455359735508,-166.607092200644,-165.609444941957,-164.611797683271,
-163.614150424584,-162.616503165898,-161.618855907211,-161.172174428328),
 .UNSPECIFIED.);
#2428=B_SPLINE_CURVE_WITH_KNOTS('',3,(#50862,#50863,#50864,#50865,#50866,
#50867,#50868,#50869,#50870,#50871,#50872,#50873,#50874,#50875,#50876,#50877,
#50878,#50879,#50880,#50881,#50882,#50883),.UNSPECIFIED.,.F.,.F.,(4,3,3,
3,3,3,3,4),(158.19382371752,158.625914131152,159.623561389838,160.621208648525,
161.618855907211,162.616503165898,163.614150424584,164.477009024699),
 .UNSPECIFIED.);
#2429=B_SPLINE_CURVE_WITH_KNOTS('',3,(#50888,#50889,#50890,#50891,#50892,
#50893,#50894,#50895,#50896,#50897,#50898,#50899,#50900,#50901,#50902,#50903,
#50904,#50905,#50906,#50907,#50908,#50909,#50910,#50911,#50912),
 .UNSPECIFIED.,.F.,.F.,(4,3,3,3,3,3,3,3,4),(-173.738545042687,-173.590623011449,
-172.592975752763,-171.595328494076,-170.59768123539,-169.600033976703,
-168.602386718017,-167.60473945933,-167.455359735508),.UNSPECIFIED.);
#2430=B_SPLINE_CURVE_WITH_KNOTS('',3,(#50913,#50914,#50915,#50916,#50917,
#50918,#50919,#50920,#50921,#50922,#50923,#50924,#50925,#50926,#50927,#50928,
#50929,#50930,#50931,#50932,#50933,#50934,#50935,#50936,#50937),
 .UNSPECIFIED.,.F.,.F.,(4,3,3,3,3,3,3,3,4),(164.477009024699,164.611797683271,
165.609444941957,166.607092200644,167.60473945933,168.602386718017,169.600033976703,
170.59768123539,170.760194331879),.UNSPECIFIED.);
#2431=B_SPLINE_CURVE_WITH_KNOTS('',3,(#50942,#50943,#50944,#50945,#50946,
#50947,#50948,#50949,#50950,#50951,#50952,#50953,#50954,#50955,#50956,#50957,
#50958,#50959,#50960,#50961,#50962,#50963),.UNSPECIFIED.,.F.,.F.,(4,3,3,
3,3,3,3,4),(-180.021730349867,-179.576506563568,-178.578859304882,-177.581212046195,
-176.583564787509,-175.585917528822,-174.588270270136,-173.738545042687),
 .UNSPECIFIED.);
#2432=B_SPLINE_CURVE_WITH_KNOTS('',3,(#50964,#50965,#50966,#50967,#50968,
#50969,#50970,#50971,#50972,#50973,#50974,#50975,#50976,#50977,#50978,#50979,
#50980,#50981,#50982,#50983,#50984,#50985),.UNSPECIFIED.,.F.,.F.,(4,3,3,
3,3,3,3,4),(170.760194331879,171.595328494076,172.592975752763,173.590623011449,
174.588270270136,175.585917528822,176.583564787509,177.043379639058),
 .UNSPECIFIED.);
#2433=B_SPLINE_CURVE_WITH_KNOTS('',3,(#50990,#50991,#50992,#50993,#50994,
#50995,#50996,#50997,#50998,#50999,#51000,#51001,#51002,#51003,#51004,#51005,
#51006,#51007,#51008,#51009,#51010,#51011),.UNSPECIFIED.,.F.,.F.,(4,3,3,
3,3,3,3,4),(-186.304915657046,-185.562390115687,-184.564742857,-183.567095598314,
-182.569448339627,-181.571801080941,-180.574153822254,-180.021730349867),
 .UNSPECIFIED.);
#2434=B_SPLINE_CURVE_WITH_KNOTS('',3,(#51012,#51013,#51014,#51015,#51016,
#51017,#51018,#51019,#51020,#51021,#51022,#51023,#51024,#51025,#51026,#51027,
#51028,#51029,#51030,#51031,#51032,#51033),.UNSPECIFIED.,.F.,.F.,(4,3,3,
3,3,3,3,4),(177.043379639058,177.581212046195,178.578859304882,179.576506563568,
180.574153822255,181.571801080941,182.569448339628,183.326564946238),
 .UNSPECIFIED.);
#2435=B_SPLINE_CURVE_WITH_KNOTS('',3,(#51038,#51039,#51040,#51041,#51042,
#51043,#51044,#51045,#51046,#51047,#51048,#51049,#51050,#51051,#51052,#51053,
#51054,#51055,#51056,#51057,#51058,#51059,#51060,#51061,#51062),
 .UNSPECIFIED.,.F.,.F.,(4,3,3,3,3,3,3,3,4),(-192.588100964226,-192.545920926492,
-191.548273667806,-190.550626409119,-189.552979150433,-188.555331891746,
-187.55768463306,-186.560037374373,-186.304915657046),.UNSPECIFIED.);
#2436=B_SPLINE_CURVE_WITH_KNOTS('',3,(#51063,#51064,#51065,#51066,#51067,
#51068,#51069,#51070,#51071,#51072,#51073,#51074,#51075,#51076,#51077,#51078,
#51079,#51080,#51081,#51082,#51083,#51084,#51085,#51086,#51087),
 .UNSPECIFIED.,.F.,.F.,(4,3,3,3,3,3,3,3,4),(183.326564946238,183.567095598314,
184.564742857001,185.562390115687,186.560037374374,187.55768463306,188.555331891746,
189.552979150433,189.609750253418),.UNSPECIFIED.);
#2437=B_SPLINE_CURVE_WITH_KNOTS('',3,(#51092,#51093,#51094,#51095,#51096,
#51097,#51098,#51099,#51100,#51101,#51102,#51103,#51104,#51105,#51106,#51107,
#51108,#51109,#51110,#51111,#51112,#51113),.UNSPECIFIED.,.F.,.F.,(4,3,3,
3,3,3,3,4),(-198.871286271405,-198.531804478611,-197.534157219925,-196.536509961238,
-195.538862702552,-194.541215443865,-193.543568185179,-192.588100964226),
 .UNSPECIFIED.);
#2438=B_SPLINE_CURVE_WITH_KNOTS('',3,(#51114,#51115,#51116,#51117,#51118,
#51119,#51120,#51121,#51122,#51123,#51124,#51125,#51126,#51127,#51128,#51129,
#51130,#51131,#51132,#51133,#51134,#51135),.UNSPECIFIED.,.F.,.F.,(4,3,3,
3,3,3,3,4),(189.609750253418,190.55062640912,191.548273667806,192.545920926492,
193.543568185179,194.541215443865,195.538862702552,195.892935560597),
 .UNSPECIFIED.);
#2439=B_SPLINE_CURVE_WITH_KNOTS('',3,(#51140,#51141,#51142,#51143,#51144,
#51145,#51146,#51147,#51148,#51149,#51150,#51151,#51152,#51153,#51154,#51155,
#51156,#51157,#51158,#51159,#51160,#51161),.UNSPECIFIED.,.F.,.F.,(4,3,3,
3,3,3,3,4),(-205.154471578585,-204.51768803073,-203.520040772044,-202.522393513357,
-201.524746254671,-200.527098995984,-199.529451737298,-198.871286271405),
 .UNSPECIFIED.);
#2440=B_SPLINE_CURVE_WITH_KNOTS('',3,(#51162,#51163,#51164,#51165,#51166,
#51167,#51168,#51169,#51170,#51171,#51172,#51173,#51174,#51175,#51176,#51177,
#51178,#51179,#51180,#51181,#51182,#51183),.UNSPECIFIED.,.F.,.F.,(4,3,3,
3,3,3,3,4),(195.892935560597,196.536509961238,197.534157219925,198.531804478611,
199.529451737298,200.527098995984,201.524746254671,202.176120867777),
 .UNSPECIFIED.);
#2441=B_SPLINE_CURVE_WITH_KNOTS('',3,(#51188,#51189,#51190,#51191,#51192,
#51193,#51194,#51195,#51196,#51197,#51198,#51199,#51200,#51201,#51202,#51203,
#51204,#51205,#51206,#51207,#51208,#51209),.UNSPECIFIED.,.F.,.F.,(4,3,3,
3,3,3,3,4),(-211.437656885764,-210.503571582849,-209.505924324163,-208.508277065476,
-207.51062980679,-206.512982548103,-205.515335289417,-205.154471578585),
 .UNSPECIFIED.);
#2442=B_SPLINE_CURVE_WITH_KNOTS('',3,(#51210,#51211,#51212,#51213,#51214,
#51215,#51216,#51217,#51218,#51219,#51220,#51221,#51222,#51223,#51224,#51225,
#51226,#51227,#51228,#51229,#51230,#51231),.UNSPECIFIED.,.F.,.F.,(4,3,3,
3,3,3,3,4),(202.176120867777,202.522393513357,203.520040772044,204.51768803073,
205.515335289417,206.512982548103,207.51062980679,208.459306174956),
 .UNSPECIFIED.);
#2443=B_SPLINE_CURVE_WITH_KNOTS('',3,(#51236,#51237,#51238,#51239,#51240,
#51241,#51242,#51243,#51244,#51245,#51246,#51247,#51248,#51249,#51250,#51251,
#51252,#51253,#51254,#51255,#51256,#51257,#51258,#51259,#51260),
 .UNSPECIFIED.,.F.,.F.,(4,3,3,3,3,3,3,3,4),(-217.720842192944,-217.487102393655,
-216.489455134968,-215.491807876282,-214.494160617595,-213.496513358909,
-212.498866100222,-211.501218841536,-211.437656885764),.UNSPECIFIED.);
#2444=B_SPLINE_CURVE_WITH_KNOTS('',3,(#51261,#51262,#51263,#51264,#51265,
#51266,#51267,#51268,#51269,#51270,#51271,#51272,#51273,#51274,#51275,#51276,
#51277,#51278,#51279,#51280,#51281,#51282,#51283,#51284,#51285),
 .UNSPECIFIED.,.F.,.F.,(4,3,3,3,3,3,3,3,4),(208.459306174956,208.508277065476,
209.505924324163,210.503571582849,211.501218841536,212.498866100222,213.496513358909,
214.494160617595,214.742491482136),.UNSPECIFIED.);
#2445=B_SPLINE_CURVE_WITH_KNOTS('',3,(#51290,#51291,#51292,#51293,#51294,
#51295,#51296,#51297,#51298,#51299,#51300,#51301,#51302,#51303,#51304,#51305,
#51306,#51307,#51308,#51309,#51310,#51311),.UNSPECIFIED.,.F.,.F.,(4,3,3,
3,3,3,3,4),(-224.004027500124,-223.472985945774,-222.475338687087,-221.477691428401,
-220.480044169714,-219.482396911028,-218.484749652341,-217.720842192944),
 .UNSPECIFIED.);
#2446=B_SPLINE_CURVE_WITH_KNOTS('',3,(#51312,#51313,#51314,#51315,#51316,
#51317,#51318,#51319,#51320,#51321,#51322,#51323,#51324,#51325,#51326,#51327,
#51328,#51329,#51330,#51331,#51332,#51333),.UNSPECIFIED.,.F.,.F.,(4,3,3,
3,3,3,3,4),(214.742491482136,215.491807876282,216.489455134968,217.487102393655,
218.484749652341,219.482396911028,220.480044169714,221.025676789315),
 .UNSPECIFIED.);
#2447=B_SPLINE_CURVE_WITH_KNOTS('',3,(#51338,#51339,#51340,#51341,#51342,
#51343,#51344,#51345,#51346,#51347,#51348,#51349,#51350,#51351,#51352,#51353,
#51354,#51355,#51356,#51357,#51358,#51359),.UNSPECIFIED.,.F.,.F.,(4,3,3,
3,3,3,3,4),(-230.287212807303,-229.458869497892,-228.461222239206,-227.463574980519,
-226.465927721833,-225.468280463147,-224.47063320446,-224.004027500124),
 .UNSPECIFIED.);
#2448=B_SPLINE_CURVE_WITH_KNOTS('',3,(#51360,#51361,#51362,#51363,#51364,
#51365,#51366,#51367,#51368,#51369,#51370,#51371,#51372,#51373,#51374,#51375,
#51376,#51377,#51378,#51379,#51380,#51381),.UNSPECIFIED.,.F.,.F.,(4,3,3,
3,3,3,3,4),(221.025676789315,221.477691428401,222.475338687087,223.472985945774,
224.47063320446,225.468280463147,226.465927721833,227.308862096495),
 .UNSPECIFIED.);
#2449=B_SPLINE_CURVE_WITH_KNOTS('',3,(#51386,#51387,#51388,#51389,#51390,
#51391,#51392,#51393,#51394,#51395,#51396,#51397,#51398,#51399,#51400,#51401,
#51402,#51403,#51404,#51405,#51406,#51407,#51408,#51409,#51410),
 .UNSPECIFIED.,.F.,.F.,(4,3,3,3,3,3,3,3,4),(-236.570398114483,-236.442400308698,
-235.444753050011,-234.447105791325,-233.449458532638,-232.451811273952,
-231.454164015265,-230.456516756579,-230.287212807303),.UNSPECIFIED.);
#2450=B_SPLINE_CURVE_WITH_KNOTS('',3,(#51411,#51412,#51413,#51414,#51415,
#51416,#51417,#51418,#51419,#51420,#51421,#51422,#51423,#51424,#51425,#51426,
#51427,#51428,#51429,#51430,#51431,#51432,#51433,#51434,#51435),
 .UNSPECIFIED.,.F.,.F.,(4,3,3,3,3,3,3,3,4),(227.308862096495,227.46357498052,
228.461222239206,229.458869497893,230.456516756579,231.454164015266,232.451811273952,
233.449458532639,233.592047403675),.UNSPECIFIED.);
#2451=B_SPLINE_CURVE_WITH_KNOTS('',3,(#51440,#51441,#51442,#51443,#51444,
#51445,#51446,#51447,#51448,#51449,#51450,#51451,#51452,#51453,#51454,#51455,
#51456,#51457,#51458,#51459,#51460,#51461),.UNSPECIFIED.,.F.,.F.,(4,3,3,
3,3,3,3,4),(-242.853583421662,-242.428283860817,-241.43063660213,-240.432989343444,
-239.435342084757,-238.437694826071,-237.440047567384,-236.570398114483),
 .UNSPECIFIED.);
#2452=B_SPLINE_CURVE_WITH_KNOTS('',3,(#51462,#51463,#51464,#51465,#51466,
#51467,#51468,#51469,#51470,#51471,#51472,#51473,#51474,#51475,#51476,#51477,
#51478,#51479,#51480,#51481,#51482,#51483),.UNSPECIFIED.,.F.,.F.,(4,3,3,
3,3,3,3,4),(233.592047403675,234.447105791325,235.444753050011,236.442400308698,
237.440047567384,238.437694826071,239.435342084757,239.875232710854),
 .UNSPECIFIED.);
#2453=B_SPLINE_CURVE_WITH_KNOTS('',3,(#51488,#51489,#51490,#51491,#51492,
#51493,#51494,#51495,#51496,#51497,#51498,#51499,#51500,#51501,#51502,#51503,
#51504,#51505,#51506,#51507,#51508,#51509),.UNSPECIFIED.,.F.,.F.,(4,3,3,
3,3,3,3,4),(-249.136768728842,-248.414167412936,-247.416520154249,-246.418872895563,
-245.421225636876,-244.42357837819,-243.425931119503,-242.853583421662),
 .UNSPECIFIED.);
#2454=B_SPLINE_CURVE_WITH_KNOTS('',3,(#51510,#51511,#51512,#51513,#51514,
#51515,#51516,#51517,#51518,#51519,#51520,#51521,#51522,#51523,#51524,#51525,
#51526,#51527,#51528,#51529,#51530,#51531),.UNSPECIFIED.,.F.,.F.,(4,3,3,
3,3,3,3,4),(239.875232710854,240.432989343444,241.43063660213,242.428283860817,
243.425931119503,244.42357837819,245.421225636876,246.158418018034),
 .UNSPECIFIED.);
#2455=B_SPLINE_CURVE_WITH_KNOTS('',3,(#51536,#51537,#51538,#51539,#51540,
#51541,#51542,#51543,#51544,#51545,#51546,#51547,#51548,#51549,#51550,#51551,
#51552,#51553,#51554,#51555,#51556,#51557,#51558,#51559,#51560),
 .UNSPECIFIED.,.F.,.F.,(4,3,3,3,3,3,3,3,4),(-255.419954036021,-255.397698223741,
-254.400050965055,-253.402403706368,-252.404756447682,-251.407109188995,
-250.409461930309,-249.411814671622,-249.136768728842),.UNSPECIFIED.);
#2456=B_SPLINE_CURVE_WITH_KNOTS('',3,(#51561,#51562,#51563,#51564,#51565,
#51566,#51567,#51568,#51569,#51570,#51571,#51572,#51573,#51574,#51575,#51576,
#51577,#51578,#51579,#51580,#51581,#51582,#51583,#51584,#51585),
 .UNSPECIFIED.,.F.,.F.,(4,3,3,3,3,3,3,3,4),(246.158418018034,246.418872895563,
247.416520154249,248.414167412936,249.411814671622,250.409461930309,251.407109188995,
252.404756447682,252.441603325213),.UNSPECIFIED.);
#2457=B_SPLINE_CURVE_WITH_KNOTS('',3,(#51590,#51591,#51592,#51593,#51594,
#51595,#51596,#51597,#51598,#51599,#51600,#51601,#51602,#51603,#51604,#51605,
#51606,#51607,#51608,#51609,#51610,#51611),.UNSPECIFIED.,.F.,.F.,(4,3,3,
3,3,3,3,4),(-261.703139343201,-261.38358177586,-260.385934517174,-259.388287258487,
-258.390639999801,-257.392992741114,-256.395345482428,-255.419954036021),
 .UNSPECIFIED.);
#2458=B_SPLINE_CURVE_WITH_KNOTS('',3,(#51612,#51613,#51614,#51615,#51616,
#51617,#51618,#51619,#51620,#51621,#51622,#51623,#51624,#51625,#51626,#51627,
#51628,#51629,#51630,#51631,#51632,#51633),.UNSPECIFIED.,.F.,.F.,(4,3,3,
3,3,3,3,4),(252.441603325213,253.402403706368,254.400050965055,255.397698223741,
256.395345482428,257.392992741114,258.390639999801,258.724788632393),
 .UNSPECIFIED.);
#2459=B_SPLINE_CURVE_WITH_KNOTS('',3,(#51639,#51640,#51641,#51642,#51643,
#51644),.UNSPECIFIED.,.F.,.F.,(4,1,1,4),(273.318560862312,273.996650553658,
274.994297812344,275.922099455125),.UNSPECIFIED.);
#2460=B_SPLINE_CURVE_WITH_KNOTS('',3,(#51647,#51648,#51649,#51650,#51651),
 .UNSPECIFIED.,.F.,.F.,(4,1,4),(273.318560862312,273.684757733346,274.682404992033),
 .UNSPECIFIED.);
#2461=B_SPLINE_CURVE_WITH_KNOTS('',3,(#51656,#51657,#51658,#51659,#51660,
#51661,#51662,#51663,#51664,#51665),.UNSPECIFIED.,.F.,.F.,(4,1,1,1,1,1,
1,4),(267.035375555132,268.010767001539,269.008414260225,270.006061518912,
271.003708777598,272.001356036285,272.999003294971,273.318560862312),
 .UNSPECIFIED.);
#2462=B_SPLINE_CURVE_WITH_KNOTS('',3,(#51666,#51667,#51668,#51669,#51670,
#51671,#51672,#51673,#51674,#51675),.UNSPECIFIED.,.F.,.F.,(4,1,1,1,1,1,
1,4),(267.035375555132,267.698874181227,268.696521439914,269.6941686986,
270.691815957287,271.689463215973,272.68711047466,273.318560862312),
 .UNSPECIFIED.);
#2463=B_SPLINE_CURVE_WITH_KNOTS('',3,(#51680,#51681,#51682,#51683,#51684,
#51685,#51686,#51687,#51688,#51689,#51690),.UNSPECIFIED.,.F.,.F.,(4,1,1,
1,1,1,1,1,4),(260.752190247953,261.027236190733,262.02488344942,263.022530708106,
264.020177966793,265.017825225479,266.015472484166,267.013119742852,267.035375555132),
 .UNSPECIFIED.);
#2464=B_SPLINE_CURVE_WITH_KNOTS('',3,(#51691,#51692,#51693,#51694,#51695,
#51696,#51697,#51698,#51699,#51700),.UNSPECIFIED.,.F.,.F.,(4,1,1,1,1,1,
1,4),(260.752190247953,261.712990629108,262.710637887795,263.708285146481,
264.705932405168,265.703579663854,266.701226922541,267.035375555132),
 .UNSPECIFIED.);
#2465=B_SPLINE_CURVE_WITH_KNOTS('',3,(#51705,#51706,#51707,#51708,#51709,
#51710,#51711,#51712,#51713,#51714),.UNSPECIFIED.,.F.,.F.,(4,1,1,1,1,1,
1,4),(254.469004940773,255.041352638614,256.038999897301,257.036647155987,
258.034294414674,259.03194167336,260.029588932047,260.752190247953),
 .UNSPECIFIED.);
#2466=B_SPLINE_CURVE_WITH_KNOTS('',3,(#51715,#51716,#51717,#51718,#51719,
#51720,#51721,#51722,#51723,#51724,#51725),.UNSPECIFIED.,.F.,.F.,(4,1,1,
1,1,1,1,1,4),(254.469004940773,254.729459818303,255.727107076989,256.724754335676,
257.722401594362,258.720048853049,259.717696111735,260.715343370422,260.752190247953),
 .UNSPECIFIED.);
#2467=B_SPLINE_CURVE_WITH_KNOTS('',3,(#51730,#51731,#51732,#51733,#51734,
#51735,#51736,#51737,#51738,#51739),.UNSPECIFIED.,.F.,.F.,(4,1,1,1,1,1,
1,4),(248.185819633594,249.055469086495,250.053116345182,251.050763603868,
252.048410862555,253.046058121241,254.043705379928,254.469004940773),
 .UNSPECIFIED.);
#2468=B_SPLINE_CURVE_WITH_KNOTS('',3,(#51740,#51741,#51742,#51743,#51744,
#51745,#51746,#51747,#51748,#51749),.UNSPECIFIED.,.F.,.F.,(4,1,1,1,1,1,
1,4),(248.185819633594,248.743576266184,249.74122352487,250.738870783557,
251.736518042243,252.73416530093,253.731812559616,254.469004940773),
 .UNSPECIFIED.);
#2469=B_SPLINE_CURVE_WITH_KNOTS('',3,(#51754,#51755,#51756,#51757,#51758,
#51759,#51760,#51761,#51762,#51763,#51764),.UNSPECIFIED.,.F.,.F.,(4,1,1,
1,1,1,1,1,4),(241.902634326414,242.07193827569,243.069585534376,244.067232793063,
245.064880051749,246.062527310436,247.060174569122,248.057821827809,248.185819633594),
 .UNSPECIFIED.);
#2470=B_SPLINE_CURVE_WITH_KNOTS('',3,(#51765,#51766,#51767,#51768,#51769,
#51770,#51771,#51772,#51773,#51774),.UNSPECIFIED.,.F.,.F.,(4,1,1,1,1,1,
1,4),(241.902634326414,242.757692714065,243.755339972752,244.752987231438,
245.750634490125,246.748281748811,247.745929007497,248.185819633594),
 .UNSPECIFIED.);
#2471=B_SPLINE_CURVE_WITH_KNOTS('',3,(#51779,#51780,#51781,#51782,#51783,
#51784,#51785,#51786,#51787,#51788),.UNSPECIFIED.,.F.,.F.,(4,1,1,1,1,1,
1,4),(235.619449019234,236.086054723571,237.083701982258,238.081349240944,
239.078996499631,240.076643758317,241.074291017004,241.902634326414),
 .UNSPECIFIED.);
#2472=B_SPLINE_CURVE_WITH_KNOTS('',3,(#51789,#51790,#51791,#51792,#51793,
#51794,#51795,#51796,#51797,#51798,#51799),.UNSPECIFIED.,.F.,.F.,(4,1,1,
1,1,1,1,1,4),(235.619449019235,235.77416190326,236.771809161946,237.769456420633,
238.767103679319,239.764750938006,240.762398196692,241.760045455379,241.902634326414),
 .UNSPECIFIED.);
#2473=B_SPLINE_CURVE_WITH_KNOTS('',3,(#51804,#51805,#51806,#51807,#51808,
#51809,#51810,#51811,#51812,#51813),.UNSPECIFIED.,.F.,.F.,(4,1,1,1,1,1,
1,4),(229.336263712055,230.100171171452,231.097818430139,232.095465688825,
233.093112947512,234.090760206198,235.088407464885,235.619449019234),
 .UNSPECIFIED.);
#2474=B_SPLINE_CURVE_WITH_KNOTS('',3,(#51814,#51815,#51816,#51817,#51818,
#51819,#51820,#51821,#51822,#51823),.UNSPECIFIED.,.F.,.F.,(4,1,1,1,1,1,
1,4),(229.336263712055,229.788278351141,230.785925609827,231.783572868514,
232.7812201272,233.778867385887,234.776514644573,235.619449019235),
 .UNSPECIFIED.);
#2475=B_SPLINE_CURVE_WITH_KNOTS('',3,(#51828,#51829,#51830,#51831,#51832,
#51833,#51834,#51835,#51836,#51837,#51838),.UNSPECIFIED.,.F.,.F.,(4,1,1,
1,1,1,1,1,4),(223.053078404875,223.116640360647,224.114287619333,225.11193487802,
226.109582136706,227.107229395393,228.104876654079,229.102523912766,229.336263712055),
 .UNSPECIFIED.);
#2476=B_SPLINE_CURVE_WITH_KNOTS('',3,(#51839,#51840,#51841,#51842,#51843,
#51844,#51845,#51846,#51847,#51848),.UNSPECIFIED.,.F.,.F.,(4,1,1,1,1,1,
1,4),(223.053078404875,223.802394799022,224.800042057708,225.797689316395,
226.795336575081,227.792983833768,228.790631092454,229.336263712055),
 .UNSPECIFIED.);
#2477=B_SPLINE_CURVE_WITH_KNOTS('',3,(#51853,#51854,#51855,#51856,#51857,
#51858,#51859,#51860,#51861,#51862),.UNSPECIFIED.,.F.,.F.,(4,1,1,1,1,1,
1,4),(216.769893097696,217.130756808528,218.128404067214,219.126051325901,
220.123698584587,221.121345843274,222.11899310196,223.053078404875),
 .UNSPECIFIED.);
#2478=B_SPLINE_CURVE_WITH_KNOTS('',3,(#51863,#51864,#51865,#51866,#51867,
#51868,#51869,#51870,#51871,#51872,#51873),.UNSPECIFIED.,.F.,.F.,(4,1,1,
1,1,1,1,1,4),(216.769893097696,216.818863988216,217.816511246903,218.814158505589,
219.811805764276,220.809453022962,221.807100281649,222.804747540335,223.053078404875),
 .UNSPECIFIED.);
#2479=B_SPLINE_CURVE_WITH_KNOTS('',3,(#51878,#51879,#51880,#51881,#51882,
#51883,#51884,#51885,#51886,#51887),.UNSPECIFIED.,.F.,.F.,(4,1,1,1,1,1,
1,4),(210.486707790516,211.144873256409,212.142520515095,213.140167773782,
214.137815032468,215.135462291155,216.133109549841,216.769893097696),
 .UNSPECIFIED.);
#2480=B_SPLINE_CURVE_WITH_KNOTS('',3,(#51888,#51889,#51890,#51891,#51892,
#51893,#51894,#51895,#51896,#51897),.UNSPECIFIED.,.F.,.F.,(4,1,1,1,1,1,
1,4),(210.486707790516,210.832980436097,211.830627694784,212.82827495347,
213.825922212157,214.823569470843,215.82121672953,216.769893097696),
 .UNSPECIFIED.);
#2481=B_SPLINE_CURVE_WITH_KNOTS('',3,(#51902,#51903,#51904,#51905,#51906,
#51907,#51908,#51909,#51910,#51911),.UNSPECIFIED.,.F.,.F.,(4,1,1,1,1,1,
1,4),(204.203522483337,205.15898970429,206.156636962976,207.154284221663,
208.151931480349,209.149578739036,210.147225997722,210.486707790516),
 .UNSPECIFIED.);
#2482=B_SPLINE_CURVE_WITH_KNOTS('',3,(#51912,#51913,#51914,#51915,#51916,
#51917,#51918,#51919,#51920,#51921),.UNSPECIFIED.,.F.,.F.,(4,1,1,1,1,1,
1,4),(204.203522483337,204.847096883978,205.844744142665,206.842391401351,
207.840038660038,208.837685918724,209.835333177411,210.486707790516),
 .UNSPECIFIED.);
#2483=B_SPLINE_CURVE_WITH_KNOTS('',3,(#51926,#51927,#51928,#51929,#51930,
#51931,#51932,#51933,#51934,#51935,#51936),.UNSPECIFIED.,.F.,.F.,(4,1,1,
1,1,1,1,1,4),(197.920337176157,198.175458893484,199.173106152171,200.170753410857,
201.168400669544,202.16604792823,203.163695186917,204.161342445603,204.203522483337),
 .UNSPECIFIED.);
#2484=B_SPLINE_CURVE_WITH_KNOTS('',3,(#51937,#51938,#51939,#51940,#51941,
#51942,#51943,#51944,#51945,#51946),.UNSPECIFIED.,.F.,.F.,(4,1,1,1,1,1,
1,4),(197.920337176157,198.86121333186,199.858860590546,200.856507849232,
201.854155107919,202.851802366605,203.849449625292,204.203522483337),
 .UNSPECIFIED.);
#2485=B_SPLINE_CURVE_WITH_KNOTS('',3,(#51951,#51952,#51953,#51954,#51955,
#51956,#51957,#51958,#51959,#51960),.UNSPECIFIED.,.F.,.F.,(4,1,1,1,1,1,
1,4),(191.637151868977,192.189575341366,193.187222600052,194.184869858739,
195.182517117425,196.180164376111,197.177811634798,197.920337176157),
 .UNSPECIFIED.);
#2486=B_SPLINE_CURVE_WITH_KNOTS('',3,(#51961,#51962,#51963,#51964,#51965,
#51966,#51967,#51968,#51969,#51970,#51971),.UNSPECIFIED.,.F.,.F.,(4,1,1,
1,1,1,1,1,4),(191.637151868978,191.877682521054,192.875329779741,193.872977038427,
194.870624297114,195.8682715558,196.865918814487,197.863566073173,197.920337176157),
 .UNSPECIFIED.);
#2487=B_SPLINE_CURVE_WITH_KNOTS('',3,(#51976,#51977,#51978,#51979,#51980,
#51981,#51982,#51983,#51984,#51985),.UNSPECIFIED.,.F.,.F.,(4,1,1,1,1,1,
1,4),(185.353966561798,186.203691789247,187.201339047933,188.19898630662,
189.196633565306,190.194280823993,191.191928082679,191.637151868977),
 .UNSPECIFIED.);
#2488=B_SPLINE_CURVE_WITH_KNOTS('',3,(#51986,#51987,#51988,#51989,#51990,
#51991,#51992,#51993,#51994,#51995),.UNSPECIFIED.,.F.,.F.,(4,1,1,1,1,1,
1,4),(185.353966561798,185.891798968935,186.889446227622,187.887093486308,
188.884740744995,189.882388003681,190.880035262368,191.637151868978),
 .UNSPECIFIED.);
#2489=B_SPLINE_CURVE_WITH_KNOTS('',3,(#52000,#52001,#52002,#52003,#52004,
#52005,#52006,#52007,#52008,#52009,#52010),.UNSPECIFIED.,.F.,.F.,(4,1,1,
1,1,1,1,1,4),(179.070781254618,179.220160978441,180.217808237128,181.215455495814,
182.213102754501,183.210750013187,184.208397271874,185.20604453056,185.353966561798),
 .UNSPECIFIED.);
#2490=B_SPLINE_CURVE_WITH_KNOTS('',3,(#52011,#52012,#52013,#52014,#52015,
#52016,#52017,#52018,#52019,#52020),.UNSPECIFIED.,.F.,.F.,(4,1,1,1,1,1,
1,4),(179.070781254619,179.905915416816,180.903562675503,181.901209934189,
182.898857192876,183.896504451562,184.894151710249,185.353966561798),
 .UNSPECIFIED.);
#2491=B_SPLINE_CURVE_WITH_KNOTS('',3,(#52025,#52026,#52027,#52028,#52029,
#52030,#52031,#52032,#52033,#52034),.UNSPECIFIED.,.F.,.F.,(4,1,1,1,1,1,
1,4),(172.787595947439,173.234277426322,174.231924685009,175.229571943695,
176.227219202382,177.224866461068,178.222513719755,179.070781254618),
 .UNSPECIFIED.);
#2492=B_SPLINE_CURVE_WITH_KNOTS('',3,(#52035,#52036,#52037,#52038,#52039,
#52040,#52041,#52042,#52043,#52044,#52045),.UNSPECIFIED.,.F.,.F.,(4,1,1,
1,1,1,1,1,4),(172.787595947439,172.922384606011,173.920031864697,174.917679123384,
175.91532638207,176.912973640757,177.910620899443,178.90826815813,179.070781254619),
 .UNSPECIFIED.);
#2493=B_SPLINE_CURVE_WITH_KNOTS('',3,(#52050,#52051,#52052,#52053,#52054,
#52055,#52056,#52057,#52058,#52059),.UNSPECIFIED.,.F.,.F.,(4,1,1,1,1,1,
1,4),(166.504410640259,167.248393874203,168.24604113289,169.243688391576,
170.241335650263,171.238982908949,172.236630167636,172.787595947439),
 .UNSPECIFIED.);
#2494=B_SPLINE_CURVE_WITH_KNOTS('',3,(#52060,#52061,#52062,#52063,#52064,
#52065,#52066,#52067,#52068,#52069),.UNSPECIFIED.,.F.,.F.,(4,1,1,1,1,1,
1,4),(166.504410640259,166.936501053892,167.934148312578,168.931795571265,
169.929442829951,170.927090088638,171.924737347324,172.787595947439),
 .UNSPECIFIED.);
#2495=B_SPLINE_CURVE_WITH_KNOTS('',3,(#52074,#52075,#52076,#52077,#52078,
#52079,#52080,#52081,#52082,#52083,#52084),.UNSPECIFIED.,.F.,.F.,(4,1,1,
1,1,1,1,1,4),(160.22122533308,160.264863063398,161.262510322084,162.260157580771,
163.257804839457,164.255452098144,165.25309935683,166.250746615517,166.504410640259),
 .UNSPECIFIED.);
#2496=B_SPLINE_CURVE_WITH_KNOTS('',3,(#52085,#52086,#52087,#52088,#52089,
#52090,#52091,#52092,#52093,#52094),.UNSPECIFIED.,.F.,.F.,(4,1,1,1,1,1,
1,4),(160.22122533308,160.950617501773,161.948264760459,162.945912019146,
163.943559277832,164.941206536519,165.938853795205,166.504410640259),
 .UNSPECIFIED.);
#2497=B_SPLINE_CURVE_WITH_KNOTS('',3,(#52099,#52100,#52101,#52102,#52103,
#52104,#52105,#52106,#52107,#52108),.UNSPECIFIED.,.F.,.F.,(4,1,1,1,1,1,
1,4),(153.9380400259,154.278979511279,155.276626769965,156.274274028652,
157.271921287338,158.269568546025,159.267215804711,160.22122533308),
 .UNSPECIFIED.);
#2498=B_SPLINE_CURVE_WITH_KNOTS('',3,(#52109,#52110,#52111,#52112,#52113,
#52114,#52115,#52116,#52117,#52118,#52119),.UNSPECIFIED.,.F.,.F.,(4,1,1,
1,1,1,1,1,4),(153.9380400259,153.967086690968,154.964733949654,155.96238120834,
156.960028467027,157.957675725713,158.9553229844,159.952970243086,160.22122533308),
 .UNSPECIFIED.);
#2499=B_SPLINE_CURVE_WITH_KNOTS('',3,(#52124,#52125,#52126,#52127,#52128,
#52129,#52130,#52131,#52132,#52133),.UNSPECIFIED.,.F.,.F.,(4,1,1,1,1,1,
1,4),(147.654854718721,148.29309595916,149.290743217847,150.288390476533,
151.286037735219,152.283684993906,153.281332252592,153.9380400259),
 .UNSPECIFIED.);
#2500=B_SPLINE_CURVE_WITH_KNOTS('',3,(#52134,#52135,#52136,#52137,#52138,
#52139,#52140,#52141,#52142,#52143),.UNSPECIFIED.,.F.,.F.,(4,1,1,1,1,1,
1,4),(147.654854718721,147.981203138849,148.978850397535,149.976497656222,
150.974144914908,151.971792173595,152.969439432281,153.9380400259),
 .UNSPECIFIED.);
#2501=B_SPLINE_CURVE_WITH_KNOTS('',3,(#52148,#52149,#52150,#52151,#52152,
#52153,#52154,#52155,#52156,#52157),.UNSPECIFIED.,.F.,.F.,(4,1,1,1,1,1,
1,4),(141.371669411541,142.307212407041,143.304859665728,144.302506924414,
145.300154183101,146.297801441787,147.295448700474,147.654854718721),
 .UNSPECIFIED.);
#2502=B_SPLINE_CURVE_WITH_KNOTS('',3,(#52158,#52159,#52160,#52161,#52162,
#52163,#52164,#52165,#52166,#52167),.UNSPECIFIED.,.F.,.F.,(4,1,1,1,1,1,
1,4),(141.371669411541,141.99531958673,142.992966845416,143.990614104103,
144.988261362789,145.985908621476,146.983555880162,147.654854718721),
 .UNSPECIFIED.);
#2503=B_SPLINE_CURVE_WITH_KNOTS('',3,(#52172,#52173,#52174,#52175,#52176,
#52177,#52178,#52179,#52180,#52181,#52182),.UNSPECIFIED.,.F.,.F.,(4,1,1,
1,1,1,1,1,4),(135.088484104361,135.323681596236,136.321328854922,137.318976113609,
138.316623372295,139.314270630982,140.311917889668,141.309565148355,141.371669411541),
 .UNSPECIFIED.);
#2504=B_SPLINE_CURVE_WITH_KNOTS('',3,(#52183,#52184,#52185,#52186,#52187,
#52188,#52189,#52190,#52191,#52192),.UNSPECIFIED.,.F.,.F.,(4,1,1,1,1,1,
1,4),(135.088484104362,136.009436034611,137.007083293297,138.004730551984,
139.00237781067,140.000025069357,140.997672328043,141.371669411541),
 .UNSPECIFIED.);
#2505=B_SPLINE_CURVE_WITH_KNOTS('',3,(#52197,#52198,#52199,#52200,#52201,
#52202,#52203,#52204,#52205,#52206),.UNSPECIFIED.,.F.,.F.,(4,1,1,1,1,1,
1,4),(128.805298797182,129.337798044117,130.335445302803,131.33309256149,
132.330739820176,133.328387078863,134.326034337549,135.088484104361),
 .UNSPECIFIED.);
#2506=B_SPLINE_CURVE_WITH_KNOTS('',3,(#52207,#52208,#52209,#52210,#52211,
#52212,#52213,#52214,#52215,#52216,#52217),.UNSPECIFIED.,.F.,.F.,(4,1,1,
1,1,1,1,1,4),(128.805298797182,129.025905223805,130.023552482492,131.021199741178,
132.018846999865,133.016494258551,134.014141517238,135.011788775924,135.088484104362),
 .UNSPECIFIED.);
#2507=B_SPLINE_CURVE_WITH_KNOTS('',3,(#52222,#52223,#52224,#52225,#52226,
#52227,#52228,#52229,#52230,#52231),.UNSPECIFIED.,.F.,.F.,(4,1,1,1,1,1,
1,4),(122.522113490002,123.351914491998,124.349561750684,125.347209009371,
126.344856268057,127.342503526744,128.34015078543,128.805298797182),
 .UNSPECIFIED.);
#2508=B_SPLINE_CURVE_WITH_KNOTS('',3,(#52232,#52233,#52234,#52235,#52236,
#52237,#52238,#52239,#52240,#52241),.UNSPECIFIED.,.F.,.F.,(4,1,1,1,1,1,
1,4),(122.522113490002,123.040021671686,124.037668930373,125.035316189059,
126.032963447746,127.030610706432,128.028257965119,128.805298797182),
 .UNSPECIFIED.);
#2509=B_SPLINE_CURVE_WITH_KNOTS('',3,(#52246,#52247,#52248,#52249,#52250,
#52251,#52252,#52253,#52254,#52255,#52256),.UNSPECIFIED.,.F.,.F.,(4,1,1,
1,1,1,1,1,4),(116.238928182823,116.368383681192,117.366030939879,118.363678198565,
119.361325457252,120.358972715938,121.356619974625,122.354267233311,122.522113490002),
 .UNSPECIFIED.);
#2510=B_SPLINE_CURVE_WITH_KNOTS('',3,(#52257,#52258,#52259,#52260,#52261,
#52262,#52263,#52264,#52265,#52266),.UNSPECIFIED.,.F.,.F.,(4,1,1,1,1,1,
1,4),(116.238928182823,117.054138119567,118.051785378254,119.04943263694,
120.047079895627,121.044727154313,122.042374413,122.522113490002),
 .UNSPECIFIED.);
#2511=B_SPLINE_CURVE_WITH_KNOTS('',3,(#52271,#52272,#52273,#52274,#52275,
#52276,#52277,#52278,#52279,#52280),.UNSPECIFIED.,.F.,.F.,(4,1,1,1,1,1,
1,4),(109.955742875643,110.382500129073,111.38014738776,112.377794646446,
113.375441905133,114.373089163819,115.370736422506,116.238928182823),
 .UNSPECIFIED.);
#2512=B_SPLINE_CURVE_WITH_KNOTS('',3,(#52281,#52282,#52283,#52284,#52285,
#52286,#52287,#52288,#52289,#52290,#52291),.UNSPECIFIED.,.F.,.F.,(4,1,1,
1,1,1,1,1,4),(109.955742875643,110.070607308762,111.068254567448,112.065901826135,
113.063549084821,114.061196343508,115.058843602194,116.056490860881,116.238928182823),
 .UNSPECIFIED.);
#2513=B_SPLINE_CURVE_WITH_KNOTS('',3,(#52296,#52297,#52298,#52299,#52300,
#52301,#52302,#52303,#52304,#52305),.UNSPECIFIED.,.F.,.F.,(4,1,1,1,1,1,
1,4),(103.672557568464,104.396616576955,105.394263835641,106.391911094327,
107.389558353014,108.3872056117,109.384852870387,109.955742875643),
 .UNSPECIFIED.);
#2514=B_SPLINE_CURVE_WITH_KNOTS('',3,(#52306,#52307,#52308,#52309,#52310,
#52311,#52312,#52313,#52314,#52315),.UNSPECIFIED.,.F.,.F.,(4,1,1,1,1,1,
1,4),(103.672557568464,104.084723756643,105.08237101533,106.080018274016,
107.077665532703,108.075312791389,109.072960050075,109.955742875643),
 .UNSPECIFIED.);
#2515=B_SPLINE_CURVE_WITH_KNOTS('',3,(#52320,#52321,#52322,#52323,#52324,
#52325,#52326,#52327,#52328,#52329,#52330),.UNSPECIFIED.,.F.,.F.,(4,1,1,
1,1,1,1,1,4),(97.3893722612839,97.4130857661491,98.4107330248356,99.4083802835221,
100.406027542209,101.403674800895,102.401322059582,103.398969318268,103.672557568464),
 .UNSPECIFIED.);
#2516=B_SPLINE_CURVE_WITH_KNOTS('',3,(#52331,#52332,#52333,#52334,#52335,
#52336,#52337,#52338,#52339,#52340),.UNSPECIFIED.,.F.,.F.,(4,1,1,1,1,1,
1,4),(97.389372261284,98.0988402045241,99.0964874632106,100.094134721897,
101.091781980584,102.08942923927,103.087076497957,103.672557568464),
 .UNSPECIFIED.);
#2517=B_SPLINE_CURVE_WITH_KNOTS('',3,(#52345,#52346,#52347,#52348,#52349,
#52350,#52351,#52352,#52353,#52354),.UNSPECIFIED.,.F.,.F.,(4,1,1,1,1,1,
1,4),(91.1061869541043,91.4272022140302,92.4248494727166,93.4224967314031,
94.4201439900896,95.4177912487761,96.4154385074626,97.3893722612839),
 .UNSPECIFIED.);
#2518=B_SPLINE_CURVE_WITH_KNOTS('',3,(#52355,#52356,#52357,#52358,#52359,
#52360,#52361,#52362,#52363,#52364,#52365),.UNSPECIFIED.,.F.,.F.,(4,1,1,
1,1,1,1,1,4),(91.1061869541044,91.1153093937187,92.1129566524052,93.1106039110917,
94.1082511697781,95.1058984284646,96.1035456871511,97.1011929458376,97.389372261284),
 .UNSPECIFIED.);
#2519=B_SPLINE_CURVE_WITH_KNOTS('',3,(#52370,#52371,#52372,#52373,#52374,
#52375,#52376,#52377,#52378,#52379),.UNSPECIFIED.,.F.,.F.,(4,1,1,1,1,1,
1,4),(84.8230016469247,85.4413186619112,86.4389659205977,87.4366131792842,
88.4342604379707,89.4319076966572,90.4295549553437,91.1061869541043),
 .UNSPECIFIED.);
#2520=B_SPLINE_CURVE_WITH_KNOTS('',3,(#52380,#52381,#52382,#52383,#52384,
#52385,#52386,#52387,#52388,#52389),.UNSPECIFIED.,.F.,.F.,(4,1,1,1,1,1,
1,4),(84.8230016469249,85.1294258415997,86.1270731002862,87.1247203589727,
88.1223676176592,89.1200148763457,90.1176621350322,91.1061869541044),
 .UNSPECIFIED.);
#2521=B_SPLINE_CURVE_WITH_KNOTS('',3,(#52394,#52395,#52396,#52397,#52398,
#52399,#52400,#52401,#52402,#52403),.UNSPECIFIED.,.F.,.F.,(4,1,1,1,1,1,
1,4),(78.5398163397451,79.4554351097923,80.4530823684788,81.4507296271653,
82.4483768858518,83.4460241445382,84.4436714032247,84.8230016469247),
 .UNSPECIFIED.);
#2522=B_SPLINE_CURVE_WITH_KNOTS('',3,(#52404,#52405,#52406,#52407,#52408,
#52409,#52410,#52411,#52412,#52413),.UNSPECIFIED.,.F.,.F.,(4,1,1,1,1,1,
1,4),(78.5398163397452,79.1435422894808,80.1411895481673,81.1388368068538,
82.1364840655403,83.1341313242268,84.1317785829133,84.8230016469249),
 .UNSPECIFIED.);
#2523=B_SPLINE_CURVE_WITH_KNOTS('',3,(#52418,#52419,#52420,#52421,#52422,
#52423,#52424,#52425,#52426,#52427,#52428),.UNSPECIFIED.,.F.,.F.,(4,1,1,
1,1,1,1,1,4),(72.2566310325655,72.4719042989869,73.4695515576734,74.4671988163598,
75.4648460750463,76.4624933337328,77.4601405924193,78.4577878511058,78.5398163397451),
 .UNSPECIFIED.);
#2524=B_SPLINE_CURVE_WITH_KNOTS('',3,(#52429,#52430,#52431,#52432,#52433,
#52434,#52435,#52436,#52437,#52438),.UNSPECIFIED.,.F.,.F.,(4,1,1,1,1,1,
1,4),(72.2566310325657,73.1576587373619,74.1553059960484,75.1529532547349,
76.1506005134213,77.1482477721078,78.1458950307943,78.5398163397452),
 .UNSPECIFIED.);
#2525=B_SPLINE_CURVE_WITH_KNOTS('',3,(#52443,#52444,#52445,#52446,#52447,
#52448,#52449,#52450,#52451,#52452),.UNSPECIFIED.,.F.,.F.,(4,1,1,1,1,1,
1,4),(65.9734457253859,66.4860207468679,67.4836680055544,68.4813152642409,
69.4789625229274,70.4766097816139,71.4742570403004,72.2566310325655),
 .UNSPECIFIED.);
#2526=B_SPLINE_CURVE_WITH_KNOTS('',3,(#52453,#52454,#52455,#52456,#52457,
#52458,#52459,#52460,#52461,#52462,#52463),.UNSPECIFIED.,.F.,.F.,(4,1,1,
1,1,1,1,1,4),(65.973445725386,66.1741279265564,67.1717751852429,68.1694224439294,
69.1670697026159,70.1647169613024,71.1623642199889,72.1600114786754,72.2566310325657),
 .UNSPECIFIED.);
#2527=B_SPLINE_CURVE_WITH_KNOTS('',3,(#52468,#52469,#52470,#52471,#52472,
#52473,#52474,#52475,#52476,#52477),.UNSPECIFIED.,.F.,.F.,(4,1,1,1,1,1,
1,4),(59.6902604182064,60.500137194749,61.4977844534355,62.495431712122,
63.4930789708085,64.490726229495,65.4883734881815,65.9734457253859),
 .UNSPECIFIED.);
#2528=B_SPLINE_CURVE_WITH_KNOTS('',3,(#52478,#52479,#52480,#52481,#52482,
#52483,#52484,#52485,#52486,#52487),.UNSPECIFIED.,.F.,.F.,(4,1,1,1,1,1,
1,4),(59.6902604182065,60.1882443744375,61.185891633124,62.1835388918105,
63.181186150497,64.1788334091835,65.17648066787,65.973445725386),
 .UNSPECIFIED.);
#2529=B_SPLINE_CURVE_WITH_KNOTS('',3,(#52492,#52493,#52494,#52495,#52496,
#52497,#52498,#52499,#52500,#52501,#52502),.UNSPECIFIED.,.F.,.F.,(4,1,1,
1,1,1,1,1,4),(53.4070751110267,53.5166063839436,54.5142536426301,55.5119009013166,
56.509548160003,57.5071954186895,58.504842677376,59.5024899360625,59.6902604182064),
 .UNSPECIFIED.);
#2530=B_SPLINE_CURVE_WITH_KNOTS('',3,(#52503,#52504,#52505,#52506,#52507,
#52508,#52509,#52510,#52511,#52512),.UNSPECIFIED.,.F.,.F.,(4,1,1,1,1,1,
1,4),(53.4070751110269,54.2023608223186,55.2000080810051,56.1976553396915,
57.195302598378,58.1929498570645,59.190597115751,59.6902604182065),
 .UNSPECIFIED.);
#2531=B_SPLINE_CURVE_WITH_KNOTS('',3,(#52517,#52518,#52519,#52520,#52521,
#52522,#52523,#52524,#52525,#52526),.UNSPECIFIED.,.F.,.F.,(4,1,1,1,1,1,
1,4),(47.1238898038472,47.5307228318246,48.5283700905111,49.5260173491976,
50.5236646078841,51.5213118665706,52.5189591252571,53.4070751110267),
 .UNSPECIFIED.);
#2532=B_SPLINE_CURVE_WITH_KNOTS('',3,(#52527,#52528,#52529,#52530,#52531,
#52532,#52533,#52534,#52535,#52536,#52537),.UNSPECIFIED.,.F.,.F.,(4,1,1,
1,1,1,1,1,4),(47.1238898038473,47.2188300115131,48.2164772701996,49.2141245288861,
50.2117717875726,51.2094190462591,52.2070663049456,53.2047135636321,53.4070751110269),
 .UNSPECIFIED.);
#2533=B_SPLINE_CURVE_WITH_KNOTS('',3,(#52542,#52543,#52544,#52545,#52546,
#52547,#52548,#52549,#52550,#52551),.UNSPECIFIED.,.F.,.F.,(4,1,1,1,1,1,
1,4),(40.8407044966676,41.5448392797057,42.5424865383922,43.5401337970787,
44.5377810557652,45.5354283144517,46.5330755731381,47.1238898038472),
 .UNSPECIFIED.);
#2534=B_SPLINE_CURVE_WITH_KNOTS('',3,(#52552,#52553,#52554,#52555,#52556,
#52557,#52558,#52559,#52560,#52561),.UNSPECIFIED.,.F.,.F.,(4,1,1,1,1,1,
1,4),(40.8407044966677,41.2329464593942,42.2305937180807,43.2282409767672,
44.2258882354537,45.2235354941402,46.2211827528266,47.1238898038473),
 .UNSPECIFIED.);
#2535=B_SPLINE_CURVE_WITH_KNOTS('',3,(#52566,#52567,#52568,#52569,#52570,
#52571,#52572,#52573,#52574,#52575,#52576),.UNSPECIFIED.,.F.,.F.,(4,1,1,
1,1,1,1,1,4),(34.557519189488,34.5613084689003,35.5589557275868,36.5566029862733,
37.5542502449598,38.5518975036462,39.5495447623327,40.5471920210192,40.8407044966676),
 .UNSPECIFIED.);
#2536=B_SPLINE_CURVE_WITH_KNOTS('',3,(#52577,#52578,#52579,#52580,#52581,
#52582,#52583,#52584,#52585,#52586),.UNSPECIFIED.,.F.,.F.,(4,1,1,1,1,1,
1,4),(34.5575191894881,35.2470629072753,36.2447101659618,37.2423574246482,
38.2400046833347,39.2376519420212,40.2352992007077,40.8407044966677),
 .UNSPECIFIED.);
#2537=B_SPLINE_CURVE_WITH_KNOTS('',3,(#52591,#52592,#52593,#52594,#52595,
#52596,#52597,#52598,#52599,#52600),.UNSPECIFIED.,.F.,.F.,(4,1,1,1,1,1,
1,4),(28.2743338823084,28.5754249167814,29.5730721754678,30.5707194341543,
31.5683666928408,32.5660139515273,33.5636612102138,34.557519189488),
 .UNSPECIFIED.);
#2538=B_SPLINE_CURVE_WITH_KNOTS('',3,(#52601,#52602,#52603,#52604,#52605,
#52606,#52607,#52608,#52609,#52610),.UNSPECIFIED.,.F.,.F.,(4,1,1,1,1,1,
1,4),(28.2743338823085,29.2611793551563,30.2588266138428,31.2564738725293,
32.2541211312158,33.2517683899023,34.2494156485888,34.5575191894881),
 .UNSPECIFIED.);
#2539=B_SPLINE_CURVE_WITH_KNOTS('',3,(#52615,#52616,#52617,#52618,#52619,
#52620,#52621,#52622,#52623,#52624),.UNSPECIFIED.,.F.,.F.,(4,1,1,1,1,1,
1,4),(21.9911485751288,22.5895413646624,23.5871886233489,24.5848358820354,
25.5824831407219,26.5801303994084,27.5777776580949,28.2743338823084),
 .UNSPECIFIED.);
#2540=B_SPLINE_CURVE_WITH_KNOTS('',3,(#52625,#52626,#52627,#52628,#52629,
#52630,#52631,#52632,#52633,#52634,#52635),.UNSPECIFIED.,.F.,.F.,(4,1,1,
1,1,1,1,1,4),(21.9911485751289,22.2776485443509,23.2752958030374,24.2729430617239,
25.2705903204104,26.2682375790969,27.2658848377834,28.2635320964698,28.2743338823085),
 .UNSPECIFIED.);
#2541=B_SPLINE_CURVE_WITH_KNOTS('',3,(#52640,#52641,#52642,#52643,#52644,
#52645,#52646,#52647,#52648,#52649),.UNSPECIFIED.,.F.,.F.,(4,1,1,1,1,1,
1,4),(15.7079632679492,16.6036578125435,17.60130507123,18.5989523299165,
19.596599588603,20.5942468472894,21.5918941059759,21.9911485751288),
 .UNSPECIFIED.);
#2542=B_SPLINE_CURVE_WITH_KNOTS('',3,(#52650,#52651,#52652,#52653,#52654,
#52655,#52656,#52657,#52658,#52659),.UNSPECIFIED.,.F.,.F.,(4,1,1,1,1,1,
1,4),(15.7079632679493,16.291764992232,17.2894122509185,18.2870595096049,
19.2847067682914,20.2823540269779,21.2800012856644,21.9911485751289),
 .UNSPECIFIED.);
#2543=B_SPLINE_CURVE_WITH_KNOTS('',3,(#52662,#52663,#52664,#52665,#52666,
#52667,#52668,#52669,#52670,#52671,#52672,#52673,#52674,#52675,#52676,#52677,
#52678,#52679,#52680,#52681,#52682,#52683,#52684,#52685,#52686,#52687,#52688,
#52689,#52690,#52691,#52692,#52693,#52694,#52695,#52696,#52697,#52698,#52699,
#52700,#52701,#52702,#52703,#52704,#52705,#52706,#52707,#52708,#52709,#52710,
#52711,#52712,#52713,#52714,#52715,#52716,#52717,#52718,#52719,#52720,#52721,
#52722,#52723,#52724,#52725,#52726,#52727,#52728,#52729,#52730,#52731,#52732,
#52733,#52734,#52735,#52736,#52737,#52738,#52739,#52740,#52741,#52742,#52743,
#52744,#52745,#52746),.UNSPECIFIED.,.F.,.F.,(4,3,3,3,3,3,3,3,3,3,3,3,3,
3,3,3,3,3,3,3,3,3,3,3,3,3,3,3,4),(-0.366397579005864,-0.355346843401997,
-0.337374205212124,-0.327023766356039,-0.321660460620163,-0.302852850386516,
-0.288389399635472,-0.281253803741762,-0.277593082466284,-0.258152985974441,
-0.238335747277564,-0.225538121552714,-0.218338269767891,-0.214826360536685,
-0.194396506267918,-0.187145244378166,-0.167439047158832,-0.156805333697672,
-0.149254241972043,-0.145835187513462,-0.125406703312949,-0.104529747281994,
-0.0834620766624818,-0.0752632118999826,-0.0721348992869,-0.0504908701427557,
-0.0287975712486206,-0.00756831909181192,0.),.UNSPECIFIED.);
#2544=B_SPLINE_CURVE_WITH_KNOTS('',3,(#52749,#52750,#52751,#52752,#52753,
#52754,#52755,#52756,#52757,#52758,#52759,#52760,#52761,#52762,#52763,#52764,
#52765,#52766,#52767,#52768,#52769,#52770,#52771,#52772,#52773,#52774,#52775,
#52776,#52777,#52778,#52779,#52780,#52781,#52782,#52783,#52784,#52785,#52786,
#52787,#52788,#52789,#52790,#52791,#52792,#52793,#52794,#52795,#52796,#52797,
#52798,#52799,#52800,#52801,#52802,#52803,#52804,#52805,#52806,#52807,#52808,
#52809,#52810,#52811,#52812,#52813,#52814,#52815,#52816,#52817,#52818,#52819,
#52820,#52821,#52822,#52823,#52824,#52825,#52826,#52827,#52828,#52829,#52830,
#52831,#52832,#52833),.UNSPECIFIED.,.F.,.F.,(4,3,3,3,3,3,3,3,3,3,3,3,3,
3,3,3,3,3,3,3,3,3,3,3,3,3,3,3,4),(-0.364629307890682,-0.351006911521526,
-0.329419062578797,-0.319153222372462,-0.313799294766335,-0.309381194149429,
-0.28805875991114,-0.272829974986374,-0.264051709713518,-0.260308217235067,
-0.239577131076176,-0.219357140458664,-0.206074975472251,-0.194939029035285,
-0.191413094196265,-0.171827379537648,-0.166228480513009,-0.145449920448883,
-0.126802705425088,-0.123658925074466,-0.104206162927893,-0.0848250947771817,
-0.0658374354857542,-0.0621954187504667,-0.0590783926424019,-0.0404862701271266,
-0.0222276738045438,-0.00455247856545703,0.),.UNSPECIFIED.);
#2545=B_SPLINE_CURVE_WITH_KNOTS('',3,(#53914,#53915,#53916,#53917,#53918,
#53919,#53920,#53921,#53922,#53923,#53924,#53925,#53926,#53927,#53928,#53929,
#53930,#53931,#53932),.UNSPECIFIED.,.F.,.F.,(4,3,3,3,3,3,4),(258.724788632393,
259.388287258487,260.385934517174,261.38358177586,262.381229034547,263.378876293233,
264.306677936014),.UNSPECIFIED.);
#2546=B_SPLINE_CURVE_WITH_KNOTS('',3,(#53934,#53935,#53936,#53937,#53938,
#53939,#53940,#53941,#53942,#53943,#53944,#53945,#53946,#53947,#53948,#53949,
#53950,#53951,#53952,#53953,#53954,#53955,#53956,#53957,#53958,#53959,#53960,
#53961,#53962,#53963,#53964,#53965,#53966,#53967,#53968,#53969,#53970,#53971,
#53972,#53973,#53974,#53975,#53976,#53977,#53978,#53979,#53980,#53981,#53982,
#53983,#53984,#53985,#53986,#53987,#53988,#53989,#53990,#53991,#53992,#53993,
#53994,#53995,#53996,#53997,#53998,#53999,#54000,#54001,#54002,#54003,#54004,
#54005,#54006,#54007,#54008,#54009,#54010,#54011,#54012,#54013,#54014,#54015,
#54016,#54017,#54018),.UNSPECIFIED.,.F.,.F.,(4,3,3,3,3,3,3,3,3,3,3,3,3,
3,3,3,3,3,3,3,3,3,3,3,3,3,3,3,4),(-0.366397579005823,-0.355346843401945,
-0.337374208775006,-0.327023772701273,-0.321660460826443,-0.302852852909943,
-0.288389401843468,-0.281253813336682,-0.277593084937738,-0.258152990277808,
-0.238335751411466,-0.225538124653135,-0.218338277322973,-0.214826365031749,
-0.19439651065702,-0.187145244378141,-0.167439048322423,-0.156805335511694,
-0.149254246961296,-0.145835189834807,-0.125406707076156,-0.104529752607351,
-0.0834620823221285,-0.0752632122609285,-0.0721348995369247,-0.0504908714072708,
-0.0287975717539159,-0.00756831536751696,0.),.UNSPECIFIED.);
#2547=B_SPLINE_CURVE_WITH_KNOTS('',3,(#54019,#54020,#54021,#54022,#54023,
#54024,#54025,#54026,#54027),.UNSPECIFIED.,.F.,.F.,(4,1,1,1,1,1,4),(10.3757270560183,
11.3035286987995,12.301175957486,13.2988232161725,14.296470474859,15.2941177335455,
15.7079632679493),.UNSPECIFIED.);
#2548=B_SPLINE_CURVE_WITH_KNOTS('',3,(#54033,#54034,#54035,#54036,#54037,
#54038,#54039,#54040,#54041,#54042,#54043,#54044,#54045,#54046,#54047,#54048,
#54049,#54050,#54051,#54052,#54053,#54054,#54055,#54056,#54057,#54058,#54059,
#54060,#54061,#54062,#54063,#54064,#54065,#54066,#54067,#54068,#54069,#54070,
#54071,#54072,#54073,#54074,#54075,#54076,#54077,#54078,#54079,#54080,#54081,
#54082,#54083,#54084,#54085,#54086,#54087,#54088,#54089,#54090,#54091,#54092,
#54093,#54094,#54095,#54096,#54097,#54098,#54099,#54100,#54101,#54102,#54103,
#54104,#54105,#54106,#54107,#54108,#54109,#54110,#54111,#54112,#54113,#54114,
#54115,#54116,#54117),.UNSPECIFIED.,.F.,.F.,(4,3,3,3,3,3,3,3,3,3,3,3,3,
3,3,3,3,3,3,3,3,3,3,3,3,3,3,3,4),(-0.364629307890672,-0.351006911521527,
-0.329419062483496,-0.319153221480068,-0.313799274448012,-0.309381188300517,
-0.288058753940656,-0.272829969762204,-0.264051699307754,-0.260308214521764,
-0.23957712793709,-0.219357134376034,-0.206074970910285,-0.194939021602606,
-0.191413092807867,-0.171827375216207,-0.166228480513036,-0.145449920448906,
-0.12680270395916,-0.123658922471174,-0.104206159570983,-0.0848250934702219,
-0.0658374384621282,-0.0621954412209474,-0.0590784413626975,-0.040486321224885,
-0.022227728381574,-0.00455253779193712,0.),.UNSPECIFIED.);
#2549=B_SPLINE_CURVE_WITH_KNOTS('',3,(#54120,#54121,#54122,#54123,#54124,
#54125,#54126,#54127),.UNSPECIFIED.,.F.,.F.,(4,1,1,1,1,4),(11.615421519111,
12.6130687777975,13.610716036484,14.6083632951705,15.606010553857,15.7079632679492),
 .UNSPECIFIED.);
#2550=B_SPLINE_CURVE_WITH_KNOTS('',3,(#55208,#55209,#55210,#55211,#55212,
#55213,#55214,#55215,#55216,#55217,#55218,#55219,#55220,#55221,#55222,#55223),
 .UNSPECIFIED.,.F.,.F.,(4,3,3,3,3,4),(-266.371818069293,-265.374170810606,
-264.37652355192,-263.378876293233,-262.381229034547,-261.703139343201),
 .UNSPECIFIED.);
#2551=B_SPLINE_CURVE_WITH_KNOTS('',3,(#56003,#56004,#56005,#56006,#56007,
#56008,#56009,#56010,#56011,#56012),.UNSPECIFIED.,.F.,.F.,(4,3,3,4),(-4.09202352044849,
-3.99829879847999,-2.99872409886,-2.07317267331967),.UNSPECIFIED.);
#2552=B_SPLINE_CURVE_WITH_KNOTS('',3,(#56015,#56016,#56017,#56018,#56019,
#56020,#56021),.UNSPECIFIED.,.F.,.F.,(4,3,4),(0.,0.99957469961999,1.12274180646236),
 .UNSPECIFIED.);
#2553=B_SPLINE_CURVE_WITH_KNOTS('',3,(#56026,#56027,#56028,#56029,#56030,
#56031,#56032,#56033,#56034,#56035,#56036,#56037,#56038,#56039,#56040,#56041,
#56042,#56043,#56044,#56045,#56046,#56047),.UNSPECIFIED.,.F.,.F.,(4,3,3,
3,3,3,3,4),(-10.3752088276281,-9.99574699619999,-8.99617229657999,-7.99659759695999,
-6.99702289733998,-5.99744819771999,-4.99787349809999,-4.09202352044849),
 .UNSPECIFIED.);
#2554=B_SPLINE_CURVE_WITH_KNOTS('',3,(#56048,#56049,#56050,#56051,#56052,
#56053,#56054,#56055,#56056,#56057,#56058,#56059,#56060,#56061,#56062,#56063,
#56064,#56065,#56066,#56067,#56068,#56069),.UNSPECIFIED.,.F.,.F.,(4,3,3,
3,3,3,3,4),(1.12274180646236,1.99914939923999,2.99872409886,3.99829879848,
4.9978734981,5.99744819772,6.99702289734001,7.40592711364193),
 .UNSPECIFIED.);
#2555=B_SPLINE_CURVE_WITH_KNOTS('',3,(#56074,#56075,#56076,#56077,#56078,
#56079,#56080,#56081,#56082,#56083,#56084,#56085,#56086,#56087,#56088,#56089,
#56090,#56091,#56092,#56093,#56094,#56095),.UNSPECIFIED.,.F.,.F.,(4,3,3,
3,3,3,3,4),(-16.6583941348077,-15.99319519392,-14.9936204943,-13.99404579468,
-12.99447109506,-11.99489639544,-10.99532169582,-10.3752088276281),
 .UNSPECIFIED.);
#2556=B_SPLINE_CURVE_WITH_KNOTS('',3,(#56096,#56097,#56098,#56099,#56100,
#56101,#56102,#56103,#56104,#56105,#56106,#56107,#56108,#56109,#56110,#56111,
#56112,#56113,#56114,#56115,#56116,#56117),.UNSPECIFIED.,.F.,.F.,(4,3,3,
3,3,3,3,4),(7.40592711364193,7.99659759696,8.99617229658,9.99574699619999,
10.99532169582,11.99489639544,12.99447109506,13.6891124208215),
 .UNSPECIFIED.);
#2557=B_SPLINE_CURVE_WITH_KNOTS('',3,(#56122,#56123,#56124,#56125,#56126,
#56127,#56128,#56129,#56130,#56131,#56132,#56133,#56134,#56135,#56136,#56137,
#56138,#56139,#56140,#56141,#56142,#56143),.UNSPECIFIED.,.F.,.F.,(4,3,3,
3,3,3,3,4),(-22.9415794419873,-21.99064339164,-20.99106869202,-19.9914939924,
-18.99191929278,-17.99234459316,-16.99276989354,-16.6583941348077),
 .UNSPECIFIED.);
#2558=B_SPLINE_CURVE_WITH_KNOTS('',3,(#56144,#56145,#56146,#56147,#56148,
#56149,#56150,#56151,#56152,#56153,#56154,#56155,#56156,#56157,#56158,#56159,
#56160,#56161,#56162,#56163,#56164,#56165),.UNSPECIFIED.,.F.,.F.,(4,3,3,
3,3,3,3,4),(13.6891124208215,13.99404579468,14.9936204943,15.99319519392,
16.99276989354,17.99234459316,18.99191929278,19.9722977280011),
 .UNSPECIFIED.);
#2559=B_SPLINE_CURVE_WITH_KNOTS('',3,(#56170,#56171,#56172,#56173,#56174,
#56175,#56176,#56177,#56178,#56179,#56180,#56181,#56182,#56183,#56184,#56185,
#56186,#56187,#56188,#56189,#56190,#56191,#56192,#56193,#56194),
 .UNSPECIFIED.,.F.,.F.,(4,3,3,3,3,3,3,3,4),(-29.2247647491669,-28.98766628898,
-27.98809158936,-26.98851688974,-25.98894219012,-24.9893674905,-23.98979279088,
-22.99021809126,-22.9415794419873),.UNSPECIFIED.);
#2560=B_SPLINE_CURVE_WITH_KNOTS('',3,(#56195,#56196,#56197,#56198,#56199,
#56200,#56201,#56202,#56203,#56204,#56205,#56206,#56207,#56208,#56209,#56210,
#56211,#56212,#56213,#56214,#56215,#56216,#56217,#56218,#56219),
 .UNSPECIFIED.,.F.,.F.,(4,3,3,3,3,3,3,3,4),(19.9722977280011,19.9914939924,
20.99106869202,21.99064339164,22.99021809126,23.98979279088,24.9893674905,
25.98894219012,26.2554830351807),.UNSPECIFIED.);
#2561=B_SPLINE_CURVE_WITH_KNOTS('',3,(#56224,#56225,#56226,#56227,#56228,
#56229,#56230,#56231,#56232,#56233,#56234,#56235,#56236,#56237,#56238,#56239,
#56240,#56241,#56242,#56243,#56244,#56245),.UNSPECIFIED.,.F.,.F.,(4,3,3,
3,3,3,3,4),(-35.5079500563464,-34.9851144867,-33.98553978708,-32.98596508746,
-31.9863903878399,-30.98681568822,-29.9872409886,-29.2247647491669),
 .UNSPECIFIED.);
#2562=B_SPLINE_CURVE_WITH_KNOTS('',3,(#56246,#56247,#56248,#56249,#56250,
#56251,#56252,#56253,#56254,#56255,#56256,#56257,#56258,#56259,#56260,#56261,
#56262,#56263,#56264,#56265,#56266,#56267),.UNSPECIFIED.,.F.,.F.,(4,3,3,
3,3,3,3,4),(26.2554830351807,26.98851688974,27.98809158936,28.98766628898,
29.9872409886,30.98681568822,31.98639038784,32.5386683423603),
 .UNSPECIFIED.);
#2563=B_SPLINE_CURVE_WITH_KNOTS('',3,(#56272,#56273,#56274,#56275,#56276,
#56277,#56278,#56279,#56280,#56281,#56282,#56283,#56284,#56285,#56286,#56287,
#56288,#56289,#56290,#56291,#56292,#56293),.UNSPECIFIED.,.F.,.F.,(4,3,3,
3,3,3,3,4),(-41.791135363526,-40.9825626844199,-39.9829879847999,-38.9834132851799,
-37.98383858556,-36.98426388594,-35.9846891863199,-35.5079500563464),
 .UNSPECIFIED.);
#2564=B_SPLINE_CURVE_WITH_KNOTS('',3,(#56294,#56295,#56296,#56297,#56298,
#56299,#56300,#56301,#56302,#56303,#56304,#56305,#56306,#56307,#56308,#56309,
#56310,#56311,#56312,#56313,#56314,#56315),.UNSPECIFIED.,.F.,.F.,(4,3,3,
3,3,3,3,4),(32.5386683423603,32.98596508746,33.98553978708,34.9851144867,
35.98468918632,36.98426388594,37.98383858556,38.8218536495399),
 .UNSPECIFIED.);
#2565=B_SPLINE_CURVE_WITH_KNOTS('',3,(#56320,#56321,#56322,#56323,#56324,
#56325,#56326,#56327,#56328,#56329,#56330,#56331,#56332,#56333,#56334,#56335,
#56336,#56337,#56338,#56339,#56340,#56341,#56342,#56343,#56344),
 .UNSPECIFIED.,.F.,.F.,(4,3,3,3,3,3,3,3,4),(-48.0743206707057,-47.9795855817599,
-46.9800108821399,-45.9804361825199,-44.9808614828999,-43.9812867832799,
-42.9817120836599,-41.9821373840399,-41.791135363526),.UNSPECIFIED.);
#2566=B_SPLINE_CURVE_WITH_KNOTS('',3,(#56345,#56346,#56347,#56348,#56349,
#56350,#56351,#56352,#56353,#56354,#56355,#56356,#56357,#56358,#56359,#56360,
#56361,#56362,#56363,#56364,#56365,#56366,#56367,#56368,#56369),
 .UNSPECIFIED.,.F.,.F.,(4,3,3,3,3,3,3,3,4),(38.8218536495399,38.98341328518,
39.9829879848,40.98256268442,41.98213738404,42.9817120836599,43.9812867832799,
44.9808614828999,45.1050389567195),.UNSPECIFIED.);
#2567=B_SPLINE_CURVE_WITH_KNOTS('',3,(#56374,#56375,#56376,#56377,#56378,
#56379,#56380,#56381,#56382,#56383,#56384,#56385,#56386,#56387,#56388,#56389,
#56390,#56391,#56392,#56393,#56394,#56395),.UNSPECIFIED.,.F.,.F.,(4,3,3,
3,3,3,3,4),(-54.3575059778852,-53.9770337794799,-52.9774590798599,-51.9778843802399,
-50.9783096806199,-49.9787349809999,-48.9791602813799,-48.0743206707057),
 .UNSPECIFIED.);
#2568=B_SPLINE_CURVE_WITH_KNOTS('',3,(#56396,#56397,#56398,#56399,#56400,
#56401,#56402,#56403,#56404,#56405,#56406,#56407,#56408,#56409,#56410,#56411,
#56412,#56413,#56414,#56415,#56416,#56417),.UNSPECIFIED.,.F.,.F.,(4,3,3,
3,3,3,3,4),(45.1050389567195,45.9804361825199,46.9800108821399,47.9795855817599,
48.9791602813799,49.9787349809999,50.9783096806199,51.388224263899),
 .UNSPECIFIED.);
#2569=B_SPLINE_CURVE_WITH_KNOTS('',3,(#56422,#56423,#56424,#56425,#56426,
#56427,#56428,#56429,#56430,#56431,#56432,#56433,#56434,#56435,#56436,#56437,
#56438,#56439,#56440,#56441,#56442,#56443),.UNSPECIFIED.,.F.,.F.,(4,3,3,
3,3,3,3,4),(-60.6406912850648,-59.9744819771999,-58.9749072775799,-57.9753325779599,
-56.9757578783399,-55.9761831787199,-54.9766084790999,-54.3575059778852),
 .UNSPECIFIED.);
#2570=B_SPLINE_CURVE_WITH_KNOTS('',3,(#56444,#56445,#56446,#56447,#56448,
#56449,#56450,#56451,#56452,#56453,#56454,#56455,#56456,#56457,#56458,#56459,
#56460,#56461,#56462,#56463,#56464,#56465),.UNSPECIFIED.,.F.,.F.,(4,3,3,
3,3,3,3,4),(51.388224263899,51.9778843802399,52.9774590798599,53.9770337794799,
54.9766084791,55.9761831787199,56.97575787834,57.6714095710787),
 .UNSPECIFIED.);
#2571=B_SPLINE_CURVE_WITH_KNOTS('',3,(#56470,#56471,#56472,#56473,#56474,
#56475,#56476,#56477,#56478,#56479,#56480,#56481,#56482,#56483,#56484,#56485,
#56486,#56487,#56488,#56489,#56490,#56491),.UNSPECIFIED.,.F.,.F.,(4,3,3,
3,3,3,3,4),(-66.9238765922444,-65.9719301749199,-64.9723554752999,-63.9727807756799,
-62.9732060760599,-61.9736313764399,-60.9740566768199,-60.6406912850648),
 .UNSPECIFIED.);
#2572=B_SPLINE_CURVE_WITH_KNOTS('',3,(#56492,#56493,#56494,#56495,#56496,
#56497,#56498,#56499,#56500,#56501,#56502,#56503,#56504,#56505,#56506,#56507,
#56508,#56509,#56510,#56511,#56512,#56513),.UNSPECIFIED.,.F.,.F.,(4,3,3,
3,3,3,3,4),(57.6714095710787,57.97533257796,58.97490727758,59.9744819772,
60.9740566768199,61.9736313764399,62.9732060760599,63.9545948782583),
 .UNSPECIFIED.);
#2573=B_SPLINE_CURVE_WITH_KNOTS('',3,(#56518,#56519,#56520,#56521,#56522,
#56523,#56524,#56525,#56526,#56527,#56528,#56529,#56530,#56531,#56532,#56533,
#56534,#56535,#56536,#56537,#56538,#56539,#56540,#56541,#56542),
 .UNSPECIFIED.,.F.,.F.,(4,3,3,3,3,3,3,3,4),(-73.207061899424,-72.9689530722599,
-71.9693783726399,-70.9698036730199,-69.9702289733999,-68.9706542737799,
-67.9710795741599,-66.9715048745399,-66.9238765922444),.UNSPECIFIED.);
#2574=B_SPLINE_CURVE_WITH_KNOTS('',3,(#56543,#56544,#56545,#56546,#56547,
#56548,#56549,#56550,#56551,#56552,#56553,#56554,#56555,#56556,#56557,#56558,
#56559,#56560,#56561,#56562,#56563,#56564,#56565,#56566,#56567),
 .UNSPECIFIED.,.F.,.F.,(4,3,3,3,3,3,3,3,4),(63.9545948782583,63.9727807756799,
64.9723554752999,65.9719301749199,66.9715048745399,67.9710795741599,68.9706542737799,
69.9702289733999,70.2377801854378),.UNSPECIFIED.);
#2575=B_SPLINE_CURVE_WITH_KNOTS('',3,(#56572,#56573,#56574,#56575,#56576,
#56577,#56578,#56579,#56580,#56581,#56582,#56583,#56584,#56585,#56586,#56587,
#56588,#56589,#56590,#56591,#56592,#56593),.UNSPECIFIED.,.F.,.F.,(4,3,3,
3,3,3,3,4),(-79.4902472066036,-78.9664012699799,-77.9668265703599,-76.9672518707399,
-75.9676771711199,-74.9681024714999,-73.9685277718799,-73.207061899424),
 .UNSPECIFIED.);
#2576=B_SPLINE_CURVE_WITH_KNOTS('',3,(#56594,#56595,#56596,#56597,#56598,
#56599,#56600,#56601,#56602,#56603,#56604,#56605,#56606,#56607,#56608,#56609,
#56610,#56611,#56612,#56613,#56614,#56615),.UNSPECIFIED.,.F.,.F.,(4,3,3,
3,3,3,3,4),(70.2377801854378,70.9698036730199,71.9693783726399,72.9689530722599,
73.9685277718799,74.9681024714999,75.9676771711199,76.5209654926174),
 .UNSPECIFIED.);
#2577=B_SPLINE_CURVE_WITH_KNOTS('',3,(#56620,#56621,#56622,#56623,#56624,
#56625,#56626,#56627,#56628,#56629,#56630,#56631,#56632,#56633,#56634,#56635,
#56636,#56637,#56638,#56639,#56640,#56641),.UNSPECIFIED.,.F.,.F.,(4,3,3,
3,3,3,3,4),(-85.7734325137832,-84.9638494676999,-83.9642747680799,-82.9647000684599,
-81.9651253688399,-80.9655506692199,-79.9659759695999,-79.4902472066036),
 .UNSPECIFIED.);
#2578=B_SPLINE_CURVE_WITH_KNOTS('',3,(#56642,#56643,#56644,#56645,#56646,
#56647,#56648,#56649,#56650,#56651,#56652,#56653,#56654,#56655,#56656,#56657,
#56658,#56659,#56660,#56661,#56662,#56663),.UNSPECIFIED.,.F.,.F.,(4,3,3,
3,3,3,3,4),(76.5209654926174,76.9672518707399,77.9668265703599,78.9664012699799,
79.9659759695999,80.9655506692199,81.9651253688399,82.804150799797),
 .UNSPECIFIED.);
#2579=B_SPLINE_CURVE_WITH_KNOTS('',3,(#56668,#56669,#56670,#56671,#56672,
#56673,#56674,#56675,#56676,#56677,#56678,#56679,#56680,#56681,#56682,#56683,
#56684,#56685,#56686,#56687,#56688,#56689,#56690,#56691,#56692),
 .UNSPECIFIED.,.F.,.F.,(4,3,3,3,3,3,3,3,4),(-92.0566178209628,-91.9608723650399,
-90.9612976654198,-89.9617229657999,-88.9621482661799,-87.9625735665599,
-86.9629988669399,-85.9634241673199,-85.7734325137832),.UNSPECIFIED.);
#2580=B_SPLINE_CURVE_WITH_KNOTS('',3,(#56693,#56694,#56695,#56696,#56697,
#56698,#56699,#56700,#56701,#56702,#56703,#56704,#56705,#56706,#56707,#56708,
#56709,#56710,#56711,#56712,#56713,#56714,#56715,#56716,#56717),
 .UNSPECIFIED.,.F.,.F.,(4,3,3,3,3,3,3,3,4),(82.804150799797,82.9647000684599,
83.9642747680799,84.9638494676999,85.9634241673199,86.9629988669399,87.9625735665599,
88.9621482661799,89.0873361069767),.UNSPECIFIED.);
#2581=B_SPLINE_CURVE_WITH_KNOTS('',3,(#56722,#56723,#56724,#56725,#56726,
#56727,#56728,#56729,#56730,#56731,#56732,#56733,#56734,#56735,#56736,#56737,
#56738,#56739,#56740,#56741,#56742,#56743),.UNSPECIFIED.,.F.,.F.,(4,3,3,
3,3,3,3,4),(-98.3398031281424,-97.9583205627599,-96.9587458631399,-95.9591711635199,
-94.9595964638998,-93.9600217642799,-92.9604470646599,-92.0566178209628),
 .UNSPECIFIED.);
#2582=B_SPLINE_CURVE_WITH_KNOTS('',3,(#56744,#56745,#56746,#56747,#56748,
#56749,#56750,#56751,#56752,#56753,#56754,#56755,#56756,#56757,#56758,#56759,
#56760,#56761,#56762,#56763,#56764,#56765),.UNSPECIFIED.,.F.,.F.,(4,3,3,
3,3,3,3,4),(89.0873361069767,89.9617229657999,90.9612976654199,91.9608723650399,
92.9604470646599,93.9600217642799,94.9595964638998,95.3705214141562),
 .UNSPECIFIED.);
#2583=B_SPLINE_CURVE_WITH_KNOTS('',3,(#56770,#56771,#56772,#56773,#56774,
#56775,#56776,#56777,#56778,#56779,#56780,#56781,#56782,#56783,#56784,#56785,
#56786,#56787,#56788,#56789,#56790,#56791),.UNSPECIFIED.,.F.,.F.,(4,3,3,
3,3,3,3,4),(-104.622988435322,-103.95576876048,-102.95619406086,-101.95661936124,
-100.95704466162,-99.9574699619998,-98.9578952623799,-98.3398031281424),
 .UNSPECIFIED.);
#2584=B_SPLINE_CURVE_WITH_KNOTS('',3,(#56792,#56793,#56794,#56795,#56796,
#56797,#56798,#56799,#56800,#56801,#56802,#56803,#56804,#56805,#56806,#56807,
#56808,#56809,#56810,#56811,#56812,#56813),.UNSPECIFIED.,.F.,.F.,(4,3,3,
3,3,3,3,4),(95.3705214141562,95.9591711635198,96.9587458631399,97.9583205627599,
98.9578952623799,99.9574699619999,100.95704466162,101.653706721336),
 .UNSPECIFIED.);
#2585=B_SPLINE_CURVE_WITH_KNOTS('',3,(#56818,#56819,#56820,#56821,#56822,
#56823,#56824,#56825,#56826,#56827,#56828,#56829,#56830,#56831,#56832,#56833,
#56834,#56835,#56836,#56837,#56838,#56839),.UNSPECIFIED.,.F.,.F.,(4,3,3,
3,3,3,3,4),(-110.906173742502,-109.9532169582,-108.95364225858,-107.95406755896,
-106.95449285934,-105.95491815972,-104.9553434601,-104.622988435322),
 .UNSPECIFIED.);
#2586=B_SPLINE_CURVE_WITH_KNOTS('',3,(#56840,#56841,#56842,#56843,#56844,
#56845,#56846,#56847,#56848,#56849,#56850,#56851,#56852,#56853,#56854,#56855,
#56856,#56857,#56858,#56859,#56860,#56861),.UNSPECIFIED.,.F.,.F.,(4,3,3,
3,3,3,3,4),(101.653706721336,101.95661936124,102.95619406086,103.95576876048,
104.9553434601,105.95491815972,106.95449285934,107.936892028515),
 .UNSPECIFIED.);
#2587=B_SPLINE_CURVE_WITH_KNOTS('',3,(#56866,#56867,#56868,#56869,#56870,
#56871,#56872,#56873,#56874,#56875,#56876,#56877,#56878,#56879,#56880,#56881,
#56882,#56883,#56884,#56885,#56886,#56887,#56888,#56889,#56890),
 .UNSPECIFIED.,.F.,.F.,(4,3,3,3,3,3,3,3,4),(-117.189359049681,-116.95023985554,
-115.95066515592,-114.9510904563,-113.95151575668,-112.95194105706,-111.95236635744,
-110.95279165782,-110.906173742502),.UNSPECIFIED.);
#2588=B_SPLINE_CURVE_WITH_KNOTS('',3,(#56891,#56892,#56893,#56894,#56895,
#56896,#56897,#56898,#56899,#56900,#56901,#56902,#56903,#56904,#56905,#56906,
#56907,#56908,#56909,#56910,#56911,#56912,#56913,#56914,#56915),
 .UNSPECIFIED.,.F.,.F.,(4,3,3,3,3,3,3,3,4),(107.936892028515,107.95406755896,
108.95364225858,109.9532169582,110.95279165782,111.95236635744,112.95194105706,
113.95151575668,114.220077335695),.UNSPECIFIED.);
#2589=B_SPLINE_CURVE_WITH_KNOTS('',3,(#56920,#56921,#56922,#56923,#56924,
#56925,#56926,#56927,#56928,#56929,#56930,#56931,#56932,#56933,#56934,#56935,
#56936,#56937,#56938,#56939,#56940,#56941),.UNSPECIFIED.,.F.,.F.,(4,3,3,
3,3,3,3,4),(-123.472544356861,-122.94768805326,-121.94811335364,-120.94853865402,
-119.9489639544,-118.94938925478,-117.94981455516,-117.189359049681),
 .UNSPECIFIED.);
#2590=B_SPLINE_CURVE_WITH_KNOTS('',3,(#56942,#56943,#56944,#56945,#56946,
#56947,#56948,#56949,#56950,#56951,#56952,#56953,#56954,#56955,#56956,#56957,
#56958,#56959,#56960,#56961,#56962,#56963),.UNSPECIFIED.,.F.,.F.,(4,3,3,
3,3,3,3,4),(114.220077335695,114.9510904563,115.95066515592,116.95023985554,
117.94981455516,118.94938925478,119.9489639544,120.503262642875),
 .UNSPECIFIED.);
#2591=B_SPLINE_CURVE_WITH_KNOTS('',3,(#56968,#56969,#56970,#56971,#56972,
#56973,#56974,#56975,#56976,#56977,#56978,#56979,#56980,#56981,#56982,#56983,
#56984,#56985,#56986,#56987,#56988,#56989),.UNSPECIFIED.,.F.,.F.,(4,3,3,
3,3,3,3,4),(-129.75572966404,-128.94513625098,-127.94556155136,-126.94598685174,
-125.94641215212,-124.9468374525,-123.94726275288,-123.472544356861),
 .UNSPECIFIED.);
#2592=B_SPLINE_CURVE_WITH_KNOTS('',3,(#56990,#56991,#56992,#56993,#56994,
#56995,#56996,#56997,#56998,#56999,#57000,#57001,#57002,#57003,#57004,#57005,
#57006,#57007,#57008,#57009,#57010,#57011),.UNSPECIFIED.,.F.,.F.,(4,3,3,
3,3,3,3,4),(120.503262642875,120.94853865402,121.94811335364,122.94768805326,
123.94726275288,124.9468374525,125.94641215212,126.786447950054),
 .UNSPECIFIED.);
#2593=B_SPLINE_CURVE_WITH_KNOTS('',3,(#57016,#57017,#57018,#57019,#57020,
#57021,#57022,#57023,#57024,#57025,#57026,#57027,#57028,#57029,#57030,#57031,
#57032,#57033,#57034,#57035,#57036,#57037,#57038,#57039,#57040),
 .UNSPECIFIED.,.F.,.F.,(4,3,3,3,3,3,3,3,4),(-136.03891497122,-135.94215914832,
-134.9425844487,-133.94300974908,-132.94343504946,-131.94386034984,-130.94428565022,
-129.9447109506,-129.75572966404),.UNSPECIFIED.);
#2594=B_SPLINE_CURVE_WITH_KNOTS('',3,(#57041,#57042,#57043,#57044,#57045,
#57046,#57047,#57048,#57049,#57050,#57051,#57052,#57053,#57054,#57055,#57056,
#57057,#57058,#57059,#57060,#57061,#57062,#57063,#57064,#57065),
 .UNSPECIFIED.,.F.,.F.,(4,3,3,3,3,3,3,3,4),(126.786447950054,126.94598685174,
127.94556155136,128.94513625098,129.9447109506,130.94428565022,131.94386034984,
132.94343504946,133.069633257234),.UNSPECIFIED.);
#2595=B_SPLINE_CURVE_WITH_KNOTS('',3,(#57070,#57071,#57072,#57073,#57074,
#57075,#57076,#57077,#57078,#57079,#57080,#57081,#57082,#57083,#57084,#57085,
#57086,#57087,#57088,#57089,#57090,#57091),.UNSPECIFIED.,.F.,.F.,(4,3,3,
3,3,3,3,4),(-142.322100278399,-141.93960734604,-140.94003264642,-139.9404579468,
-138.94088324718,-137.94130854756,-136.94173384794,-136.03891497122),
 .UNSPECIFIED.);
#2596=B_SPLINE_CURVE_WITH_KNOTS('',3,(#57092,#57093,#57094,#57095,#57096,
#57097,#57098,#57099,#57100,#57101,#57102,#57103,#57104,#57105,#57106,#57107,
#57108,#57109,#57110,#57111,#57112,#57113),.UNSPECIFIED.,.F.,.F.,(4,3,3,
3,3,3,3,4),(133.069633257234,133.94300974908,134.9425844487,135.94215914832,
136.94173384794,137.94130854756,138.94088324718,139.352818564413),
 .UNSPECIFIED.);
#2597=B_SPLINE_CURVE_WITH_KNOTS('',3,(#57118,#57119,#57120,#57121,#57122,
#57123,#57124,#57125,#57126,#57127,#57128,#57129,#57130,#57131,#57132,#57133,
#57134,#57135,#57136,#57137,#57138,#57139),.UNSPECIFIED.,.F.,.F.,(4,3,3,
3,3,3,3,4),(-148.605285585579,-147.93705554376,-146.93748084414,-145.93790614452,
-144.9383314449,-143.93875674528,-142.93918204566,-142.322100278399),
 .UNSPECIFIED.);
#2598=B_SPLINE_CURVE_WITH_KNOTS('',3,(#57140,#57141,#57142,#57143,#57144,
#57145,#57146,#57147,#57148,#57149,#57150,#57151,#57152,#57153,#57154,#57155,
#57156,#57157,#57158,#57159,#57160,#57161),.UNSPECIFIED.,.F.,.F.,(4,3,3,
3,3,3,3,4),(139.352818564413,139.9404579468,140.94003264642,141.93960734604,
142.93918204566,143.93875674528,144.9383314449,145.636003871593),
 .UNSPECIFIED.);
#2599=B_SPLINE_CURVE_WITH_KNOTS('',3,(#57166,#57167,#57168,#57169,#57170,
#57171,#57172,#57173,#57174,#57175,#57176,#57177,#57178,#57179,#57180,#57181,
#57182,#57183,#57184,#57185,#57186,#57187),.UNSPECIFIED.,.F.,.F.,(4,3,3,
3,3,3,3,4),(-154.888470892759,-153.93450374148,-152.93492904186,-151.93535434224,
-150.93577964262,-149.936204943,-148.93663024338,-148.605285585579),
 .UNSPECIFIED.);
#2600=B_SPLINE_CURVE_WITH_KNOTS('',3,(#57188,#57189,#57190,#57191,#57192,
#57193,#57194,#57195,#57196,#57197,#57198,#57199,#57200,#57201,#57202,#57203,
#57204,#57205,#57206,#57207,#57208,#57209),.UNSPECIFIED.,.F.,.F.,(4,3,3,
3,3,3,3,4),(145.636003871593,145.93790614452,146.93748084414,147.93705554376,
148.93663024338,149.936204943,150.93577964262,151.919189178772),
 .UNSPECIFIED.);
#2601=B_SPLINE_CURVE_WITH_KNOTS('',3,(#57214,#57215,#57216,#57217,#57218,
#57219,#57220,#57221,#57222,#57223,#57224,#57225,#57226,#57227,#57228,#57229,
#57230,#57231,#57232,#57233,#57234,#57235,#57236,#57237,#57238),
 .UNSPECIFIED.,.F.,.F.,(4,3,3,3,3,3,3,3,4),(-161.171656199938,-160.93152663882,
-159.9319519392,-158.93237723958,-157.93280253996,-156.93322784034,-155.93365314072,
-154.9340784411,-154.888470892759),.UNSPECIFIED.);
#2602=B_SPLINE_CURVE_WITH_KNOTS('',3,(#57239,#57240,#57241,#57242,#57243,
#57244,#57245,#57246,#57247,#57248,#57249,#57250,#57251,#57252,#57253,#57254,
#57255,#57256,#57257,#57258,#57259,#57260,#57261,#57262,#57263),
 .UNSPECIFIED.,.F.,.F.,(4,3,3,3,3,3,3,3,4),(151.919189178772,151.93535434224,
152.93492904186,153.93450374148,154.9340784411,155.93365314072,156.93322784034,
157.93280253996,158.202374485952),.UNSPECIFIED.);
#2603=B_SPLINE_CURVE_WITH_KNOTS('',3,(#57268,#57269,#57270,#57271,#57272,
#57273,#57274,#57275,#57276,#57277,#57278,#57279,#57280,#57281,#57282,#57283,
#57284,#57285,#57286,#57287,#57288,#57289),.UNSPECIFIED.,.F.,.F.,(4,3,3,
3,3,3,3,4),(-167.454841507118,-166.92897483654,-165.92940013692,-164.9298254373,
-163.93025073768,-162.93067603806,-161.93110133844,-161.171656199938),
 .UNSPECIFIED.);
#2604=B_SPLINE_CURVE_WITH_KNOTS('',3,(#57290,#57291,#57292,#57293,#57294,
#57295,#57296,#57297,#57298,#57299,#57300,#57301,#57302,#57303,#57304,#57305,
#57306,#57307,#57308,#57309,#57310,#57311),.UNSPECIFIED.,.F.,.F.,(4,3,3,
3,3,3,3,4),(158.202374485952,158.93237723958,159.9319519392,160.93152663882,
161.93110133844,162.93067603806,163.93025073768,164.485559793132),
 .UNSPECIFIED.);
#2605=B_SPLINE_CURVE_WITH_KNOTS('',3,(#57316,#57317,#57318,#57319,#57320,
#57321,#57322,#57323,#57324,#57325,#57326,#57327,#57328,#57329,#57330,#57331,
#57332,#57333,#57334,#57335,#57336,#57337),.UNSPECIFIED.,.F.,.F.,(4,3,3,
3,3,3,3,4),(-173.738026814297,-172.92642303426,-171.92684833464,-170.92727363502,
-169.9276989354,-168.92812423578,-167.92854953616,-167.454841507118),
 .UNSPECIFIED.);
#2606=B_SPLINE_CURVE_WITH_KNOTS('',3,(#57338,#57339,#57340,#57341,#57342,
#57343,#57344,#57345,#57346,#57347,#57348,#57349,#57350,#57351,#57352,#57353,
#57354,#57355,#57356,#57357,#57358,#57359),.UNSPECIFIED.,.F.,.F.,(4,3,3,
3,3,3,3,4),(164.485559793132,164.9298254373,165.92940013692,166.92897483654,
167.92854953616,168.92812423578,169.9276989354,170.768745100311),
 .UNSPECIFIED.);
#2607=B_SPLINE_CURVE_WITH_KNOTS('',3,(#57364,#57365,#57366,#57367,#57368,
#57369,#57370,#57371,#57372,#57373,#57374,#57375,#57376,#57377,#57378,#57379,
#57380,#57381,#57382,#57383,#57384,#57385,#57386,#57387,#57388),
 .UNSPECIFIED.,.F.,.F.,(4,3,3,3,3,3,3,3,4),(-180.021212121477,-179.9234459316,
-178.92387123198,-177.92429653236,-176.92472183274,-175.92514713312,-174.9255724335,
-173.92599773388,-173.738026814297),.UNSPECIFIED.);
#2608=B_SPLINE_CURVE_WITH_KNOTS('',3,(#57389,#57390,#57391,#57392,#57393,
#57394,#57395,#57396,#57397,#57398,#57399,#57400,#57401,#57402,#57403,#57404,
#57405,#57406,#57407,#57408,#57409,#57410,#57411,#57412,#57413),
 .UNSPECIFIED.,.F.,.F.,(4,3,3,3,3,3,3,3,4),(170.768745100311,170.92727363502,
171.92684833464,172.92642303426,173.92599773388,174.9255724335,175.92514713312,
176.92472183274,177.051930407491),.UNSPECIFIED.);
#2609=B_SPLINE_CURVE_WITH_KNOTS('',3,(#57418,#57419,#57420,#57421,#57422,
#57423,#57424,#57425,#57426,#57427,#57428,#57429,#57430,#57431,#57432,#57433,
#57434,#57435,#57436,#57437,#57438,#57439),.UNSPECIFIED.,.F.,.F.,(4,3,3,
3,3,3,3,4),(-186.304397428656,-185.92089412932,-184.9213194297,-183.92174473008,
-182.92217003046,-181.92259533084,-180.92302063122,-180.021212121477),
 .UNSPECIFIED.);
#2610=B_SPLINE_CURVE_WITH_KNOTS('',3,(#57440,#57441,#57442,#57443,#57444,
#57445,#57446,#57447,#57448,#57449,#57450,#57451,#57452,#57453,#57454,#57455,
#57456,#57457,#57458,#57459,#57460,#57461),.UNSPECIFIED.,.F.,.F.,(4,3,3,
3,3,3,3,4),(177.051930407491,177.92429653236,178.92387123198,179.9234459316,
180.92302063122,181.92259533084,182.92217003046,183.33511571467),
 .UNSPECIFIED.);
#2611=B_SPLINE_CURVE_WITH_KNOTS('',3,(#57466,#57467,#57468,#57469,#57470,
#57471,#57472,#57473,#57474,#57475,#57476,#57477,#57478,#57479,#57480,#57481,
#57482,#57483,#57484,#57485,#57486,#57487),.UNSPECIFIED.,.F.,.F.,(4,3,3,
3,3,3,3,4),(-192.587582735836,-191.91834232704,-190.91876762742,-189.9191929278,
-188.91961822818,-187.92004352856,-186.92046882894,-186.304397428656),
 .UNSPECIFIED.);
#2612=B_SPLINE_CURVE_WITH_KNOTS('',3,(#57488,#57489,#57490,#57491,#57492,
#57493,#57494,#57495,#57496,#57497,#57498,#57499,#57500,#57501,#57502,#57503,
#57504,#57505,#57506,#57507,#57508,#57509),.UNSPECIFIED.,.F.,.F.,(4,3,3,
3,3,3,3,4),(183.33511571467,183.92174473008,184.9213194297,185.92089412932,
186.92046882894,187.92004352856,188.91961822818,189.61830102185),
 .UNSPECIFIED.);
#2613=B_SPLINE_CURVE_WITH_KNOTS('',3,(#57514,#57515,#57516,#57517,#57518,
#57519,#57520,#57521,#57522,#57523,#57524,#57525,#57526,#57527,#57528,#57529,
#57530,#57531,#57532,#57533,#57534,#57535),.UNSPECIFIED.,.F.,.F.,(4,3,3,
3,3,3,3,4),(-198.870768043016,-197.91579052476,-196.91621582514,-195.91664112552,
-194.9170664259,-193.91749172628,-192.91791702666,-192.587582735836),
 .UNSPECIFIED.);
#2614=B_SPLINE_CURVE_WITH_KNOTS('',3,(#57536,#57537,#57538,#57539,#57540,
#57541,#57542,#57543,#57544,#57545,#57546,#57547,#57548,#57549,#57550,#57551,
#57552,#57553,#57554,#57555,#57556,#57557),.UNSPECIFIED.,.F.,.F.,(4,3,3,
3,3,3,3,4),(189.61830102185,189.9191929278,190.91876762742,191.91834232704,
192.91791702666,193.91749172628,194.9170664259,195.901486329029),
 .UNSPECIFIED.);
#2615=B_SPLINE_CURVE_WITH_KNOTS('',3,(#57562,#57563,#57564,#57565,#57566,
#57567,#57568,#57569,#57570,#57571,#57572,#57573,#57574,#57575,#57576,#57577,
#57578,#57579,#57580,#57581,#57582,#57583,#57584,#57585,#57586),
 .UNSPECIFIED.,.F.,.F.,(4,3,3,3,3,3,3,3,4),(-205.153953350195,-204.9128134221,
-203.91323872248,-202.91366402286,-201.91408932324,-200.91451462362,-199.914939924,
-198.91536522438,-198.870768043016),.UNSPECIFIED.);
#2616=B_SPLINE_CURVE_WITH_KNOTS('',3,(#57587,#57588,#57589,#57590,#57591,
#57592,#57593,#57594,#57595,#57596,#57597,#57598,#57599,#57600,#57601,#57602,
#57603,#57604,#57605,#57606,#57607,#57608,#57609,#57610,#57611),
 .UNSPECIFIED.,.F.,.F.,(4,3,3,3,3,3,3,3,4),(195.901486329029,195.91664112552,
196.91621582514,197.91579052476,198.91536522438,199.914939924,200.91451462362,
201.91408932324,202.184671636209),.UNSPECIFIED.);
#2617=B_SPLINE_CURVE_WITH_KNOTS('',3,(#57616,#57617,#57618,#57619,#57620,
#57621,#57622,#57623,#57624,#57625,#57626,#57627,#57628,#57629,#57630,#57631,
#57632,#57633,#57634,#57635,#57636,#57637),.UNSPECIFIED.,.F.,.F.,(4,3,3,
3,3,3,3,4),(-211.437138657375,-210.91026161982,-209.9106869202,-208.91111222058,
-207.91153752096,-206.91196282134,-205.91238812172,-205.153953350195),
 .UNSPECIFIED.);
#2618=B_SPLINE_CURVE_WITH_KNOTS('',3,(#57638,#57639,#57640,#57641,#57642,
#57643,#57644,#57645,#57646,#57647,#57648,#57649,#57650,#57651,#57652,#57653,
#57654,#57655,#57656,#57657,#57658,#57659),.UNSPECIFIED.,.F.,.F.,(4,3,3,
3,3,3,3,4),(202.184671636209,202.91366402286,203.91323872248,204.9128134221,
205.91238812172,206.91196282134,207.91153752096,208.467856943389),
 .UNSPECIFIED.);
#2619=B_SPLINE_CURVE_WITH_KNOTS('',3,(#57664,#57665,#57666,#57667,#57668,
#57669,#57670,#57671,#57672,#57673,#57674,#57675,#57676,#57677,#57678,#57679,
#57680,#57681,#57682,#57683,#57684,#57685),.UNSPECIFIED.,.F.,.F.,(4,3,3,
3,3,3,3,4),(-217.720323964554,-216.90770981754,-215.90813511792,-214.9085604183,
-213.90898571868,-212.90941101906,-211.90983631944,-211.437138657375),
 .UNSPECIFIED.);
#2620=B_SPLINE_CURVE_WITH_KNOTS('',3,(#57686,#57687,#57688,#57689,#57690,
#57691,#57692,#57693,#57694,#57695,#57696,#57697,#57698,#57699,#57700,#57701,
#57702,#57703,#57704,#57705,#57706,#57707),.UNSPECIFIED.,.F.,.F.,(4,3,3,
3,3,3,3,4),(208.467856943389,208.91111222058,209.9106869202,210.91026161982,
211.90983631944,212.90941101906,213.90898571868,214.751042250568),
 .UNSPECIFIED.);
#2621=B_SPLINE_CURVE_WITH_KNOTS('',3,(#57712,#57713,#57714,#57715,#57716,
#57717,#57718,#57719,#57720,#57721,#57722,#57723,#57724,#57725,#57726,#57727,
#57728,#57729,#57730,#57731,#57732,#57733,#57734,#57735,#57736),
 .UNSPECIFIED.,.F.,.F.,(4,3,3,3,3,3,3,3,4),(-224.003509271734,-223.90473271488,
-222.90515801526,-221.90558331564,-220.90600861602,-219.9064339164,-218.90685921678,
-217.90728451716,-217.720323964554),.UNSPECIFIED.);
#2622=B_SPLINE_CURVE_WITH_KNOTS('',3,(#57737,#57738,#57739,#57740,#57741,
#57742,#57743,#57744,#57745,#57746,#57747,#57748,#57749,#57750,#57751,#57752,
#57753,#57754,#57755,#57756,#57757,#57758,#57759,#57760,#57761),
 .UNSPECIFIED.,.F.,.F.,(4,3,3,3,3,3,3,3,4),(214.751042250568,214.9085604183,
215.90813511792,216.90770981754,217.90728451716,218.90685921678,219.9064339164,
220.90600861602,221.034227557748),.UNSPECIFIED.);
#2623=B_SPLINE_CURVE_WITH_KNOTS('',3,(#57766,#57767,#57768,#57769,#57770,
#57771,#57772,#57773,#57774,#57775,#57776,#57777,#57778,#57779,#57780,#57781,
#57782,#57783,#57784,#57785,#57786,#57787),.UNSPECIFIED.,.F.,.F.,(4,3,3,
3,3,3,3,4),(-230.286694578913,-229.9021809126,-228.90260621298,-227.90303151336,
-226.90345681374,-225.90388211412,-224.9043074145,-224.003509271734),
 .UNSPECIFIED.);
#2624=B_SPLINE_CURVE_WITH_KNOTS('',3,(#57788,#57789,#57790,#57791,#57792,
#57793,#57794,#57795,#57796,#57797,#57798,#57799,#57800,#57801,#57802,#57803,
#57804,#57805,#57806,#57807,#57808,#57809),.UNSPECIFIED.,.F.,.F.,(4,3,3,
3,3,3,3,4),(221.034227557748,221.90558331564,222.90515801526,223.90473271488,
224.9043074145,225.90388211412,226.90345681374,227.317412864927),
 .UNSPECIFIED.);
#2625=B_SPLINE_CURVE_WITH_KNOTS('',3,(#57814,#57815,#57816,#57817,#57818,
#57819,#57820,#57821,#57822,#57823,#57824,#57825,#57826,#57827,#57828,#57829,
#57830,#57831,#57832,#57833,#57834,#57835),.UNSPECIFIED.,.F.,.F.,(4,3,3,
3,3,3,3,4),(-236.569879886093,-235.89962911032,-234.9000544107,-233.90047971108,
-232.90090501146,-231.90133031184,-230.90175561222,-230.286694578913),
 .UNSPECIFIED.);
#2626=B_SPLINE_CURVE_WITH_KNOTS('',3,(#57836,#57837,#57838,#57839,#57840,
#57841,#57842,#57843,#57844,#57845,#57846,#57847,#57848,#57849,#57850,#57851,
#57852,#57853,#57854,#57855,#57856,#57857),.UNSPECIFIED.,.F.,.F.,(4,3,3,
3,3,3,3,4),(227.317412864927,227.90303151336,228.90260621298,229.9021809126,
230.90175561222,231.90133031184,232.90090501146,233.600598172107),
 .UNSPECIFIED.);
#2627=B_SPLINE_CURVE_WITH_KNOTS('',3,(#57862,#57863,#57864,#57865,#57866,
#57867,#57868,#57869,#57870,#57871,#57872,#57873,#57874,#57875,#57876,#57877,
#57878,#57879,#57880,#57881,#57882,#57883),.UNSPECIFIED.,.F.,.F.,(4,3,3,
3,3,3,3,4),(-242.853065193272,-241.89707730804,-240.89750260842,-239.8979279088,
-238.89835320918,-237.89877850956,-236.89920380994,-236.569879886093),
 .UNSPECIFIED.);
#2628=B_SPLINE_CURVE_WITH_KNOTS('',3,(#57884,#57885,#57886,#57887,#57888,
#57889,#57890,#57891,#57892,#57893,#57894,#57895,#57896,#57897,#57898,#57899,
#57900,#57901,#57902,#57903,#57904,#57905),.UNSPECIFIED.,.F.,.F.,(4,3,3,
3,3,3,3,4),(233.600598172107,233.90047971108,234.9000544107,235.89962911032,
236.89920380994,237.89877850956,238.89835320918,239.883783479286),
 .UNSPECIFIED.);
#2629=B_SPLINE_CURVE_WITH_KNOTS('',3,(#57910,#57911,#57912,#57913,#57914,
#57915,#57916,#57917,#57918,#57919,#57920,#57921,#57922,#57923,#57924,#57925,
#57926,#57927,#57928,#57929,#57930,#57931,#57932,#57933,#57934),
 .UNSPECIFIED.,.F.,.F.,(4,3,3,3,3,3,3,3,4),(-249.136250500452,-248.89410020538,
-247.89452550576,-246.89495080614,-245.89537610652,-244.8958014069,-243.89622670728,
-242.89665200766,-242.853065193272),.UNSPECIFIED.);
#2630=B_SPLINE_CURVE_WITH_KNOTS('',3,(#57935,#57936,#57937,#57938,#57939,
#57940,#57941,#57942,#57943,#57944,#57945,#57946,#57947,#57948,#57949,#57950,
#57951,#57952,#57953,#57954,#57955,#57956,#57957,#57958,#57959),
 .UNSPECIFIED.,.F.,.F.,(4,3,3,3,3,3,3,3,4),(239.883783479286,239.8979279088,
240.89750260842,241.89707730804,242.89665200766,243.89622670728,244.8958014069,
245.89537610652,246.166968786466),.UNSPECIFIED.);
#2631=B_SPLINE_CURVE_WITH_KNOTS('',3,(#57964,#57965,#57966,#57967,#57968,
#57969,#57970,#57971,#57972,#57973,#57974,#57975,#57976,#57977,#57978,#57979,
#57980,#57981,#57982,#57983,#57984,#57985),.UNSPECIFIED.,.F.,.F.,(4,3,3,
3,3,3,3,4),(-255.419435807632,-254.8915484031,-253.89197370348,-252.89239900386,
-251.89282430424,-250.89324960462,-249.893674905,-249.136250500452),
 .UNSPECIFIED.);
#2632=B_SPLINE_CURVE_WITH_KNOTS('',3,(#57986,#57987,#57988,#57989,#57990,
#57991,#57992,#57993,#57994,#57995,#57996,#57997,#57998,#57999,#58000,#58001,
#58002,#58003,#58004,#58005,#58006,#58007),.UNSPECIFIED.,.F.,.F.,(4,3,3,
3,3,3,3,4),(246.166968786466,246.89495080614,247.89452550576,248.89410020538,
249.893674905,250.89324960462,251.89282430424,252.450154093645),
 .UNSPECIFIED.);
#2633=B_SPLINE_CURVE_WITH_KNOTS('',3,(#58012,#58013,#58014,#58015,#58016,
#58017,#58018,#58019,#58020,#58021,#58022,#58023,#58024,#58025,#58026,#58027,
#58028,#58029,#58030,#58031,#58032,#58033),.UNSPECIFIED.,.F.,.F.,(4,3,3,
3,3,3,3,4),(-261.702621114811,-260.88899660082,-259.8894219012,-258.88984720158,
-257.89027250196,-256.89069780234,-255.89112310272,-255.419435807632),
 .UNSPECIFIED.);
#2634=B_SPLINE_CURVE_WITH_KNOTS('',3,(#58034,#58035,#58036,#58037,#58038,
#58039,#58040,#58041,#58042,#58043,#58044,#58045,#58046,#58047,#58048,#58049,
#58050,#58051,#58052,#58053,#58054,#58055),.UNSPECIFIED.,.F.,.F.,(4,3,3,
3,3,3,3,4),(252.450154093645,252.89239900386,253.89197370348,254.8915484031,
255.89112310272,256.89069780234,257.89027250196,258.733339400825),
 .UNSPECIFIED.);
#2635=B_SPLINE_CURVE_WITH_KNOTS('',3,(#58060,#58061,#58062,#58063,#58064,
#58065,#58066,#58067,#58068,#58069,#58070,#58071,#58072,#58073,#58074,#58075,
#58076,#58077,#58078,#58079,#58080,#58081,#58082,#58083,#58084),
 .UNSPECIFIED.,.F.,.F.,(4,3,3,3,3,3,3,3,4),(-267.985806421991,-267.88601949816,
-266.88644479854,-265.88687009892,-264.8872953993,-263.88772069968,-262.88814600006,
-261.88857130044,-261.702621114811),.UNSPECIFIED.);
#2636=B_SPLINE_CURVE_WITH_KNOTS('',3,(#58085,#58086,#58087,#58088,#58089,
#58090,#58091,#58092,#58093,#58094,#58095,#58096,#58097,#58098,#58099,#58100,
#58101,#58102,#58103,#58104,#58105,#58106,#58107,#58108,#58109),
 .UNSPECIFIED.,.F.,.F.,(4,3,3,3,3,3,3,3,4),(258.733339400825,258.88984720158,
259.8894219012,260.88899660082,261.88857130044,262.88814600006,263.88772069968,
264.8872953993,265.016524708005),.UNSPECIFIED.);
#2637=B_SPLINE_CURVE_WITH_KNOTS('',3,(#58114,#58115,#58116,#58117,#58118,
#58119,#58120,#58121,#58122,#58123,#58124,#58125,#58126,#58127,#58128,#58129,
#58130,#58131,#58132,#58133,#58134,#58135),.UNSPECIFIED.,.F.,.F.,(4,3,3,
3,3,3,3,4),(-274.26899172917,-273.88346769588,-272.88389299626,-271.88431829664,
-270.88474359702,-269.8851688974,-268.88559419778,-267.985806421991),
 .UNSPECIFIED.);
#2638=B_SPLINE_CURVE_WITH_KNOTS('',3,(#58136,#58137,#58138,#58139,#58140,
#58141,#58142,#58143,#58144,#58145,#58146,#58147,#58148,#58149,#58150,#58151,
#58152,#58153,#58154,#58155,#58156,#58157),.UNSPECIFIED.,.F.,.F.,(4,3,3,
3,3,3,3,4),(265.016524708005,265.88687009892,266.88644479854,267.88601949816,
268.88559419778,269.8851688974,270.88474359702,271.299710015184),
 .UNSPECIFIED.);
#2639=B_SPLINE_CURVE_WITH_KNOTS('',3,(#58162,#58163,#58164,#58165,#58166,
#58167,#58168,#58169,#58170,#58171,#58172,#58173,#58174,#58175,#58176,#58177,
#58178,#58179,#58180,#58181,#58182,#58183),.UNSPECIFIED.,.F.,.F.,(4,3,3,
3,3,3,3,4),(-280.55217703635,-279.8809158936,-278.88134119398,-277.88176649436,
-276.88219179474,-275.88261709512,-274.8830423955,-274.26899172917),
 .UNSPECIFIED.);
#2640=B_SPLINE_CURVE_WITH_KNOTS('',3,(#58184,#58185,#58186,#58187,#58188,
#58189,#58190,#58191,#58192,#58193,#58194,#58195,#58196,#58197,#58198,#58199,
#58200,#58201,#58202,#58203,#58204,#58205),.UNSPECIFIED.,.F.,.F.,(4,3,3,
3,3,3,3,4),(271.299710015184,271.88431829664,272.88389299626,273.88346769588,
274.8830423955,275.88261709512,276.88219179474,277.582895322364),
 .UNSPECIFIED.);
#2641=B_SPLINE_CURVE_WITH_KNOTS('',3,(#58210,#58211,#58212,#58213,#58214,
#58215,#58216,#58217,#58218,#58219,#58220,#58221,#58222,#58223,#58224,#58225,
#58226,#58227,#58228,#58229,#58230,#58231),.UNSPECIFIED.,.F.,.F.,(4,3,3,
3,3,3,3,4),(-286.835362343529,-285.87836409132,-284.8787893917,-283.87921469208,
-282.87963999246,-281.88006529284,-280.88049059322,-280.55217703635),
 .UNSPECIFIED.);
#2642=B_SPLINE_CURVE_WITH_KNOTS('',3,(#58232,#58233,#58234,#58235,#58236,
#58237,#58238,#58239,#58240,#58241,#58242,#58243,#58244,#58245,#58246,#58247,
#58248,#58249,#58250,#58251,#58252,#58253),.UNSPECIFIED.,.F.,.F.,(4,3,3,
3,3,3,3,4),(277.582895322364,277.88176649436,278.88134119398,279.8809158936,
280.88049059322,281.88006529284,282.87963999246,283.866080629543),
 .UNSPECIFIED.);
#2643=B_SPLINE_CURVE_WITH_KNOTS('',3,(#58258,#58259,#58260,#58261,#58262,
#58263,#58264,#58265,#58266,#58267,#58268,#58269,#58270,#58271,#58272,#58273,
#58274,#58275,#58276,#58277,#58278,#58279,#58280,#58281,#58282),
 .UNSPECIFIED.,.F.,.F.,(4,3,3,3,3,3,3,3,4),(-293.118547650709,-292.87538698866,
-291.87581228904,-290.87623758942,-289.8766628898,-288.87708819018,-287.87751349056,
-286.87793879094,-286.835362343529),.UNSPECIFIED.);
#2644=B_SPLINE_CURVE_WITH_KNOTS('',3,(#58283,#58284,#58285,#58286,#58287,
#58288,#58289,#58290,#58291,#58292,#58293,#58294,#58295,#58296,#58297,#58298,
#58299,#58300,#58301,#58302,#58303,#58304,#58305,#58306,#58307),
 .UNSPECIFIED.,.F.,.F.,(4,3,3,3,3,3,3,3,4),(283.866080629543,283.87921469208,
284.8787893917,285.87836409132,286.87793879094,287.87751349056,288.87708819018,
289.8766628898,290.149265936723),.UNSPECIFIED.);
#2645=B_SPLINE_CURVE_WITH_KNOTS('',3,(#58312,#58313,#58314,#58315,#58316,
#58317,#58318,#58319,#58320,#58321,#58322,#58323,#58324,#58325,#58326,#58327,
#58328,#58329,#58330,#58331,#58332,#58333),.UNSPECIFIED.,.F.,.F.,(4,3,3,
3,3,3,3,4),(-299.401732957889,-298.87283518638,-297.87326048676,-296.87368578714,
-295.87411108752,-294.8745363879,-293.87496168828,-293.118547650709),
 .UNSPECIFIED.);
#2646=B_SPLINE_CURVE_WITH_KNOTS('',3,(#58334,#58335,#58336,#58337,#58338,
#58339,#58340,#58341,#58342,#58343,#58344,#58345,#58346,#58347,#58348,#58349,
#58350,#58351,#58352,#58353,#58354,#58355),.UNSPECIFIED.,.F.,.F.,(4,3,3,
3,3,3,3,4),(290.149265936723,290.87623758942,291.87581228904,292.87538698866,
293.87496168828,294.8745363879,295.87411108752,296.432451243902),
 .UNSPECIFIED.);
#2647=B_SPLINE_CURVE_WITH_KNOTS('',3,(#58360,#58361,#58362,#58363,#58364,
#58365,#58366,#58367,#58368,#58369,#58370,#58371,#58372,#58373,#58374,#58375,
#58376,#58377,#58378,#58379,#58380,#58381),.UNSPECIFIED.,.F.,.F.,(4,3,3,
3,3,3,3,4),(-305.684918265068,-304.8702833841,-303.87070868448,-302.87113398486,
-301.87155928524,-300.87198458562,-299.872409886,-299.401732957889),
 .UNSPECIFIED.);
#2648=B_SPLINE_CURVE_WITH_KNOTS('',3,(#58382,#58383,#58384,#58385,#58386,
#58387,#58388,#58389,#58390,#58391,#58392,#58393,#58394,#58395,#58396,#58397,
#58398,#58399,#58400,#58401,#58402,#58403),.UNSPECIFIED.,.F.,.F.,(4,3,3,
3,3,3,3,4),(296.432451243902,296.87368578714,297.87326048676,298.87283518638,
299.872409886,300.87198458562,301.87155928524,302.715636551082),
 .UNSPECIFIED.);
#2649=B_SPLINE_CURVE_WITH_KNOTS('',3,(#58408,#58409,#58410,#58411,#58412,
#58413,#58414,#58415,#58416,#58417,#58418,#58419,#58420,#58421,#58422,#58423,
#58424,#58425,#58426,#58427,#58428,#58429,#58430,#58431,#58432),
 .UNSPECIFIED.,.F.,.F.,(4,3,3,3,3,3,3,3,4),(-311.968103572248,-311.86730628144,
-310.867731581819,-309.868156882199,-308.868582182579,-307.86900748296,
-306.869432783339,-305.86985808372,-305.684918265068),.UNSPECIFIED.);
#2650=B_SPLINE_CURVE_WITH_KNOTS('',3,(#58433,#58434,#58435,#58436,#58437,
#58438,#58439,#58440,#58441,#58442,#58443,#58444,#58445,#58446,#58447,#58448,
#58449,#58450,#58451,#58452,#58453,#58454,#58455,#58456,#58457),
 .UNSPECIFIED.,.F.,.F.,(4,3,3,3,3,3,3,3,4),(302.715636551082,302.87113398486,
303.87070868448,304.8702833841,305.86985808372,306.86943278334,307.86900748296,
308.86858218258,308.998821858262),.UNSPECIFIED.);
#2651=B_SPLINE_CURVE_WITH_KNOTS('',3,(#58462,#58463,#58464,#58465,#58466,
#58467,#58468,#58469,#58470,#58471,#58472,#58473,#58474,#58475,#58476,#58477,
#58478,#58479,#58480,#58481,#58482,#58483),.UNSPECIFIED.,.F.,.F.,(4,3,3,
3,3,3,3,4),(-318.251288879427,-317.86475447916,-316.86517977954,-315.865605079919,
-314.866030380299,-313.86645568068,-312.866880981059,-311.968103572248),
 .UNSPECIFIED.);
#2652=B_SPLINE_CURVE_WITH_KNOTS('',3,(#58484,#58485,#58486,#58487,#58488,
#58489,#58490,#58491,#58492,#58493,#58494,#58495,#58496,#58497,#58498,#58499,
#58500,#58501,#58502,#58503,#58504,#58505),.UNSPECIFIED.,.F.,.F.,(4,3,3,
3,3,3,3,4),(308.998821858262,309.8681568822,310.86773158182,311.86730628144,
312.86688098106,313.86645568068,314.8660303803,315.282007165441),
 .UNSPECIFIED.);
#2653=B_SPLINE_CURVE_WITH_KNOTS('',3,(#58510,#58511,#58512,#58513,#58514,
#58515,#58516,#58517,#58518,#58519,#58520,#58521,#58522,#58523,#58524,#58525,
#58526,#58527,#58528,#58529,#58530,#58531),.UNSPECIFIED.,.F.,.F.,(4,3,3,
3,3,3,3,4),(-324.534474186607,-323.86220267688,-322.862627977259,-321.863053277639,
-320.86347857802,-319.8639038784,-318.864329178779,-318.251288879427),
 .UNSPECIFIED.);
#2654=B_SPLINE_CURVE_WITH_KNOTS('',3,(#58532,#58533,#58534,#58535,#58536,
#58537,#58538,#58539,#58540,#58541,#58542,#58543,#58544,#58545,#58546,#58547,
#58548,#58549,#58550,#58551,#58552,#58553),.UNSPECIFIED.,.F.,.F.,(4,3,3,
3,3,3,3,4),(315.282007165441,315.86560507992,316.86517977954,317.86475447916,
318.86432917878,319.8639038784,320.86347857802,321.565192472621),
 .UNSPECIFIED.);
#2655=B_SPLINE_CURVE_WITH_KNOTS('',3,(#58558,#58559,#58560,#58561,#58562,
#58563,#58564,#58565,#58566,#58567,#58568,#58569,#58570,#58571,#58572,#58573,
#58574,#58575,#58576,#58577,#58578,#58579),.UNSPECIFIED.,.F.,.F.,(4,3,3,
3,3,3,3,4),(-330.817659493786,-329.859650874599,-328.860076174979,-327.86050147536,
-326.860926775739,-325.861352076119,-324.8617773765,-324.534474186607),
 .UNSPECIFIED.);
#2656=B_SPLINE_CURVE_WITH_KNOTS('',3,(#58580,#58581,#58582,#58583,#58584,
#58585,#58586,#58587,#58588,#58589,#58590,#58591,#58592,#58593,#58594,#58595,
#58596,#58597,#58598,#58599,#58600,#58601),.UNSPECIFIED.,.F.,.F.,(4,3,3,
3,3,3,3,4),(321.565192472621,321.86305327764,322.86262797726,323.86220267688,
324.8617773765,325.86135207612,326.86092677574,327.8483777798),
 .UNSPECIFIED.);
#2657=B_SPLINE_CURVE_WITH_KNOTS('',3,(#58606,#58607,#58608,#58609,#58610,
#58611,#58612,#58613,#58614,#58615,#58616,#58617,#58618,#58619,#58620,#58621,
#58622,#58623,#58624,#58625,#58626,#58627,#58628,#58629,#58630),
 .UNSPECIFIED.,.F.,.F.,(4,3,3,3,3,3,3,3,4),(-337.100844800966,-336.85667377194,
-335.857099072319,-334.857524372699,-333.857949673079,-332.858374973459,
-331.858800273839,-330.859225574219,-330.817659493786),.UNSPECIFIED.);
#2658=B_SPLINE_CURVE_WITH_KNOTS('',3,(#58631,#58632,#58633,#58634,#58635,
#58636,#58637,#58638,#58639,#58640,#58641,#58642,#58643,#58644,#58645,#58646,
#58647,#58648,#58649,#58650,#58651,#58652,#58653,#58654,#58655),
 .UNSPECIFIED.,.F.,.F.,(4,3,3,3,3,3,3,3,4),(327.8483777798,327.86050147536,
328.86007617498,329.8596508746,330.85922557422,331.85880027384,332.85837497346,
333.85794967308,334.13156308698),.UNSPECIFIED.);
#2659=B_SPLINE_CURVE_WITH_KNOTS('',3,(#58660,#58661,#58662,#58663,#58664,
#58665,#58666,#58667,#58668,#58669,#58670,#58671,#58672,#58673,#58674,#58675,
#58676,#58677,#58678,#58679,#58680,#58681),.UNSPECIFIED.,.F.,.F.,(4,3,3,
3,3,3,3,4),(-343.384030108146,-342.854121969659,-341.85454727004,-340.854972570419,
-339.855397870799,-338.855823171179,-337.856248471559,-337.100844800966),
 .UNSPECIFIED.);
#2660=B_SPLINE_CURVE_WITH_KNOTS('',3,(#58682,#58683,#58684,#58685,#58686,
#58687,#58688,#58689,#58690,#58691,#58692,#58693,#58694,#58695,#58696,#58697,
#58698,#58699,#58700,#58701,#58702,#58703),.UNSPECIFIED.,.F.,.F.,(4,3,3,
3,3,3,3,4),(334.13156308698,334.8575243727,335.85709907232,336.85667377194,
337.85624847156,338.85582317118,339.8553978708,340.414748394159),
 .UNSPECIFIED.);
#2661=B_SPLINE_CURVE_WITH_KNOTS('',3,(#58708,#58709,#58710,#58711,#58712,
#58713,#58714,#58715,#58716,#58717,#58718,#58719,#58720,#58721,#58722,#58723,
#58724,#58725,#58726,#58727,#58728,#58729),.UNSPECIFIED.,.F.,.F.,(4,3,3,
3,3,3,3,4),(-349.667215415325,-348.851570167379,-347.851995467759,-346.852420768139,
-345.852846068519,-344.853271368899,-343.853696669279,-343.384030108146),
 .UNSPECIFIED.);
#2662=B_SPLINE_CURVE_WITH_KNOTS('',3,(#58730,#58731,#58732,#58733,#58734,
#58735,#58736,#58737,#58738,#58739,#58740,#58741,#58742,#58743,#58744,#58745,
#58746,#58747,#58748,#58749,#58750,#58751),.UNSPECIFIED.,.F.,.F.,(4,3,3,
3,3,3,3,4),(340.414748394159,340.85497257042,341.85454727004,342.85412196966,
343.85369666928,344.8532713689,345.85284606852,346.697933701339),
 .UNSPECIFIED.);
#2663=B_SPLINE_CURVE_WITH_KNOTS('',3,(#58756,#58757,#58758,#58759,#58760,
#58761,#58762,#58763,#58764,#58765,#58766,#58767,#58768,#58769,#58770,#58771,
#58772,#58773,#58774,#58775,#58776,#58777,#58778,#58779,#58780),
 .UNSPECIFIED.,.F.,.F.,(4,3,3,3,3,3,3,3,4),(-355.950400722505,-355.848593064719,
-354.849018365099,-353.849443665479,-352.849868965859,-351.850294266239,
-350.850719566619,-349.851144866999,-349.667215415325),.UNSPECIFIED.);
#2664=B_SPLINE_CURVE_WITH_KNOTS('',3,(#58781,#58782,#58783,#58784,#58785,
#58786,#58787,#58788,#58789,#58790,#58791,#58792,#58793,#58794,#58795,#58796,
#58797,#58798,#58799,#58800,#58801,#58802,#58803,#58804,#58805),
 .UNSPECIFIED.,.F.,.F.,(4,3,3,3,3,3,3,3,4),(346.697933701339,346.85242076814,
347.85199546776,348.85157016738,349.851144867,350.85071956662,351.85029426624,
352.84986896586,352.981119008518),.UNSPECIFIED.);
#2665=B_SPLINE_CURVE_WITH_KNOTS('',3,(#58810,#58811,#58812,#58813,#58814,
#58815,#58816,#58817,#58818,#58819,#58820,#58821,#58822,#58823,#58824,#58825,
#58826,#58827,#58828,#58829,#58830,#58831),.UNSPECIFIED.,.F.,.F.,(4,3,3,
3,3,3,3,4),(-362.233586029684,-361.846041262439,-360.846466562819,-359.846891863199,
-358.847317163579,-357.847742463959,-356.848167764339,-355.950400722505),
 .UNSPECIFIED.);
#2666=B_SPLINE_CURVE_WITH_KNOTS('',3,(#58832,#58833,#58834,#58835,#58836,
#58837,#58838,#58839,#58840,#58841,#58842,#58843,#58844,#58845,#58846,#58847,
#58848,#58849,#58850,#58851,#58852,#58853),.UNSPECIFIED.,.F.,.F.,(4,3,3,
3,3,3,3,4),(352.981119008518,353.84944366548,354.8490183651,355.84859306472,
356.84816776434,357.84774246396,358.84731716358,359.264304315698),
 .UNSPECIFIED.);
#2667=B_SPLINE_CURVE_WITH_KNOTS('',3,(#58858,#58859,#58860,#58861,#58862,
#58863,#58864,#58865,#58866,#58867,#58868,#58869,#58870,#58871,#58872,#58873,
#58874,#58875,#58876,#58877,#58878,#58879),.UNSPECIFIED.,.F.,.F.,(4,3,3,
3,3,3,3,4),(-368.516771336864,-367.843489460159,-366.843914760539,-365.844340060919,
-364.844765361299,-363.845190661679,-362.845615962059,-362.233586029684),
 .UNSPECIFIED.);
#2668=B_SPLINE_CURVE_WITH_KNOTS('',3,(#58880,#58881,#58882,#58883,#58884,
#58885,#58886,#58887,#58888,#58889,#58890,#58891,#58892,#58893,#58894,#58895,
#58896,#58897,#58898,#58899,#58900,#58901),.UNSPECIFIED.,.F.,.F.,(4,3,3,
3,3,3,3,4),(359.264304315698,359.8468918632,360.84646656282,361.84604126244,
362.84561596206,363.84519066168,364.8447653613,365.547489622878),
 .UNSPECIFIED.);
#2669=B_SPLINE_CURVE_WITH_KNOTS('',3,(#58906,#58907,#58908,#58909,#58910,
#58911,#58912,#58913,#58914,#58915,#58916,#58917,#58918,#58919,#58920,#58921,
#58922,#58923,#58924,#58925,#58926,#58927),.UNSPECIFIED.,.F.,.F.,(4,3,3,
3,3,3,3,4),(-374.799956644043,-373.840937657879,-372.841362958259,-371.841788258639,
-370.842213559019,-369.842638859399,-368.843064159779,-368.516771336864),
 .UNSPECIFIED.);
#2670=B_SPLINE_CURVE_WITH_KNOTS('',3,(#58928,#58929,#58930,#58931,#58932,
#58933,#58934,#58935,#58936,#58937,#58938,#58939,#58940,#58941,#58942,#58943,
#58944,#58945,#58946,#58947,#58948,#58949),.UNSPECIFIED.,.F.,.F.,(4,3,3,
3,3,3,3,4),(365.547489622878,365.84434006092,366.84391476054,367.84348946016,
368.84306415978,369.8426388594,370.84221355902,371.830674930057),
 .UNSPECIFIED.);
#2671=B_SPLINE_CURVE_WITH_KNOTS('',3,(#58954,#58955,#58956,#58957,#58958,
#58959,#58960,#58961,#58962,#58963,#58964,#58965,#58966,#58967,#58968,#58969,
#58970,#58971,#58972,#58973,#58974,#58975,#58976,#58977,#58978),
 .UNSPECIFIED.,.F.,.F.,(4,3,3,3,3,3,3,3,4),(-381.083141951223,-380.837960555219,
-379.838385855599,-378.838811155979,-377.839236456359,-376.839661756739,
-375.840087057119,-374.840512357499,-374.799956644043),.UNSPECIFIED.);
#2672=B_SPLINE_CURVE_WITH_KNOTS('',3,(#58979,#58980,#58981,#58982,#58983,
#58984,#58985,#58986,#58987,#58988,#58989,#58990,#58991,#58992,#58993,#58994,
#58995,#58996,#58997,#58998,#58999,#59000,#59001,#59002,#59003),
 .UNSPECIFIED.,.F.,.F.,(4,3,3,3,3,3,3,3,4),(371.830674930057,371.84178825864,
372.84136295826,373.84093765788,374.8405123575,375.84008705712,376.83966175674,
377.83923645636,378.113860237237),.UNSPECIFIED.);
#2673=B_SPLINE_CURVE_WITH_KNOTS('',3,(#59008,#59009,#59010,#59011,#59012,
#59013,#59014,#59015,#59016,#59017,#59018,#59019,#59020,#59021,#59022,#59023,
#59024,#59025,#59026,#59027,#59028,#59029),.UNSPECIFIED.,.F.,.F.,(4,3,3,
3,3,3,3,4),(-387.366327258402,-386.835408752939,-385.835834053319,-384.836259353699,
-383.836684654079,-382.837109954459,-381.837535254839,-381.083141951223),
 .UNSPECIFIED.);
#2674=B_SPLINE_CURVE_WITH_KNOTS('',3,(#59030,#59031,#59032,#59033,#59034,
#59035,#59036,#59037,#59038,#59039,#59040,#59041,#59042,#59043,#59044,#59045,
#59046,#59047,#59048,#59049,#59050,#59051),.UNSPECIFIED.,.F.,.F.,(4,3,3,
3,3,3,3,4),(378.113860237237,378.83881115598,379.8383858556,380.83796055522,
381.83753525484,382.83710995446,383.83668465408,384.397045544416),
 .UNSPECIFIED.);
#2675=B_SPLINE_CURVE_WITH_KNOTS('',3,(#59056,#59057,#59058,#59059,#59060,
#59061,#59062,#59063,#59064,#59065,#59066,#59067,#59068,#59069,#59070,#59071,
#59072,#59073,#59074,#59075,#59076,#59077),.UNSPECIFIED.,.F.,.F.,(4,3,3,
3,3,3,3,4),(-393.649512565582,-392.832856950659,-391.833282251039,-390.833707551419,
-389.834132851799,-388.834558152179,-387.834983452559,-387.366327258402),
 .UNSPECIFIED.);
#2676=B_SPLINE_CURVE_WITH_KNOTS('',3,(#59078,#59079,#59080,#59081,#59082,
#59083,#59084,#59085,#59086,#59087,#59088,#59089,#59090,#59091,#59092,#59093,
#59094,#59095,#59096,#59097,#59098,#59099),.UNSPECIFIED.,.F.,.F.,(4,3,3,
3,3,3,3,4),(384.397045544416,384.8362593537,385.83583405332,386.83540875294,
387.83498345256,388.83455815218,389.8341328518,390.680230851596),
 .UNSPECIFIED.);
#2677=B_SPLINE_CURVE_WITH_KNOTS('',3,(#59104,#59105,#59106,#59107,#59108,
#59109,#59110,#59111,#59112,#59113,#59114,#59115,#59116,#59117,#59118,#59119,
#59120,#59121,#59122,#59123,#59124,#59125,#59126,#59127,#59128),
 .UNSPECIFIED.,.F.,.F.,(4,3,3,3,3,3,3,3,4),(-399.932697872762,-399.829879847999,
-398.830305148379,-397.830730448759,-396.831155749139,-395.831581049519,
-394.832006349899,-393.832431650279,-393.649512565582),.UNSPECIFIED.);
#2678=B_SPLINE_CURVE_WITH_KNOTS('',3,(#59129,#59130,#59131,#59132,#59133,
#59134,#59135,#59136,#59137,#59138,#59139,#59140,#59141,#59142,#59143,#59144,
#59145,#59146,#59147,#59148,#59149,#59150,#59151,#59152,#59153),
 .UNSPECIFIED.,.F.,.F.,(4,3,3,3,3,3,3,3,4),(390.680230851596,390.83370755142,
391.83328225104,392.83285695066,393.83243165028,394.8320063499,395.83158104952,
396.83115574914,396.963416158775),.UNSPECIFIED.);
#2679=B_SPLINE_CURVE_WITH_KNOTS('',3,(#59158,#59159,#59160,#59161,#59162,
#59163,#59164,#59165,#59166,#59167,#59168,#59169,#59170,#59171,#59172,#59173,
#59174,#59175,#59176,#59177,#59178,#59179),.UNSPECIFIED.,.F.,.F.,(4,3,3,
3,3,3,3,4),(-406.215883179941,-405.827328045719,-404.827753346099,-403.828178646479,
-402.828603946859,-401.829029247239,-400.829454547619,-399.932697872762),
 .UNSPECIFIED.);
#2680=B_SPLINE_CURVE_WITH_KNOTS('',3,(#59180,#59181,#59182,#59183,#59184,
#59185,#59186,#59187,#59188,#59189,#59190,#59191,#59192,#59193,#59194,#59195,
#59196,#59197,#59198,#59199,#59200,#59201),.UNSPECIFIED.,.F.,.F.,(4,3,3,
3,3,3,3,4),(396.963416158775,397.83073044876,398.83030514838,399.829879848,
400.82945454762,401.82902924724,402.82860394686,403.246601465955),
 .UNSPECIFIED.);
#2681=B_SPLINE_CURVE_WITH_KNOTS('',3,(#59206,#59207,#59208,#59209,#59210,
#59211,#59212,#59213,#59214,#59215,#59216,#59217,#59218,#59219,#59220,#59221,
#59222,#59223,#59224,#59225,#59226,#59227),.UNSPECIFIED.,.F.,.F.,(4,3,3,
3,3,3,3,4),(-412.499068487121,-411.824776243439,-410.825201543819,-409.825626844199,
-408.826052144579,-407.826477444959,-406.826902745339,-406.215883179941),
 .UNSPECIFIED.);
#2682=B_SPLINE_CURVE_WITH_KNOTS('',3,(#59228,#59229,#59230,#59231,#59232,
#59233,#59234,#59235,#59236,#59237,#59238,#59239,#59240,#59241,#59242,#59243,
#59244,#59245,#59246,#59247,#59248,#59249),.UNSPECIFIED.,.F.,.F.,(4,3,3,
3,3,3,3,4),(403.246601465955,403.82817864648,404.8277533461,405.82732804572,
406.82690274534,407.82647744496,408.82605214458,409.529786773135),
 .UNSPECIFIED.);
#2683=B_SPLINE_CURVE_WITH_KNOTS('',3,(#59254,#59255,#59256,#59257,#59258,
#59259,#59260,#59261,#59262,#59263,#59264,#59265,#59266,#59267,#59268,#59269,
#59270,#59271,#59272,#59273,#59274,#59275),.UNSPECIFIED.,.F.,.F.,(4,3,3,
3,3,3,3,4),(-418.7822537943,-417.822224441159,-416.822649741539,-415.823075041919,
-414.823500342299,-413.823925642679,-412.824350943059,-412.499068487121),
 .UNSPECIFIED.);
#2684=B_SPLINE_CURVE_WITH_KNOTS('',3,(#59276,#59277,#59278,#59279,#59280,
#59281,#59282,#59283,#59284,#59285,#59286,#59287,#59288,#59289,#59290,#59291,
#59292,#59293,#59294,#59295,#59296,#59297),.UNSPECIFIED.,.F.,.F.,(4,3,3,
3,3,3,3,4),(409.529786773135,409.8256268442,410.82520154382,411.82477624344,
412.82435094306,413.82392564268,414.8235003423,415.812972080314),
 .UNSPECIFIED.);
#2685=B_SPLINE_CURVE_WITH_KNOTS('',3,(#59302,#59303,#59304,#59305,#59306,
#59307,#59308,#59309,#59310,#59311,#59312,#59313,#59314,#59315,#59316,#59317,
#59318,#59319,#59320,#59321,#59322,#59323,#59324,#59325,#59326),
 .UNSPECIFIED.,.F.,.F.,(4,3,3,3,3,3,3,3,4),(-425.06543910148,-424.819247338499,
-423.819672638879,-422.820097939259,-421.820523239639,-420.820948540019,
-419.821373840399,-418.821799140779,-418.7822537943),.UNSPECIFIED.);
#2686=B_SPLINE_CURVE_WITH_KNOTS('',3,(#59327,#59328,#59329,#59330,#59331,
#59332,#59333,#59334,#59335,#59336,#59337,#59338,#59339,#59340,#59341,#59342,
#59343,#59344,#59345,#59346,#59347,#59348,#59349,#59350,#59351),
 .UNSPECIFIED.,.F.,.F.,(4,3,3,3,3,3,3,3,4),(415.812972080314,415.82307504192,
416.82264974154,417.82222444116,418.82179914078,419.8213738404,420.82094854002,
421.82052323964,422.096157387494),.UNSPECIFIED.);
#2687=B_SPLINE_CURVE_WITH_KNOTS('',3,(#59356,#59357,#59358,#59359,#59360,
#59361,#59362,#59363,#59364,#59365,#59366,#59367,#59368,#59369,#59370,#59371,
#59372,#59373,#59374,#59375,#59376,#59377),.UNSPECIFIED.,.F.,.F.,(4,3,3,
3,3,3,3,4),(-431.348624408659,-430.816695536219,-429.817120836599,-428.817546136979,
-427.817971437359,-426.818396737739,-425.818822038119,-425.06543910148),
 .UNSPECIFIED.);
#2688=B_SPLINE_CURVE_WITH_KNOTS('',3,(#59378,#59379,#59380,#59381,#59382,
#59383,#59384,#59385,#59386,#59387,#59388,#59389,#59390,#59391,#59392,#59393,
#59394,#59395,#59396,#59397,#59398,#59399),.UNSPECIFIED.,.F.,.F.,(4,3,3,
3,3,3,3,4),(422.096157387494,422.82009793926,423.81967263888,424.8192473385,
425.81882203812,426.81839673774,427.81797143736,428.379342694673),
 .UNSPECIFIED.);
#2689=B_SPLINE_CURVE_WITH_KNOTS('',3,(#59405,#59406,#59407,#59408,#59409),
 .UNSPECIFIED.,.F.,.F.,(4,1,4),(442.964564156161,443.432209983341,444.357761408881),
 .UNSPECIFIED.);
#2690=B_SPLINE_CURVE_WITH_KNOTS('',3,(#59412,#59413,#59414,#59415),
 .UNSPECIFIED.,.F.,.F.,(4,4),(442.964564156161,443.117030489009),
 .UNSPECIFIED.);
#2691=B_SPLINE_CURVE_WITH_KNOTS('',3,(#59420,#59421,#59422,#59423,#59424,
#59425,#59426,#59427,#59428,#59429),.UNSPECIFIED.,.F.,.F.,(4,1,1,1,1,1,
1,4),(436.681378848981,437.434761785621,438.434336485241,439.433911184861,
440.433485884481,441.433060584101,442.432635283721,442.964564156161),
 .UNSPECIFIED.);
#2692=B_SPLINE_CURVE_WITH_KNOTS('',3,(#59430,#59431,#59432,#59433,#59434,
#59435,#59436,#59437,#59438,#59439),.UNSPECIFIED.,.F.,.F.,(4,1,1,1,1,1,
1,4),(436.681378848981,437.119582291289,438.119156990909,439.118731690529,
440.118306390149,441.117881089769,442.117455789389,442.964564156161),
 .UNSPECIFIED.);
#2693=B_SPLINE_CURVE_WITH_KNOTS('',3,(#59444,#59445,#59446,#59447,#59448,
#59449,#59450,#59451,#59452,#59453,#59454),.UNSPECIFIED.,.F.,.F.,(4,1,1,
1,1,1,1,1,4),(430.398193541801,430.437738888281,431.437313587901,432.436888287521,
433.436462987141,434.436037686761,435.435612386381,436.435187086001,436.681378848981),
 .UNSPECIFIED.);
#2694=B_SPLINE_CURVE_WITH_KNOTS('',3,(#59455,#59456,#59457,#59458,#59459,
#59460,#59461,#59462,#59463,#59464),.UNSPECIFIED.,.F.,.F.,(4,1,1,1,1,1,
1,4),(430.398193541802,431.122134093569,432.121708793189,433.121283492809,
434.120858192429,435.120432892049,436.120007591669,436.681378848981),
 .UNSPECIFIED.);
#2695=B_SPLINE_CURVE_WITH_KNOTS('',3,(#59469,#59470,#59471,#59472,#59473,
#59474,#59475,#59476,#59477,#59478),.UNSPECIFIED.,.F.,.F.,(4,1,1,1,1,1,
1,4),(424.115008234622,424.440290690561,425.439865390181,426.439440089801,
427.439014789421,428.438589489041,429.438164188661,430.398193541801),
 .UNSPECIFIED.);
#2696=B_SPLINE_CURVE_WITH_KNOTS('',3,(#59479,#59480,#59481,#59482,#59483,
#59484,#59485,#59486,#59487,#59488,#59489),.UNSPECIFIED.,.F.,.F.,(4,1,1,
1,1,1,1,1,4),(424.115008234622,424.125111196229,425.124685895849,426.124260595469,
427.123835295089,428.123409994709,429.122984694329,430.122559393949,430.398193541802),
 .UNSPECIFIED.);
#2697=B_SPLINE_CURVE_WITH_KNOTS('',3,(#59494,#59495,#59496,#59497,#59498,
#59499,#59500,#59501,#59502,#59503),.UNSPECIFIED.,.F.,.F.,(4,1,1,1,1,1,
1,4),(417.831822927442,418.442842492841,419.442417192461,420.441991892081,
421.441566591701,422.441141291321,423.440715990941,424.115008234622),
 .UNSPECIFIED.);
#2698=B_SPLINE_CURVE_WITH_KNOTS('',3,(#59504,#59505,#59506,#59507,#59508,
#59509,#59510,#59511,#59512,#59513),.UNSPECIFIED.,.F.,.F.,(4,1,1,1,1,1,
1,4),(417.831822927443,418.127662998509,419.127237698129,420.126812397749,
421.126387097369,422.125961796989,423.125536496609,424.115008234622),
 .UNSPECIFIED.);
#2699=B_SPLINE_CURVE_WITH_KNOTS('',3,(#59518,#59519,#59520,#59521,#59522,
#59523,#59524,#59525,#59526,#59527),.UNSPECIFIED.,.F.,.F.,(4,1,1,1,1,1,
1,4),(411.548637620263,412.445394295121,413.444968994741,414.444543694361,
415.444118393981,416.443693093601,417.443267793221,417.831822927442),
 .UNSPECIFIED.);
#2700=B_SPLINE_CURVE_WITH_KNOTS('',3,(#59528,#59529,#59530,#59531,#59532,
#59533,#59534,#59535,#59536,#59537),.UNSPECIFIED.,.F.,.F.,(4,1,1,1,1,1,
1,4),(411.548637620263,412.130214800789,413.129789500409,414.129364200029,
415.128938899649,416.128513599269,417.128088298889,417.831822927443),
 .UNSPECIFIED.);
#2701=B_SPLINE_CURVE_WITH_KNOTS('',3,(#59542,#59543,#59544,#59545,#59546,
#59547,#59548,#59549,#59550,#59551,#59552),.UNSPECIFIED.,.F.,.F.,(4,1,1,
1,1,1,1,1,4),(405.265452313083,405.448371397781,406.447946097401,407.447520797021,
408.447095496641,409.446670196261,410.446244895881,411.445819595501,411.548637620263),
 .UNSPECIFIED.);
#2702=B_SPLINE_CURVE_WITH_KNOTS('',3,(#59553,#59554,#59555,#59556,#59557,
#59558,#59559,#59560,#59561,#59562),.UNSPECIFIED.,.F.,.F.,(4,1,1,1,1,1,
1,4),(405.265452313083,406.132766603069,407.132341302689,408.131916002309,
409.131490701929,410.131065401549,411.130640101169,411.548637620263),
 .UNSPECIFIED.);
#2703=B_SPLINE_CURVE_WITH_KNOTS('',3,(#59567,#59568,#59569,#59570,#59571,
#59572,#59573,#59574,#59575,#59576),.UNSPECIFIED.,.F.,.F.,(4,1,1,1,1,1,
1,4),(398.982267005904,399.450923200061,400.450497899681,401.450072599301,
402.449647298921,403.449221998541,404.448796698161,405.265452313083),
 .UNSPECIFIED.);
#2704=B_SPLINE_CURVE_WITH_KNOTS('',3,(#59577,#59578,#59579,#59580,#59581,
#59582,#59583,#59584,#59585,#59586,#59587),.UNSPECIFIED.,.F.,.F.,(4,1,1,
1,1,1,1,1,4),(398.982267005904,399.135743705729,400.135318405349,401.134893104969,
402.134467804589,403.134042504209,404.133617203829,405.133191903449,405.265452313083),
 .UNSPECIFIED.);
#2705=B_SPLINE_CURVE_WITH_KNOTS('',3,(#59592,#59593,#59594,#59595,#59596,
#59597,#59598,#59599,#59600,#59601),.UNSPECIFIED.,.F.,.F.,(4,1,1,1,1,1,
1,4),(392.699081698724,393.453475002341,394.453049701961,395.452624401581,
396.452199101201,397.451773800821,398.451348500441,398.982267005904),
 .UNSPECIFIED.);
#2706=B_SPLINE_CURVE_WITH_KNOTS('',3,(#59602,#59603,#59604,#59605,#59606,
#59607,#59608,#59609,#59610,#59611),.UNSPECIFIED.,.F.,.F.,(4,1,1,1,1,1,
1,4),(392.699081698724,393.138295508009,394.137870207629,395.137444907249,
396.137019606869,397.136594306489,398.136169006109,398.982267005904),
 .UNSPECIFIED.);
#2707=B_SPLINE_CURVE_WITH_KNOTS('',3,(#59616,#59617,#59618,#59619,#59620,
#59621,#59622,#59623,#59624,#59625,#59626),.UNSPECIFIED.,.F.,.F.,(4,1,1,
1,1,1,1,1,4),(386.415896391544,386.456452105001,387.456026804621,388.455601504241,
389.455176203861,390.454750903481,391.454325603101,392.453900302721,392.699081698724),
 .UNSPECIFIED.);
#2708=B_SPLINE_CURVE_WITH_KNOTS('',3,(#59627,#59628,#59629,#59630,#59631,
#59632,#59633,#59634,#59635,#59636),.UNSPECIFIED.,.F.,.F.,(4,1,1,1,1,1,
1,4),(386.415896391545,387.140847310289,388.140422009909,389.139996709529,
390.139571409149,391.139146108769,392.138720808389,392.699081698724),
 .UNSPECIFIED.);
#2709=B_SPLINE_CURVE_WITH_KNOTS('',3,(#59641,#59642,#59643,#59644,#59645,
#59646,#59647,#59648,#59649,#59650),.UNSPECIFIED.,.F.,.F.,(4,1,1,1,1,1,
1,4),(380.132711084365,380.459003907281,381.458578606901,382.458153306521,
383.457728006141,384.457302705761,385.456877405381,386.415896391544),
 .UNSPECIFIED.);
#2710=B_SPLINE_CURVE_WITH_KNOTS('',3,(#59651,#59652,#59653,#59654,#59655,
#59656,#59657,#59658,#59659,#59660,#59661),.UNSPECIFIED.,.F.,.F.,(4,1,1,
1,1,1,1,1,4),(380.132711084365,380.143824412949,381.143399112569,382.142973812189,
383.142548511809,384.142123211429,385.141697911049,386.141272610669,386.415896391545),
 .UNSPECIFIED.);
#2711=B_SPLINE_CURVE_WITH_KNOTS('',3,(#59666,#59667,#59668,#59669,#59670,
#59671,#59672,#59673,#59674,#59675),.UNSPECIFIED.,.F.,.F.,(4,1,1,1,1,1,
1,4),(373.849525777185,374.461555709561,375.461130409181,376.460705108801,
377.460279808421,378.459854508041,379.459429207661,380.132711084365),
 .UNSPECIFIED.);
#2712=B_SPLINE_CURVE_WITH_KNOTS('',3,(#59676,#59677,#59678,#59679,#59680,
#59681,#59682,#59683,#59684,#59685),.UNSPECIFIED.,.F.,.F.,(4,1,1,1,1,1,
1,4),(373.849525777185,374.146376215229,375.145950914849,376.145525614469,
377.145100314089,378.144675013709,379.144249713329,380.132711084365),
 .UNSPECIFIED.);
#2713=B_SPLINE_CURVE_WITH_KNOTS('',3,(#59690,#59691,#59692,#59693,#59694,
#59695,#59696,#59697,#59698,#59699),.UNSPECIFIED.,.F.,.F.,(4,1,1,1,1,1,
1,4),(367.566340470006,368.464107511841,369.463682211461,370.463256911081,
371.462831610701,372.462406310321,373.461981009941,373.849525777185),
 .UNSPECIFIED.);
#2714=B_SPLINE_CURVE_WITH_KNOTS('',3,(#59700,#59701,#59702,#59703,#59704,
#59705,#59706,#59707,#59708,#59709),.UNSPECIFIED.,.F.,.F.,(4,1,1,1,1,1,
1,4),(367.566340470006,368.148928017509,369.148502717129,370.148077416749,
371.147652116369,372.147226815989,373.146801515609,373.849525777185),
 .UNSPECIFIED.);
#2715=B_SPLINE_CURVE_WITH_KNOTS('',3,(#59714,#59715,#59716,#59717,#59718,
#59719,#59720,#59721,#59722,#59723,#59724),.UNSPECIFIED.,.F.,.F.,(4,1,1,
1,1,1,1,1,4),(361.283155162826,361.467084614501,362.466659314121,363.466234013741,
364.465808713361,365.465383412981,366.464958112601,367.464532812221,367.566340470006),
 .UNSPECIFIED.);
#2716=B_SPLINE_CURVE_WITH_KNOTS('',3,(#59725,#59726,#59727,#59728,#59729,
#59730,#59731,#59732,#59733,#59734),.UNSPECIFIED.,.F.,.F.,(4,1,1,1,1,1,
1,4),(361.283155162826,362.151479819789,363.151054519409,364.150629219029,
365.150203918649,366.149778618269,367.149353317889,367.566340470006),
 .UNSPECIFIED.);
#2717=B_SPLINE_CURVE_WITH_KNOTS('',3,(#59739,#59740,#59741,#59742,#59743,
#59744,#59745,#59746,#59747,#59748),.UNSPECIFIED.,.F.,.F.,(4,1,1,1,1,1,
1,4),(354.999969855647,355.469636416781,356.469211116401,357.468785816021,
358.468360515641,359.467935215261,360.467509914881,361.283155162826),
 .UNSPECIFIED.);
#2718=B_SPLINE_CURVE_WITH_KNOTS('',3,(#59749,#59750,#59751,#59752,#59753,
#59754,#59755,#59756,#59757,#59758,#59759),.UNSPECIFIED.,.F.,.F.,(4,1,1,
1,1,1,1,1,4),(354.999969855647,355.154456922449,356.154031622069,357.153606321689,
358.153181021309,359.152755720929,360.152330420549,361.151905120169,361.283155162826),
 .UNSPECIFIED.);
#2719=B_SPLINE_CURVE_WITH_KNOTS('',3,(#59764,#59765,#59766,#59767,#59768,
#59769,#59770,#59771,#59772,#59773),.UNSPECIFIED.,.F.,.F.,(4,1,1,1,1,1,
1,4),(348.716784548467,349.472188219061,350.471762918681,351.471337618301,
352.470912317921,353.470487017541,354.470061717161,354.999969855647),
 .UNSPECIFIED.);
#2720=B_SPLINE_CURVE_WITH_KNOTS('',3,(#59774,#59775,#59776,#59777,#59778,
#59779,#59780,#59781,#59782,#59783),.UNSPECIFIED.,.F.,.F.,(4,1,1,1,1,1,
1,4),(348.716784548467,349.157008724729,350.156583424349,351.156158123969,
352.155732823589,353.155307523209,354.154882222829,354.999969855647),
 .UNSPECIFIED.);
#2721=B_SPLINE_CURVE_WITH_KNOTS('',3,(#59788,#59789,#59790,#59791,#59792,
#59793,#59794,#59795,#59796,#59797,#59798),.UNSPECIFIED.,.F.,.F.,(4,1,1,
1,1,1,1,1,4),(342.433599241287,342.475165321721,343.474740021341,344.474314720961,
345.473889420581,346.473464120201,347.473038819821,348.472613519441,348.716784548467),
 .UNSPECIFIED.);
#2722=B_SPLINE_CURVE_WITH_KNOTS('',3,(#59799,#59800,#59801,#59802,#59803,
#59804,#59805,#59806,#59807,#59808),.UNSPECIFIED.,.F.,.F.,(4,1,1,1,1,1,
1,4),(342.433599241288,343.159560527009,344.159135226629,345.158709926249,
346.158284625869,347.157859325489,348.157434025109,348.716784548467),
 .UNSPECIFIED.);
#2723=B_SPLINE_CURVE_WITH_KNOTS('',3,(#59813,#59814,#59815,#59816,#59817,
#59818,#59819,#59820,#59821,#59822),.UNSPECIFIED.,.F.,.F.,(4,1,1,1,1,1,
1,4),(336.150413934108,336.477717124001,337.477291823621,338.476866523241,
339.476441222861,340.476015922481,341.475590622101,342.433599241287),
 .UNSPECIFIED.);
#2724=B_SPLINE_CURVE_WITH_KNOTS('',3,(#59823,#59824,#59825,#59826,#59827,
#59828,#59829,#59830,#59831,#59832,#59833),.UNSPECIFIED.,.F.,.F.,(4,1,1,
1,1,1,1,1,4),(336.150413934108,336.162537629669,337.162112329289,338.161687028909,
339.161261728529,340.160836428149,341.160411127769,342.159985827389,342.433599241288),
 .UNSPECIFIED.);
#2725=B_SPLINE_CURVE_WITH_KNOTS('',3,(#59838,#59839,#59840,#59841,#59842,
#59843,#59844,#59845,#59846,#59847),.UNSPECIFIED.,.F.,.F.,(4,1,1,1,1,1,
1,4),(329.867228626928,330.480268926281,331.479843625901,332.479418325521,
333.478993025141,334.478567724761,335.478142424381,336.150413934108),
 .UNSPECIFIED.);
#2726=B_SPLINE_CURVE_WITH_KNOTS('',3,(#59848,#59849,#59850,#59851,#59852,
#59853,#59854,#59855,#59856,#59857),.UNSPECIFIED.,.F.,.F.,(4,1,1,1,1,1,
1,4),(329.867228626929,330.165089431949,331.164664131569,332.164238831189,
333.163813530809,334.163388230429,335.162962930049,336.150413934108),
 .UNSPECIFIED.);
#2727=B_SPLINE_CURVE_WITH_KNOTS('',3,(#59862,#59863,#59864,#59865,#59866,
#59867,#59868,#59869,#59870,#59871),.UNSPECIFIED.,.F.,.F.,(4,1,1,1,1,1,
1,4),(323.584043319749,324.482820728561,325.482395428181,326.481970127801,
327.481544827421,328.481119527041,329.480694226661,329.867228626928),
 .UNSPECIFIED.);
#2728=B_SPLINE_CURVE_WITH_KNOTS('',3,(#59872,#59873,#59874,#59875,#59876,
#59877,#59878,#59879,#59880,#59881),.UNSPECIFIED.,.F.,.F.,(4,1,1,1,1,1,
1,4),(323.584043319749,324.167641234229,325.167215933849,326.166790633469,
327.166365333089,328.165940032709,329.165514732329,329.867228626929),
 .UNSPECIFIED.);
#2729=B_SPLINE_CURVE_WITH_KNOTS('',3,(#59886,#59887,#59888,#59889,#59890,
#59891,#59892,#59893,#59894,#59895,#59896),.UNSPECIFIED.,.F.,.F.,(4,1,1,
1,1,1,1,1,4),(317.300858012569,317.485797831221,318.485372530841,319.484947230461,
320.484521930081,321.484096629701,322.483671329321,323.483246028941,323.584043319749),
 .UNSPECIFIED.);
#2730=B_SPLINE_CURVE_WITH_KNOTS('',3,(#59897,#59898,#59899,#59900,#59901,
#59902,#59903,#59904,#59905,#59906),.UNSPECIFIED.,.F.,.F.,(4,1,1,1,1,1,
1,4),(317.300858012569,318.170193036509,319.169767736129,320.169342435749,
321.168917135369,322.168491834989,323.168066534609,323.584043319749),
 .UNSPECIFIED.);
#2731=B_SPLINE_CURVE_WITH_KNOTS('',3,(#59911,#59912,#59913,#59914,#59915,
#59916,#59917,#59918,#59919,#59920),.UNSPECIFIED.,.F.,.F.,(4,1,1,1,1,1,
1,4),(311.01767270539,311.488349633501,312.487924333121,313.487499032741,
314.487073732361,315.486648431981,316.486223131601,317.300858012569),
 .UNSPECIFIED.);
#2732=B_SPLINE_CURVE_WITH_KNOTS('',3,(#59921,#59922,#59923,#59924,#59925,
#59926,#59927,#59928,#59929,#59930,#59931),.UNSPECIFIED.,.F.,.F.,(4,1,1,
1,1,1,1,1,4),(311.01767270539,311.173170139169,312.172744838789,313.172319538409,
314.171894238029,315.171468937649,316.171043637269,317.170618336889,317.300858012569),
 .UNSPECIFIED.);
#2733=B_SPLINE_CURVE_WITH_KNOTS('',3,(#59936,#59937,#59938,#59939,#59940,
#59941,#59942,#59943,#59944,#59945),.UNSPECIFIED.,.F.,.F.,(4,1,1,1,1,1,
1,4),(304.73448739821,305.490901435781,306.490476135401,307.490050835021,
308.489625534641,309.489200234261,310.488774933881,311.01767270539),
 .UNSPECIFIED.);
#2734=B_SPLINE_CURVE_WITH_KNOTS('',3,(#59946,#59947,#59948,#59949,#59950,
#59951,#59952,#59953,#59954,#59955),.UNSPECIFIED.,.F.,.F.,(4,1,1,1,1,1,
1,4),(304.73448739821,305.175721941449,306.175296641069,307.174871340689,
308.174446040309,309.174020739929,310.173595439549,311.01767270539),
 .UNSPECIFIED.);
#2735=B_SPLINE_CURVE_WITH_KNOTS('',3,(#59960,#59961,#59962,#59963,#59964,
#59965,#59966,#59967,#59968,#59969,#59970),.UNSPECIFIED.,.F.,.F.,(4,1,1,
1,1,1,1,1,4),(298.451302091031,298.493878538441,299.493453238061,300.493027937681,
301.492602637301,302.492177336921,303.491752036541,304.491326736161,304.73448739821),
 .UNSPECIFIED.);
#2736=B_SPLINE_CURVE_WITH_KNOTS('',3,(#59971,#59972,#59973,#59974,#59975,
#59976,#59977,#59978,#59979,#59980),.UNSPECIFIED.,.F.,.F.,(4,1,1,1,1,1,
1,4),(298.451302091031,299.178273743729,300.177848443349,301.177423142969,
302.176997842589,303.176572542209,304.176147241829,304.73448739821),
 .UNSPECIFIED.);
#2737=B_SPLINE_CURVE_WITH_KNOTS('',3,(#59985,#59986,#59987,#59988,#59989,
#59990,#59991,#59992,#59993,#59994),.UNSPECIFIED.,.F.,.F.,(4,1,1,1,1,1,
1,4),(292.168116783851,292.496430340721,293.496005040341,294.495579739961,
295.495154439581,296.494729139201,297.494303838821,298.451302091031),
 .UNSPECIFIED.);
#2738=B_SPLINE_CURVE_WITH_KNOTS('',3,(#59995,#59996,#59997,#59998,#59999,
#60000,#60001,#60002,#60003,#60004,#60005),.UNSPECIFIED.,.F.,.F.,(4,1,1,
1,1,1,1,1,4),(292.168116783851,292.181250846389,293.180825546009,294.180400245629,
295.179974945249,296.179549644869,297.179124344489,298.178699044109,298.451302091031),
 .UNSPECIFIED.);
#2739=B_SPLINE_CURVE_WITH_KNOTS('',3,(#60010,#60011,#60012,#60013,#60014,
#60015,#60016,#60017,#60018,#60019),.UNSPECIFIED.,.F.,.F.,(4,1,1,1,1,1,
1,4),(285.884931476671,286.498982143001,287.498556842621,288.498131542241,
289.497706241861,290.497280941481,291.496855641101,292.168116783851),
 .UNSPECIFIED.);
#2740=B_SPLINE_CURVE_WITH_KNOTS('',3,(#60020,#60021,#60022,#60023,#60024,
#60025,#60026,#60027,#60028,#60029),.UNSPECIFIED.,.F.,.F.,(4,1,1,1,1,1,
1,4),(285.884931476672,286.183802648669,287.183377348289,288.182952047909,
289.182526747529,290.182101447149,291.181676146769,292.168116783851),
 .UNSPECIFIED.);
#2741=B_SPLINE_CURVE_WITH_KNOTS('',3,(#60034,#60035,#60036,#60037,#60038,
#60039,#60040,#60041,#60042,#60043),.UNSPECIFIED.,.F.,.F.,(4,1,1,1,1,1,
1,4),(279.601746169492,280.501533945281,281.501108644901,282.500683344521,
283.500258044141,284.499832743761,285.499407443381,285.884931476671),
 .UNSPECIFIED.);
#2742=B_SPLINE_CURVE_WITH_KNOTS('',3,(#60044,#60045,#60046,#60047,#60048,
#60049,#60050,#60051,#60052,#60053),.UNSPECIFIED.,.F.,.F.,(4,1,1,1,1,1,
1,4),(279.601746169492,280.186354450949,281.185929150569,282.185503850189,
283.185078549809,284.184653249429,285.184227949049,285.884931476672),
 .UNSPECIFIED.);
#2743=B_SPLINE_CURVE_WITH_KNOTS('',3,(#60058,#60059,#60060,#60061,#60062,
#60063,#60064,#60065,#60066,#60067,#60068),.UNSPECIFIED.,.F.,.F.,(4,1,1,
1,1,1,1,1,4),(273.318560862312,273.504511047941,274.504085747561,275.503660447181,
276.503235146801,277.502809846421,278.502384546041,279.501959245661,279.601746169492),
 .UNSPECIFIED.);
#2744=B_SPLINE_CURVE_WITH_KNOTS('',3,(#60069,#60070,#60071,#60072,#60073,
#60074,#60075,#60076,#60077,#60078),.UNSPECIFIED.,.F.,.F.,(4,1,1,1,1,1,
1,4),(273.318560862312,274.188906253229,275.188480952849,276.188055652469,
277.187630352089,278.187205051709,279.186779751329,279.601746169492),
 .UNSPECIFIED.);
#2745=B_SPLINE_CURVE_WITH_KNOTS('',3,(#60083,#60084,#60085,#60086,#60087,
#60088,#60089,#60090,#60091,#60092),.UNSPECIFIED.,.F.,.F.,(4,1,1,1,1,1,
1,4),(267.035375555133,267.507062850221,268.506637549841,269.506212249461,
270.505786949081,271.505361648701,272.504936348321,273.318560862312),
 .UNSPECIFIED.);
#2746=B_SPLINE_CURVE_WITH_KNOTS('',3,(#60093,#60094,#60095,#60096,#60097,
#60098,#60099,#60100,#60101,#60102,#60103),.UNSPECIFIED.,.F.,.F.,(4,1,1,
1,1,1,1,1,4),(267.035375555133,267.191883355889,268.191458055509,269.191032755129,
270.190607454749,271.190182154369,272.189756853989,273.189331553609,273.318560862312),
 .UNSPECIFIED.);
#2747=B_SPLINE_CURVE_WITH_KNOTS('',3,(#60108,#60109,#60110,#60111,#60112,
#60113,#60114,#60115,#60116,#60117),.UNSPECIFIED.,.F.,.F.,(4,1,1,1,1,1,
1,4),(260.752190247953,261.509614652501,262.509189352121,263.508764051741,
264.508338751361,265.507913450981,266.507488150601,267.035375555133),
 .UNSPECIFIED.);
#2748=B_SPLINE_CURVE_WITH_KNOTS('',3,(#60118,#60119,#60120,#60121,#60122,
#60123,#60124,#60125,#60126,#60127),.UNSPECIFIED.,.F.,.F.,(4,1,1,1,1,1,
1,4),(260.752190247953,261.194435158169,262.194009857789,263.193584557409,
264.193159257029,265.192733956649,266.192308656269,267.035375555133),
 .UNSPECIFIED.);
#2749=B_SPLINE_CURVE_WITH_KNOTS('',3,(#60132,#60133,#60134,#60135,#60136,
#60137,#60138,#60139,#60140,#60141,#60142),.UNSPECIFIED.,.F.,.F.,(4,1,1,
1,1,1,1,1,4),(254.469004940774,254.512591755161,255.512166454781,256.511741154401,
257.511315854021,258.510890553641,259.510465253261,260.510039952881,260.752190247953),
 .UNSPECIFIED.);
#2750=B_SPLINE_CURVE_WITH_KNOTS('',3,(#60143,#60144,#60145,#60146,#60147,
#60148,#60149,#60150,#60151,#60152),.UNSPECIFIED.,.F.,.F.,(4,1,1,1,1,1,
1,4),(254.469004940774,255.196986960449,256.196561660069,257.196136359689,
258.195711059309,259.195285758929,260.194860458549,260.752190247953),
 .UNSPECIFIED.);
#2751=B_SPLINE_CURVE_WITH_KNOTS('',3,(#60157,#60158,#60159,#60160,#60161,
#60162,#60163,#60164,#60165,#60166),.UNSPECIFIED.,.F.,.F.,(4,1,1,1,1,1,
1,4),(248.185819633594,248.515143557441,249.514718257061,250.514292956681,
251.513867656301,252.513442355921,253.513017055541,254.469004940774),
 .UNSPECIFIED.);
#2752=B_SPLINE_CURVE_WITH_KNOTS('',3,(#60167,#60168,#60169,#60170,#60171,
#60172,#60173,#60174,#60175,#60176,#60177),.UNSPECIFIED.,.F.,.F.,(4,1,1,
1,1,1,1,1,4),(248.185819633594,248.199964063109,249.199538762729,250.199113462349,
251.198688161969,252.198262861589,253.197837561209,254.197412260829,254.469004940774),
 .UNSPECIFIED.);
#2753=B_SPLINE_CURVE_WITH_KNOTS('',3,(#60182,#60183,#60184,#60185,#60186,
#60187,#60188,#60189,#60190,#60191),.UNSPECIFIED.,.F.,.F.,(4,1,1,1,1,1,
1,4),(241.902634326414,242.517695359721,243.517270059341,244.516844758961,
245.516419458581,246.515994158201,247.515568857821,248.185819633594),
 .UNSPECIFIED.);
#2754=B_SPLINE_CURVE_WITH_KNOTS('',3,(#60192,#60193,#60194,#60195,#60196,
#60197,#60198,#60199,#60200,#60201),.UNSPECIFIED.,.F.,.F.,(4,1,1,1,1,1,
1,4),(241.902634326415,242.202515865389,243.202090565009,244.201665264629,
245.201239964249,246.200814663869,247.200389363489,248.185819633594),
 .UNSPECIFIED.);
#2755=B_SPLINE_CURVE_WITH_KNOTS('',3,(#60206,#60207,#60208,#60209,#60210,
#60211,#60212,#60213,#60214,#60215),.UNSPECIFIED.,.F.,.F.,(4,1,1,1,1,1,
1,4),(235.619449019235,236.520247162001,237.519821861621,238.519396561241,
239.518971260861,240.518545960481,241.518120660101,241.902634326414),
 .UNSPECIFIED.);
#2756=B_SPLINE_CURVE_WITH_KNOTS('',3,(#60216,#60217,#60218,#60219,#60220,
#60221,#60222,#60223,#60224,#60225),.UNSPECIFIED.,.F.,.F.,(4,1,1,1,1,1,
1,4),(235.619449019235,236.205067667669,237.204642367289,238.204217066909,
239.203791766529,240.203366466149,241.202941165769,241.902634326415),
 .UNSPECIFIED.);
#2757=B_SPLINE_CURVE_WITH_KNOTS('',3,(#60230,#60231,#60232,#60233,#60234,
#60235,#60236,#60237,#60238,#60239,#60240),.UNSPECIFIED.,.F.,.F.,(4,1,1,
1,1,1,1,1,4),(229.336263712055,229.523224264661,230.522798964281,231.522373663901,
232.521948363521,233.521523063141,234.521097762761,235.520672462381,235.619449019235),
 .UNSPECIFIED.);
#2758=B_SPLINE_CURVE_WITH_KNOTS('',3,(#60241,#60242,#60243,#60244,#60245,
#60246,#60247,#60248,#60249,#60250),.UNSPECIFIED.,.F.,.F.,(4,1,1,1,1,1,
1,4),(229.336263712056,230.207619469949,231.207194169569,232.206768869189,
233.206343568809,234.205918268429,235.205492968049,235.619449019235),
 .UNSPECIFIED.);
#2759=B_SPLINE_CURVE_WITH_KNOTS('',3,(#60255,#60256,#60257,#60258,#60259,
#60260,#60261,#60262,#60263,#60264),.UNSPECIFIED.,.F.,.F.,(4,1,1,1,1,1,
1,4),(223.053078404876,223.525776066941,224.525350766561,225.524925466181,
226.524500165801,227.524074865421,228.523649565041,229.336263712055),
 .UNSPECIFIED.);
#2760=B_SPLINE_CURVE_WITH_KNOTS('',3,(#60265,#60266,#60267,#60268,#60269,
#60270,#60271,#60272,#60273,#60274,#60275),.UNSPECIFIED.,.F.,.F.,(4,1,1,
1,1,1,1,1,4),(223.053078404876,223.210596572609,224.210171272229,225.209745971849,
226.209320671469,227.208895371089,228.208470070709,229.208044770329,229.336263712056),
 .UNSPECIFIED.);
#2761=B_SPLINE_CURVE_WITH_KNOTS('',3,(#60280,#60281,#60282,#60283,#60284,
#60285,#60286,#60287,#60288,#60289),.UNSPECIFIED.,.F.,.F.,(4,1,1,1,1,1,
1,4),(216.769893097696,217.528327869221,218.527902568841,219.527477268461,
220.527051968081,221.526626667701,222.526201367321,223.053078404876),
 .UNSPECIFIED.);
#2762=B_SPLINE_CURVE_WITH_KNOTS('',3,(#60290,#60291,#60292,#60293,#60294,
#60295,#60296,#60297,#60298,#60299),.UNSPECIFIED.,.F.,.F.,(4,1,1,1,1,1,
1,4),(216.769893097696,217.213148374889,218.212723074509,219.212297774129,
220.211872473749,221.211447173369,222.211021872989,223.053078404876),
 .UNSPECIFIED.);
#2763=B_SPLINE_CURVE_WITH_KNOTS('',3,(#60304,#60305,#60306,#60307,#60308,
#60309,#60310,#60311,#60312,#60313,#60314),.UNSPECIFIED.,.F.,.F.,(4,1,1,
1,1,1,1,1,4),(210.486707790517,210.531304971881,211.530879671501,212.530454371121,
213.530029070741,214.529603770361,215.529178469981,216.528753169601,216.769893097696),
 .UNSPECIFIED.);
#2764=B_SPLINE_CURVE_WITH_KNOTS('',3,(#60315,#60316,#60317,#60318,#60319,
#60320,#60321,#60322,#60323,#60324),.UNSPECIFIED.,.F.,.F.,(4,1,1,1,1,1,
1,4),(210.486707790517,211.215700177169,212.215274876789,213.214849576409,
214.214424276029,215.213998975649,216.213573675269,216.769893097696),
 .UNSPECIFIED.);
#2765=B_SPLINE_CURVE_WITH_KNOTS('',3,(#60329,#60330,#60331,#60332,#60333,
#60334,#60335,#60336,#60337,#60338),.UNSPECIFIED.,.F.,.F.,(4,1,1,1,1,1,
1,4),(204.203522483337,204.533856774161,205.533431473781,206.533006173401,
207.532580873021,208.532155572641,209.531730272261,210.486707790517),
 .UNSPECIFIED.);
#2766=B_SPLINE_CURVE_WITH_KNOTS('',3,(#60339,#60340,#60341,#60342,#60343,
#60344,#60345,#60346,#60347,#60348,#60349),.UNSPECIFIED.,.F.,.F.,(4,1,1,
1,1,1,1,1,4),(204.203522483337,204.218677279829,205.218251979449,206.217826679069,
207.217401378689,208.216976078309,209.216550777929,210.216125477549,210.486707790517),
 .UNSPECIFIED.);
#2767=B_SPLINE_CURVE_WITH_KNOTS('',3,(#60354,#60355,#60356,#60357,#60358,
#60359,#60360,#60361,#60362,#60363),.UNSPECIFIED.,.F.,.F.,(4,1,1,1,1,1,
1,4),(197.920337176158,198.536408576441,199.535983276061,200.535557975681,
201.535132675301,202.534707374921,203.534282074541,204.203522483337),
 .UNSPECIFIED.);
#2768=B_SPLINE_CURVE_WITH_KNOTS('',3,(#60364,#60365,#60366,#60367,#60368,
#60369,#60370,#60371,#60372,#60373),.UNSPECIFIED.,.F.,.F.,(4,1,1,1,1,1,
1,4),(197.920337176158,198.221229082109,199.220803781729,200.220378481349,
201.219953180969,202.219527880589,203.219102580209,204.203522483337),
 .UNSPECIFIED.);
#2769=B_SPLINE_CURVE_WITH_KNOTS('',3,(#60378,#60379,#60380,#60381,#60382,
#60383,#60384,#60385,#60386,#60387),.UNSPECIFIED.,.F.,.F.,(4,1,1,1,1,1,
1,4),(191.637151868978,192.538960378721,193.538535078341,194.538109777961,
195.537684477581,196.537259177201,197.536833876821,197.920337176158),
 .UNSPECIFIED.);
#2770=B_SPLINE_CURVE_WITH_KNOTS('',3,(#60388,#60389,#60390,#60391,#60392,
#60393,#60394,#60395,#60396,#60397),.UNSPECIFIED.,.F.,.F.,(4,1,1,1,1,1,
1,4),(191.637151868978,192.223780884389,193.223355584009,194.222930283629,
195.222504983249,196.222079682869,197.221654382489,197.920337176158),
 .UNSPECIFIED.);
#2771=B_SPLINE_CURVE_WITH_KNOTS('',3,(#60402,#60403,#60404,#60405,#60406,
#60407,#60408,#60409,#60410,#60411,#60412),.UNSPECIFIED.,.F.,.F.,(4,1,1,
1,1,1,1,1,4),(185.353966561798,185.541937481381,186.541512181001,187.541086880621,
188.540661580241,189.540236279861,190.539810979481,191.539385679101,191.637151868978),
 .UNSPECIFIED.);
#2772=B_SPLINE_CURVE_WITH_KNOTS('',3,(#60413,#60414,#60415,#60416,#60417,
#60418,#60419,#60420,#60421,#60422),.UNSPECIFIED.,.F.,.F.,(4,1,1,1,1,1,
1,4),(185.353966561799,186.226332686669,187.225907386289,188.225482085909,
189.225056785529,190.224631485149,191.224206184769,191.637151868978),
 .UNSPECIFIED.);
#2773=B_SPLINE_CURVE_WITH_KNOTS('',3,(#60427,#60428,#60429,#60430,#60431,
#60432,#60433,#60434,#60435,#60436),.UNSPECIFIED.,.F.,.F.,(4,1,1,1,1,1,
1,4),(179.070781254619,179.544489283661,180.544063983281,181.543638682901,
182.543213382521,183.542788082141,184.542362781761,185.353966561798),
 .UNSPECIFIED.);
#2774=B_SPLINE_CURVE_WITH_KNOTS('',3,(#60437,#60438,#60439,#60440,#60441,
#60442,#60443,#60444,#60445,#60446,#60447),.UNSPECIFIED.,.F.,.F.,(4,1,1,
1,1,1,1,1,4),(179.070781254619,179.229309789329,180.228884488949,181.228459188569,
182.228033888189,183.227608587809,184.227183287429,185.226757987049,185.353966561799),
 .UNSPECIFIED.);
#2775=B_SPLINE_CURVE_WITH_KNOTS('',3,(#60452,#60453,#60454,#60455,#60456,
#60457,#60458,#60459,#60460,#60461),.UNSPECIFIED.,.F.,.F.,(4,1,1,1,1,1,
1,4),(172.787595947439,173.547041085941,174.546615785561,175.546190485181,
176.545765184801,177.545339884421,178.544914584041,179.070781254619),
 .UNSPECIFIED.);
#2776=B_SPLINE_CURVE_WITH_KNOTS('',3,(#60462,#60463,#60464,#60465,#60466,
#60467,#60468,#60469,#60470,#60471),.UNSPECIFIED.,.F.,.F.,(4,1,1,1,1,1,
1,4),(172.78759594744,173.231861591609,174.231436291229,175.231010990849,
176.230585690469,177.230160390089,178.229735089709,179.070781254619),
 .UNSPECIFIED.);
#2777=B_SPLINE_CURVE_WITH_KNOTS('',3,(#60476,#60477,#60478,#60479,#60480,
#60481,#60482,#60483,#60484,#60485,#60486),.UNSPECIFIED.,.F.,.F.,(4,1,1,
1,1,1,1,1,4),(166.50441064026,166.550018188601,167.549592888221,168.549167587841,
169.548742287461,170.548316987081,171.547891686701,172.547466386321,172.787595947439),
 .UNSPECIFIED.);
#2778=B_SPLINE_CURVE_WITH_KNOTS('',3,(#60487,#60488,#60489,#60490,#60491,
#60492,#60493,#60494,#60495,#60496),.UNSPECIFIED.,.F.,.F.,(4,1,1,1,1,1,
1,4),(166.50441064026,167.234413393889,168.233988093509,169.233562793129,
170.233137492749,171.232712192369,172.232286891989,172.78759594744),
 .UNSPECIFIED.);
#2779=B_SPLINE_CURVE_WITH_KNOTS('',3,(#60501,#60502,#60503,#60504,#60505,
#60506,#60507,#60508,#60509,#60510),.UNSPECIFIED.,.F.,.F.,(4,1,1,1,1,1,
1,4),(160.22122533308,160.552569990881,161.552144690501,162.551719390121,
163.551294089741,164.550868789361,165.550443488981,166.50441064026),
 .UNSPECIFIED.);
#2780=B_SPLINE_CURVE_WITH_KNOTS('',3,(#60511,#60512,#60513,#60514,#60515,
#60516,#60517,#60518,#60519,#60520,#60521),.UNSPECIFIED.,.F.,.F.,(4,1,1,
1,1,1,1,1,4),(160.22122533308,160.237390496549,161.236965196169,162.236539895789,
163.236114595409,164.235689295029,165.235263994649,166.234838694269,166.50441064026),
 .UNSPECIFIED.);
#2781=B_SPLINE_CURVE_WITH_KNOTS('',3,(#60526,#60527,#60528,#60529,#60530,
#60531,#60532,#60533,#60534,#60535),.UNSPECIFIED.,.F.,.F.,(4,1,1,1,1,1,
1,4),(153.938040025901,154.555121793161,155.554696492781,156.554271192401,
157.553845892021,158.553420591641,159.552995291261,160.22122533308),
 .UNSPECIFIED.);
#2782=B_SPLINE_CURVE_WITH_KNOTS('',3,(#60536,#60537,#60538,#60539,#60540,
#60541,#60542,#60543,#60544,#60545),.UNSPECIFIED.,.F.,.F.,(4,1,1,1,1,1,
1,4),(153.938040025901,154.239942298829,155.239516998449,156.239091698069,
157.238666397689,158.238241097309,159.237815796929,160.22122533308),
 .UNSPECIFIED.);
#2783=B_SPLINE_CURVE_WITH_KNOTS('',3,(#60550,#60551,#60552,#60553,#60554,
#60555,#60556,#60557,#60558,#60559),.UNSPECIFIED.,.F.,.F.,(4,1,1,1,1,1,
1,4),(147.654854718721,148.557673595441,149.557248295061,150.556822994681,
151.556397694301,152.555972393921,153.555547093541,153.938040025901),
 .UNSPECIFIED.);
#2784=B_SPLINE_CURVE_WITH_KNOTS('',3,(#60560,#60561,#60562,#60563,#60564,
#60565,#60566,#60567,#60568,#60569),.UNSPECIFIED.,.F.,.F.,(4,1,1,1,1,1,
1,4),(147.654854718721,148.242494101109,149.242068800729,150.241643500349,
151.241218199969,152.240792899589,153.240367599209,153.938040025901),
 .UNSPECIFIED.);
#2785=B_SPLINE_CURVE_WITH_KNOTS('',3,(#60574,#60575,#60576,#60577,#60578,
#60579,#60580,#60581,#60582,#60583,#60584),.UNSPECIFIED.,.F.,.F.,(4,1,1,
1,1,1,1,1,4),(141.371669411541,141.560650698101,142.560225397721,143.559800097341,
144.559374796961,145.558949496581,146.558524196201,147.558098895821,147.654854718721),
 .UNSPECIFIED.);
#2786=B_SPLINE_CURVE_WITH_KNOTS('',3,(#60585,#60586,#60587,#60588,#60589,
#60590,#60591,#60592,#60593,#60594),.UNSPECIFIED.,.F.,.F.,(4,1,1,1,1,1,
1,4),(141.371669411542,142.245045903389,143.244620603009,144.244195302629,
145.243770002249,146.243344701869,147.242919401489,147.654854718721),
 .UNSPECIFIED.);
#2787=B_SPLINE_CURVE_WITH_KNOTS('',3,(#60599,#60600,#60601,#60602,#60603,
#60604,#60605,#60606,#60607,#60608),.UNSPECIFIED.,.F.,.F.,(4,1,1,1,1,1,
1,4),(135.088484104362,135.563202500381,136.562777200001,137.562351899621,
138.561926599241,139.561501298861,140.561075998481,141.371669411541),
 .UNSPECIFIED.);
#2788=B_SPLINE_CURVE_WITH_KNOTS('',3,(#60609,#60610,#60611,#60612,#60613,
#60614,#60615,#60616,#60617,#60618,#60619),.UNSPECIFIED.,.F.,.F.,(4,1,1,
1,1,1,1,1,4),(135.088484104362,135.248023006049,136.247597705669,137.247172405289,
138.246747104909,139.246321804529,140.245896504149,141.245471203769,141.371669411542),
 .UNSPECIFIED.);
#2789=B_SPLINE_CURVE_WITH_KNOTS('',3,(#60624,#60625,#60626,#60627,#60628,
#60629,#60630,#60631,#60632,#60633),.UNSPECIFIED.,.F.,.F.,(4,1,1,1,1,1,
1,4),(128.805298797182,129.565754302661,130.565329002281,131.564903701901,
132.564478401521,133.564053101141,134.563627800761,135.088484104362),
 .UNSPECIFIED.);
#2790=B_SPLINE_CURVE_WITH_KNOTS('',3,(#60634,#60635,#60636,#60637,#60638,
#60639,#60640,#60641,#60642,#60643),.UNSPECIFIED.,.F.,.F.,(4,1,1,1,1,1,
1,4),(128.805298797183,129.250574808329,130.250149507949,131.249724207569,
132.249298907189,133.248873606809,134.248448306429,135.088484104362),
 .UNSPECIFIED.);
#2791=B_SPLINE_CURVE_WITH_KNOTS('',3,(#60648,#60649,#60650,#60651,#60652,
#60653,#60654,#60655,#60656,#60657,#60658),.UNSPECIFIED.,.F.,.F.,(4,1,1,
1,1,1,1,1,4),(122.522113490003,122.568731405321,123.568306104941,124.567880804561,
125.567455504181,126.567030203801,127.566604903421,128.566179603041,128.805298797182),
 .UNSPECIFIED.);
#2792=B_SPLINE_CURVE_WITH_KNOTS('',3,(#60659,#60660,#60661,#60662,#60663,
#60664,#60665,#60666,#60667,#60668),.UNSPECIFIED.,.F.,.F.,(4,1,1,1,1,1,
1,4),(122.522113490003,123.253126610609,124.252701310229,125.252276009849,
126.251850709469,127.251425409089,128.251000108709,128.805298797183),
 .UNSPECIFIED.);
#2793=B_SPLINE_CURVE_WITH_KNOTS('',3,(#60673,#60674,#60675,#60676,#60677,
#60678,#60679,#60680,#60681,#60682),.UNSPECIFIED.,.F.,.F.,(4,1,1,1,1,1,
1,4),(116.238928182823,116.571283207601,117.570857907221,118.570432606841,
119.570007306461,120.569582006081,121.569156705701,122.522113490003),
 .UNSPECIFIED.);
#2794=B_SPLINE_CURVE_WITH_KNOTS('',3,(#60683,#60684,#60685,#60686,#60687,
#60688,#60689,#60690,#60691,#60692,#60693),.UNSPECIFIED.,.F.,.F.,(4,1,1,
1,1,1,1,1,4),(116.238928182823,116.256103713269,117.255678412889,118.255253112509,
119.254827812129,120.254402511749,121.253977211369,122.253551910989,122.522113490003),
 .UNSPECIFIED.);
#2795=B_SPLINE_CURVE_WITH_KNOTS('',3,(#60698,#60699,#60700,#60701,#60702,
#60703,#60704,#60705,#60706,#60707),.UNSPECIFIED.,.F.,.F.,(4,1,1,1,1,1,
1,4),(109.955742875644,110.573835009881,111.573409709501,112.572984409121,
113.572559108741,114.572133808361,115.571708507981,116.238928182823),
 .UNSPECIFIED.);
#2796=B_SPLINE_CURVE_WITH_KNOTS('',3,(#60708,#60709,#60710,#60711,#60712,
#60713,#60714,#60715,#60716,#60717),.UNSPECIFIED.,.F.,.F.,(4,1,1,1,1,1,
1,4),(109.955742875644,110.258655515549,111.258230215169,112.257804914789,
113.257379614409,114.256954314029,115.256529013649,116.238928182823),
 .UNSPECIFIED.);
#2797=B_SPLINE_CURVE_WITH_KNOTS('',3,(#60722,#60723,#60724,#60725,#60726,
#60727,#60728,#60729,#60730,#60731),.UNSPECIFIED.,.F.,.F.,(4,1,1,1,1,1,
1,4),(103.672557568464,104.576386812161,105.575961511781,106.575536211401,
107.575110911021,108.574685610641,109.574260310261,109.955742875644),
 .UNSPECIFIED.);
#2798=B_SPLINE_CURVE_WITH_KNOTS('',3,(#60732,#60733,#60734,#60735,#60736,
#60737,#60738,#60739,#60740,#60741),.UNSPECIFIED.,.F.,.F.,(4,1,1,1,1,1,
1,4),(103.672557568464,104.261207317829,105.260782017449,106.260356717069,
107.259931416689,108.259506116309,109.259080815929,109.955742875644),
 .UNSPECIFIED.);
#2799=B_SPLINE_CURVE_WITH_KNOTS('',3,(#60746,#60747,#60748,#60749,#60750,
#60751,#60752,#60753,#60754,#60755,#60756),.UNSPECIFIED.,.F.,.F.,(4,1,1,
1,1,1,1,1,4),(97.3893722612844,97.5793639148213,98.5789386144413,99.5785133140613,
100.578088013681,101.577662713301,102.577237412921,103.576812112541,103.672557568464),
 .UNSPECIFIED.);
#2800=B_SPLINE_CURVE_WITH_KNOTS('',3,(#60757,#60758,#60759,#60760,#60761,
#60762,#60763,#60764,#60765,#60766),.UNSPECIFIED.,.F.,.F.,(4,1,1,1,1,1,
1,4),(97.3893722612846,98.2637591201091,99.2633338197291,100.262908519349,
101.262483218969,102.262057918589,103.261632618209,103.672557568464),
 .UNSPECIFIED.);
#2801=B_SPLINE_CURVE_WITH_KNOTS('',3,(#60771,#60772,#60773,#60774,#60775,
#60776,#60777,#60778,#60779,#60780),.UNSPECIFIED.,.F.,.F.,(4,1,1,1,1,1,
1,4),(91.1061869541047,91.5819157171013,92.5814904167213,93.5810651163413,
94.5806398159613,95.5802145155813,96.5797892152013,97.3893722612844),
 .UNSPECIFIED.);
#2802=B_SPLINE_CURVE_WITH_KNOTS('',3,(#60781,#60782,#60783,#60784,#60785,
#60786,#60787,#60788,#60789,#60790,#60791),.UNSPECIFIED.,.F.,.F.,(4,1,1,
1,1,1,1,1,4),(91.106186954105,91.2667362227691,92.2663109223891,93.2658856220091,
94.265460321629,95.265035021249,96.264609720869,97.264184420489,97.3893722612846),
 .UNSPECIFIED.);
#2803=B_SPLINE_CURVE_WITH_KNOTS('',3,(#60796,#60797,#60798,#60799,#60800,
#60801,#60802,#60803,#60804,#60805),.UNSPECIFIED.,.F.,.F.,(4,1,1,1,1,1,
1,4),(84.8230016469252,85.5844675193813,86.5840422190013,87.5836169186213,
88.5831916182413,89.5827663178613,90.5823410174813,91.1061869541047),
 .UNSPECIFIED.);
#2804=B_SPLINE_CURVE_WITH_KNOTS('',3,(#60806,#60807,#60808,#60809,#60810,
#60811,#60812,#60813,#60814,#60815),.UNSPECIFIED.,.F.,.F.,(4,1,1,1,1,1,
1,4),(84.8230016469254,85.2692880250491,86.2688627246691,87.2684374242891,
88.2680121239091,89.2675868235291,90.2671615231491,91.106186954105),
 .UNSPECIFIED.);
#2805=B_SPLINE_CURVE_WITH_KNOTS('',3,(#60820,#60821,#60822,#60823,#60824,
#60825,#60826,#60827,#60828,#60829,#60830),.UNSPECIFIED.,.F.,.F.,(4,1,1,
1,1,1,1,1,4),(78.5398163397456,78.5874446220413,79.5870193216613,80.5865940212813,
81.5861687209013,82.5857434205213,83.5853181201413,84.5848928197613,84.8230016469252),
 .UNSPECIFIED.);
#2806=B_SPLINE_CURVE_WITH_KNOTS('',3,(#60831,#60832,#60833,#60834,#60835,
#60836,#60837,#60838,#60839,#60840),.UNSPECIFIED.,.F.,.F.,(4,1,1,1,1,1,
1,4),(78.5398163397458,79.2718398273291,80.2714145269491,81.2709892265691,
82.2705639261891,83.2701386258091,84.2697133254291,84.8230016469254),
 .UNSPECIFIED.);
#2807=B_SPLINE_CURVE_WITH_KNOTS('',3,(#60845,#60846,#60847,#60848,#60849,
#60850,#60851,#60852,#60853,#60854),.UNSPECIFIED.,.F.,.F.,(4,1,1,1,1,1,
1,4),(72.256631032566,72.5899964243213,73.5895711239413,74.5891458235613,
75.5887205231813,76.5882952228013,77.5878699224213,78.5398163397456),
 .UNSPECIFIED.);
#2808=B_SPLINE_CURVE_WITH_KNOTS('',3,(#60855,#60856,#60857,#60858,#60859,
#60860,#60861,#60862,#60863,#60864,#60865),.UNSPECIFIED.,.F.,.F.,(4,1,1,
1,1,1,1,1,4),(72.2566310325662,72.2748169299891,73.2743916296091,74.2739663292291,
75.2735410288491,76.2731157284691,77.2726904280891,78.2722651277091,78.5398163397458),
 .UNSPECIFIED.);
#2809=B_SPLINE_CURVE_WITH_KNOTS('',3,(#60870,#60871,#60872,#60873,#60874,
#60875,#60876,#60877,#60878,#60879),.UNSPECIFIED.,.F.,.F.,(4,1,1,1,1,1,
1,4),(65.9734457253864,66.5925482266013,67.5921229262213,68.5916976258413,
69.5912723254613,70.5908470250813,71.5904217247013,72.256631032566),
 .UNSPECIFIED.);
#2810=B_SPLINE_CURVE_WITH_KNOTS('',3,(#60880,#60881,#60882,#60883,#60884,
#60885,#60886,#60887,#60888,#60889),.UNSPECIFIED.,.F.,.F.,(4,1,1,1,1,1,
1,4),(65.9734457253866,66.2773687322691,67.2769434318891,68.2765181315091,
69.2760928311291,70.2756675307491,71.2752422303691,72.2566310325662),
 .UNSPECIFIED.);
#2811=B_SPLINE_CURVE_WITH_KNOTS('',3,(#60894,#60895,#60896,#60897,#60898,
#60899,#60900,#60901,#60902,#60903),.UNSPECIFIED.,.F.,.F.,(4,1,1,1,1,1,
1,4),(59.6902604182068,60.5951000288813,61.5946747285013,62.5942494281213,
63.5938241277413,64.5933988273613,65.5929735269813,65.9734457253864),
 .UNSPECIFIED.);
#2812=B_SPLINE_CURVE_WITH_KNOTS('',3,(#60904,#60905,#60906,#60907,#60908,
#60909,#60910,#60911,#60912,#60913),.UNSPECIFIED.,.F.,.F.,(4,1,1,1,1,1,
1,4),(59.690260418207,60.2799205345491,61.2794952341691,62.2790699337891,
63.2786446334091,64.2782193330291,65.2777940326491,65.9734457253866),
 .UNSPECIFIED.);
#2813=B_SPLINE_CURVE_WITH_KNOTS('',3,(#60918,#60919,#60920,#60921,#60922,
#60923,#60924,#60925,#60926,#60927,#60928),.UNSPECIFIED.,.F.,.F.,(4,1,1,
1,1,1,1,1,4),(53.4070751110272,53.5980771315413,54.5976518311613,55.5972265307813,
56.5968012304013,57.5963759300213,58.5959506296413,59.5955253292613,59.6902604182068),
 .UNSPECIFIED.);
#2814=B_SPLINE_CURVE_WITH_KNOTS('',3,(#60929,#60930,#60931,#60932,#60933,
#60934,#60935,#60936,#60937,#60938),.UNSPECIFIED.,.F.,.F.,(4,1,1,1,1,1,
1,4),(53.4070751110274,54.2824723368291,55.2820470364491,56.2816217360691,
57.2811964356891,58.2807711353091,59.2803458349291,59.690260418207),
 .UNSPECIFIED.);
#2815=B_SPLINE_CURVE_WITH_KNOTS('',3,(#60943,#60944,#60945,#60946,#60947,
#60948,#60949,#60950,#60951,#60952),.UNSPECIFIED.,.F.,.F.,(4,1,1,1,1,1,
1,4),(47.1238898038476,47.6006289338214,48.6002036334414,49.5997783330614,
50.5993530326813,51.5989277323013,52.5985024319213,53.4070751110272),
 .UNSPECIFIED.);
#2816=B_SPLINE_CURVE_WITH_KNOTS('',3,(#60953,#60954,#60955,#60956,#60957,
#60958,#60959,#60960,#60961,#60962,#60963),.UNSPECIFIED.,.F.,.F.,(4,1,1,
1,1,1,1,1,4),(47.1238898038478,47.2854494394891,48.2850241391091,49.2845988387291,
50.2841735383491,51.2837482379691,52.2833229375891,53.2828976372091,53.4070751110274),
 .UNSPECIFIED.);
#2817=B_SPLINE_CURVE_WITH_KNOTS('',3,(#60968,#60969,#60970,#60971,#60972,
#60973,#60974,#60975,#60976,#60977),.UNSPECIFIED.,.F.,.F.,(4,1,1,1,1,1,
1,4),(40.840704496668,41.6031807361014,42.6027554357214,43.6023301353414,
44.6019048349614,45.6014795345814,46.6010542342014,47.1238898038476),
 .UNSPECIFIED.);
#2818=B_SPLINE_CURVE_WITH_KNOTS('',3,(#60978,#60979,#60980,#60981,#60982,
#60983,#60984,#60985,#60986,#60987),.UNSPECIFIED.,.F.,.F.,(4,1,1,1,1,1,
1,4),(40.8407044966683,41.2880012417691,42.2875759413891,43.2871506410091,
44.2867253406291,45.2863000402491,46.2858747398691,47.1238898038478),
 .UNSPECIFIED.);
#2819=B_SPLINE_CURVE_WITH_KNOTS('',3,(#60992,#60993,#60994,#60995,#60996,
#60997,#60998,#60999,#61000,#61001,#61002),.UNSPECIFIED.,.F.,.F.,(4,1,1,
1,1,1,1,1,4),(34.5575191894884,34.6061578387614,35.6057325383814,36.6053072380014,
37.6048819376214,38.6044566372414,39.6040313368614,40.6036060364814,40.840704496668),
 .UNSPECIFIED.);
#2820=B_SPLINE_CURVE_WITH_KNOTS('',3,(#61003,#61004,#61005,#61006,#61007,
#61008,#61009,#61010,#61011,#61012),.UNSPECIFIED.,.F.,.F.,(4,1,1,1,1,1,
1,4),(34.5575191894887,35.2905530440491,36.2901277436691,37.2897024432891,
38.2892771429091,39.2888518425291,40.2884265421491,40.8407044966683),
 .UNSPECIFIED.);
#2821=B_SPLINE_CURVE_WITH_KNOTS('',3,(#61017,#61018,#61019,#61020,#61021,
#61022,#61023,#61024,#61025,#61026),.UNSPECIFIED.,.F.,.F.,(4,1,1,1,1,1,
1,4),(28.2743338823088,28.6087096410414,29.6082843406614,30.6078590402814,
31.6074337399014,32.6070084395214,33.6065831391414,34.5575191894884),
 .UNSPECIFIED.);
#2822=B_SPLINE_CURVE_WITH_KNOTS('',3,(#61027,#61028,#61029,#61030,#61031,
#61032,#61033,#61034,#61035,#61036,#61037),.UNSPECIFIED.,.F.,.F.,(4,1,1,
1,1,1,1,1,4),(28.2743338823091,28.2935301467091,29.2931048463291,30.2926795459491,
31.2922542455691,32.2918289451891,33.2914036448091,34.2909783444291,34.5575191894887),
 .UNSPECIFIED.);
#2823=B_SPLINE_CURVE_WITH_KNOTS('',3,(#61042,#61043,#61044,#61045,#61046,
#61047,#61048,#61049,#61050,#61051),.UNSPECIFIED.,.F.,.F.,(4,1,1,1,1,1,
1,4),(21.9911485751293,22.6112614433214,23.6108361429414,24.6104108425614,
25.6099855421814,26.6095602418014,27.6091349414214,28.2743338823088),
 .UNSPECIFIED.);
#2824=B_SPLINE_CURVE_WITH_KNOTS('',3,(#61052,#61053,#61054,#61055,#61056,
#61057,#61058,#61059,#61060,#61061),.UNSPECIFIED.,.F.,.F.,(4,1,1,1,1,1,
1,4),(21.9911485751295,22.2960819489891,23.2956566486091,24.2952313482291,
25.2948060478491,26.2943807474691,27.2939554470891,28.2743338823091),
 .UNSPECIFIED.);
#2825=B_SPLINE_CURVE_WITH_KNOTS('',3,(#61066,#61067,#61068,#61069,#61070,
#61071,#61072,#61073,#61074,#61075),.UNSPECIFIED.,.F.,.F.,(4,1,1,1,1,1,
1,4),(15.7079632679497,16.6138132456014,17.6133879452214,18.6129626448414,
19.6125373444614,20.6121120440814,21.6116867437014,21.9911485751293),
 .UNSPECIFIED.);
#2826=B_SPLINE_CURVE_WITH_KNOTS('',3,(#61076,#61077,#61078,#61079,#61080,
#61081,#61082,#61083,#61084,#61085),.UNSPECIFIED.,.F.,.F.,(4,1,1,1,1,1,
1,4),(15.7079632679499,16.2986337512691,17.2982084508891,18.2977831505091,
19.2973578501291,20.2969325497491,21.2965072493691,21.9911485751295),
 .UNSPECIFIED.);
#2827=B_SPLINE_CURVE_WITH_KNOTS('',3,(#61088,#61089,#61090,#61091,#61092,
#61093,#61094,#61095,#61096,#61097,#61098,#61099,#61100,#61101,#61102,#61103,
#61104,#61105,#61106,#61107,#61108,#61109,#61110,#61111,#61112,#61113,#61114,
#61115,#61116,#61117,#61118,#61119,#61120,#61121,#61122,#61123,#61124,#61125,
#61126,#61127,#61128,#61129,#61130,#61131,#61132,#61133,#61134,#61135,#61136,
#61137,#61138,#61139,#61140,#61141,#61142,#61143,#61144,#61145,#61146,#61147,
#61148,#61149,#61150,#61151,#61152,#61153,#61154,#61155,#61156,#61157,#61158,
#61159,#61160,#61161,#61162,#61163,#61164,#61165,#61166,#61167,#61168,#61169,
#61170,#61171,#61172),.UNSPECIFIED.,.F.,.F.,(4,3,3,3,3,3,3,3,3,3,3,3,3,
3,3,3,3,3,3,3,3,3,3,3,3,3,3,3,4),(-0.276631791712738,-0.26777280382095,
-0.253162595967305,-0.247575468035802,-0.244113223126194,-0.228893324436004,
-0.217867136109351,-0.213228637626788,-0.209216864955607,-0.193459635982162,
-0.177407427195511,-0.168226524852329,-0.162410876603139,-0.159528053086101,
-0.143000073191966,-0.140683817822782,-0.124741429572464,-0.116250765378535,
-0.111155360582251,-0.107652961500464,-0.0910939615488431,-0.0741766492334206,
-0.0647050431380984,-0.0582172002991486,-0.0537828459296116,-0.0363196889473096,
-0.0181598444736548,-0.00111710893352747,0.),.UNSPECIFIED.);
#2828=B_SPLINE_CURVE_WITH_KNOTS('',3,(#61177,#61178,#61179,#61180,#61181,
#61182,#61183,#61184,#61185,#61186,#61187,#61188,#61189,#61190,#61191,#61192,
#61193,#61194,#61195,#61196,#61197,#61198,#61199,#61200,#61201,#61202,#61203,
#61204,#61205,#61206,#61207,#61208,#61209,#61210,#61211,#61212,#61213,#61214,
#61215,#61216,#61217,#61218,#61219,#61220,#61221,#61222,#61223,#61224,#61225,
#61226,#61227,#61228,#61229,#61230,#61231,#61232,#61233,#61234,#61235,#61236,
#61237,#61238,#61239,#61240,#61241,#61242,#61243,#61244,#61245,#61246,#61247,
#61248,#61249,#61250,#61251,#61252,#61253,#61254,#61255,#61256,#61257,#61258),
 .UNSPECIFIED.,.F.,.F.,(4,3,3,3,3,3,3,3,3,3,3,3,3,3,3,3,3,3,3,3,3,3,3,3,
3,3,3,4),(-0.275362278356834,-0.264551439176698,-0.247185256457859,-0.238155454944618,
-0.234297382099102,-0.21709561190626,-0.205661407596225,-0.200946096586765,
-0.196794724908398,-0.180042528899867,-0.163712523477344,-0.154189886964504,
-0.148003615780328,-0.144168982533267,-0.128317505169721,-0.125621977425983,
-0.109669333874548,-0.101986130473596,-0.0960165185644219,-0.093169255793087,
-0.0774033899336095,-0.0617050632725603,-0.0534800915089582,-0.0478612930675681,
-0.0448398831927098,-0.0297305382808535,-0.0148652691404268,0.),
 .UNSPECIFIED.);
#2829=B_SPLINE_CURVE_WITH_KNOTS('',3,(#63011,#63012,#63013,#63014,#63015,
#63016,#63017,#63018,#63019,#63020,#63021,#63022,#63023,#63024,#63025,#63026),
 .UNSPECIFIED.,.F.,.F.,(4,3,3,3,3,4),(428.379342694673,428.81754613698,
429.8171208366,430.81669553622,431.81627023584,432.74182166138),
 .UNSPECIFIED.);
#2830=B_SPLINE_CURVE_WITH_KNOTS('',3,(#63028,#63029,#63030,#63031,#63032,
#63033,#63034,#63035,#63036,#63037,#63038,#63039,#63040,#63041,#63042,#63043,
#63044,#63045,#63046,#63047,#63048,#63049,#63050,#63051,#63052,#63053,#63054,
#63055,#63056,#63057,#63058,#63059,#63060,#63061,#63062,#63063,#63064,#63065,
#63066,#63067,#63068,#63069,#63070,#63071,#63072,#63073,#63074,#63075,#63076,
#63077,#63078,#63079,#63080,#63081,#63082,#63083,#63084,#63085,#63086,#63087,
#63088,#63089,#63090,#63091,#63092,#63093,#63094,#63095,#63096,#63097,#63098,
#63099,#63100,#63101,#63102,#63103,#63104,#63105,#63106,#63107,#63108,#63109,
#63110,#63111,#63112),.UNSPECIFIED.,.F.,.F.,(4,3,3,3,3,3,3,3,3,3,3,3,3,
3,3,3,3,3,3,3,3,3,3,3,3,3,3,3,4),(-0.276631791712687,-0.267772803820864,
-0.253162597214951,-0.24757547093428,-0.244113224588513,-0.228893326817863,
-0.217867138193469,-0.213228641517051,-0.209216865648389,-0.19345963730386,
-0.177407428450592,-0.168226525793622,-0.162410877946272,-0.159528054577906,
-0.143000074615614,-0.140683817822713,-0.124741430017734,-0.116250765733781,
-0.111155360560927,-0.107652961444369,-0.0910939620347423,-0.0741766502224574,
-0.0647050432131039,-0.0582172004360556,-0.0537828456880876,-0.0363196890394545,
-0.0181598445197272,-0.00111710732716392,0.),.UNSPECIFIED.);
#2831=B_SPLINE_CURVE_WITH_KNOTS('',3,(#63113,#63114,#63115,#63116,#63117,
#63118,#63119,#63120,#63121),.UNSPECIFIED.,.F.,.F.,(4,1,1,1,1,1,4),(10.3752088276291,
11.3007602531692,12.3003349527892,13.2999096524091,14.2994843520291,15.2990590516491,
15.7079632679499),.UNSPECIFIED.);
#2832=B_SPLINE_CURVE_WITH_KNOTS('',3,(#63127,#63128,#63129,#63130,#63131,
#63132,#63133,#63134,#63135,#63136,#63137,#63138,#63139,#63140,#63141,#63142,
#63143,#63144,#63145,#63146,#63147,#63148,#63149,#63150,#63151,#63152,#63153,
#63154,#63155,#63156,#63157,#63158,#63159,#63160,#63161,#63162,#63163,#63164,
#63165,#63166,#63167,#63168,#63169,#63170,#63171,#63172,#63173,#63174,#63175,
#63176,#63177,#63178,#63179,#63180,#63181,#63182,#63183,#63184,#63185,#63186,
#63187,#63188,#63189,#63190,#63191,#63192,#63193,#63194,#63195,#63196,#63197,
#63198,#63199,#63200,#63201,#63202,#63203,#63204,#63205,#63206,#63207,#63208),
 .UNSPECIFIED.,.F.,.F.,(4,3,3,3,3,3,3,3,3,3,3,3,3,3,3,3,3,3,3,3,3,3,3,3,
3,3,3,4),(-0.275362278356922,-0.264551439176764,-0.247185256457921,-0.238155454613246,
-0.234297381972466,-0.217095611759951,-0.20566140746821,-0.200946095991088,
-0.196794724755822,-0.180042528611185,-0.163712522131083,-0.154189885954817,
-0.148003612972641,-0.144168982208487,-0.128317503830928,-0.12562197742602,
-0.109669343900505,-0.101986144157958,-0.0960166186373187,-0.0931694064854494,
-0.0774035414773043,-0.0617052132751136,-0.0534801524126021,-0.0478615116658561,
-0.0448398640447273,-0.0297305204847559,-0.0148652602423779,0.),
 .UNSPECIFIED.);
#2833=B_SPLINE_CURVE_WITH_KNOTS('',3,(#63211,#63212,#63213,#63214,#63215,
#63216,#63217,#63218),.UNSPECIFIED.,.F.,.F.,(4,1,1,1,1,4),(11.6159397475014,
12.6155144471214,13.6150891467414,14.6146638463614,15.6142385459814,15.7079632679497),
 .UNSPECIFIED.);
#2834=B_SPLINE_CURVE_WITH_KNOTS('',3,(#64971,#64972,#64973,#64974,#64975,
#64976,#64977,#64978,#64979,#64980,#64981,#64982,#64983),.UNSPECIFIED.,
 .F.,.F.,(4,3,3,3,4),(-434.814994334699,-433.815419635079,-432.815844935459,
-431.816270235839,-431.348624408659),.UNSPECIFIED.);
#2835=B_SPLINE_CURVE_WITH_KNOTS('',3,(#66057,#66058,#66059,#66060,#66061,
#66062,#66063,#66064,#66065,#66066,#66067,#66068,#66069,#66070,#66071,#66072),
 .UNSPECIFIED.,.F.,.F.,(4,3,3,3,3,4),(-4.09289414414337,-3.98721409151323,
-3.48881233007407,-2.99041056863492,-2.49200880719577,-2.07135887395549),
 .UNSPECIFIED.);
#2836=B_SPLINE_CURVE_WITH_KNOTS('',3,(#66075,#66076,#66077,#66078,#66079,
#66080,#66081,#66082,#66083,#66084),.UNSPECIFIED.,.F.,.F.,(4,3,3,4),(0.,
0.498401761439146,0.996803522878299,1.12005738340184),.UNSPECIFIED.);
#2837=B_SPLINE_CURVE_WITH_KNOTS('',3,(#66089,#66090,#66091,#66092,#66093,
#66094,#66095,#66096,#66097,#66098,#66099,#66100,#66101,#66102,#66103,#66104,
#66105,#66106,#66107,#66108,#66109,#66110,#66111,#66112,#66113,#66114,#66115,
#66116,#66117,#66118,#66119,#66120,#66121,#66122,#66123,#66124,#66125,#66126,
#66127,#66128),.UNSPECIFIED.,.F.,.F.,(4,3,3,3,3,3,3,3,3,3,3,3,3,4),(-10.376079451323,
-9.96803522878307,-9.46963346734392,-8.97123170590477,-8.47282994446562,
-7.97442818302646,-7.47602642158731,-6.97762466014815,-6.479222898709,-5.98082113726984,
-5.48241937583069,-4.98401761439154,-4.48561585295238,-4.09289414414337),
 .UNSPECIFIED.);
#2838=B_SPLINE_CURVE_WITH_KNOTS('',3,(#66129,#66130,#66131,#66132,#66133,
#66134,#66135,#66136,#66137,#66138,#66139,#66140,#66141,#66142,#66143,#66144,
#66145,#66146,#66147,#66148,#66149,#66150,#66151,#66152,#66153,#66154,#66155,
#66156,#66157,#66158,#66159,#66160,#66161,#66162,#66163,#66164,#66165,#66166,
#66167,#66168),.UNSPECIFIED.,.F.,.F.,(4,3,3,3,3,3,3,3,3,3,3,3,3,4),(1.12005738340184,
1.49520528431745,1.99360704575661,2.49200880719576,2.99041056863492,3.48881233007407,
3.98721409151323,4.48561585295238,4.98401761439154,5.48241937583069,5.98082113726985,
6.479222898709,6.97762466014816,7.40324269058142),.UNSPECIFIED.);
#2839=B_SPLINE_CURVE_WITH_KNOTS('',3,(#66173,#66174,#66175,#66176,#66177,
#66178,#66179,#66180,#66181,#66182,#66183,#66184,#66185,#66186,#66187,#66188,
#66189,#66190,#66191,#66192,#66193,#66194,#66195,#66196,#66197,#66198,#66199,
#66200,#66201,#66202,#66203,#66204,#66205,#66206,#66207,#66208,#66209,#66210,
#66211,#66212,#66213,#66214,#66215),.UNSPECIFIED.,.F.,.F.,(4,3,3,3,3,3,
3,3,3,3,3,3,3,3,4),(-16.6592647585025,-16.4472581274921,-15.9488563660529,
-15.4504546046138,-14.9520528431746,-14.4536510817355,-13.9552493202963,
-13.4568475588571,-12.958445797418,-12.4600440359788,-11.9616422745397,
-11.4632405131005,-10.9648387516614,-10.4664369902222,-10.376079451323),
 .UNSPECIFIED.);
#2840=B_SPLINE_CURVE_WITH_KNOTS('',3,(#66216,#66217,#66218,#66219,#66220,
#66221,#66222,#66223,#66224,#66225,#66226,#66227,#66228,#66229,#66230,#66231,
#66232,#66233,#66234,#66235,#66236,#66237,#66238,#66239,#66240,#66241,#66242,
#66243,#66244,#66245,#66246,#66247,#66248,#66249,#66250,#66251,#66252,#66253,
#66254,#66255,#66256,#66257,#66258),.UNSPECIFIED.,.F.,.F.,(4,3,3,3,3,3,
3,3,3,3,3,3,3,3,4),(7.40324269058142,7.47602642158731,7.97442818302646,
8.47282994446562,8.97123170590477,9.46963346734393,9.96803522878308,10.4664369902222,
10.9648387516614,11.4632405131005,11.9616422745397,12.4600440359788,12.958445797418,
13.4568475588571,13.686427997761),.UNSPECIFIED.);
#2841=B_SPLINE_CURVE_WITH_KNOTS('',3,(#66263,#66264,#66265,#66266,#66267,
#66268,#66269,#66270,#66271,#66272,#66273,#66274,#66275,#66276,#66277,#66278,
#66279,#66280,#66281,#66282,#66283,#66284,#66285,#66286,#66287,#66288,#66289,
#66290,#66291,#66292,#66293,#66294,#66295,#66296,#66297,#66298,#66299,#66300,
#66301,#66302,#66303,#66304,#66305),.UNSPECIFIED.,.F.,.F.,(4,3,3,3,3,3,
3,3,3,3,3,3,3,3,4),(-22.9424500656821,-22.9264810262011,-22.4280792647619,
-21.9296775033228,-21.4312757418836,-20.9328739804445,-20.4344722190053,
-19.9360704575661,-19.437668696127,-18.9392669346878,-18.4408651732487,
-17.9424634118095,-17.4440616503704,-16.9456598889312,-16.6592647585025),
 .UNSPECIFIED.);
#2842=B_SPLINE_CURVE_WITH_KNOTS('',3,(#66306,#66307,#66308,#66309,#66310,
#66311,#66312,#66313,#66314,#66315,#66316,#66317,#66318,#66319,#66320,#66321,
#66322,#66323,#66324,#66325,#66326,#66327,#66328,#66329,#66330,#66331,#66332,
#66333,#66334,#66335,#66336,#66337,#66338,#66339,#66340,#66341,#66342,#66343,
#66344,#66345,#66346,#66347,#66348),.UNSPECIFIED.,.F.,.F.,(4,3,3,3,3,3,
3,3,3,3,3,3,3,3,4),(13.686427997761,13.9552493202963,14.4536510817355,14.9520528431746,
15.4504546046138,15.9488563660529,16.4472581274921,16.9456598889312,17.4440616503704,
17.9424634118095,18.4408651732487,18.9392669346878,19.437668696127,19.9360704575661,
19.9696133049406),.UNSPECIFIED.);
#2843=B_SPLINE_CURVE_WITH_KNOTS('',3,(#66353,#66354,#66355,#66356,#66357,
#66358,#66359,#66360,#66361,#66362,#66363,#66364,#66365,#66366,#66367,#66368,
#66369,#66370,#66371,#66372,#66373,#66374,#66375,#66376,#66377,#66378,#66379,
#66380,#66381,#66382,#66383,#66384,#66385,#66386,#66387,#66388,#66389,#66390,
#66391,#66392),.UNSPECIFIED.,.F.,.F.,(4,3,3,3,3,3,3,3,3,3,3,3,3,4),(-29.2256353728617,
-28.9073021634709,-28.4089004020318,-27.9104986405926,-27.4120968791534,
-26.9136951177143,-26.4152933562751,-25.916891594836,-25.4184898333968,
-24.9200880719577,-24.4216863105185,-23.9232845490794,-23.4248827876402,
-22.9424500656821),.UNSPECIFIED.);
#2844=B_SPLINE_CURVE_WITH_KNOTS('',3,(#66393,#66394,#66395,#66396,#66397,
#66398,#66399,#66400,#66401,#66402,#66403,#66404,#66405,#66406,#66407,#66408,
#66409,#66410,#66411,#66412,#66413,#66414,#66415,#66416,#66417,#66418,#66419,
#66420,#66421,#66422,#66423,#66424,#66425,#66426,#66427,#66428,#66429,#66430,
#66431,#66432),.UNSPECIFIED.,.F.,.F.,(4,3,3,3,3,3,3,3,3,3,3,3,3,4),(19.9696133049406,
20.4344722190053,20.9328739804445,21.4312757418836,21.9296775033228,22.4280792647619,
22.9264810262011,23.4248827876402,23.9232845490794,24.4216863105185,24.9200880719577,
25.4184898333968,25.916891594836,26.2527986121202),.UNSPECIFIED.);
#2845=B_SPLINE_CURVE_WITH_KNOTS('',3,(#66437,#66438,#66439,#66440,#66441,
#66442,#66443,#66444,#66445,#66446,#66447,#66448,#66449,#66450,#66451,#66452,
#66453,#66454,#66455,#66456,#66457,#66458,#66459,#66460,#66461,#66462,#66463,
#66464,#66465,#66466,#66467,#66468,#66469,#66470,#66471,#66472,#66473,#66474,
#66475,#66476,#66477,#66478,#66479),.UNSPECIFIED.,.F.,.F.,(4,3,3,3,3,3,
3,3,3,3,3,3,3,3,4),(-35.5088206800413,-35.3865250621799,-34.8881233007408,
-34.3897215393016,-33.8913197778624,-33.3929180164233,-32.8945162549841,
-32.396114493545,-31.8977127321058,-31.3993109706667,-30.9009092092275,
-30.4025074477884,-29.9041056863492,-29.4057039249101,-29.2256353728617),
 .UNSPECIFIED.);
#2846=B_SPLINE_CURVE_WITH_KNOTS('',3,(#66480,#66481,#66482,#66483,#66484,
#66485,#66486,#66487,#66488,#66489,#66490,#66491,#66492,#66493,#66494,#66495,
#66496,#66497,#66498,#66499,#66500,#66501,#66502,#66503,#66504,#66505,#66506,
#66507,#66508,#66509,#66510,#66511,#66512,#66513,#66514,#66515,#66516,#66517,
#66518,#66519,#66520,#66521,#66522),.UNSPECIFIED.,.F.,.F.,(4,3,3,3,3,3,
3,3,3,3,3,3,3,3,4),(26.2527986121202,26.4152933562751,26.9136951177143,
27.4120968791534,27.9104986405926,28.4089004020318,28.9073021634709,29.4057039249101,
29.9041056863492,30.4025074477884,30.9009092092275,31.3993109706667,31.8977127321058,
32.396114493545,32.5359839192998),.UNSPECIFIED.);
#2847=B_SPLINE_CURVE_WITH_KNOTS('',3,(#66527,#66528,#66529,#66530,#66531,
#66532,#66533,#66534,#66535,#66536,#66537,#66538,#66539,#66540,#66541,#66542,
#66543,#66544,#66545,#66546,#66547,#66548,#66549,#66550,#66551,#66552,#66553,
#66554,#66555,#66556,#66557,#66558,#66559,#66560,#66561,#66562,#66563,#66564,
#66565,#66566),.UNSPECIFIED.,.F.,.F.,(4,3,3,3,3,3,3,3,3,3,3,3,3,4),(-41.7920059872209,
-41.3673461994497,-40.8689444380106,-40.3705426765714,-39.8721409151323,
-39.3737391536931,-38.875337392254,-38.3769356308148,-37.8785338693757,
-37.3801321079365,-36.8817303464974,-36.3833285850582,-35.8849268236191,
-35.5088206800413),.UNSPECIFIED.);
#2848=B_SPLINE_CURVE_WITH_KNOTS('',3,(#66567,#66568,#66569,#66570,#66571,
#66572,#66573,#66574,#66575,#66576,#66577,#66578,#66579,#66580,#66581,#66582,
#66583,#66584,#66585,#66586,#66587,#66588,#66589,#66590,#66591,#66592,#66593,
#66594,#66595,#66596,#66597,#66598,#66599,#66600,#66601,#66602,#66603,#66604,
#66605,#66606),.UNSPECIFIED.,.F.,.F.,(4,3,3,3,3,3,3,3,3,3,3,3,3,4),(32.5359839192998,
32.8945162549841,33.3929180164233,33.8913197778625,34.3897215393016,34.8881233007408,
35.3865250621799,35.8849268236191,36.3833285850582,36.8817303464974,37.3801321079365,
37.8785338693757,38.3769356308148,38.8191692264794),.UNSPECIFIED.);
#2849=B_SPLINE_CURVE_WITH_KNOTS('',3,(#66611,#66612,#66613,#66614,#66615,
#66616,#66617,#66618,#66619,#66620,#66621,#66622,#66623,#66624,#66625,#66626,
#66627,#66628,#66629,#66630,#66631,#66632,#66633,#66634,#66635,#66636,#66637,
#66638,#66639,#66640,#66641,#66642,#66643,#66644,#66645,#66646,#66647,#66648,
#66649,#66650,#66651,#66652,#66653),.UNSPECIFIED.,.F.,.F.,(4,3,3,3,3,3,
3,3,3,3,3,3,3,3,4),(-48.0751912944005,-47.8465690981587,-47.3481673367196,
-46.8497655752804,-46.3513638138413,-45.8529620524021,-45.354560290963,
-44.8561585295238,-44.3577567680847,-43.8593550066455,-43.3609532452064,
-42.8625514837672,-42.3641497223281,-41.8657479608889,-41.7920059872209),
 .UNSPECIFIED.);
#2850=B_SPLINE_CURVE_WITH_KNOTS('',3,(#66654,#66655,#66656,#66657,#66658,
#66659,#66660,#66661,#66662,#66663,#66664,#66665,#66666,#66667,#66668,#66669,
#66670,#66671,#66672,#66673,#66674,#66675,#66676,#66677,#66678,#66679,#66680,
#66681,#66682,#66683,#66684,#66685,#66686,#66687,#66688,#66689,#66690,#66691,
#66692,#66693,#66694,#66695,#66696),.UNSPECIFIED.,.F.,.F.,(4,3,3,3,3,3,
3,3,3,3,3,3,3,3,4),(38.8191692264794,38.875337392254,39.3737391536931,39.8721409151323,
40.3705426765714,40.8689444380106,41.3673461994498,41.8657479608889,42.3641497223281,
42.8625514837672,43.3609532452064,43.8593550066455,44.3577567680847,44.8561585295238,
45.102354533659),.UNSPECIFIED.);
#2851=B_SPLINE_CURVE_WITH_KNOTS('',3,(#66701,#66702,#66703,#66704,#66705,
#66706,#66707,#66708,#66709,#66710,#66711,#66712,#66713,#66714,#66715,#66716,
#66717,#66718,#66719,#66720,#66721,#66722,#66723,#66724,#66725,#66726,#66727,
#66728,#66729,#66730,#66731,#66732,#66733,#66734,#66735,#66736,#66737,#66738,
#66739,#66740,#66741,#66742,#66743),.UNSPECIFIED.,.F.,.F.,(4,3,3,3,3,3,
3,3,3,3,3,3,3,3,4),(-54.3583766015801,-54.3257919968678,-53.8273902354286,
-53.3289884739894,-52.8305867125503,-52.3321849511111,-51.833783189672,
-51.3353814282328,-50.8369796667937,-50.3385779053545,-49.8401761439154,
-49.3417743824762,-48.8433726210371,-48.3449708595979,-48.0751912944005),
 .UNSPECIFIED.);
#2852=B_SPLINE_CURVE_WITH_KNOTS('',3,(#66744,#66745,#66746,#66747,#66748,
#66749,#66750,#66751,#66752,#66753,#66754,#66755,#66756,#66757,#66758,#66759,
#66760,#66761,#66762,#66763,#66764,#66765,#66766,#66767,#66768,#66769,#66770,
#66771,#66772,#66773,#66774,#66775,#66776,#66777,#66778,#66779,#66780,#66781,
#66782,#66783,#66784,#66785,#66786),.UNSPECIFIED.,.F.,.F.,(4,3,3,3,3,3,
3,3,3,3,3,3,3,3,4),(45.102354533659,45.354560290963,45.8529620524021,46.3513638138413,
46.8497655752804,47.3481673367196,47.8465690981588,48.3449708595979,48.8433726210371,
49.3417743824762,49.8401761439154,50.3385779053545,50.8369796667937,51.3353814282328,
51.3855398408386),.UNSPECIFIED.);
#2853=B_SPLINE_CURVE_WITH_KNOTS('',3,(#66791,#66792,#66793,#66794,#66795,
#66796,#66797,#66798,#66799,#66800,#66801,#66802,#66803,#66804,#66805,#66806,
#66807,#66808,#66809,#66810,#66811,#66812,#66813,#66814,#66815,#66816,#66817,
#66818,#66819,#66820,#66821,#66822,#66823,#66824,#66825,#66826,#66827,#66828,
#66829,#66830),.UNSPECIFIED.,.F.,.F.,(4,3,3,3,3,3,3,3,3,3,3,3,3,4),(-60.6415619087597,
-60.3066131341376,-59.8082113726984,-59.3098096112593,-58.8114078498201,
-58.313006088381,-57.8146043269418,-57.3162025655027,-56.8178008040635,
-56.3193990426244,-55.8209972811852,-55.3225955197461,-54.8241937583069,
-54.3583766015801),.UNSPECIFIED.);
#2854=B_SPLINE_CURVE_WITH_KNOTS('',3,(#66831,#66832,#66833,#66834,#66835,
#66836,#66837,#66838,#66839,#66840,#66841,#66842,#66843,#66844,#66845,#66846,
#66847,#66848,#66849,#66850,#66851,#66852,#66853,#66854,#66855,#66856,#66857,
#66858,#66859,#66860,#66861,#66862,#66863,#66864,#66865,#66866,#66867,#66868,
#66869,#66870),.UNSPECIFIED.,.F.,.F.,(4,3,3,3,3,3,3,3,3,3,3,3,3,4),(51.3855398408386,
51.833783189672,52.3321849511111,52.8305867125503,53.3289884739894,53.8273902354286,
54.3257919968677,54.8241937583069,55.3225955197461,55.8209972811852,56.3193990426244,
56.8178008040635,57.3162025655027,57.6687251480181),.UNSPECIFIED.);
#2855=B_SPLINE_CURVE_WITH_KNOTS('',3,(#66875,#66876,#66877,#66878,#66879,
#66880,#66881,#66882,#66883,#66884,#66885,#66886,#66887,#66888,#66889,#66890,
#66891,#66892,#66893,#66894,#66895,#66896,#66897,#66898,#66899,#66900,#66901,
#66902,#66903,#66904,#66905,#66906,#66907,#66908,#66909,#66910,#66911,#66912,
#66913,#66914,#66915,#66916,#66917),.UNSPECIFIED.,.F.,.F.,(4,3,3,3,3,3,
3,3,3,3,3,3,3,3,4),(-66.9247472159393,-66.7858360328466,-66.2874342714074,
-65.7890325099683,-65.2906307485291,-64.79222898709,-64.2938272256508,-63.7954254642117,
-63.2970237027725,-62.7986219413334,-62.3002201798942,-61.8018184184551,
-61.3034166570159,-60.8050148955767,-60.6415619087597),.UNSPECIFIED.);
#2856=B_SPLINE_CURVE_WITH_KNOTS('',3,(#66918,#66919,#66920,#66921,#66922,
#66923,#66924,#66925,#66926,#66927,#66928,#66929,#66930,#66931,#66932,#66933,
#66934,#66935,#66936,#66937,#66938,#66939,#66940,#66941,#66942,#66943,#66944,
#66945,#66946,#66947,#66948,#66949,#66950,#66951,#66952,#66953,#66954,#66955,
#66956,#66957,#66958,#66959,#66960),.UNSPECIFIED.,.F.,.F.,(4,3,3,3,3,3,
3,3,3,3,3,3,3,3,4),(57.6687251480181,57.8146043269418,58.313006088381,58.8114078498201,
59.3098096112593,59.8082113726984,60.3066131341376,60.8050148955767,61.3034166570159,
61.801818418455,62.3002201798942,62.7986219413334,63.2970237027725,63.7954254642117,
63.9519104551977),.UNSPECIFIED.);
#2857=B_SPLINE_CURVE_WITH_KNOTS('',3,(#66965,#66966,#66967,#66968,#66969,
#66970,#66971,#66972,#66973,#66974,#66975,#66976,#66977,#66978,#66979,#66980,
#66981,#66982,#66983,#66984,#66985,#66986,#66987,#66988,#66989,#66990,#66991,
#66992,#66993,#66994,#66995,#66996,#66997,#66998,#66999,#67000,#67001,#67002,
#67003,#67004),.UNSPECIFIED.,.F.,.F.,(4,3,3,3,3,3,3,3,3,3,3,3,3,4),(-73.2079325231189,
-72.7666571701164,-72.2682554086773,-71.7698536472381,-71.271451885799,
-70.7730501243598,-70.2746483629207,-69.7762466014815,-69.2778448400424,
-68.7794430786032,-68.2810413171641,-67.7826395557249,-67.2842377942858,
-66.9247472159393),.UNSPECIFIED.);
#2858=B_SPLINE_CURVE_WITH_KNOTS('',3,(#67005,#67006,#67007,#67008,#67009,
#67010,#67011,#67012,#67013,#67014,#67015,#67016,#67017,#67018,#67019,#67020,
#67021,#67022,#67023,#67024,#67025,#67026,#67027,#67028,#67029,#67030,#67031,
#67032,#67033,#67034,#67035,#67036,#67037,#67038,#67039,#67040,#67041,#67042,
#67043,#67044),.UNSPECIFIED.,.F.,.F.,(4,3,3,3,3,3,3,3,3,3,3,3,3,4),(63.9519104551977,
64.2938272256508,64.79222898709,65.2906307485291,65.7890325099683,66.2874342714074,
66.7858360328466,67.2842377942857,67.7826395557249,68.2810413171641,68.7794430786032,
69.2778448400424,69.7762466014815,70.2350957623773),.UNSPECIFIED.);
#2859=B_SPLINE_CURVE_WITH_KNOTS('',3,(#67049,#67050,#67051,#67052,#67053,
#67054,#67055,#67056,#67057,#67058,#67059,#67060,#67061,#67062,#67063,#67064,
#67065,#67066,#67067,#67068,#67069,#67070,#67071,#67072,#67073,#67074,#67075,
#67076,#67077,#67078,#67079,#67080,#67081,#67082,#67083,#67084,#67085,#67086,
#67087,#67088,#67089,#67090,#67091),.UNSPECIFIED.,.F.,.F.,(4,3,3,3,3,3,
3,3,3,3,3,3,3,3,4),(-79.4911178302985,-79.2458800688254,-78.7474783073863,
-78.2490765459471,-77.750674784508,-77.2522730230688,-76.7538712616297,
-76.2554695001905,-75.7570677387514,-75.2586659773122,-74.760264215873,
-74.2618624544339,-73.7634606929947,-73.2650589315556,-73.2079325231189),
 .UNSPECIFIED.);
#2860=B_SPLINE_CURVE_WITH_KNOTS('',3,(#67092,#67093,#67094,#67095,#67096,
#67097,#67098,#67099,#67100,#67101,#67102,#67103,#67104,#67105,#67106,#67107,
#67108,#67109,#67110,#67111,#67112,#67113,#67114,#67115,#67116,#67117,#67118,
#67119,#67120,#67121,#67122,#67123,#67124,#67125,#67126,#67127,#67128,#67129,
#67130,#67131,#67132,#67133,#67134),.UNSPECIFIED.,.F.,.F.,(4,3,3,3,3,3,
3,3,3,3,3,3,3,3,4),(70.2350957623773,70.2746483629207,70.7730501243598,
71.271451885799,71.7698536472381,72.2682554086773,72.7666571701164,73.2650589315556,
73.7634606929947,74.2618624544339,74.760264215873,75.2586659773122,75.7570677387513,
76.2554695001905,76.5182810695569),.UNSPECIFIED.);
#2861=B_SPLINE_CURVE_WITH_KNOTS('',3,(#67139,#67140,#67141,#67142,#67143,
#67144,#67145,#67146,#67147,#67148,#67149,#67150,#67151,#67152,#67153,#67154,
#67155,#67156,#67157,#67158,#67159,#67160,#67161,#67162,#67163,#67164,#67165,
#67166,#67167,#67168,#67169,#67170,#67171,#67172,#67173,#67174,#67175,#67176,
#67177,#67178,#67179,#67180,#67181),.UNSPECIFIED.,.F.,.F.,(4,3,3,3,3,3,
3,3,3,3,3,3,3,3,4),(-85.774303137478,-85.7251029675344,-85.2267012060953,
-84.7282994446561,-84.229897683217,-83.7314959217778,-83.2330941603387,
-82.7346923988995,-82.2362906374604,-81.7378888760212,-81.239487114582,
-80.7410853531429,-80.2426835917038,-79.7442818302646,-79.4911178302985),
 .UNSPECIFIED.);
#2862=B_SPLINE_CURVE_WITH_KNOTS('',3,(#67182,#67183,#67184,#67185,#67186,
#67187,#67188,#67189,#67190,#67191,#67192,#67193,#67194,#67195,#67196,#67197,
#67198,#67199,#67200,#67201,#67202,#67203,#67204,#67205,#67206,#67207,#67208,
#67209,#67210,#67211,#67212,#67213,#67214,#67215,#67216,#67217,#67218,#67219,
#67220,#67221,#67222,#67223,#67224),.UNSPECIFIED.,.F.,.F.,(4,3,3,3,3,3,
3,3,3,3,3,3,3,3,4),(76.5182810695569,76.7538712616297,77.2522730230688,
77.750674784508,78.2490765459471,78.7474783073863,79.2458800688254,79.7442818302646,
80.2426835917037,80.7410853531429,81.239487114582,81.7378888760212,82.2362906374604,
82.7346923988995,82.8014663767365),.UNSPECIFIED.);
#2863=B_SPLINE_CURVE_WITH_KNOTS('',3,(#67229,#67230,#67231,#67232,#67233,
#67234,#67235,#67236,#67237,#67238,#67239,#67240,#67241,#67242,#67243,#67244,
#67245,#67246,#67247,#67248,#67249,#67250,#67251,#67252,#67253,#67254,#67255,
#67256,#67257,#67258,#67259,#67260,#67261,#67262,#67263,#67264,#67265,#67266,
#67267,#67268),.UNSPECIFIED.,.F.,.F.,(4,3,3,3,3,3,3,3,3,3,3,3,3,4),(-92.0574884446577,
-91.7059241048043,-91.2075223433651,-90.709120581926,-90.2107188204868,
-89.7123170590477,-89.2139152976085,-88.7155135361694,-88.2171117747302,
-87.718710013291,-87.2203082518519,-86.7219064904127,-86.2235047289736,
-85.774303137478),.UNSPECIFIED.);
#2864=B_SPLINE_CURVE_WITH_KNOTS('',3,(#67269,#67270,#67271,#67272,#67273,
#67274,#67275,#67276,#67277,#67278,#67279,#67280,#67281,#67282,#67283,#67284,
#67285,#67286,#67287,#67288,#67289,#67290,#67291,#67292,#67293,#67294,#67295,
#67296,#67297,#67298,#67299,#67300,#67301,#67302,#67303,#67304,#67305,#67306,
#67307,#67308),.UNSPECIFIED.,.F.,.F.,(4,3,3,3,3,3,3,3,3,3,3,3,3,4),(82.8014663767365,
83.2330941603387,83.7314959217778,84.229897683217,84.7282994446561,85.2267012060953,
85.7251029675344,86.2235047289736,86.7219064904127,87.2203082518519,87.718710013291,
88.2171117747302,88.7155135361694,89.0846516839161),.UNSPECIFIED.);
#2865=B_SPLINE_CURVE_WITH_KNOTS('',3,(#67313,#67314,#67315,#67316,#67317,
#67318,#67319,#67320,#67321,#67322,#67323,#67324,#67325,#67326,#67327,#67328,
#67329,#67330,#67331,#67332,#67333,#67334,#67335,#67336,#67337,#67338,#67339,
#67340,#67341,#67342,#67343,#67344,#67345,#67346,#67347,#67348,#67349,#67350,
#67351,#67352,#67353,#67354,#67355),.UNSPECIFIED.,.F.,.F.,(4,3,3,3,3,3,
3,3,3,3,3,3,3,3,4),(-98.3406737518372,-98.1851470035133,-97.6867452420741,
-97.188343480635,-96.6899417191958,-96.1915399577567,-95.6931381963175,
-95.1947364348784,-94.6963346734392,-94.197932912,-93.6995311505609,-93.2011293891217,
-92.7027276276826,-92.2043258662434,-92.0574884446577),.UNSPECIFIED.);
#2866=B_SPLINE_CURVE_WITH_KNOTS('',3,(#67356,#67357,#67358,#67359,#67360,
#67361,#67362,#67363,#67364,#67365,#67366,#67367,#67368,#67369,#67370,#67371,
#67372,#67373,#67374,#67375,#67376,#67377,#67378,#67379,#67380,#67381,#67382,
#67383,#67384,#67385,#67386,#67387,#67388,#67389,#67390,#67391,#67392,#67393,
#67394,#67395,#67396,#67397,#67398),.UNSPECIFIED.,.F.,.F.,(4,3,3,3,3,3,
3,3,3,3,3,3,3,3,4),(89.0846516839161,89.2139152976085,89.7123170590477,
90.2107188204868,90.709120581926,91.2075223433651,91.7059241048043,92.2043258662434,
92.7027276276826,93.2011293891217,93.6995311505609,94.197932912,94.6963346734392,
95.1947364348784,95.3678369910957),.UNSPECIFIED.);
#2867=B_SPLINE_CURVE_WITH_KNOTS('',3,(#67404,#67405,#67406,#67407),
 .UNSPECIFIED.,.F.,.F.,(4,4),(109.955742875643,110.220866060559),
 .UNSPECIFIED.);
#2868=B_SPLINE_CURVE_WITH_KNOTS('',3,(#67413,#67414,#67415,#67416,#67417,
#67418,#67419,#67420,#67421,#67422,#67423,#67424,#67425,#67426,#67427,#67428,
#67429),.UNSPECIFIED.,.F.,.F.,(4,1,1,1,1,1,1,1,1,1,1,1,1,1,4),(103.672557568463,
103.819394990049,104.317796751488,104.816198512927,105.314600274366,105.813002035806,
106.311403797245,106.809805558684,107.308207320123,107.806609081562,108.305010843001,
108.80341260444,109.30181436588,109.800216127319,109.955742875643),
 .UNSPECIFIED.);
#2869=B_SPLINE_CURVE_WITH_KNOTS('',3,(#67432,#67433,#67434,#67435,#67436,
#67437,#67438,#67439,#67440,#67441,#67442,#67443,#67444,#67445),
 .UNSPECIFIED.,.F.,.F.,(4,1,1,1,1,1,1,1,1,1,1,4),(103.672557568463,103.997858773685,
104.496260535124,104.994662296563,105.493064058002,105.991465819441,106.489867580881,
106.98826934232,107.486671103759,107.985072865198,108.483474626637,108.981876388076),
 .UNSPECIFIED.);
#2870=B_SPLINE_CURVE_WITH_KNOTS('',3,(#67450,#67451,#67452,#67453,#67454,
#67455,#67456,#67457,#67458,#67459,#67460,#67461,#67462,#67463,#67464,#67465),
 .UNSPECIFIED.,.F.,.F.,(4,1,1,1,1,1,1,1,1,1,1,1,1,4),(97.3893722612836,
97.8385738527791,98.3369756142182,98.8353773756574,99.3337791370966,99.8321808985357,
100.330582659975,100.828984421414,101.327386182853,101.825787944292,102.324189705731,
102.822591467171,103.32099322861,103.672557568463),.UNSPECIFIED.);
#2871=B_SPLINE_CURVE_WITH_KNOTS('',3,(#67466,#67467,#67468,#67469,#67470,
#67471,#67472,#67473,#67474,#67475,#67476,#67477,#67478,#67479,#67480,#67481,
#67482),.UNSPECIFIED.,.F.,.F.,(4,1,1,1,1,1,1,1,1,1,1,1,1,1,4),(97.3893722612836,
97.5186358749759,98.017037636415,98.5154393978542,99.0138411592933,99.5122429207325,
100.010644682172,100.509046443611,101.00744820505,101.505849966489,102.004251727928,
102.502653489367,103.001055250807,103.499457012246,103.672557568463),
 .UNSPECIFIED.);
#2872=B_SPLINE_CURVE_WITH_KNOTS('',3,(#67487,#67488,#67489,#67490,#67491,
#67492,#67493,#67494,#67495,#67496,#67497,#67498,#67499,#67500,#67501,#67502,
#67503),.UNSPECIFIED.,.F.,.F.,(4,1,1,1,1,1,1,1,1,1,1,1,1,1,4),(91.106186954104,
91.3593509540701,91.8577527155093,92.3561544769484,92.8545562383876,93.3529579998267,
93.8513597612659,94.349761522705,94.8481632841442,95.3465650455833,95.8449668070225,
96.3433685684616,96.8417703299008,97.34017209134,97.3893722612836),
 .UNSPECIFIED.);
#2873=B_SPLINE_CURVE_WITH_KNOTS('',3,(#67504,#67505,#67506,#67507,#67508,
#67509,#67510,#67511,#67512,#67513,#67514,#67515,#67516,#67517,#67518,#67519),
 .UNSPECIFIED.,.F.,.F.,(4,1,1,1,1,1,1,1,1,1,1,1,1,4),(91.106186954104,91.537814737706,
92.0362164991452,92.5346182605844,93.0330200220235,93.5314217834626,94.0298235449018,
94.528225306341,95.0266270677801,95.5250288292193,96.0234305906584,96.5218323520976,
97.0202341135367,97.3893722612836),.UNSPECIFIED.);
#2874=B_SPLINE_CURVE_WITH_KNOTS('',3,(#67524,#67525,#67526,#67527,#67528,
#67529,#67530,#67531,#67532,#67533,#67534,#67535,#67536,#67537,#67538,#67539,
#67540),.UNSPECIFIED.,.F.,.F.,(4,1,1,1,1,1,1,1,1,1,1,1,1,1,4),(84.8230016469244,
84.8801280553611,85.3785298168003,85.8769315782394,86.3753333396786,86.8737351011177,
87.3721368625569,87.870538623996,88.3689403854352,88.8673421468743,89.3657439083135,
89.8641456697526,90.3625474311918,90.860949192631,91.106186954104),
 .UNSPECIFIED.);
#2875=B_SPLINE_CURVE_WITH_KNOTS('',3,(#67541,#67542,#67543,#67544,#67545,
#67546,#67547,#67548,#67549,#67550,#67551,#67552,#67553,#67554,#67555,#67556,
#67557),.UNSPECIFIED.,.F.,.F.,(4,1,1,1,1,1,1,1,1,1,1,1,1,1,4),(84.8230016469244,
85.058591838997,85.5569936004362,86.0553953618753,86.5537971233145,87.0521988847537,
87.5506006461928,88.049002407632,88.5474041690711,89.0458059305103,89.5442076919494,
90.0426094533886,90.5410112148277,91.0394129762669,91.106186954104),
 .UNSPECIFIED.);
#2876=B_SPLINE_CURVE_WITH_KNOTS('',3,(#67562,#67563,#67564,#67565,#67566,
#67567,#67568,#67569,#67570,#67571,#67572,#67573,#67574,#67575,#67576,#67577),
 .UNSPECIFIED.,.F.,.F.,(4,1,1,1,1,1,1,1,1,1,1,1,1,4),(78.5398163397448,
78.8993069180913,79.3977086795304,79.8961104409696,80.3945122024087,80.8929139638479,
81.391315725287,81.8897174867262,82.3881192481653,82.8865210096045,83.3849227710436,
83.8833245324828,84.381726293922,84.8230016469244),.UNSPECIFIED.);
#2877=B_SPLINE_CURVE_WITH_KNOTS('',3,(#67578,#67579,#67580,#67581,#67582,
#67583,#67584,#67585,#67586,#67587,#67588,#67589,#67590,#67591,#67592,#67593,
#67594),.UNSPECIFIED.,.F.,.F.,(4,1,1,1,1,1,1,1,1,1,1,1,1,1,4),(78.5398163397448,
78.579368940288,79.0777707017272,79.5761724631663,80.0745742246055,80.5729759860447,
81.0713777474838,81.569779508923,82.0681812703621,82.5665830318013,83.0649847932404,
83.5633865546796,84.0617883161187,84.5601900775579,84.8230016469244),
 .UNSPECIFIED.);
#2878=B_SPLINE_CURVE_WITH_KNOTS('',3,(#67599,#67600,#67601,#67602,#67603,
#67604,#67605,#67606,#67607,#67608,#67609,#67610,#67611,#67612,#67613,#67614,
#67615),.UNSPECIFIED.,.F.,.F.,(4,1,1,1,1,1,1,1,1,1,1,1,1,1,4),(72.2566310325652,
72.4200840193823,72.9184857808214,73.4168875422606,73.9152893036997,74.4136910651389,
74.912092826578,75.4104945880172,75.9088963494563,76.4072981108955,76.9056998723347,
77.4041016337738,77.902503395213,78.4009051566521,78.5398163397448),
 .UNSPECIFIED.);
#2879=B_SPLINE_CURVE_WITH_KNOTS('',3,(#67616,#67617,#67618,#67619,#67620,
#67621,#67622,#67623,#67624,#67625,#67626,#67627,#67628,#67629,#67630,#67631),
 .UNSPECIFIED.,.F.,.F.,(4,1,1,1,1,1,1,1,1,1,1,1,1,4),(72.2566310325652,
72.5985478030182,73.0969495644573,73.5953513258965,74.0937530873357,74.5921548487748,
75.090556610214,75.5889583716531,76.0873601330923,76.5857618945314,77.0841636559706,
77.5825654174097,78.0809671788489,78.5398163397448),.UNSPECIFIED.);
#2880=B_SPLINE_CURVE_WITH_KNOTS('',3,(#67636,#67637,#67638,#67639,#67640,
#67641,#67642,#67643,#67644,#67645,#67646,#67647,#67648,#67649,#67650,#67651),
 .UNSPECIFIED.,.F.,.F.,(4,1,1,1,1,1,1,1,1,1,1,1,1,4),(65.9734457253856,
66.4392628821124,66.9376646435516,67.4360664049907,67.9344681664299,68.432869927869,
68.9312716893082,69.4296734507473,69.9280752121865,70.4264769736257,70.9248787350648,
71.4232804965039,71.9216822579431,72.2566310325652),.UNSPECIFIED.);
#2881=B_SPLINE_CURVE_WITH_KNOTS('',3,(#67652,#67653,#67654,#67655,#67656,
#67657,#67658,#67659,#67660,#67661,#67662,#67663,#67664,#67665,#67666,#67667,
#67668),.UNSPECIFIED.,.F.,.F.,(4,1,1,1,1,1,1,1,1,1,1,1,1,1,4),(65.9734457253856,
66.1193249043092,66.6177266657484,67.1161284271875,67.6145301886267,68.1129319500658,
68.611333711505,69.1097354729441,69.6081372343833,70.1065389958224,70.6049407572616,
71.1033425187007,71.6017442801399,72.1001460415791,72.2566310325652),
 .UNSPECIFIED.);
#2882=B_SPLINE_CURVE_WITH_KNOTS('',3,(#67673,#67674,#67675,#67676,#67677,
#67678,#67679,#67680,#67681,#67682,#67683,#67684,#67685,#67686,#67687,#67688,
#67689),.UNSPECIFIED.,.F.,.F.,(4,1,1,1,1,1,1,1,1,1,1,1,1,1,4),(59.690260418206,
59.9600399834034,60.4584417448426,60.9568435062817,61.4552452677209,61.95364702916,
62.4520487905992,62.9504505520383,63.4488523134775,63.9472540749166,64.4456558363558,
64.944057597795,65.4424593592341,65.9408611206733,65.9734457253856),
 .UNSPECIFIED.);
#2883=B_SPLINE_CURVE_WITH_KNOTS('',3,(#67690,#67691,#67692,#67693,#67694,
#67695,#67696,#67697,#67698,#67699,#67700,#67701,#67702,#67703,#67704,#67705),
 .UNSPECIFIED.,.F.,.F.,(4,1,1,1,1,1,1,1,1,1,1,1,1,4),(59.690260418206,60.1385037670394,
60.6369055284785,61.1353072899177,61.6337090513568,62.132110812796,62.6305125742351,
63.1289143356743,63.6273160971134,64.1257178585526,64.6241196199917,65.1225213814309,
65.6209231428701,65.9734457253856),.UNSPECIFIED.);
#2884=B_SPLINE_CURVE_WITH_KNOTS('',3,(#67710,#67711,#67712,#67713,#67714,
#67715,#67716,#67717,#67718,#67719,#67720,#67721,#67722,#67723,#67724,#67725,
#67726),.UNSPECIFIED.,.F.,.F.,(4,1,1,1,1,1,1,1,1,1,1,1,1,1,4),(53.4070751110264,
53.4808170846944,53.9792188461336,54.4776206075727,54.9760223690119,55.474424130451,
55.9728258918902,56.4712276533293,56.9696294147685,57.4680311762077,57.9664329376468,
58.464834699086,58.9632364605251,59.4616382219643,59.690260418206),
 .UNSPECIFIED.);
#2885=B_SPLINE_CURVE_WITH_KNOTS('',3,(#67727,#67728,#67729,#67730,#67731,
#67732,#67733,#67734,#67735,#67736,#67737,#67738,#67739,#67740,#67741,#67742,
#67743),.UNSPECIFIED.,.F.,.F.,(4,1,1,1,1,1,1,1,1,1,1,1,1,1,4),(53.4070751110264,
53.6592808683304,54.1576826297695,54.6560843912087,55.1544861526478,55.652887914087,
56.1512896755261,56.6496914369653,57.1480931984044,57.6464949598436,58.1448967212827,
58.6432984827219,59.1417002441611,59.6401020056002,59.690260418206),
 .UNSPECIFIED.);
#2886=B_SPLINE_CURVE_WITH_KNOTS('',3,(#67748,#67749,#67750,#67751,#67752,
#67753,#67754,#67755,#67756,#67757,#67758,#67759,#67760,#67761,#67762,#67763),
 .UNSPECIFIED.,.F.,.F.,(4,1,1,1,1,1,1,1,1,1,1,1,1,4),(47.1238898038469,
47.4999959474246,47.9983977088637,48.4967994703029,48.995201231742,49.4936029931812,
49.9920047546203,50.4904065160595,50.9888082774987,51.4872100389378,51.985611800377,
52.4840135618161,52.9824153232553,53.4070751110264),.UNSPECIFIED.);
#2887=B_SPLINE_CURVE_WITH_KNOTS('',3,(#67764,#67765,#67766,#67767,#67768,
#67769,#67770,#67771,#67772,#67773,#67774,#67775,#67776,#67777,#67778,#67779,
#67780),.UNSPECIFIED.,.F.,.F.,(4,1,1,1,1,1,1,1,1,1,1,1,1,1,4),(47.1238898038468,
47.1800579696214,47.6784597310605,48.1768614924997,48.6752632539388,49.173665015378,
49.6720667768171,50.1704685382563,50.6688702996954,51.1672720611346,51.6656738225738,
52.1640755840129,52.6624773454521,53.1608791068912,53.4070751110264),
 .UNSPECIFIED.);
#2888=B_SPLINE_CURVE_WITH_KNOTS('',3,(#67785,#67786,#67787,#67788,#67789,
#67790,#67791,#67792,#67793,#67794,#67795,#67796,#67797,#67798,#67799,#67800,
#67801),.UNSPECIFIED.,.F.,.F.,(4,1,1,1,1,1,1,1,1,1,1,1,1,1,4),(40.8407044966672,
41.0207730487156,41.5191748101547,42.0175765715939,42.515978333033,43.0143800944722,
43.5127818559113,44.0111836173505,44.5095853787897,45.0079871402288,45.506388901668,
46.0047906631071,46.5031924245463,47.0015941859854,47.1238898038469),
 .UNSPECIFIED.);
#2889=B_SPLINE_CURVE_WITH_KNOTS('',3,(#67802,#67803,#67804,#67805,#67806,
#67807,#67808,#67809,#67810,#67811,#67812,#67813,#67814,#67815,#67816,#67817),
 .UNSPECIFIED.,.F.,.F.,(4,1,1,1,1,1,1,1,1,1,1,1,1,4),(40.8407044966672,
41.1992368323515,41.6976385937907,42.1960403552298,42.694442116669,43.1928438781081,
43.6912456395473,44.1896474009864,44.6880491624256,45.1864509238648,45.6848526853039,
46.1832544467431,46.6816562081822,47.1238898038468),.UNSPECIFIED.);
#2890=B_SPLINE_CURVE_WITH_KNOTS('',3,(#67822,#67823,#67824,#67825,#67826,
#67827,#67828,#67829,#67830,#67831,#67832,#67833,#67834,#67835,#67836,#67837),
 .UNSPECIFIED.,.F.,.F.,(4,1,1,1,1,1,1,1,1,1,1,1,1,4),(34.5575191894876,
35.0399519114457,35.5383536728849,36.036755434324,36.5351571957632,37.0335589572024,
37.5319607186415,38.0303624800807,38.5287642415198,39.027166002959,39.5255677643981,
40.0239695258373,40.5223712872764,40.8407044966672),.UNSPECIFIED.);
#2891=B_SPLINE_CURVE_WITH_KNOTS('',3,(#67838,#67839,#67840,#67841,#67842,
#67843,#67844,#67845,#67846,#67847,#67848,#67849,#67850,#67851,#67852,#67853,
#67854),.UNSPECIFIED.,.F.,.F.,(4,1,1,1,1,1,1,1,1,1,1,1,1,1,4),(34.5575191894876,
34.7200139336425,35.2184156950817,35.7168174565208,36.21521921796,36.7136209793991,
37.2120227408383,37.7104245022774,38.2088262637166,38.7072280251558,39.2056297865949,
39.7040315480341,40.2024333094732,40.7008350709124,40.8407044966672),
 .UNSPECIFIED.);
#2892=B_SPLINE_CURVE_WITH_KNOTS('',3,(#67859,#67860,#67861,#67862,#67863,
#67864,#67865,#67866,#67867,#67868,#67869,#67870,#67871,#67872,#67873,#67874,
#67875),.UNSPECIFIED.,.F.,.F.,(4,1,1,1,1,1,1,1,1,1,1,1,1,1,4),(28.2743338823081,
28.5607290127367,29.0591307741759,29.5575325356151,30.0559342970542,30.5543360584934,
31.0527378199325,31.5511395813717,32.0495413428108,32.54794310425,33.0463448656891,
33.5447466271283,34.0431483885674,34.5415501500066,34.5575191894876),
 .UNSPECIFIED.);
#2893=B_SPLINE_CURVE_WITH_KNOTS('',3,(#67876,#67877,#67878,#67879,#67880,
#67881,#67882,#67883,#67884,#67885,#67886,#67887,#67888,#67889,#67890,#67891),
 .UNSPECIFIED.,.F.,.F.,(4,1,1,1,1,1,1,1,1,1,1,1,1,4),(28.2743338823081,
28.7391927963727,29.2375945578118,29.735996319251,30.2343980806901,30.7327998421293,
31.2312016035684,31.7296033650076,32.2280051264468,32.7264068878859,33.2248086493251,
33.7232104107642,34.2216121722034,34.5575191894876),.UNSPECIFIED.);
#2894=B_SPLINE_CURVE_WITH_KNOTS('',3,(#67896,#67897,#67898,#67899,#67900,
#67901,#67902,#67903,#67904,#67905,#67906,#67907,#67908,#67909,#67910,#67911,
#67912),.UNSPECIFIED.,.F.,.F.,(4,1,1,1,1,1,1,1,1,1,1,1,1,1,4),(21.9911485751285,
22.0815061140277,22.5799078754669,23.0783096369061,23.5767113983452,24.0751131597844,
24.5735149212235,25.0719166826627,25.5703184441018,26.068720205541,26.5671219669801,
27.0655237284193,27.5639254898584,28.0623272512976,28.2743338823081),
 .UNSPECIFIED.);
#2895=B_SPLINE_CURVE_WITH_KNOTS('',3,(#67913,#67914,#67915,#67916,#67917,
#67918,#67919,#67920,#67921,#67922,#67923,#67924,#67925,#67926,#67927,#67928,
#67929),.UNSPECIFIED.,.F.,.F.,(4,1,1,1,1,1,1,1,1,1,1,1,1,1,4),(21.9911485751285,
22.2599698976637,22.7583716591028,23.256773420542,23.7551751819811,24.2535769434203,
24.7519787048595,25.2503804662986,25.7487822277378,26.2471839891769,26.7455857506161,
27.2439875120552,27.7423892734944,28.2407910349335,28.2743338823081),
 .UNSPECIFIED.);
#2896=B_SPLINE_CURVE_WITH_KNOTS('',3,(#67934,#67935,#67936,#67937,#67938,
#67939,#67940,#67941,#67942,#67943,#67944,#67945,#67946,#67947,#67948,#67949),
 .UNSPECIFIED.,.F.,.F.,(4,1,1,1,1,1,1,1,1,1,1,1,1,4),(15.7079632679489,
16.1006849767579,16.5990867381971,17.0974884996362,17.5958902610754,18.0942920225145,
18.5926937839537,19.0910955453928,19.589497306832,20.0878990682711,20.5863008297103,
21.0847025911494,21.5831043525886,21.9911485751285),.UNSPECIFIED.);
#2897=B_SPLINE_CURVE_WITH_KNOTS('',3,(#67950,#67951,#67952,#67953,#67954,
#67955,#67956,#67957,#67958,#67959,#67960,#67961,#67962,#67963,#67964,#67965,
#67966),.UNSPECIFIED.,.F.,.F.,(4,1,1,1,1,1,1,1,1,1,1,1,1,1,4),(15.7079632679489,
15.7807469989547,16.2791487603938,16.777550521833,17.2759522832721,17.7743540447113,
18.2727558061505,18.7711575675896,19.2695593290288,19.7679610904679,20.2663628519071,
20.7647646133462,21.2631663747854,21.7615681362245,21.9911485751285),
 .UNSPECIFIED.);
#2898=B_SPLINE_CURVE_WITH_KNOTS('',3,(#67983,#67984,#67985,#67986,#67987,
#67988),.UNSPECIFIED.,.F.,.F.,(4,2,4),(0.164470082438344,0.176405072826056,
0.235193913087612),.UNSPECIFIED.);
#2899=B_SPLINE_CURVE_WITH_KNOTS('',3,(#67990,#67991,#67992,#67993,#67994,
#67995),.UNSPECIFIED.,.F.,.F.,(4,2,4),(0.235193913087612,0.293982753349168,
0.30591774373688),.UNSPECIFIED.);
#2900=B_SPLINE_CURVE_WITH_KNOTS('',3,(#67999,#68000,#68001,#68002,#68003,
#68004,#68005,#68006,#68007,#68008),.UNSPECIFIED.,.F.,.F.,(4,2,2,2,4),(0.634857908613568,
0.64679289900128,0.705581739262836,0.764370579524392,0.776305569912104),
 .UNSPECIFIED.);
#2901=B_SPLINE_CURVE_WITH_KNOTS('',3,(#68132,#68133,#68134,#68135,#68136,
#68137,#68138,#68139,#68140,#68141,#68142,#68143,#68144,#68145,#68146,#68147,
#68148,#68149,#68150,#68151,#68152,#68153),.UNSPECIFIED.,.F.,.F.,(4,1,2,
1,1,1,2,2,2,1,1,1,1,1,1,4),(0.,0.0584568917522064,0.116913783504413,0.175370117903373,
0.233826452302333,0.263054619501813,0.350739121100252,0.409196012852459,
0.467652904604665,0.526109517680248,0.569951977486936,0.584566130755832,
0.672251050369206,0.686865203638102,0.69417228027255,0.701479356906998),
 .UNSPECIFIED.);
#2902=B_SPLINE_CURVE_WITH_KNOTS('',3,(#68154,#68155,#68156,#68157,#68158,
#68159,#68160,#68161),.UNSPECIFIED.,.F.,.F.,(4,1,1,1,1,4),(0.701479356906998,
0.774550123251477,0.818392583058164,0.847620889595956,0.876849196133747,
0.93530580920933),.UNSPECIFIED.);
#2903=B_SPLINE_CURVE_WITH_KNOTS('',3,(#68162,#68163,#68164,#68165,#68166,
#68167,#68168,#68169,#68170,#68171,#68172,#68173,#68174,#68175,#68176,#68177,
#68178,#68179,#68180,#68181,#68182,#68183,#68184,#68185,#68186,#68187,#68188),
 .UNSPECIFIED.,.T.,.F.,(4,1,1,1,1,1,1,1,1,1,1,1,2,2,2,1,1,1,2,1,4),(-0.93530580920933,
-0.876849196133747,-0.847620889595956,-0.818392583058164,-0.774550123251477,
-0.701479356906998,-0.69417228027255,-0.686865203638102,-0.672251050369206,
-0.584566130755832,-0.569951977486936,-0.526109517680248,-0.467652904604665,
-0.409196012852459,-0.350739121100252,-0.263054619501813,-0.233826452302333,
-0.175370117903373,-0.116913783504413,-0.0584568917522064,0.),
 .UNSPECIFIED.);
#2904=B_SPLINE_CURVE_WITH_KNOTS('',3,(#69020,#69021,#69022,#69023,#69024,
#69025,#69026,#69027,#69028,#69029,#69030,#69031,#69032,#69033,#69034,#69035,
#69036,#69037,#69038,#69039,#69040,#69041,#69042,#69043,#69044,#69045,#69046,
#69047,#69048,#69049,#69050,#69051,#69052,#69053,#69054,#69055,#69056,#69057,
#69058,#69059,#69060,#69061,#69062,#69063,#69064,#69065,#69066,#69067,#69068,
#69069,#69070,#69071,#69072,#69073,#69074,#69075,#69076,#69077,#69078,#69079,
#69080,#69081,#69082,#69083,#69084,#69085,#69086,#69087,#69088,#69089,#69090,
#69091,#69092,#69093,#69094,#69095,#69096,#69097,#69098,#69099,#69100,#69101,
#69102,#69103,#69104,#69105,#69106,#69107,#69108,#69109,#69110,#69111,#69112,
#69113,#69114,#69115,#69116,#69117,#69118,#69119,#69120,#69121,#69122,#69123,
#69124,#69125,#69126,#69127,#69128,#69129,#69130,#69131,#69132,#69133,#69134),
 .UNSPECIFIED.,.F.,.F.,(4,3,3,3,3,3,3,3,3,3,3,3,3,3,3,3,3,3,3,3,3,3,3,3,
3,3,3,3,3,3,3,3,3,3,3,3,3,3,4),(-1.36616069392046,-1.31234511237088,-1.25590688369221,
-1.22043336320159,-1.19978988322529,-1.18977195970498,-1.18171686644571,
-1.12581307785687,-1.07017593161874,-1.02114732569299,-1.0124506254895,
-1.00557445843696,-0.972118719767242,-0.917136617675091,-0.861845521301615,
-0.806301914613285,-0.764644209597037,-0.752957249475711,-0.746332111135441,
-0.691988100457753,-0.639671094548295,-0.585206903159839,-0.530950162134808,
-0.504026220241107,-0.496690883172722,-0.490851144198066,-0.437265553293869,
-0.383730648991155,-0.330847439887809,-0.315558626985201,-0.276113798612051,
-0.258856686198798,-0.248596553131286,-0.240631547682685,-0.188137041660069,
-0.135346646621427,-0.0828734739367624,-0.0314201096525192,0.),
 .UNSPECIFIED.);
#2905=B_SPLINE_CURVE_WITH_KNOTS('',3,(#69135,#69136,#69137,#69138,#69139,
#69140,#69141,#69142,#69143,#69144,#69145,#69146,#69147,#69148,#69149,#69150,
#69151,#69152,#69153,#69154,#69155,#69156),.UNSPECIFIED.,.F.,.F.,(4,3,3,
3,3,3,3,4),(95.3678369910957,95.6931381963175,96.1915399577567,96.6899417191958,
97.188343480635,97.6867452420741,98.1851470035133,98.6057969367535),
 .UNSPECIFIED.);
#2906=B_SPLINE_CURVE_WITH_KNOTS('',3,(#69158,#69159,#69160,#69161,#69162,
#69163,#69164,#69165,#69166,#69167,#69168,#69169,#69170,#69171,#69172,#69173,
#69174,#69175,#69176,#69177,#69178,#69179,#69180,#69181,#69182,#69183,#69184,
#69185,#69186,#69187,#69188,#69189,#69190,#69191,#69192,#69193,#69194,#69195,
#69196,#69197,#69198,#69199,#69200,#69201,#69202,#69203,#69204,#69205,#69206,
#69207,#69208,#69209,#69210,#69211,#69212,#69213,#69214,#69215,#69216,#69217,
#69218,#69219,#69220,#69221,#69222,#69223,#69224,#69225,#69226,#69227,#69228,
#69229,#69230,#69231,#69232,#69233,#69234,#69235,#69236,#69237,#69238,#69239,
#69240,#69241,#69242,#69243,#69244,#69245,#69246,#69247,#69248,#69249,#69250,
#69251,#69252,#69253,#69254,#69255,#69256,#69257,#69258,#69259,#69260,#69261,
#69262,#69263,#69264,#69265,#69266,#69267,#69268,#69269),.UNSPECIFIED.,
 .F.,.F.,(4,3,3,3,3,3,3,3,3,3,3,3,3,3,3,3,3,3,3,3,3,3,3,3,3,3,3,3,3,3,3,
3,3,3,3,3,3,4),(-1.3692760959275,-1.32059746496365,-1.26831585127865,-1.23521527309061,
-1.21194803095155,-1.20083137328431,-1.14767293878112,-1.09434061971044,
-1.04892592274238,-1.04156502142363,-1.0342810920432,-1.00351122577432,
-0.950462707727008,-0.896724595787321,-0.841890453382919,-0.800764846579617,
-0.789580710740268,-0.783394562059837,-0.728633107476855,-0.677388026169712,
-0.622874329736254,-0.568068343407881,-0.53991042266811,-0.531693285272613,
-0.524470610547756,-0.469207417019949,-0.413568213634201,-0.358037807451751,
-0.342804977489712,-0.299954355303498,-0.281207208097029,-0.270867643373009,
-0.263531854817724,-0.208138358731652,-0.151751170205445,-0.0952554154038859,
-0.0393377089155784,0.),.UNSPECIFIED.);
#2907=B_SPLINE_CURVE_WITH_KNOTS('',3,(#69270,#69271,#69272,#69273,#69274,
#69275,#69276,#69277,#69278,#69279,#69280,#69281,#69282,#69283),
 .UNSPECIFIED.,.F.,.F.,(4,1,1,1,1,1,1,1,1,1,1,4),(10.3760794513229,10.7967293845631,
11.2951311460023,11.7935329074415,12.2919346688806,12.7903364303198,13.2887381917589,
13.7871399531981,14.2855417146372,14.7839434760764,15.2823452375155,15.7079632679489),
 .UNSPECIFIED.);
#2908=B_SPLINE_CURVE_WITH_KNOTS('',3,(#69289,#69290,#69291,#69292,#69293,
#69294,#69295,#69296,#69297,#69298,#69299,#69300,#69301,#69302,#69303,#69304,
#69305,#69306,#69307,#69308,#69309,#69310,#69311,#69312,#69313,#69314,#69315,
#69316,#69317,#69318,#69319,#69320,#69321,#69322,#69323,#69324,#69325,#69326,
#69327,#69328,#69329,#69330,#69331,#69332,#69333,#69334,#69335,#69336,#69337,
#69338,#69339,#69340,#69341,#69342,#69343,#69344,#69345,#69346,#69347,#69348,
#69349,#69350,#69351,#69352,#69353,#69354,#69355,#69356,#69357,#69358,#69359,
#69360,#69361,#69362,#69363,#69364,#69365,#69366,#69367,#69368,#69369,#69370,
#69371,#69372,#69373,#69374,#69375,#69376,#69377,#69378,#69379,#69380,#69381,
#69382,#69383,#69384,#69385,#69386,#69387,#69388,#69389,#69390,#69391,#69392,
#69393,#69394,#69395,#69396,#69397,#69398,#69399,#69400,#69401,#69402,#69403),
 .UNSPECIFIED.,.F.,.F.,(4,3,3,3,3,3,3,3,3,3,3,3,3,3,3,3,3,3,3,3,3,3,3,3,
3,3,3,3,3,3,3,3,3,3,3,3,3,3,4),(-1.36616069392045,-1.31234511237089,-1.25590688348171,
-1.2204333630174,-1.19978988220562,-1.18977196024391,-1.18171686684243,
-1.12581307864118,-1.0701759321844,-1.02114732597582,-1.01245062620987,
-1.00557445941498,-0.972118719767232,-0.917136616953618,-0.861845521732145,
-0.806301914936184,-0.764644209839213,-0.752957251104887,-0.74633211206392,
-0.691988105836551,-0.6396710945483,-0.58520690320579,-0.530950150202216,
-0.504026209800091,-0.49669074307685,-0.490850922101458,-0.437265330746164,
-0.383730417642567,-0.330847185660873,-0.315558626985216,-0.276113798612064,
-0.25885668619881,-0.248596553277842,-0.240631547783679,-0.188137027104224,
-0.135346638809626,-0.0828734852353619,-0.031420154055552,0.),
 .UNSPECIFIED.);
#2909=B_SPLINE_CURVE_WITH_KNOTS('',3,(#69406,#69407,#69408,#69409,#69410,
#69411,#69412,#69413,#69414,#69415,#69416,#69417),.UNSPECIFIED.,.F.,.F.,
(4,1,1,1,1,1,1,1,1,4),(11.6150691238055,12.1134708852447,12.6118726466838,
13.110274408123,13.6086761695621,14.1070779310013,14.6054796924404,15.1038814538796,
15.6022832153187,15.7079632679489),.UNSPECIFIED.);
#2910=B_SPLINE_CURVE_WITH_KNOTS('',3,(#70239,#70240,#70241,#70242,#70243,
#70244,#70245,#70246,#70247,#70248,#70249,#70250,#70251,#70252,#70253,#70254,
#70255,#70256,#70257,#70258,#70259,#70260,#70261,#70262,#70263,#70264,#70265,
#70266,#70267,#70268,#70269,#70270,#70271,#70272,#70273,#70274,#70275,#70276,
#70277,#70278,#70279,#70280,#70281,#70282,#70283,#70284,#70285,#70286,#70287,
#70288,#70289,#70290,#70291,#70292,#70293,#70294,#70295,#70296,#70297,#70298,
#70299,#70300,#70301,#70302,#70303,#70304,#70305,#70306,#70307,#70308,#70309,
#70310,#70311,#70312,#70313,#70314,#70315,#70316,#70317,#70318,#70319,#70320,
#70321,#70322,#70323,#70324,#70325,#70326,#70327,#70328,#70329,#70330,#70331,
#70332,#70333,#70334,#70335,#70336,#70337,#70338,#70339,#70340,#70341,#70342,
#70343,#70344,#70345,#70346,#70347,#70348,#70349,#70350),.UNSPECIFIED.,
 .F.,.F.,(4,3,3,3,3,3,3,3,3,3,3,3,3,3,3,3,3,3,3,3,3,3,3,3,3,3,3,3,3,3,3,
3,3,3,3,3,3,4),(-1.36927609592744,-1.32059746496358,-1.26831584736848,-1.2352152696692,
-1.21194802431441,-1.20083137389322,-1.14767293782772,-1.09434061945375,
-1.04892592261401,-1.0415650212466,-1.03428109205196,-1.00351122577428,
-0.950462711904765,-0.896724600945316,-0.841890457251413,-0.800764849480985,
-0.789580715694322,-0.78339457205448,-0.728633117749904,-0.677388026169701,
-0.622874336103501,-0.568068350793894,-0.539910429130868,-0.53169331053965,
-0.524470612233283,-0.469207425202408,-0.413568223926661,-0.358037807603194,
-0.342804977489683,-0.299954355303473,-0.281207208097006,-0.270867643816207,
-0.263531854461882,-0.208138335712682,-0.151751137623188,-0.0952553853759454,
-0.0393377021735775,0.),.UNSPECIFIED.);
#2911=B_SPLINE_CURVE_WITH_KNOTS('',3,(#70351,#70352,#70353,#70354,#70355,
#70356,#70357,#70358,#70359,#70360,#70361,#70362,#70363,#70364,#70365,#70366),
 .UNSPECIFIED.,.F.,.F.,(4,3,3,3,3,4),(-100.677155810709,-100.17875404927,
-99.6803522878307,-99.1819505263916,-98.6835487649524,-98.3406737518372),
 .UNSPECIFIED.);
#2912=B_SPLINE_CURVE_WITH_KNOTS('',3,(#70397,#70398,#70399,#70400,#70401,
#70402,#70403,#70404,#70405,#70406),.UNSPECIFIED.,.F.,.F.,(4,3,3,4),(-4.09323272002468,
-3.99664109620274,-2.99748082215206,-2.08103247056466),.UNSPECIFIED.);
#2913=B_SPLINE_CURVE_WITH_KNOTS('',3,(#70409,#70410,#70411,#70412,#70413,
#70414,#70415,#70416,#70417,#70418),.UNSPECIFIED.,.F.,.F.,(4,3,3,4),(0.,
0.499580137025342,0.999160274050685,1.12939240413109),.UNSPECIFIED.);
#2914=B_SPLINE_CURVE_WITH_KNOTS('',3,(#70423,#70424,#70425,#70426,#70427,
#70428,#70429,#70430,#70431,#70432,#70433,#70434,#70435,#70436,#70437,#70438,
#70439,#70440,#70441,#70442,#70443,#70444),.UNSPECIFIED.,.F.,.F.,(4,3,3,
3,3,3,3,4),(-10.3764180272043,-9.99160274050685,-8.99244246645616,-7.99328219240548,
-6.9941219183548,-5.99496164430411,-4.99580137025343,-4.09323272002468),
 .UNSPECIFIED.);
#2915=B_SPLINE_CURVE_WITH_KNOTS('',3,(#70445,#70446,#70447,#70448,#70449,
#70450,#70451,#70452,#70453,#70454,#70455,#70456,#70457,#70458,#70459,#70460,
#70461,#70462,#70463,#70464,#70465,#70466),.UNSPECIFIED.,.F.,.F.,(4,3,3,
3,3,3,3,4),(1.12939240413109,1.99832054810137,2.99748082215204,3.99664109620273,
4.9958013702534,5.99496164430408,6.99412191835476,7.41257771131067),
 .UNSPECIFIED.);
#2916=B_SPLINE_CURVE_WITH_KNOTS('',3,(#70471,#70472,#70473,#70474,#70475,
#70476,#70477,#70478,#70479,#70480,#70481,#70482,#70483,#70484,#70485,#70486,
#70487,#70488,#70489,#70490,#70491,#70492),.UNSPECIFIED.,.F.,.F.,(4,3,3,
3,3,3,3,4),(-16.6596033343839,-15.986564384811,-14.9874041107603,-13.9882438367096,
-12.9890835626589,-11.9899232886082,-10.9907630145575,-10.3764180272043),
 .UNSPECIFIED.);
#2917=B_SPLINE_CURVE_WITH_KNOTS('',3,(#70493,#70494,#70495,#70496,#70497,
#70498,#70499,#70500,#70501,#70502,#70503,#70504,#70505,#70506,#70507,#70508,
#70509,#70510,#70511,#70512,#70513,#70514),.UNSPECIFIED.,.F.,.F.,(4,3,3,
3,3,3,3,4),(7.41257771131067,7.99328219240545,8.99244246645615,9.99160274050685,
10.9907630145575,11.9899232886082,12.9890835626589,13.6957630184903),
 .UNSPECIFIED.);
#2918=B_SPLINE_CURVE_WITH_KNOTS('',3,(#70519,#70520,#70521,#70522,#70523,
#70524,#70525,#70526,#70527,#70528,#70529,#70530,#70531,#70532,#70533,#70534,
#70535,#70536,#70537,#70538,#70539,#70540),.UNSPECIFIED.,.F.,.F.,(4,3,3,
3,3,3,3,4),(-22.9427886415634,-21.9815260291151,-20.9823657550644,-19.9832054810137,
-18.984045206963,-17.9848849329123,-16.9857246588616,-16.6596033343839),
 .UNSPECIFIED.);
#2919=B_SPLINE_CURVE_WITH_KNOTS('',3,(#70541,#70542,#70543,#70544,#70545,
#70546,#70547,#70548,#70549,#70550,#70551,#70552,#70553,#70554,#70555,#70556,
#70557,#70558,#70559,#70560,#70561,#70562),.UNSPECIFIED.,.F.,.F.,(4,3,3,
3,3,3,3,4),(13.6957630184903,13.9882438367096,14.9874041107603,15.986564384811,
16.9857246588617,17.9848849329123,18.984045206963,19.9789483256699),
 .UNSPECIFIED.);
#2920=B_SPLINE_CURVE_WITH_KNOTS('',3,(#70567,#70568,#70569,#70570,#70571,
#70572,#70573,#70574,#70575,#70576,#70577,#70578,#70579,#70580,#70581,#70582,
#70583,#70584,#70585,#70586,#70587,#70588,#70589,#70590,#70591),
 .UNSPECIFIED.,.F.,.F.,(4,3,3,3,3,3,3,3,4),(-29.225973948743,-28.9756479474699,
-27.9764876734192,-26.9773273993685,-25.9781671253178,-24.9790068512671,
-23.9798465772164,-22.9806863031658,-22.9427886415634),.UNSPECIFIED.);
#2921=B_SPLINE_CURVE_WITH_KNOTS('',3,(#70592,#70593,#70594,#70595,#70596,
#70597,#70598,#70599,#70600,#70601,#70602,#70603,#70604,#70605,#70606,#70607,
#70608,#70609,#70610,#70611,#70612,#70613,#70614,#70615,#70616),
 .UNSPECIFIED.,.F.,.F.,(4,3,3,3,3,3,3,3,4),(19.9789483256699,19.9832054810137,
20.9823657550644,21.9815260291151,22.9806863031658,23.9798465772165,24.9790068512671,
25.9781671253178,26.2621336328494),.UNSPECIFIED.);
#2922=B_SPLINE_CURVE_WITH_KNOTS('',3,(#70621,#70622,#70623,#70624,#70625,
#70626,#70627,#70628,#70629,#70630,#70631,#70632,#70633,#70634,#70635,#70636,
#70637,#70638,#70639,#70640,#70641,#70642),.UNSPECIFIED.,.F.,.F.,(4,3,3,
3,3,3,3,4),(-35.5091592559226,-34.970609591774,-33.9714493177233,-32.9722890436726,
-31.9731287696219,-30.9739684955712,-29.9748082215206,-29.225973948743),
 .UNSPECIFIED.);
#2923=B_SPLINE_CURVE_WITH_KNOTS('',3,(#70643,#70644,#70645,#70646,#70647,
#70648,#70649,#70650,#70651,#70652,#70653,#70654,#70655,#70656,#70657,#70658,
#70659,#70660,#70661,#70662,#70663,#70664),.UNSPECIFIED.,.F.,.F.,(4,3,3,
3,3,3,3,4),(26.2621336328494,26.9773273993685,27.9764876734192,28.9756479474699,
29.9748082215206,30.9739684955713,31.9731287696219,32.545318940029),
 .UNSPECIFIED.);
#2924=B_SPLINE_CURVE_WITH_KNOTS('',3,(#70669,#70670,#70671,#70672,#70673,
#70674,#70675,#70676,#70677,#70678,#70679,#70680,#70681,#70682,#70683,#70684,
#70685,#70686,#70687,#70688,#70689,#70690),.UNSPECIFIED.,.F.,.F.,(4,3,3,
3,3,3,3,4),(-41.7923445631022,-40.9655712360781,-39.9664109620274,-38.9672506879767,
-37.968090413926,-36.9689301398754,-35.9697698658247,-35.5091592559226),
 .UNSPECIFIED.);
#2925=B_SPLINE_CURVE_WITH_KNOTS('',3,(#70691,#70692,#70693,#70694,#70695,
#70696,#70697,#70698,#70699,#70700,#70701,#70702,#70703,#70704,#70705,#70706,
#70707,#70708,#70709,#70710,#70711,#70712),.UNSPECIFIED.,.F.,.F.,(4,3,3,
3,3,3,3,4),(32.545318940029,32.9722890436726,33.9714493177233,34.970609591774,
35.9697698658247,36.9689301398753,37.968090413926,38.8285042472086),
 .UNSPECIFIED.);
#2926=B_SPLINE_CURVE_WITH_KNOTS('',3,(#70717,#70718,#70719,#70720,#70721,
#70722,#70723,#70724,#70725,#70726,#70727,#70728,#70729,#70730,#70731,#70732,
#70733,#70734,#70735,#70736,#70737,#70738,#70739,#70740,#70741),
 .UNSPECIFIED.,.F.,.F.,(4,3,3,3,3,3,3,3,4),(-48.0755298702818,-47.9596931544329,
-46.9605328803822,-45.9613726063315,-44.9622123322808,-43.9630520582302,
-42.9638917841795,-41.9647315101288,-41.7923445631022),.UNSPECIFIED.);
#2927=B_SPLINE_CURVE_WITH_KNOTS('',3,(#70742,#70743,#70744,#70745,#70746,
#70747,#70748,#70749,#70750,#70751,#70752,#70753,#70754,#70755,#70756,#70757,
#70758,#70759,#70760,#70761,#70762,#70763,#70764,#70765,#70766),
 .UNSPECIFIED.,.F.,.F.,(4,3,3,3,3,3,3,3,4),(38.8285042472086,38.9672506879767,
39.9664109620274,40.9655712360781,41.9647315101288,42.9638917841795,43.9630520582302,
44.9622123322809,45.1116895543882),.UNSPECIFIED.);
#2928=B_SPLINE_CURVE_WITH_KNOTS('',3,(#70771,#70772,#70773,#70774,#70775,
#70776,#70777,#70778,#70779,#70780,#70781,#70782,#70783,#70784,#70785,#70786,
#70787,#70788,#70789,#70790,#70791,#70792),.UNSPECIFIED.,.F.,.F.,(4,3,3,
3,3,3,3,4),(-54.3587151774614,-53.954654798737,-52.9554945246863,-51.9563342506356,
-50.9571739765849,-49.9580137025343,-48.9588534284836,-48.0755298702818),
 .UNSPECIFIED.);
#2929=B_SPLINE_CURVE_WITH_KNOTS('',3,(#70793,#70794,#70795,#70796,#70797,
#70798,#70799,#70800,#70801,#70802,#70803,#70804,#70805,#70806,#70807,#70808,
#70809,#70810,#70811,#70812,#70813,#70814),.UNSPECIFIED.,.F.,.F.,(4,3,3,
3,3,3,3,4),(45.1116895543882,45.9613726063316,46.9605328803822,47.9596931544329,
48.9588534284836,49.9580137025343,50.9571739765849,51.3948748615678),
 .UNSPECIFIED.);
#2930=B_SPLINE_CURVE_WITH_KNOTS('',3,(#70819,#70820,#70821,#70822,#70823,
#70824,#70825,#70826,#70827,#70828,#70829,#70830,#70831,#70832,#70833,#70834,
#70835,#70836,#70837,#70838,#70839,#70840),.UNSPECIFIED.,.F.,.F.,(4,3,3,
3,3,3,3,4),(-60.641900484641,-59.9496164430411,-58.9504561689904,-57.9512958949397,
-56.9521356208891,-55.9529753468384,-54.9538150727877,-54.3587151774614),
 .UNSPECIFIED.);
#2931=B_SPLINE_CURVE_WITH_KNOTS('',3,(#70841,#70842,#70843,#70844,#70845,
#70846,#70847,#70848,#70849,#70850,#70851,#70852,#70853,#70854,#70855,#70856,
#70857,#70858,#70859,#70860,#70861,#70862),.UNSPECIFIED.,.F.,.F.,(4,3,3,
3,3,3,3,4),(51.3948748615678,51.9563342506356,52.9554945246863,53.954654798737,
54.9538150727877,55.9529753468384,56.9521356208891,57.6780601687474),
 .UNSPECIFIED.);
#2932=B_SPLINE_CURVE_WITH_KNOTS('',3,(#70867,#70868,#70869,#70870,#70871,
#70872,#70873,#70874,#70875,#70876,#70877,#70878,#70879,#70880,#70881,#70882,
#70883,#70884,#70885,#70886,#70887,#70888),.UNSPECIFIED.,.F.,.F.,(4,3,3,
3,3,3,3,4),(-66.9250857918206,-65.9445780873452,-64.9454178132945,-63.9462575392438,
-62.9470972651932,-61.9479369911425,-60.9487767170918,-60.641900484641),
 .UNSPECIFIED.);
#2933=B_SPLINE_CURVE_WITH_KNOTS('',3,(#70889,#70890,#70891,#70892,#70893,
#70894,#70895,#70896,#70897,#70898,#70899,#70900,#70901,#70902,#70903,#70904,
#70905,#70906,#70907,#70908,#70909,#70910,#70911,#70912,#70913),
 .UNSPECIFIED.,.F.,.F.,(4,3,3,3,3,3,3,3,4),(57.6780601687474,57.9512958949398,
58.9504561689905,59.9496164430411,60.9487767170918,61.9479369911425,62.9470972651932,
63.9462575392438,63.961245475927),.UNSPECIFIED.);
#2934=B_SPLINE_CURVE_WITH_KNOTS('',3,(#70918,#70919,#70920,#70921,#70922,
#70923,#70924,#70925,#70926,#70927,#70928,#70929,#70930,#70931,#70932,#70933,
#70934,#70935,#70936,#70937,#70938,#70939,#70940,#70941,#70942),
 .UNSPECIFIED.,.F.,.F.,(4,3,3,3,3,3,3,3,4),(-73.2082710990002,-72.9387000057,
-71.9395397316493,-70.9403794575987,-69.941219183548,-68.9420589094973,
-67.9428986354466,-66.9437383613959,-66.9250857918206),.UNSPECIFIED.);
#2935=B_SPLINE_CURVE_WITH_KNOTS('',3,(#70943,#70944,#70945,#70946,#70947,
#70948,#70949,#70950,#70951,#70952,#70953,#70954,#70955,#70956,#70957,#70958,
#70959,#70960,#70961,#70962,#70963,#70964),.UNSPECIFIED.,.F.,.F.,(4,3,3,
3,3,3,3,4),(63.961245475927,64.9454178132945,65.9445780873452,66.9437383613959,
67.9428986354466,68.9420589094973,69.941219183548,70.2444307831066),
 .UNSPECIFIED.);
#2936=B_SPLINE_CURVE_WITH_KNOTS('',3,(#70969,#70970,#70971,#70972,#70973,
#70974,#70975,#70976,#70977,#70978,#70979,#70980,#70981,#70982,#70983,#70984,
#70985,#70986,#70987,#70988,#70989,#70990),.UNSPECIFIED.,.F.,.F.,(4,3,3,
3,3,3,3,4),(-79.4914564061798,-78.9336616500041,-77.9345013759535,-76.9353411019028,
-75.9361808278521,-74.9370205538014,-73.9378602797507,-73.2082710990002),
 .UNSPECIFIED.);
#2937=B_SPLINE_CURVE_WITH_KNOTS('',3,(#70991,#70992,#70993,#70994,#70995,
#70996,#70997,#70998,#70999,#71000,#71001,#71002,#71003,#71004,#71005,#71006,
#71007,#71008,#71009,#71010,#71011,#71012),.UNSPECIFIED.,.F.,.F.,(4,3,3,
3,3,3,3,4),(70.2444307831066,70.9403794575987,71.9395397316494,72.9387000057001,
73.9378602797507,74.9370205538014,75.9361808278521,76.5276160902862),
 .UNSPECIFIED.);
#2938=B_SPLINE_CURVE_WITH_KNOTS('',3,(#71017,#71018,#71019,#71020,#71021,
#71022,#71023,#71024,#71025,#71026,#71027,#71028,#71029,#71030,#71031,#71032,
#71033,#71034,#71035,#71036,#71037,#71038),.UNSPECIFIED.,.F.,.F.,(4,3,3,
3,3,3,3,4),(-85.7746417133594,-84.9286232943083,-83.9294630202576,-82.9303027462069,
-81.9311424721562,-80.9319821981055,-79.9328219240548,-79.4914564061798),
 .UNSPECIFIED.);
#2939=B_SPLINE_CURVE_WITH_KNOTS('',3,(#71039,#71040,#71041,#71042,#71043,
#71044,#71045,#71046,#71047,#71048,#71049,#71050,#71051,#71052,#71053,#71054,
#71055,#71056,#71057,#71058,#71059,#71060),.UNSPECIFIED.,.F.,.F.,(4,3,3,
3,3,3,3,4),(76.5276160902862,76.9353411019028,77.9345013759535,78.9336616500042,
79.9328219240548,80.9319821981055,81.9311424721562,82.8108013974658),
 .UNSPECIFIED.);
#2940=B_SPLINE_CURVE_WITH_KNOTS('',3,(#71065,#71066,#71067,#71068,#71069,
#71070,#71071,#71072,#71073,#71074,#71075,#71076,#71077,#71078,#71079,#71080,
#71081,#71082,#71083,#71084,#71085,#71086,#71087,#71088,#71089),
 .UNSPECIFIED.,.F.,.F.,(4,3,3,3,3,3,3,3,4),(-92.057827020539,-91.922745212663,
-90.9235849386124,-89.9244246645617,-88.925264390511,-87.9261041164603,
-86.9269438424096,-85.9277835683589,-85.7746417133594),.UNSPECIFIED.);
#2941=B_SPLINE_CURVE_WITH_KNOTS('',3,(#71090,#71091,#71092,#71093,#71094,
#71095,#71096,#71097,#71098,#71099,#71100,#71101,#71102,#71103,#71104,#71105,
#71106,#71107,#71108,#71109,#71110,#71111,#71112,#71113,#71114),
 .UNSPECIFIED.,.F.,.F.,(4,3,3,3,3,3,3,3,4),(82.8108013974658,82.9303027462069,
83.9294630202576,84.9286232943083,85.9277835683589,86.9269438424096,87.9261041164603,
88.925264390511,89.0939867046454),.UNSPECIFIED.);
#2942=B_SPLINE_CURVE_WITH_KNOTS('',3,(#71119,#71120,#71121,#71122,#71123,
#71124,#71125,#71126,#71127,#71128,#71129,#71130,#71131,#71132,#71133,#71134,
#71135,#71136,#71137,#71138,#71139,#71140),.UNSPECIFIED.,.F.,.F.,(4,3,3,
3,3,3,3,4),(-98.3410123277185,-97.9177068569672,-96.9185465829165,-95.9193863088658,
-94.9202260348151,-93.9210657607644,-92.9219054867137,-92.057827020539),
 .UNSPECIFIED.);
#2943=B_SPLINE_CURVE_WITH_KNOTS('',3,(#71141,#71142,#71143,#71144,#71145,
#71146,#71147,#71148,#71149,#71150,#71151,#71152,#71153,#71154,#71155,#71156,
#71157,#71158,#71159,#71160,#71161,#71162),.UNSPECIFIED.,.F.,.F.,(4,3,3,
3,3,3,3,4),(89.0939867046454,89.9244246645617,90.9235849386124,91.922745212663,
92.9219054867137,93.9210657607644,94.9202260348151,95.377172011825),
 .UNSPECIFIED.);
#2944=B_SPLINE_CURVE_WITH_KNOTS('',3,(#71167,#71168,#71169,#71170,#71171,
#71172,#71173,#71174,#71175,#71176,#71177,#71178,#71179,#71180,#71181,#71182,
#71183,#71184,#71185,#71186,#71187,#71188),.UNSPECIFIED.,.F.,.F.,(4,3,3,
3,3,3,3,4),(-104.624197634898,-103.912668501271,-102.913508227221,-101.91434795317,
-100.915187679119,-99.9160274050685,-98.9168671310179,-98.3410123277185),
 .UNSPECIFIED.);
#2945=B_SPLINE_CURVE_WITH_KNOTS('',3,(#71189,#71190,#71191,#71192,#71193,
#71194,#71195,#71196,#71197,#71198,#71199,#71200,#71201,#71202,#71203,#71204,
#71205,#71206,#71207,#71208,#71209,#71210),.UNSPECIFIED.,.F.,.F.,(4,3,3,
3,3,3,3,4),(95.377172011825,95.9193863088658,96.9185465829165,97.9177068569672,
98.9168671310178,99.9160274050685,100.915187679119,101.660357319005),
 .UNSPECIFIED.);
#2946=B_SPLINE_CURVE_WITH_KNOTS('',3,(#71215,#71216,#71217,#71218,#71219,
#71220,#71221,#71222,#71223,#71224,#71225,#71226,#71227,#71228,#71229,#71230,
#71231,#71232,#71233,#71234,#71235,#71236),.UNSPECIFIED.,.F.,.F.,(4,3,3,
3,3,3,3,4),(-110.907382942078,-109.907630145575,-108.908469871525,-107.909309597474,
-106.910149323423,-105.910989049373,-104.911828775322,-104.624197634898),
 .UNSPECIFIED.);
#2947=B_SPLINE_CURVE_WITH_KNOTS('',3,(#71237,#71238,#71239,#71240,#71241,
#71242,#71243,#71244,#71245,#71246,#71247,#71248,#71249,#71250,#71251,#71252,
#71253,#71254,#71255,#71256,#71257,#71258,#71259,#71260,#71261),
 .UNSPECIFIED.,.F.,.F.,(4,3,3,3,3,3,3,3,4),(101.660357319005,101.91434795317,
102.913508227221,103.912668501271,104.911828775322,105.910989049373,106.910149323423,
107.909309597474,107.943542626184),.UNSPECIFIED.);
#2948=B_SPLINE_CURVE_WITH_KNOTS('',3,(#71266,#71267,#71268,#71269,#71270,
#71271,#71272,#71273,#71274,#71275,#71276,#71277,#71278,#71279,#71280,#71281,
#71282,#71283,#71284,#71285,#71286,#71287),.UNSPECIFIED.,.F.,.F.,(4,3,3,
3,3,3,3,4),(-117.190568249257,-116.90175206393,-115.902591789879,-114.903431515829,
-113.904271241778,-112.905110967727,-111.905950693677,-110.907382942078),
 .UNSPECIFIED.);
#2949=B_SPLINE_CURVE_WITH_KNOTS('',3,(#71288,#71289,#71290,#71291,#71292,
#71293,#71294,#71295,#71296,#71297,#71298,#71299,#71300,#71301,#71302,#71303,
#71304,#71305,#71306,#71307,#71308,#71309),.UNSPECIFIED.,.F.,.F.,(4,3,3,
3,3,3,3,4),(107.943542626184,108.908469871525,109.907630145575,110.906790419626,
111.905950693677,112.905110967727,113.904271241778,114.226727933364),
 .UNSPECIFIED.);
#2950=B_SPLINE_CURVE_WITH_KNOTS('',3,(#71314,#71315,#71316,#71317,#71318,
#71319,#71320,#71321,#71322,#71323,#71324,#71325,#71326,#71327,#71328,#71329,
#71330,#71331,#71332,#71333,#71334,#71335),.UNSPECIFIED.,.F.,.F.,(4,3,3,
3,3,3,3,4),(-123.473753556437,-122.896713708234,-121.897553434184,-120.898393160133,
-119.899232886082,-118.900072612032,-117.900912337981,-117.190568249257),
 .UNSPECIFIED.);
#2951=B_SPLINE_CURVE_WITH_KNOTS('',3,(#71336,#71337,#71338,#71339,#71340,
#71341,#71342,#71343,#71344,#71345,#71346,#71347,#71348,#71349,#71350,#71351,
#71352,#71353,#71354,#71355,#71356,#71357),.UNSPECIFIED.,.F.,.F.,(4,3,3,
3,3,3,3,4),(114.226727933364,114.903431515829,115.90259178988,116.90175206393,
117.900912337981,118.900072612032,119.899232886082,120.509913240543),
 .UNSPECIFIED.);
#2952=B_SPLINE_CURVE_WITH_KNOTS('',3,(#71362,#71363,#71364,#71365,#71366,
#71367,#71368,#71369,#71370,#71371,#71372,#71373,#71374,#71375,#71376,#71377,
#71378,#71379,#71380,#71381,#71382,#71383),.UNSPECIFIED.,.F.,.F.,(4,3,3,
3,3,3,3,4),(-129.756938863617,-128.891675352538,-127.892515078488,-126.893354804437,
-125.894194530386,-124.895034256336,-123.895873982285,-123.473753556437),
 .UNSPECIFIED.);
#2953=B_SPLINE_CURVE_WITH_KNOTS('',3,(#71384,#71385,#71386,#71387,#71388,
#71389,#71390,#71391,#71392,#71393,#71394,#71395,#71396,#71397,#71398,#71399,
#71400,#71401,#71402,#71403,#71404,#71405),.UNSPECIFIED.,.F.,.F.,(4,3,3,
3,3,3,3,4),(120.509913240543,120.898393160133,121.897553434184,122.896713708234,
123.895873982285,124.895034256336,125.894194530386,126.793098547723),
 .UNSPECIFIED.);
#2954=B_SPLINE_CURVE_WITH_KNOTS('',3,(#71410,#71411,#71412,#71413,#71414,
#71415,#71416,#71417,#71418,#71419,#71420,#71421,#71422,#71423,#71424,#71425,
#71426,#71427,#71428,#71429,#71430,#71431,#71432,#71433,#71434),
 .UNSPECIFIED.,.F.,.F.,(4,3,3,3,3,3,3,3,4),(-136.040124170796,-135.885797270893,
-134.886636996842,-133.887476722792,-132.888316448741,-131.88915617469,
-130.88999590064,-129.890835626589,-129.756938863617),.UNSPECIFIED.);
#2955=B_SPLINE_CURVE_WITH_KNOTS('',3,(#71435,#71436,#71437,#71438,#71439,
#71440,#71441,#71442,#71443,#71444,#71445,#71446,#71447,#71448,#71449,#71450,
#71451,#71452,#71453,#71454,#71455,#71456,#71457,#71458,#71459),
 .UNSPECIFIED.,.F.,.F.,(4,3,3,3,3,3,3,3,4),(126.793098547723,126.893354804437,
127.892515078488,128.891675352538,129.890835626589,130.88999590064,131.88915617469,
132.888316448741,133.076283854902),.UNSPECIFIED.);
#2956=B_SPLINE_CURVE_WITH_KNOTS('',3,(#71464,#71465,#71466,#71467,#71468,
#71469,#71470,#71471,#71472,#71473,#71474,#71475,#71476,#71477,#71478,#71479,
#71480,#71481,#71482,#71483,#71484,#71485),.UNSPECIFIED.,.F.,.F.,(4,3,3,
3,3,3,3,4),(-142.323309477976,-141.880758915197,-140.881598641147,-139.882438367096,
-138.883278093045,-137.884117818995,-136.884957544944,-136.040124170796),
 .UNSPECIFIED.);
#2957=B_SPLINE_CURVE_WITH_KNOTS('',3,(#71486,#71487,#71488,#71489,#71490,
#71491,#71492,#71493,#71494,#71495,#71496,#71497,#71498,#71499,#71500,#71501,
#71502,#71503,#71504,#71505,#71506,#71507),.UNSPECIFIED.,.F.,.F.,(4,3,3,
3,3,3,3,4),(133.076283854902,133.887476722792,134.886636996843,135.885797270893,
136.884957544944,137.884117818995,138.883278093045,139.359469162082),
 .UNSPECIFIED.);
#2958=B_SPLINE_CURVE_WITH_KNOTS('',3,(#71512,#71513,#71514,#71515,#71516,
#71517,#71518,#71519,#71520,#71521,#71522,#71523,#71524,#71525,#71526,#71527,
#71528,#71529,#71530,#71531,#71532,#71533),.UNSPECIFIED.,.F.,.F.,(4,3,3,
3,3,3,3,4),(-148.606494785155,-147.875720559501,-146.876560285451,-145.8774000114,
-144.878239737349,-143.879079463299,-142.879919189248,-142.323309477976),
 .UNSPECIFIED.);
#2959=B_SPLINE_CURVE_WITH_KNOTS('',3,(#71534,#71535,#71536,#71537,#71538,
#71539,#71540,#71541,#71542,#71543,#71544,#71545,#71546,#71547,#71548,#71549,
#71550,#71551,#71552,#71553,#71554,#71555),.UNSPECIFIED.,.F.,.F.,(4,3,3,
3,3,3,3,4),(139.359469162082,139.882438367096,140.881598641147,141.880758915197,
142.879919189248,143.879079463299,144.878239737349,145.642654469262),
 .UNSPECIFIED.);
#2960=B_SPLINE_CURVE_WITH_KNOTS('',3,(#71560,#71561,#71562,#71563,#71564,
#71565,#71566,#71567,#71568,#71569,#71570,#71571,#71572,#71573,#71574,#71575,
#71576,#71577,#71578,#71579,#71580,#71581,#71582,#71583,#71584),
 .UNSPECIFIED.,.F.,.F.,(4,3,3,3,3,3,3,3,4),(-154.889680092335,-154.869842477856,
-153.870682203806,-152.871521929755,-151.872361655704,-150.873201381653,
-149.874041107603,-148.874880833552,-148.606494785155),.UNSPECIFIED.);
#2961=B_SPLINE_CURVE_WITH_KNOTS('',3,(#71585,#71586,#71587,#71588,#71589,
#71590,#71591,#71592,#71593,#71594,#71595,#71596,#71597,#71598,#71599,#71600,
#71601,#71602,#71603,#71604,#71605,#71606,#71607,#71608,#71609),
 .UNSPECIFIED.,.F.,.F.,(4,3,3,3,3,3,3,3,4),(145.642654469262,145.8774000114,
146.876560285451,147.875720559501,148.874880833552,149.874041107603,150.873201381653,
151.872361655704,151.925839776441),.UNSPECIFIED.);
#2962=B_SPLINE_CURVE_WITH_KNOTS('',3,(#71614,#71615,#71616,#71617,#71618,
#71619,#71620,#71621,#71622,#71623,#71624,#71625,#71626,#71627,#71628,#71629,
#71630,#71631,#71632,#71633,#71634,#71635),.UNSPECIFIED.,.F.,.F.,(4,3,3,
3,3,3,3,4),(-161.172865399514,-160.86480412216,-159.86564384811,-158.866483574059,
-157.867323300008,-156.868163025958,-155.869002751907,-154.889680092335),
 .UNSPECIFIED.);
#2963=B_SPLINE_CURVE_WITH_KNOTS('',3,(#71636,#71637,#71638,#71639,#71640,
#71641,#71642,#71643,#71644,#71645,#71646,#71647,#71648,#71649,#71650,#71651,
#71652,#71653,#71654,#71655,#71656,#71657),.UNSPECIFIED.,.F.,.F.,(4,3,3,
3,3,3,3,4),(151.925839776441,152.871521929755,153.870682203806,154.869842477856,
155.869002751907,156.868163025958,157.867323300008,158.209025083621),
 .UNSPECIFIED.);
#2964=B_SPLINE_CURVE_WITH_KNOTS('',3,(#71662,#71663,#71664,#71665,#71666,
#71667,#71668,#71669,#71670,#71671,#71672,#71673,#71674,#71675,#71676,#71677,
#71678,#71679,#71680,#71681,#71682,#71683),.UNSPECIFIED.,.F.,.F.,(4,3,3,
3,3,3,3,4),(-167.456050706694,-166.859765766464,-165.860605492414,-164.861445218363,
-163.862284944312,-162.863124670262,-161.863964396211,-161.172865399514),
 .UNSPECIFIED.);
#2965=B_SPLINE_CURVE_WITH_KNOTS('',3,(#71684,#71685,#71686,#71687,#71688,
#71689,#71690,#71691,#71692,#71693,#71694,#71695,#71696,#71697,#71698,#71699,
#71700,#71701,#71702,#71703,#71704,#71705),.UNSPECIFIED.,.F.,.F.,(4,3,3,
3,3,3,3,4),(158.209025083621,158.866483574059,159.86564384811,160.86480412216,
161.863964396211,162.863124670262,163.862284944312,164.4922103908),
 .UNSPECIFIED.);
#2966=B_SPLINE_CURVE_WITH_KNOTS('',3,(#71710,#71711,#71712,#71713,#71714,
#71715,#71716,#71717,#71718,#71719,#71720,#71721,#71722,#71723,#71724,#71725,
#71726,#71727,#71728,#71729,#71730,#71731),.UNSPECIFIED.,.F.,.F.,(4,3,3,
3,3,3,3,4),(-173.739236013873,-172.854727410769,-171.855567136718,-170.856406862667,
-169.857246588616,-168.858086314566,-167.858926040515,-167.456050706694),
 .UNSPECIFIED.);
#2967=B_SPLINE_CURVE_WITH_KNOTS('',3,(#71732,#71733,#71734,#71735,#71736,
#71737,#71738,#71739,#71740,#71741,#71742,#71743,#71744,#71745,#71746,#71747,
#71748,#71749,#71750,#71751,#71752,#71753),.UNSPECIFIED.,.F.,.F.,(4,3,3,
3,3,3,3,4),(164.4922103908,164.861445218363,165.860605492414,166.859765766465,
167.858926040515,168.858086314566,169.857246588617,170.77539569798),
 .UNSPECIFIED.);
#2968=B_SPLINE_CURVE_WITH_KNOTS('',3,(#71758,#71759,#71760,#71761,#71762,
#71763,#71764,#71765,#71766,#71767,#71768,#71769,#71770,#71771,#71772,#71773,
#71774,#71775,#71776,#71777,#71778,#71779,#71780,#71781,#71782),
 .UNSPECIFIED.,.F.,.F.,(4,3,3,3,3,3,3,3,4),(-180.022421321053,-179.848849329123,
-178.849689055073,-177.850528781022,-176.851368506971,-175.852208232921,
-174.85304795887,-173.853887684819,-173.739236013873),.UNSPECIFIED.);
#2969=B_SPLINE_CURVE_WITH_KNOTS('',3,(#71783,#71784,#71785,#71786,#71787,
#71788,#71789,#71790,#71791,#71792,#71793,#71794,#71795,#71796,#71797,#71798,
#71799,#71800,#71801,#71802,#71803,#71804,#71805,#71806,#71807),
 .UNSPECIFIED.,.F.,.F.,(4,3,3,3,3,3,3,3,4),(170.77539569798,170.856406862667,
171.855567136718,172.854727410769,173.853887684819,174.85304795887,175.852208232921,
176.851368506971,177.058581005159),.UNSPECIFIED.);
#2970=B_SPLINE_CURVE_WITH_KNOTS('',3,(#71812,#71813,#71814,#71815,#71816,
#71817,#71818,#71819,#71820,#71821,#71822,#71823,#71824,#71825,#71826,#71827,
#71828,#71829,#71830,#71831,#71832,#71833),.UNSPECIFIED.,.F.,.F.,(4,3,3,
3,3,3,3,4),(-186.305606628233,-185.843810973427,-184.844650699377,-183.845490425326,
-182.846330151275,-181.847169877225,-180.848009603174,-180.022421321053),
 .UNSPECIFIED.);
#2971=B_SPLINE_CURVE_WITH_KNOTS('',3,(#71834,#71835,#71836,#71837,#71838,
#71839,#71840,#71841,#71842,#71843,#71844,#71845,#71846,#71847,#71848,#71849,
#71850,#71851,#71852,#71853,#71854,#71855),.UNSPECIFIED.,.F.,.F.,(4,3,3,
3,3,3,3,4),(177.058581005159,177.850528781022,178.849689055073,179.848849329123,
180.848009603174,181.847169877225,182.846330151275,183.341766312339),
 .UNSPECIFIED.);
#2972=B_SPLINE_CURVE_WITH_KNOTS('',3,(#71860,#71861,#71862,#71863,#71864,
#71865,#71866,#71867,#71868,#71869,#71870,#71871,#71872,#71873,#71874,#71875,
#71876,#71877,#71878,#71879,#71880,#71881),.UNSPECIFIED.,.F.,.F.,(4,3,3,
3,3,3,3,4),(-192.588791935412,-191.838772617732,-190.839612343681,-189.84045206963,
-188.841291795579,-187.842131521529,-186.842971247478,-186.305606628233),
 .UNSPECIFIED.);
#2973=B_SPLINE_CURVE_WITH_KNOTS('',3,(#71882,#71883,#71884,#71885,#71886,
#71887,#71888,#71889,#71890,#71891,#71892,#71893,#71894,#71895,#71896,#71897,
#71898,#71899,#71900,#71901,#71902,#71903),.UNSPECIFIED.,.F.,.F.,(4,3,3,
3,3,3,3,4),(183.341766312339,183.845490425326,184.844650699377,185.843810973427,
186.842971247478,187.842131521529,188.84129179558,189.624951619519),
 .UNSPECIFIED.);
#2974=B_SPLINE_CURVE_WITH_KNOTS('',3,(#71908,#71909,#71910,#71911,#71912,
#71913,#71914,#71915,#71916,#71917,#71918,#71919,#71920,#71921,#71922,#71923,
#71924,#71925,#71926,#71927,#71928,#71929,#71930,#71931,#71932),
 .UNSPECIFIED.,.F.,.F.,(4,3,3,3,3,3,3,3,4),(-198.871977242592,-198.832894536086,
-197.833734262036,-196.834573987985,-195.835413713934,-194.836253439884,
-193.837093165833,-192.837932891782,-192.588791935412),.UNSPECIFIED.);
#2975=B_SPLINE_CURVE_WITH_KNOTS('',3,(#71933,#71934,#71935,#71936,#71937,
#71938,#71939,#71940,#71941,#71942,#71943,#71944,#71945,#71946,#71947,#71948,
#71949,#71950,#71951,#71952,#71953,#71954,#71955,#71956,#71957),
 .UNSPECIFIED.,.F.,.F.,(4,3,3,3,3,3,3,3,4),(189.624951619519,189.84045206963,
190.839612343681,191.838772617732,192.837932891782,193.837093165833,194.836253439884,
195.835413713934,195.908136926698),.UNSPECIFIED.);
#2976=B_SPLINE_CURVE_WITH_KNOTS('',3,(#71962,#71963,#71964,#71965,#71966,
#71967,#71968,#71969,#71970,#71971,#71972,#71973,#71974,#71975,#71976,#71977,
#71978,#71979,#71980,#71981,#71982,#71983),.UNSPECIFIED.,.F.,.F.,(4,3,3,
3,3,3,3,4),(-205.155162549771,-204.82785618039,-203.82869590634,-202.829535632289,
-201.830375358238,-200.831215084188,-199.832054810137,-198.871977242592),
 .UNSPECIFIED.);
#2977=B_SPLINE_CURVE_WITH_KNOTS('',3,(#71984,#71985,#71986,#71987,#71988,
#71989,#71990,#71991,#71992,#71993,#71994,#71995,#71996,#71997,#71998,#71999,
#72000,#72001,#72002,#72003,#72004,#72005),.UNSPECIFIED.,.F.,.F.,(4,3,3,
3,3,3,3,4),(195.908136926698,196.834573987985,197.833734262036,198.832894536086,
199.832054810137,200.831215084188,201.830375358238,202.191322233878),
 .UNSPECIFIED.);
#2978=B_SPLINE_CURVE_WITH_KNOTS('',3,(#72010,#72011,#72012,#72013,#72014,
#72015,#72016,#72017,#72018,#72019,#72020,#72021,#72022,#72023,#72024,#72025,
#72026,#72027,#72028,#72029,#72030,#72031),.UNSPECIFIED.,.F.,.F.,(4,3,3,
3,3,3,3,4),(-211.438347856951,-210.822817824695,-209.823657550644,-208.824497276593,
-207.825337002543,-206.826176728492,-205.827016454441,-205.155162549771),
 .UNSPECIFIED.);
#2979=B_SPLINE_CURVE_WITH_KNOTS('',3,(#72032,#72033,#72034,#72035,#72036,
#72037,#72038,#72039,#72040,#72041,#72042,#72043,#72044,#72045,#72046,#72047,
#72048,#72049,#72050,#72051,#72052,#72053),.UNSPECIFIED.,.F.,.F.,(4,3,3,
3,3,3,3,4),(202.191322233878,202.829535632289,203.82869590634,204.82785618039,
205.827016454441,206.826176728492,207.825337002543,208.474507541057),
 .UNSPECIFIED.);
#2980=B_SPLINE_CURVE_WITH_KNOTS('',3,(#72058,#72059,#72060,#72061,#72062,
#72063,#72064,#72065,#72066,#72067,#72068,#72069,#72070,#72071,#72072,#72073,
#72074,#72075,#72076,#72077,#72078,#72079),.UNSPECIFIED.,.F.,.F.,(4,3,3,
3,3,3,3,4),(-217.72153316413,-216.817779468999,-215.818619194948,-214.819458920897,
-213.820298646847,-212.821138372796,-211.821978098745,-211.438347856951),
 .UNSPECIFIED.);
#2981=B_SPLINE_CURVE_WITH_KNOTS('',3,(#72080,#72081,#72082,#72083,#72084,
#72085,#72086,#72087,#72088,#72089,#72090,#72091,#72092,#72093,#72094,#72095,
#72096,#72097,#72098,#72099,#72100,#72101),.UNSPECIFIED.,.F.,.F.,(4,3,3,
3,3,3,3,4),(208.474507541057,208.824497276593,209.823657550644,210.822817824695,
211.821978098745,212.821138372796,213.820298646847,214.757692848237),
 .UNSPECIFIED.);
#2982=B_SPLINE_CURVE_WITH_KNOTS('',3,(#72106,#72107,#72108,#72109,#72110,
#72111,#72112,#72113,#72114,#72115,#72116,#72117,#72118,#72119,#72120,#72121,
#72122,#72123,#72124,#72125,#72126,#72127,#72128,#72129,#72130),
 .UNSPECIFIED.,.F.,.F.,(4,3,3,3,3,3,3,3,4),(-224.00471847131,-223.811901387354,
-222.812741113303,-221.813580839252,-220.814420565201,-219.815260291151,
-218.8161000171,-217.816939743049,-217.72153316413),.UNSPECIFIED.);
#2983=B_SPLINE_CURVE_WITH_KNOTS('',3,(#72131,#72132,#72133,#72134,#72135,
#72136,#72137,#72138,#72139,#72140,#72141,#72142,#72143,#72144,#72145,#72146,
#72147,#72148,#72149,#72150,#72151,#72152,#72153,#72154,#72155),
 .UNSPECIFIED.,.F.,.F.,(4,3,3,3,3,3,3,3,4),(214.757692848237,214.819458920897,
215.818619194948,216.817779468999,217.816939743049,218.8161000171,219.815260291151,
220.814420565201,221.040878155416),.UNSPECIFIED.);
#2984=B_SPLINE_CURVE_WITH_KNOTS('',3,(#72160,#72161,#72162,#72163,#72164,
#72165,#72166,#72167,#72168,#72169,#72170,#72171,#72172,#72173,#72174,#72175,
#72176,#72177,#72178,#72179,#72180,#72181),.UNSPECIFIED.,.F.,.F.,(4,3,3,
3,3,3,3,4),(-230.287903778489,-229.806863031658,-228.807702757607,-227.808542483556,
-226.809382209506,-225.810221935455,-224.811061661404,-224.00471847131),
 .UNSPECIFIED.);
#2985=B_SPLINE_CURVE_WITH_KNOTS('',3,(#72182,#72183,#72184,#72185,#72186,
#72187,#72188,#72189,#72190,#72191,#72192,#72193,#72194,#72195,#72196,#72197,
#72198,#72199,#72200,#72201,#72202,#72203),.UNSPECIFIED.,.F.,.F.,(4,3,3,
3,3,3,3,4),(221.040878155416,221.813580839252,222.812741113303,223.811901387354,
224.811061661404,225.810221935455,226.809382209506,227.324063462596),
 .UNSPECIFIED.);
#2986=B_SPLINE_CURVE_WITH_KNOTS('',3,(#72208,#72209,#72210,#72211,#72212,
#72213,#72214,#72215,#72216,#72217,#72218,#72219,#72220,#72221,#72222,#72223,
#72224,#72225,#72226,#72227,#72228,#72229),.UNSPECIFIED.,.F.,.F.,(4,3,3,
3,3,3,3,4),(-236.571089085669,-235.801824675962,-234.802664401911,-233.80350412786,
-232.80434385381,-231.805183579759,-230.806023305708,-230.287903778489),
 .UNSPECIFIED.);
#2987=B_SPLINE_CURVE_WITH_KNOTS('',3,(#72230,#72231,#72232,#72233,#72234,
#72235,#72236,#72237,#72238,#72239,#72240,#72241,#72242,#72243,#72244,#72245,
#72246,#72247,#72248,#72249,#72250,#72251),.UNSPECIFIED.,.F.,.F.,(4,3,3,
3,3,3,3,4),(227.324063462596,227.808542483556,228.807702757607,229.806863031658,
230.806023305708,231.805183579759,232.80434385381,233.607248769776),
 .UNSPECIFIED.);
#2988=B_SPLINE_CURVE_WITH_KNOTS('',3,(#72256,#72257,#72258,#72259,#72260,
#72261,#72262,#72263,#72264,#72265,#72266,#72267,#72268,#72269,#72270,#72271,
#72272,#72273,#72274,#72275,#72276,#72277,#72278,#72279,#72280),
 .UNSPECIFIED.,.F.,.F.,(4,3,3,3,3,3,3,3,4),(-242.854274392849,-242.795946594317,
-241.796786320266,-240.797626046215,-239.798465772164,-238.799305498114,
-237.800145224063,-236.800984950012,-236.571089085669),.UNSPECIFIED.);
#2989=B_SPLINE_CURVE_WITH_KNOTS('',3,(#72281,#72282,#72283,#72284,#72285,
#72286,#72287,#72288,#72289,#72290,#72291,#72292,#72293,#72294,#72295,#72296,
#72297,#72298,#72299,#72300,#72301,#72302,#72303,#72304,#72305),
 .UNSPECIFIED.,.F.,.F.,(4,3,3,3,3,3,3,3,4),(233.607248769776,233.80350412786,
234.802664401911,235.801824675962,236.800984950012,237.800145224063,238.799305498114,
239.798465772164,239.890434076955),.UNSPECIFIED.);
#2990=B_SPLINE_CURVE_WITH_KNOTS('',3,(#72310,#72311,#72312,#72313,#72314,
#72315,#72316,#72317,#72318,#72319,#72320,#72321,#72322,#72323,#72324,#72325,
#72326,#72327,#72328,#72329,#72330,#72331),.UNSPECIFIED.,.F.,.F.,(4,3,3,
3,3,3,3,4),(-249.137459700028,-248.790908238621,-247.79174796457,-246.792587690519,
-245.793427416469,-244.794267142418,-243.795106868367,-242.854274392849),
 .UNSPECIFIED.);
#2991=B_SPLINE_CURVE_WITH_KNOTS('',3,(#72332,#72333,#72334,#72335,#72336,
#72337,#72338,#72339,#72340,#72341,#72342,#72343,#72344,#72345,#72346,#72347,
#72348,#72349,#72350,#72351,#72352,#72353),.UNSPECIFIED.,.F.,.F.,(4,3,3,
3,3,3,3,4),(239.890434076955,240.797626046215,241.796786320266,242.795946594317,
243.795106868367,244.794267142418,245.793427416469,246.173619384135),
 .UNSPECIFIED.);
#2992=B_SPLINE_CURVE_WITH_KNOTS('',3,(#72358,#72359,#72360,#72361,#72362,
#72363,#72364,#72365,#72366,#72367,#72368,#72369,#72370,#72371,#72372,#72373,
#72374,#72375,#72376,#72377,#72378,#72379),.UNSPECIFIED.,.F.,.F.,(4,3,3,
3,3,3,3,4),(-255.420645007208,-254.785869882925,-253.786709608874,-252.787549334823,
-251.788389060773,-250.789228786722,-249.790068512671,-249.137459700028),
 .UNSPECIFIED.);
#2993=B_SPLINE_CURVE_WITH_KNOTS('',3,(#72380,#72381,#72382,#72383,#72384,
#72385,#72386,#72387,#72388,#72389,#72390,#72391,#72392,#72393,#72394,#72395,
#72396,#72397,#72398,#72399,#72400,#72401),.UNSPECIFIED.,.F.,.F.,(4,3,3,
3,3,3,3,4),(246.173619384135,246.792587690519,247.79174796457,248.790908238621,
249.790068512671,250.789228786722,251.788389060773,252.456804691314),
 .UNSPECIFIED.);
#2994=B_SPLINE_CURVE_WITH_KNOTS('',3,(#72406,#72407,#72408,#72409,#72410,
#72411,#72412,#72413,#72414,#72415,#72416,#72417,#72418,#72419,#72420,#72421,
#72422,#72423,#72424,#72425,#72426,#72427),.UNSPECIFIED.,.F.,.F.,(4,3,3,
3,3,3,3,4),(-261.703830314387,-260.780831527229,-259.781671253178,-258.782510979127,
-257.783350705077,-256.784190431026,-255.785030156975,-255.420645007208),
 .UNSPECIFIED.);
#2995=B_SPLINE_CURVE_WITH_KNOTS('',3,(#72428,#72429,#72430,#72431,#72432,
#72433,#72434,#72435,#72436,#72437,#72438,#72439,#72440,#72441,#72442,#72443,
#72444,#72445,#72446,#72447,#72448,#72449),.UNSPECIFIED.,.F.,.F.,(4,3,3,
3,3,3,3,4),(252.456804691314,252.787549334823,253.786709608874,254.785869882925,
255.785030156975,256.784190431026,257.783350705077,258.739989998494),
 .UNSPECIFIED.);
#2996=B_SPLINE_CURVE_WITH_KNOTS('',3,(#72454,#72455,#72456,#72457,#72458,
#72459,#72460,#72461,#72462,#72463,#72464,#72465,#72466,#72467,#72468,#72469,
#72470,#72471,#72472,#72473,#72474,#72475,#72476,#72477,#72478),
 .UNSPECIFIED.,.F.,.F.,(4,3,3,3,3,3,3,3,4),(-267.987015621567,-267.774953445584,
-266.775793171533,-265.776632897482,-264.777472623432,-263.778312349381,
-262.77915207533,-261.77999180128,-261.703830314387),.UNSPECIFIED.);
#2997=B_SPLINE_CURVE_WITH_KNOTS('',3,(#72479,#72480,#72481,#72482,#72483,
#72484,#72485,#72486,#72487,#72488,#72489,#72490,#72491,#72492,#72493,#72494,
#72495,#72496,#72497,#72498,#72499,#72500,#72501,#72502,#72503),
 .UNSPECIFIED.,.F.,.F.,(4,3,3,3,3,3,3,3,4),(258.739989998494,258.782510979128,
259.781671253178,260.780831527229,261.77999180128,262.77915207533,263.778312349381,
264.777472623432,265.023175305673),.UNSPECIFIED.);
#2998=B_SPLINE_CURVE_WITH_KNOTS('',3,(#72508,#72509,#72510,#72511,#72512,
#72513,#72514,#72515,#72516,#72517,#72518,#72519,#72520,#72521,#72522,#72523,
#72524,#72525,#72526,#72527,#72528,#72529),.UNSPECIFIED.,.F.,.F.,(4,3,3,
3,3,3,3,4),(-274.270200928747,-273.769915089888,-272.770754815837,-271.771594541786,
-270.772434267736,-269.773273993685,-268.774113719634,-267.987015621567),
 .UNSPECIFIED.);
#2999=B_SPLINE_CURVE_WITH_KNOTS('',3,(#72530,#72531,#72532,#72533,#72534,
#72535,#72536,#72537,#72538,#72539,#72540,#72541,#72542,#72543,#72544,#72545,
#72546,#72547,#72548,#72549,#72550,#72551),.UNSPECIFIED.,.F.,.F.,(4,3,3,
3,3,3,3,4),(265.023175305673,265.776632897482,266.775793171533,267.774953445584,
268.774113719634,269.773273993685,270.772434267736,271.306360612853),
 .UNSPECIFIED.);
#3000=B_SPLINE_CURVE_WITH_KNOTS('',3,(#72556,#72557,#72558,#72559,#72560,
#72561,#72562,#72563,#72564,#72565,#72566,#72567,#72568,#72569,#72570,#72571,
#72572,#72573,#72574,#72575,#72576,#72577),.UNSPECIFIED.,.F.,.F.,(4,3,3,
3,3,3,3,4),(-280.553386235926,-279.764876734192,-278.765716460141,-277.76655618609,
-276.76739591204,-275.768235637989,-274.769075363938,-274.270200928747),
 .UNSPECIFIED.);
#3001=B_SPLINE_CURVE_WITH_KNOTS('',3,(#72578,#72579,#72580,#72581,#72582,
#72583,#72584,#72585,#72586,#72587,#72588,#72589,#72590,#72591,#72592,#72593,
#72594,#72595,#72596,#72597,#72598,#72599),.UNSPECIFIED.,.F.,.F.,(4,3,3,
3,3,3,3,4),(271.306360612853,271.771594541786,272.770754815837,273.769915089888,
274.769075363938,275.768235637989,276.76739591204,277.589545920032),
 .UNSPECIFIED.);
#3002=B_SPLINE_CURVE_WITH_KNOTS('',3,(#72604,#72605,#72606,#72607,#72608,
#72609,#72610,#72611,#72612,#72613,#72614,#72615,#72616,#72617,#72618,#72619,
#72620,#72621,#72622,#72623,#72624,#72625,#72626,#72627,#72628),
 .UNSPECIFIED.,.F.,.F.,(4,3,3,3,3,3,3,3,4),(-286.836571543106,-286.758998652547,
-285.759838378496,-284.760678104445,-283.761517830395,-282.762357556344,
-281.763197282293,-280.764037008243,-280.553386235926),.UNSPECIFIED.);
#3003=B_SPLINE_CURVE_WITH_KNOTS('',3,(#72629,#72630,#72631,#72632,#72633,
#72634,#72635,#72636,#72637,#72638,#72639,#72640,#72641,#72642,#72643,#72644,
#72645,#72646,#72647,#72648,#72649,#72650,#72651,#72652,#72653),
 .UNSPECIFIED.,.F.,.F.,(4,3,3,3,3,3,3,3,4),(277.589545920032,277.766556186091,
278.765716460141,279.764876734192,280.764037008243,281.763197282293,282.762357556344,
283.761517830395,283.872731227212),.UNSPECIFIED.);
#3004=B_SPLINE_CURVE_WITH_KNOTS('',3,(#72658,#72659,#72660,#72661,#72662,
#72663,#72664,#72665,#72666,#72667,#72668,#72669,#72670,#72671,#72672,#72673,
#72674,#72675,#72676,#72677,#72678,#72679),.UNSPECIFIED.,.F.,.F.,(4,3,3,
3,3,3,3,4),(-293.119756850285,-292.753960296851,-291.7548000228,-290.755639748749,
-289.756479474699,-288.757319200648,-287.758158926597,-286.836571543106),
 .UNSPECIFIED.);
#3005=B_SPLINE_CURVE_WITH_KNOTS('',3,(#72680,#72681,#72682,#72683,#72684,
#72685,#72686,#72687,#72688,#72689,#72690,#72691,#72692,#72693,#72694,#72695,
#72696,#72697,#72698,#72699,#72700,#72701),.UNSPECIFIED.,.F.,.F.,(4,3,3,
3,3,3,3,4),(283.872731227212,284.760678104445,285.759838378496,286.758998652547,
287.758158926597,288.757319200648,289.756479474699,290.155916534392),
 .UNSPECIFIED.);
#3006=B_SPLINE_CURVE_WITH_KNOTS('',3,(#72706,#72707,#72708,#72709,#72710,
#72711,#72712,#72713,#72714,#72715,#72716,#72717,#72718,#72719,#72720,#72721,
#72722,#72723,#72724,#72725,#72726,#72727),.UNSPECIFIED.,.F.,.F.,(4,3,3,
3,3,3,3,4),(-299.402942157465,-298.748921941155,-297.749761667104,-296.750601393054,
-295.751441119003,-294.752280844952,-293.753120570902,-293.119756850285),
 .UNSPECIFIED.);
#3007=B_SPLINE_CURVE_WITH_KNOTS('',3,(#72728,#72729,#72730,#72731,#72732,
#72733,#72734,#72735,#72736,#72737,#72738,#72739,#72740,#72741,#72742,#72743,
#72744,#72745,#72746,#72747,#72748,#72749),.UNSPECIFIED.,.F.,.F.,(4,3,3,
3,3,3,3,4),(290.155916534392,290.755639748749,291.7548000228,292.753960296851,
293.753120570902,294.752280844952,295.751441119003,296.439101841571),
 .UNSPECIFIED.);
#3008=B_SPLINE_CURVE_WITH_KNOTS('',3,(#72754,#72755,#72756,#72757,#72758,
#72759,#72760,#72761,#72762,#72763,#72764,#72765,#72766,#72767,#72768,#72769,
#72770,#72771,#72772,#72773,#72774,#72775),.UNSPECIFIED.,.F.,.F.,(4,3,3,
3,3,3,3,4),(-305.686127464644,-304.743883585459,-303.744723311408,-302.745563037358,
-301.746402763307,-300.747242489256,-299.748082215206,-299.402942157465),
 .UNSPECIFIED.);
#3009=B_SPLINE_CURVE_WITH_KNOTS('',3,(#72776,#72777,#72778,#72779,#72780,
#72781,#72782,#72783,#72784,#72785,#72786,#72787,#72788,#72789,#72790,#72791,
#72792,#72793,#72794,#72795,#72796,#72797),.UNSPECIFIED.,.F.,.F.,(4,3,3,
3,3,3,3,4),(296.439101841571,296.750601393054,297.749761667104,298.748921941155,
299.748082215206,300.747242489256,301.746402763307,302.722287148751),
 .UNSPECIFIED.);
#3010=B_SPLINE_CURVE_WITH_KNOTS('',3,(#72802,#72803,#72804,#72805,#72806,
#72807,#72808,#72809,#72810,#72811,#72812,#72813,#72814,#72815,#72816,#72817,
#72818,#72819,#72820,#72821,#72822,#72823,#72824,#72825,#72826),
 .UNSPECIFIED.,.F.,.F.,(4,3,3,3,3,3,3,3,4),(-311.969312771824,-311.738005503814,
-310.738845229763,-309.739684955712,-308.740524681662,-307.741364407611,
-306.74220413356,-305.74304385951,-305.686127464644),.UNSPECIFIED.);
#3011=B_SPLINE_CURVE_WITH_KNOTS('',3,(#72827,#72828,#72829,#72830,#72831,
#72832,#72833,#72834,#72835,#72836,#72837,#72838,#72839,#72840,#72841,#72842,
#72843,#72844,#72845,#72846,#72847,#72848,#72849,#72850,#72851),
 .UNSPECIFIED.,.F.,.F.,(4,3,3,3,3,3,3,3,4),(302.722287148751,302.745563037358,
303.744723311408,304.743883585459,305.74304385951,306.74220413356,307.741364407611,
308.740524681662,309.00547245593),.UNSPECIFIED.);
#3012=B_SPLINE_CURVE_WITH_KNOTS('',3,(#72856,#72857,#72858,#72859,#72860,
#72861,#72862,#72863,#72864,#72865,#72866,#72867,#72868,#72869,#72870,#72871,
#72872,#72873,#72874,#72875,#72876,#72877),.UNSPECIFIED.,.F.,.F.,(4,3,3,
3,3,3,3,4),(-318.252498079003,-317.732967148118,-316.733806874067,-315.734646600017,
-314.735486325966,-313.736326051915,-312.737165777864,-311.969312771824),
 .UNSPECIFIED.);
#3013=B_SPLINE_CURVE_WITH_KNOTS('',3,(#72878,#72879,#72880,#72881,#72882,
#72883,#72884,#72885,#72886,#72887,#72888,#72889,#72890,#72891,#72892,#72893,
#72894,#72895,#72896,#72897,#72898,#72899),.UNSPECIFIED.,.F.,.F.,(4,3,3,
3,3,3,3,4),(309.00547245593,309.739684955712,310.738845229763,311.738005503814,
312.737165777865,313.736326051915,314.735486325966,315.28865776311),
 .UNSPECIFIED.);
#3014=B_SPLINE_CURVE_WITH_KNOTS('',3,(#72904,#72905,#72906,#72907,#72908,
#72909,#72910,#72911,#72912,#72913,#72914,#72915,#72916,#72917,#72918,#72919,
#72920,#72921,#72922,#72923,#72924,#72925),.UNSPECIFIED.,.F.,.F.,(4,3,3,
3,3,3,3,4),(-324.535683386183,-323.727928792422,-322.728768518371,-321.729608244321,
-320.73044797027,-319.731287696219,-318.732127422169,-318.252498079003),
 .UNSPECIFIED.);
#3015=B_SPLINE_CURVE_WITH_KNOTS('',3,(#72926,#72927,#72928,#72929,#72930,
#72931,#72932,#72933,#72934,#72935,#72936,#72937,#72938,#72939,#72940,#72941,
#72942,#72943,#72944,#72945,#72946,#72947),.UNSPECIFIED.,.F.,.F.,(4,3,3,
3,3,3,3,4),(315.28865776311,315.734646600017,316.733806874067,317.732967148118,
318.732127422169,319.731287696219,320.73044797027,321.571843070289),
 .UNSPECIFIED.);
#3016=B_SPLINE_CURVE_WITH_KNOTS('',3,(#72952,#72953,#72954,#72955,#72956,
#72957,#72958,#72959,#72960,#72961,#72962,#72963,#72964,#72965,#72966,#72967,
#72968,#72969,#72970,#72971,#72972,#72973,#72974,#72975,#72976),
 .UNSPECIFIED.,.F.,.F.,(4,3,3,3,3,3,3,3,4),(-330.818868693363,-330.722050710777,
-329.722890436726,-328.723730162676,-327.724569888625,-326.725409614574,
-325.726249340523,-324.727089066473,-324.535683386183),.UNSPECIFIED.);
#3017=B_SPLINE_CURVE_WITH_KNOTS('',3,(#72977,#72978,#72979,#72980,#72981,
#72982,#72983,#72984,#72985,#72986,#72987,#72988,#72989,#72990,#72991,#72992,
#72993,#72994,#72995,#72996,#72997,#72998,#72999,#73000,#73001),
 .UNSPECIFIED.,.F.,.F.,(4,3,3,3,3,3,3,3,4),(321.571843070289,321.729608244321,
322.728768518371,323.727928792422,324.727089066473,325.726249340523,326.725409614574,
327.724569888625,327.855028377469),.UNSPECIFIED.);
#3018=B_SPLINE_CURVE_WITH_KNOTS('',3,(#73006,#73007,#73008,#73009,#73010,
#73011,#73012,#73013,#73014,#73015,#73016,#73017,#73018,#73019,#73020,#73021,
#73022,#73023,#73024,#73025,#73026,#73027),.UNSPECIFIED.,.F.,.F.,(4,3,3,
3,3,3,3,4),(-337.102054000542,-336.717012355081,-335.71785208103,-334.71869180698,
-333.719531532929,-332.720371258878,-331.721210984828,-330.818868693363),
 .UNSPECIFIED.);
#3019=B_SPLINE_CURVE_WITH_KNOTS('',3,(#73028,#73029,#73030,#73031,#73032,
#73033,#73034,#73035,#73036,#73037,#73038,#73039,#73040,#73041,#73042,#73043,
#73044,#73045,#73046,#73047,#73048,#73049),.UNSPECIFIED.,.F.,.F.,(4,3,3,
3,3,3,3,4),(327.855028377469,328.723730162675,329.722890436726,330.722050710777,
331.721210984828,332.720371258878,333.719531532929,334.138213684649),
 .UNSPECIFIED.);
#3020=B_SPLINE_CURVE_WITH_KNOTS('',3,(#73054,#73055,#73056,#73057,#73058,
#73059,#73060,#73061,#73062,#73063,#73064,#73065,#73066,#73067,#73068,#73069,
#73070,#73071,#73072,#73073,#73074,#73075),.UNSPECIFIED.,.F.,.F.,(4,3,3,
3,3,3,3,4),(-343.385239307722,-342.711973999385,-341.712813725334,-340.713653451284,
-339.714493177233,-338.715332903182,-337.716172629132,-337.102054000542),
 .UNSPECIFIED.);
#3021=B_SPLINE_CURVE_WITH_KNOTS('',3,(#73076,#73077,#73078,#73079,#73080,
#73081,#73082,#73083,#73084,#73085,#73086,#73087,#73088,#73089,#73090,#73091,
#73092,#73093,#73094,#73095,#73096,#73097),.UNSPECIFIED.,.F.,.F.,(4,3,3,
3,3,3,3,4),(334.138213684649,334.71869180698,335.71785208103,336.717012355081,
337.716172629132,338.715332903182,339.714493177233,340.421398991828),
 .UNSPECIFIED.);
#3022=B_SPLINE_CURVE_WITH_KNOTS('',3,(#73102,#73103,#73104,#73105,#73106,
#73107,#73108,#73109,#73110,#73111,#73112,#73113,#73114,#73115,#73116,#73117,
#73118,#73119,#73120,#73121,#73122,#73123),.UNSPECIFIED.,.F.,.F.,(4,3,3,
3,3,3,3,4),(-349.668424614901,-348.706935643689,-347.707775369639,-346.708615095588,
-345.709454821537,-344.710294547486,-343.711134273436,-343.385239307722),
 .UNSPECIFIED.);
#3023=B_SPLINE_CURVE_WITH_KNOTS('',3,(#73124,#73125,#73126,#73127,#73128,
#73129,#73130,#73131,#73132,#73133,#73134,#73135,#73136,#73137,#73138,#73139,
#73140,#73141,#73142,#73143,#73144,#73145),.UNSPECIFIED.,.F.,.F.,(4,3,3,
3,3,3,3,4),(340.421398991828,340.713653451284,341.712813725334,342.711973999385,
343.711134273436,344.710294547487,345.709454821537,346.704584299008),
 .UNSPECIFIED.);
#3024=B_SPLINE_CURVE_WITH_KNOTS('',3,(#73150,#73151,#73152,#73153,#73154,
#73155,#73156,#73157,#73158,#73159,#73160,#73161,#73162,#73163,#73164,#73165,
#73166,#73167,#73168,#73169,#73170,#73171,#73172,#73173,#73174),
 .UNSPECIFIED.,.F.,.F.,(4,3,3,3,3,3,3,3,4),(-355.951609922081,-355.701057562044,
-354.701897287993,-353.702737013943,-352.703576739892,-351.704416465841,
-350.705256191791,-349.70609591774,-349.668424614901),.UNSPECIFIED.);
#3025=B_SPLINE_CURVE_WITH_KNOTS('',3,(#73175,#73176,#73177,#73178,#73179,
#73180,#73181,#73182,#73183,#73184,#73185,#73186,#73187,#73188,#73189,#73190,
#73191,#73192,#73193,#73194,#73195,#73196,#73197,#73198,#73199),
 .UNSPECIFIED.,.F.,.F.,(4,3,3,3,3,3,3,3,4),(346.704584299008,346.708615095588,
347.707775369639,348.706935643689,349.70609591774,350.705256191791,351.704416465841,
352.703576739892,352.987769606187),.UNSPECIFIED.);
#3026=B_SPLINE_CURVE_WITH_KNOTS('',3,(#73204,#73205,#73206,#73207,#73208,
#73209,#73210,#73211,#73212,#73213,#73214,#73215,#73216,#73217,#73218,#73219,
#73220,#73221,#73222,#73223,#73224,#73225),.UNSPECIFIED.,.F.,.F.,(4,3,3,
3,3,3,3,4),(-362.23479522926,-361.696019206348,-360.696858932297,-359.697698658247,
-358.698538384196,-357.699378110145,-356.700217836095,-355.951609922081),
 .UNSPECIFIED.);
#3027=B_SPLINE_CURVE_WITH_KNOTS('',3,(#73226,#73227,#73228,#73229,#73230,
#73231,#73232,#73233,#73234,#73235,#73236,#73237,#73238,#73239,#73240,#73241,
#73242,#73243,#73244,#73245,#73246,#73247),.UNSPECIFIED.,.F.,.F.,(4,3,3,
3,3,3,3,4),(352.987769606187,353.702737013943,354.701897287993,355.701057562044,
356.700217836095,357.699378110145,358.698538384196,359.270954913367),
 .UNSPECIFIED.);
#3028=B_SPLINE_CURVE_WITH_KNOTS('',3,(#73252,#73253,#73254,#73255,#73256,
#73257,#73258,#73259,#73260,#73261,#73262,#73263,#73264,#73265,#73266,#73267,
#73268,#73269,#73270,#73271,#73272,#73273),.UNSPECIFIED.,.F.,.F.,(4,3,3,
3,3,3,3,4),(-368.51798053644,-367.690980850652,-366.691820576602,-365.692660302551,
-364.6935000285,-363.694339754449,-362.695179480399,-362.23479522926),
 .UNSPECIFIED.);
#3029=B_SPLINE_CURVE_WITH_KNOTS('',3,(#73274,#73275,#73276,#73277,#73278,
#73279,#73280,#73281,#73282,#73283,#73284,#73285,#73286,#73287,#73288,#73289,
#73290,#73291,#73292,#73293,#73294,#73295),.UNSPECIFIED.,.F.,.F.,(4,3,3,
3,3,3,3,4),(359.270954913367,359.697698658247,360.696858932297,361.696019206348,
362.695179480399,363.69433975445,364.6935000285,365.554140220546),
 .UNSPECIFIED.);
#3030=B_SPLINE_CURVE_WITH_KNOTS('',3,(#73300,#73301,#73302,#73303,#73304,
#73305,#73306,#73307,#73308,#73309,#73310,#73311,#73312,#73313,#73314,#73315,
#73316,#73317,#73318,#73319,#73320,#73321,#73322,#73323,#73324),
 .UNSPECIFIED.,.F.,.F.,(4,3,3,3,3,3,3,3,4),(-374.80116584362,-374.685102769007,
-373.685942494956,-372.686782220906,-371.687621946855,-370.688461672804,
-369.689301398754,-368.690141124703,-368.51798053644),.UNSPECIFIED.);
#3031=B_SPLINE_CURVE_WITH_KNOTS('',3,(#73325,#73326,#73327,#73328,#73329,
#73330,#73331,#73332,#73333,#73334,#73335,#73336,#73337,#73338,#73339,#73340,
#73341,#73342,#73343,#73344,#73345,#73346,#73347,#73348,#73349),
 .UNSPECIFIED.,.F.,.F.,(4,3,3,3,3,3,3,3,4),(365.554140220546,365.692660302551,
366.691820576602,367.690980850652,368.690141124703,369.689301398754,370.688461672804,
371.687621946855,371.837325527726),.UNSPECIFIED.);
#3032=B_SPLINE_CURVE_WITH_KNOTS('',3,(#73354,#73355,#73356,#73357,#73358,
#73359,#73360,#73361,#73362,#73363,#73364,#73365,#73366,#73367,#73368,#73369,
#73370,#73371,#73372,#73373,#73374,#73375),.UNSPECIFIED.,.F.,.F.,(4,3,3,
3,3,3,3,4),(-381.084351150799,-380.680064413311,-379.68090413926,-378.68174386521,
-377.682583591159,-376.683423317108,-375.684263043058,-374.80116584362),
 .UNSPECIFIED.);
#3033=B_SPLINE_CURVE_WITH_KNOTS('',3,(#73376,#73377,#73378,#73379,#73380,
#73381,#73382,#73383,#73384,#73385,#73386,#73387,#73388,#73389,#73390,#73391,
#73392,#73393,#73394,#73395,#73396,#73397),.UNSPECIFIED.,.F.,.F.,(4,3,3,
3,3,3,3,4),(371.837325527726,372.686782220906,373.685942494956,374.685102769007,
375.684263043058,376.683423317108,377.682583591159,378.120510834905),
 .UNSPECIFIED.);
#3034=B_SPLINE_CURVE_WITH_KNOTS('',3,(#73402,#73403,#73404,#73405,#73406,
#73407,#73408,#73409,#73410,#73411,#73412,#73413,#73414,#73415,#73416,#73417,
#73418,#73419,#73420,#73421,#73422,#73423),.UNSPECIFIED.,.F.,.F.,(4,3,3,
3,3,3,3,4),(-387.367536457979,-386.675026057615,-385.675865783564,-384.676705509514,
-383.677545235463,-382.678384961412,-381.679224687362,-381.084351150799),
 .UNSPECIFIED.);
#3035=B_SPLINE_CURVE_WITH_KNOTS('',3,(#73424,#73425,#73426,#73427,#73428,
#73429,#73430,#73431,#73432,#73433,#73434,#73435,#73436,#73437,#73438,#73439,
#73440,#73441,#73442,#73443,#73444,#73445),.UNSPECIFIED.,.F.,.F.,(4,3,3,
3,3,3,3,4),(378.120510834905,378.68174386521,379.68090413926,380.680064413311,
381.679224687362,382.678384961412,383.677545235463,384.403696142085),
 .UNSPECIFIED.);
#3036=B_SPLINE_CURVE_WITH_KNOTS('',3,(#73450,#73451,#73452,#73453,#73454,
#73455,#73456,#73457,#73458,#73459,#73460,#73461,#73462,#73463,#73464,#73465,
#73466,#73467,#73468,#73469,#73470,#73471),.UNSPECIFIED.,.F.,.F.,(4,3,3,
3,3,3,3,4),(-393.650721765158,-392.669987701919,-391.670827427869,-390.671667153818,
-389.672506879767,-388.673346605717,-387.674186331666,-387.367536457979),
 .UNSPECIFIED.);
#3037=B_SPLINE_CURVE_WITH_KNOTS('',3,(#73472,#73473,#73474,#73475,#73476,
#73477,#73478,#73479,#73480,#73481,#73482,#73483,#73484,#73485,#73486,#73487,
#73488,#73489,#73490,#73491,#73492,#73493,#73494,#73495,#73496),
 .UNSPECIFIED.,.F.,.F.,(4,3,3,3,3,3,3,3,4),(384.403696142085,384.676705509514,
385.675865783564,386.675026057615,387.674186331666,388.673346605717,389.672506879767,
390.671667153818,390.686881449265),.UNSPECIFIED.);
#3038=B_SPLINE_CURVE_WITH_KNOTS('',3,(#73501,#73502,#73503,#73504,#73505,
#73506,#73507,#73508,#73509,#73510,#73511,#73512,#73513,#73514,#73515,#73516,
#73517,#73518,#73519,#73520,#73521,#73522,#73523,#73524,#73525),
 .UNSPECIFIED.,.F.,.F.,(4,3,3,3,3,3,3,3,4),(-399.933907072338,-399.664109620274,
-398.664949346223,-397.665789072173,-396.666628798122,-395.667468524071,
-394.668308250021,-393.66914797597,-393.650721765158),.UNSPECIFIED.);
#3039=B_SPLINE_CURVE_WITH_KNOTS('',3,(#73526,#73527,#73528,#73529,#73530,
#73531,#73532,#73533,#73534,#73535,#73536,#73537,#73538,#73539,#73540,#73541,
#73542,#73543,#73544,#73545,#73546,#73547),.UNSPECIFIED.,.F.,.F.,(4,3,3,
3,3,3,3,4),(390.686881449265,391.670827427869,392.669987701919,393.66914797597,
394.668308250021,395.667468524071,396.666628798122,396.970066756444),
 .UNSPECIFIED.);
#3040=B_SPLINE_CURVE_WITH_KNOTS('',3,(#73552,#73553,#73554,#73555,#73556,
#73557,#73558,#73559,#73560,#73561,#73562,#73563,#73564,#73565,#73566,#73567,
#73568,#73569,#73570,#73571,#73572,#73573),.UNSPECIFIED.,.F.,.F.,(4,3,3,
3,3,3,3,4),(-406.217092379517,-405.659071264578,-404.659910990528,-403.660750716477,
-402.661590442426,-401.662430168375,-400.663269894325,-399.933907072338),
 .UNSPECIFIED.);
#3041=B_SPLINE_CURVE_WITH_KNOTS('',3,(#73574,#73575,#73576,#73577,#73578,
#73579,#73580,#73581,#73582,#73583,#73584,#73585,#73586,#73587,#73588,#73589,
#73590,#73591,#73592,#73593,#73594,#73595),.UNSPECIFIED.,.F.,.F.,(4,3,3,
3,3,3,3,4),(396.970066756444,397.665789072173,398.664949346223,399.664109620274,
400.663269894325,401.662430168376,402.661590442426,403.253252063624),
 .UNSPECIFIED.);
#3042=B_SPLINE_CURVE_WITH_KNOTS('',3,(#73600,#73601,#73602,#73603,#73604,
#73605,#73606,#73607,#73608,#73609,#73610,#73611,#73612,#73613,#73614,#73615,
#73616,#73617,#73618,#73619,#73620,#73621),.UNSPECIFIED.,.F.,.F.,(4,3,3,
3,3,3,3,4),(-412.500277686697,-411.654032908882,-410.654872634832,-409.655712360781,
-408.65655208673,-407.65739181268,-406.658231538629,-406.217092379517),
 .UNSPECIFIED.);
#3043=B_SPLINE_CURVE_WITH_KNOTS('',3,(#73622,#73623,#73624,#73625,#73626,
#73627,#73628,#73629,#73630,#73631,#73632,#73633,#73634,#73635,#73636,#73637,
#73638,#73639,#73640,#73641,#73642,#73643),.UNSPECIFIED.,.F.,.F.,(4,3,3,
3,3,3,3,4),(403.253252063624,403.660750716477,404.659910990528,405.659071264578,
406.658231538629,407.65739181268,408.65655208673,409.536437370803),
 .UNSPECIFIED.);
#3044=B_SPLINE_CURVE_WITH_KNOTS('',3,(#73648,#73649,#73650,#73651,#73652,
#73653,#73654,#73655,#73656,#73657,#73658,#73659,#73660,#73661,#73662,#73663,
#73664,#73665,#73666,#73667,#73668,#73669,#73670,#73671,#73672),
 .UNSPECIFIED.,.F.,.F.,(4,3,3,3,3,3,3,3,4),(-418.783462993876,-418.648154827237,
-417.648994553186,-416.649834279136,-415.650674005085,-414.651513731034,
-413.652353456984,-412.653193182933,-412.500277686697),.UNSPECIFIED.);
#3045=B_SPLINE_CURVE_WITH_KNOTS('',3,(#73673,#73674,#73675,#73676,#73677,
#73678,#73679,#73680,#73681,#73682,#73683,#73684,#73685,#73686,#73687,#73688,
#73689,#73690,#73691,#73692,#73693,#73694,#73695,#73696,#73697),
 .UNSPECIFIED.,.F.,.F.,(4,3,3,3,3,3,3,3,4),(409.536437370803,409.655712360781,
410.654872634832,411.654032908882,412.653193182933,413.652353456984,414.651513731034,
415.650674005085,415.819622677983),.UNSPECIFIED.);
#3046=B_SPLINE_CURVE_WITH_KNOTS('',3,(#73702,#73703,#73704,#73705,#73706,
#73707,#73708,#73709,#73710,#73711,#73712,#73713,#73714,#73715,#73716,#73717,
#73718,#73719,#73720,#73721,#73722,#73723),.UNSPECIFIED.,.F.,.F.,(4,3,3,
3,3,3,3,4),(-425.066648301056,-424.643116471541,-423.643956197491,-422.64479592344,
-421.645635649389,-420.646475375338,-419.647315101288,-418.783462993876),
 .UNSPECIFIED.);
#3047=B_SPLINE_CURVE_WITH_KNOTS('',3,(#73724,#73725,#73726,#73727,#73728,
#73729,#73730,#73731,#73732,#73733,#73734,#73735,#73736,#73737,#73738,#73739,
#73740,#73741,#73742,#73743,#73744,#73745),.UNSPECIFIED.,.F.,.F.,(4,3,3,
3,3,3,3,4),(415.819622677983,416.649834279136,417.648994553187,418.648154827237,
419.647315101288,420.646475375339,421.645635649389,422.102807985162),
 .UNSPECIFIED.);
#3048=B_SPLINE_CURVE_WITH_KNOTS('',3,(#73750,#73751,#73752,#73753,#73754,
#73755,#73756,#73757,#73758,#73759,#73760,#73761,#73762,#73763,#73764,#73765,
#73766,#73767,#73768,#73769,#73770,#73771),.UNSPECIFIED.,.F.,.F.,(4,3,3,
3,3,3,3,4),(-431.349833608236,-430.638078115845,-429.638917841795,-428.639757567744,
-427.640597293693,-426.641437019643,-425.642276745592,-425.066648301056),
 .UNSPECIFIED.);
#3049=B_SPLINE_CURVE_WITH_KNOTS('',3,(#73772,#73773,#73774,#73775,#73776,
#73777,#73778,#73779,#73780,#73781,#73782,#73783,#73784,#73785,#73786,#73787,
#73788,#73789,#73790,#73791,#73792,#73793),.UNSPECIFIED.,.F.,.F.,(4,3,3,
3,3,3,3,4),(422.102807985162,422.64479592344,423.643956197491,424.643116471541,
425.642276745592,426.641437019643,427.640597293693,428.385993292342),
 .UNSPECIFIED.);
#3050=B_SPLINE_CURVE_WITH_KNOTS('',3,(#73798,#73799,#73800,#73801,#73802,
#73803,#73804,#73805,#73806,#73807,#73808,#73809,#73810,#73811,#73812,#73813,
#73814,#73815,#73816,#73817,#73818,#73819),.UNSPECIFIED.,.F.,.F.,(4,3,3,
3,3,3,3,4),(-437.633018915415,-436.633039760149,-435.633879486099,-434.634719212048,
-433.635558937997,-432.636398663947,-431.637238389896,-431.349833608236),
 .UNSPECIFIED.);
#3051=B_SPLINE_CURVE_WITH_KNOTS('',3,(#73820,#73821,#73822,#73823,#73824,
#73825,#73826,#73827,#73828,#73829,#73830,#73831,#73832,#73833,#73834,#73835,
#73836,#73837,#73838,#73839,#73840,#73841,#73842,#73843,#73844),
 .UNSPECIFIED.,.F.,.F.,(4,3,3,3,3,3,3,3,4),(428.385993292342,428.639757567744,
429.638917841795,430.638078115845,431.637238389896,432.636398663947,433.635558937997,
434.634719212048,434.669178599522),.UNSPECIFIED.);
#3052=B_SPLINE_CURVE_WITH_KNOTS('',3,(#73849,#73850,#73851,#73852,#73853,
#73854,#73855,#73856,#73857,#73858,#73859,#73860,#73861,#73862,#73863,#73864,
#73865,#73866,#73867,#73868,#73869,#73870),.UNSPECIFIED.,.F.,.F.,(4,3,3,
3,3,3,3,4),(-443.916204222595,-443.627161678504,-442.628001404454,-441.628841130403,
-440.629680856352,-439.630520582302,-438.631360308251,-437.633018915415),
 .UNSPECIFIED.);
#3053=B_SPLINE_CURVE_WITH_KNOTS('',3,(#73871,#73872,#73873,#73874,#73875,
#73876,#73877,#73878,#73879,#73880,#73881,#73882,#73883,#73884,#73885,#73886,
#73887,#73888,#73889,#73890,#73891,#73892),.UNSPECIFIED.,.F.,.F.,(4,3,3,
3,3,3,3,4),(434.669178599522,435.633879486099,436.633039760149,437.6322000342,
438.631360308251,439.630520582302,440.629680856352,440.952363906701),
 .UNSPECIFIED.);
#3054=B_SPLINE_CURVE_WITH_KNOTS('',3,(#73897,#73898,#73899,#73900,#73901,
#73902,#73903,#73904,#73905,#73906,#73907,#73908,#73909,#73910,#73911,#73912,
#73913,#73914,#73915,#73916,#73917,#73918),.UNSPECIFIED.,.F.,.F.,(4,3,3,
3,3,3,3,4),(-450.199389529774,-449.622123322808,-448.622963048758,-447.623802774707,
-446.624642500656,-445.625482226606,-444.626321952555,-443.916204222595),
 .UNSPECIFIED.);
#3055=B_SPLINE_CURVE_WITH_KNOTS('',3,(#73919,#73920,#73921,#73922,#73923,
#73924,#73925,#73926,#73927,#73928,#73929,#73930,#73931,#73932,#73933,#73934,
#73935,#73936,#73937,#73938,#73939,#73940),.UNSPECIFIED.,.F.,.F.,(4,3,3,
3,3,3,3,4),(440.952363906701,441.628841130403,442.628001404454,443.627161678504,
444.626321952555,445.625482226606,446.624642500656,447.235549213881),
 .UNSPECIFIED.);
#3056=B_SPLINE_CURVE_WITH_KNOTS('',3,(#73945,#73946,#73947,#73948,#73949,
#73950,#73951,#73952,#73953,#73954,#73955,#73956,#73957,#73958,#73959,#73960,
#73961,#73962,#73963,#73964,#73965,#73966),.UNSPECIFIED.,.F.,.F.,(4,3,3,
3,3,3,3,4),(-456.482574836954,-455.617084967113,-454.617924693062,-453.618764419011,
-452.61960414496,-451.62044387091,-450.621283596859,-450.199389529774),
 .UNSPECIFIED.);
#3057=B_SPLINE_CURVE_WITH_KNOTS('',3,(#73967,#73968,#73969,#73970,#73971,
#73972,#73973,#73974,#73975,#73976,#73977,#73978,#73979,#73980,#73981,#73982,
#73983,#73984,#73985,#73986,#73987,#73988),.UNSPECIFIED.,.F.,.F.,(4,3,3,
3,3,3,3,4),(447.235549213881,447.623802774707,448.622963048758,449.622123322808,
450.621283596859,451.62044387091,452.61960414496,453.51873452106),
 .UNSPECIFIED.);
#3058=B_SPLINE_CURVE_WITH_KNOTS('',3,(#73993,#73994,#73995,#73996,#73997,
#73998,#73999,#74000,#74001,#74002,#74003,#74004,#74005,#74006,#74007,#74008,
#74009,#74010,#74011,#74012,#74013,#74014,#74015,#74016,#74017),
 .UNSPECIFIED.,.F.,.F.,(4,3,3,3,3,3,3,3,4),(-462.765760144133,-462.611206885467,
-461.612046611417,-460.612886337366,-459.613726063315,-458.614565789265,
-457.615405515214,-456.616245241163,-456.482574836954),.UNSPECIFIED.);
#3059=B_SPLINE_CURVE_WITH_KNOTS('',3,(#74018,#74019,#74020,#74021,#74022,
#74023,#74024,#74025,#74026,#74027,#74028,#74029,#74030,#74031,#74032,#74033,
#74034,#74035,#74036,#74037,#74038,#74039,#74040,#74041,#74042),
 .UNSPECIFIED.,.F.,.F.,(4,3,3,3,3,3,3,3,4),(453.51873452106,453.618764419011,
454.617924693062,455.617084967112,456.616245241163,457.615405515214,458.614565789265,
459.613726063315,459.80191982824),.UNSPECIFIED.);
#3060=B_SPLINE_CURVE_WITH_KNOTS('',3,(#74047,#74048,#74049,#74050,#74051,
#74052,#74053,#74054,#74055,#74056,#74057,#74058,#74059,#74060,#74061,#74062,
#74063,#74064,#74065,#74066,#74067,#74068),.UNSPECIFIED.,.F.,.F.,(4,3,3,
3,3,3,3,4),(-469.048945451313,-468.606168529771,-467.607008255721,-466.60784798167,
-465.608687707619,-464.609527433569,-463.610367159518,-462.765760144133),
 .UNSPECIFIED.);
#3061=B_SPLINE_CURVE_WITH_KNOTS('',3,(#74069,#74070,#74071,#74072,#74073,
#74074,#74075,#74076,#74077,#74078,#74079,#74080,#74081,#74082,#74083,#74084,
#74085,#74086,#74087,#74088,#74089,#74090),.UNSPECIFIED.,.F.,.F.,(4,3,3,
3,3,3,3,4),(459.80191982824,460.612886337366,461.612046611417,462.611206885467,
463.610367159518,464.609527433569,465.608687707619,466.085105135419),
 .UNSPECIFIED.);
#3062=B_SPLINE_CURVE_WITH_KNOTS('',3,(#74096,#74097,#74098,#74099,#74100),
 .UNSPECIFIED.,.F.,.F.,(4,1,4),(480.663675999238,481.220059351747,482.136507703335),
 .UNSPECIFIED.);
#3063=B_SPLINE_CURVE_WITH_KNOTS('',3,(#74103,#74104,#74105,#74106),
 .UNSPECIFIED.,.F.,.F.,(4,4),(480.663675999238,480.898195182615),
 .UNSPECIFIED.);
#3064=B_SPLINE_CURVE_WITH_KNOTS('',3,(#74111,#74112,#74113,#74114,#74115,
#74116,#74117,#74118,#74119,#74120),.UNSPECIFIED.,.F.,.F.,(4,1,1,1,1,1,
1,4),(474.380490692059,475.225097707443,476.224257981494,477.223418255545,
478.222578529595,479.221738803646,480.220899077697,480.663675999238),
 .UNSPECIFIED.);
#3065=B_SPLINE_CURVE_WITH_KNOTS('',3,(#74121,#74122,#74123,#74124,#74125,
#74126,#74127,#74128,#74129,#74130,#74131),.UNSPECIFIED.,.F.,.F.,(4,1,1,
1,1,1,1,1,4),(474.380490692059,474.903233538311,475.902393812361,476.901554086412,
477.900714360463,478.899874634513,479.899034908564,480.398615045589,480.663675999238),
 .UNSPECIFIED.);
#3066=B_SPLINE_CURVE_WITH_KNOTS('',3,(#74136,#74137,#74138,#74139,#74140,
#74141,#74142,#74143,#74144,#74145,#74146),.UNSPECIFIED.,.F.,.F.,(4,1,1,
1,1,1,1,1,4),(468.097305384879,468.230975789088,469.230136063139,470.22929633719,
471.228456611241,472.227616885291,473.226777159342,474.225937433393,474.380490692059),
 .UNSPECIFIED.);
#3067=B_SPLINE_CURVE_WITH_KNOTS('',3,(#74147,#74148,#74149,#74150,#74151,
#74152,#74153,#74154,#74155,#74156),.UNSPECIFIED.,.F.,.F.,(4,1,1,1,1,1,
1,4),(468.097305384879,468.908271894006,469.907432168057,470.906592442108,
471.905752716158,472.904912990209,473.90407326426,474.380490692059),
 .UNSPECIFIED.);
#3068=B_SPLINE_CURVE_WITH_KNOTS('',3,(#74161,#74162,#74163,#74164,#74165,
#74166,#74167,#74168,#74169,#74170),.UNSPECIFIED.,.F.,.F.,(4,1,1,1,1,1,
1,4),(461.814120077699,462.236014144784,463.235174418835,464.234334692886,
465.233494966936,466.232655240987,467.231815515038,468.097305384879),
 .UNSPECIFIED.);
#3069=B_SPLINE_CURVE_WITH_KNOTS('',3,(#74171,#74172,#74173,#74174,#74175,
#74176,#74177,#74178,#74179,#74180,#74181),.UNSPECIFIED.,.F.,.F.,(4,1,1,
1,1,1,1,1,4),(461.8141200777,461.914149975652,462.913310249702,463.912470523753,
464.911630797804,465.910791071854,466.909951345905,467.909111619956,468.097305384879),
 .UNSPECIFIED.);
#3070=B_SPLINE_CURVE_WITH_KNOTS('',3,(#74186,#74187,#74188,#74189,#74190,
#74191,#74192,#74193,#74194,#74195),.UNSPECIFIED.,.F.,.F.,(4,1,1,1,1,1,
1,4),(455.53093477052,456.24105250048,457.240212774531,458.239373048582,
459.238533322632,460.237693596683,461.236853870734,461.814120077699),
 .UNSPECIFIED.);
#3071=B_SPLINE_CURVE_WITH_KNOTS('',3,(#74196,#74197,#74198,#74199,#74200,
#74201,#74202,#74203,#74204,#74205),.UNSPECIFIED.,.F.,.F.,(4,1,1,1,1,1,
1,4),(455.53093477052,455.919188331348,456.918348605398,457.917508879449,
458.9166691535,459.91582942755,460.914989701601,461.8141200777),
 .UNSPECIFIED.);
#3072=B_SPLINE_CURVE_WITH_KNOTS('',3,(#74210,#74211,#74212,#74213,#74214,
#74215,#74216,#74217,#74218,#74219),.UNSPECIFIED.,.F.,.F.,(4,1,1,1,1,1,
1,4),(449.24774946334,450.246090856176,451.245251130227,452.244411404278,
453.243571678328,454.242731952379,455.24189222643,455.53093477052),
 .UNSPECIFIED.);
#3073=B_SPLINE_CURVE_WITH_KNOTS('',3,(#74220,#74221,#74222,#74223,#74224,
#74225,#74226,#74227,#74228,#74229),.UNSPECIFIED.,.F.,.F.,(4,1,1,1,1,1,
1,4),(449.24774946334,449.924226687043,450.923386961094,451.922547235145,
452.921707509195,453.920867783246,454.920028057297,455.53093477052),
 .UNSPECIFIED.);
#3074=B_SPLINE_CURVE_WITH_KNOTS('',3,(#74234,#74235,#74236,#74237,#74238,
#74239,#74240,#74241,#74242,#74243,#74244),.UNSPECIFIED.,.F.,.F.,(4,1,1,
1,1,1,1,1,4),(442.964564156161,443.251968937821,444.251129211872,445.250289485923,
446.249449759973,447.248610034024,448.247770308075,449.246930582125,449.24774946334),
 .UNSPECIFIED.);
#3075=B_SPLINE_CURVE_WITH_KNOTS('',3,(#74245,#74246,#74247,#74248,#74249,
#74250,#74251,#74252,#74253,#74254),.UNSPECIFIED.,.F.,.F.,(4,1,1,1,1,1,
1,4),(442.964564156161,443.929265042739,444.92842531679,445.927585590841,
446.926745864891,447.925906138942,448.925066412993,449.24774946334),
 .UNSPECIFIED.);
#3076=B_SPLINE_CURVE_WITH_KNOTS('',3,(#74259,#74260,#74261,#74262,#74263,
#74264,#74265,#74266,#74267,#74268),.UNSPECIFIED.,.F.,.F.,(4,1,1,1,1,1,
1,4),(436.681378848981,437.257007293517,438.256167567568,439.255327841619,
440.254488115669,441.25364838972,442.252808663771,442.964564156161),
 .UNSPECIFIED.);
#3077=B_SPLINE_CURVE_WITH_KNOTS('',3,(#74269,#74270,#74271,#74272,#74273,
#74274,#74275,#74276,#74277,#74278,#74279),.UNSPECIFIED.,.F.,.F.,(4,1,1,
1,1,1,1,1,4),(436.681378848981,436.935143124384,437.934303398435,438.933463672486,
439.932623946537,440.931784220587,441.930944494638,442.930104768689,442.964564156161),
 .UNSPECIFIED.);
#3078=B_SPLINE_CURVE_WITH_KNOTS('',3,(#74284,#74285,#74286,#74287,#74288,
#74289,#74290,#74291,#74292,#74293),.UNSPECIFIED.,.F.,.F.,(4,1,1,1,1,1,
1,4),(430.398193541802,431.262045649213,432.261205923264,433.260366197314,
434.259526471365,435.258686745416,436.257847019467,436.681378848981),
 .UNSPECIFIED.);
#3079=B_SPLINE_CURVE_WITH_KNOTS('',3,(#74294,#74295,#74296,#74297,#74298,
#74299,#74300,#74301,#74302,#74303),.UNSPECIFIED.,.F.,.F.,(4,1,1,1,1,1,
1,4),(430.398193541802,430.94018148008,431.939341754131,432.938502028182,
433.937662302232,434.936822576283,435.935982850334,436.681378848981),
 .UNSPECIFIED.);
#3080=B_SPLINE_CURVE_WITH_KNOTS('',3,(#74308,#74309,#74310,#74311,#74312,
#74313,#74314,#74315,#74316,#74317,#74318),.UNSPECIFIED.,.F.,.F.,(4,1,1,
1,1,1,1,1,4),(424.115008234622,424.267923730858,425.267084004909,426.26624427896,
427.26540455301,428.264564827061,429.263725101112,430.262885375162,430.398193541802),
 .UNSPECIFIED.);
#3081=B_SPLINE_CURVE_WITH_KNOTS('',3,(#74319,#74320,#74321,#74322,#74323,
#74324,#74325,#74326,#74327,#74328),.UNSPECIFIED.,.F.,.F.,(4,1,1,1,1,1,
1,4),(424.115008234622,424.945219835776,425.944380109827,426.943540383878,
427.942700657928,428.941860931979,429.94102120603,430.398193541802),
 .UNSPECIFIED.);
#3082=B_SPLINE_CURVE_WITH_KNOTS('',3,(#74333,#74334,#74335,#74336,#74337,
#74338,#74339,#74340,#74341,#74342),.UNSPECIFIED.,.F.,.F.,(4,1,1,1,1,1,
1,4),(417.831822927443,418.272962086554,419.272122360605,420.271282634656,
421.270442908706,422.269603182757,423.268763456808,424.115008234622),
 .UNSPECIFIED.);
#3083=B_SPLINE_CURVE_WITH_KNOTS('',3,(#74343,#74344,#74345,#74346,#74347,
#74348,#74349,#74350,#74351,#74352,#74353),.UNSPECIFIED.,.F.,.F.,(4,1,1,
1,1,1,1,1,4),(417.831822927443,417.951097917421,418.950258191472,419.949418465523,
420.948578739574,421.947739013624,422.946899287675,423.946059561726,424.115008234622),
 .UNSPECIFIED.);
#3084=B_SPLINE_CURVE_WITH_KNOTS('',3,(#74358,#74359,#74360,#74361,#74362,
#74363,#74364,#74365,#74366,#74367),.UNSPECIFIED.,.F.,.F.,(4,1,1,1,1,1,
1,4),(411.548637620263,412.27800044225,413.277160716301,414.276320990351,
415.275481264402,416.274641538453,417.273801812504,417.831822927443),
 .UNSPECIFIED.);
#3085=B_SPLINE_CURVE_WITH_KNOTS('',3,(#74368,#74369,#74370,#74371,#74372,
#74373,#74374,#74375,#74376,#74377),.UNSPECIFIED.,.F.,.F.,(4,1,1,1,1,1,
1,4),(411.548637620263,411.956136273117,412.955296547168,413.954456821219,
414.953617095269,415.95277736932,416.951937643371,417.831822927443),
 .UNSPECIFIED.);
#3086=B_SPLINE_CURVE_WITH_KNOTS('',3,(#74382,#74383,#74384,#74385,#74386,
#74387,#74388,#74389,#74390,#74391,#74392),.UNSPECIFIED.,.F.,.F.,(4,1,1,
1,1,1,1,1,4),(405.265452313083,405.283878523895,406.283038797946,407.282199071997,
408.281359346047,409.280519620098,410.279679894149,411.278840168199,411.548637620263),
 .UNSPECIFIED.);
#3087=B_SPLINE_CURVE_WITH_KNOTS('',3,(#74393,#74394,#74395,#74396,#74397,
#74398,#74399,#74400,#74401,#74402),.UNSPECIFIED.,.F.,.F.,(4,1,1,1,1,1,
1,4),(405.265452313083,405.961174628813,406.960334902864,407.959495176915,
408.958655450965,409.957815725016,410.956975999067,411.548637620263),
 .UNSPECIFIED.);
#3088=B_SPLINE_CURVE_WITH_KNOTS('',3,(#74407,#74408,#74409,#74410,#74411,
#74412,#74413,#74414,#74415,#74416),.UNSPECIFIED.,.F.,.F.,(4,1,1,1,1,1,
1,4),(398.982267005904,399.288916879591,400.288077153642,401.287237427693,
402.286397701743,403.285557975794,404.284718249845,405.265452313083),
 .UNSPECIFIED.);
#3089=B_SPLINE_CURVE_WITH_KNOTS('',3,(#74417,#74418,#74419,#74420,#74421,
#74422,#74423,#74424,#74425,#74426),.UNSPECIFIED.,.F.,.F.,(4,1,1,1,1,1,
1,4),(398.982267005904,399.966212984509,400.96537325856,401.964533532611,
402.963693806661,403.962854080712,404.962014354763,405.265452313083),
 .UNSPECIFIED.);
#3090=B_SPLINE_CURVE_WITH_KNOTS('',3,(#74431,#74432,#74433,#74434,#74435,
#74436,#74437,#74438,#74439,#74440),.UNSPECIFIED.,.F.,.F.,(4,1,1,1,1,1,
1,4),(392.699081698724,393.293955235287,394.293115509338,395.292275783388,
396.291436057439,397.29059633149,398.289756605541,398.982267005904),
 .UNSPECIFIED.);
#3091=B_SPLINE_CURVE_WITH_KNOTS('',3,(#74441,#74442,#74443,#74444,#74445,
#74446,#74447,#74448,#74449,#74450,#74451),.UNSPECIFIED.,.F.,.F.,(4,1,1,
1,1,1,1,1,4),(392.699081698724,392.972091066154,393.971251340205,394.970411614256,
395.969571888306,396.968732162357,397.967892436408,398.967052710458,398.982267005904),
 .UNSPECIFIED.);
#3092=B_SPLINE_CURVE_WITH_KNOTS('',3,(#74456,#74457,#74458,#74459,#74460,
#74461,#74462,#74463,#74464,#74465),.UNSPECIFIED.,.F.,.F.,(4,1,1,1,1,1,
1,4),(386.415896391545,387.298993590983,388.298153865034,389.297314139084,
390.296474413135,391.295634687186,392.294794961236,392.699081698724),
 .UNSPECIFIED.);
#3093=B_SPLINE_CURVE_WITH_KNOTS('',3,(#74466,#74467,#74468,#74469,#74470,
#74471,#74472,#74473,#74474,#74475),.UNSPECIFIED.,.F.,.F.,(4,1,1,1,1,1,
1,4),(386.415896391545,386.97712942185,387.976289695901,388.975449969952,
389.974610244002,390.973770518053,391.972930792104,392.699081698724),
 .UNSPECIFIED.);
#3094=B_SPLINE_CURVE_WITH_KNOTS('',3,(#74480,#74481,#74482,#74483,#74484,
#74485,#74486,#74487,#74488,#74489,#74490),.UNSPECIFIED.,.F.,.F.,(4,1,1,
1,1,1,1,1,4),(380.132711084365,380.304871672628,381.304031946679,382.303192220729,
383.30235249478,384.301512768831,385.300673042882,386.299833316932,386.415896391545),
 .UNSPECIFIED.);
#3095=B_SPLINE_CURVE_WITH_KNOTS('',3,(#74491,#74492,#74493,#74494,#74495,
#74496,#74497,#74498,#74499,#74500),.UNSPECIFIED.,.F.,.F.,(4,1,1,1,1,1,
1,4),(380.132711084365,380.982167777546,381.981328051597,382.980488325648,
383.979648599698,384.978808873749,385.9779691478,386.415896391545),
 .UNSPECIFIED.);
#3096=B_SPLINE_CURVE_WITH_KNOTS('',3,(#74505,#74506,#74507,#74508,#74509,
#74510,#74511,#74512,#74513,#74514),.UNSPECIFIED.,.F.,.F.,(4,1,1,1,1,1,
1,4),(373.849525777186,374.309910028324,375.309070302375,376.308230576425,
377.307390850476,378.306551124527,379.305711398577,380.132711084365),
 .UNSPECIFIED.);
#3097=B_SPLINE_CURVE_WITH_KNOTS('',3,(#74515,#74516,#74517,#74518,#74519,
#74520,#74521,#74522,#74523,#74524,#74525),.UNSPECIFIED.,.F.,.F.,(4,1,1,
1,1,1,1,1,4),(373.849525777186,373.988045859191,374.987206133242,375.986366407293,
376.985526681343,377.984686955394,378.983847229445,379.983007503495,380.132711084365),
 .UNSPECIFIED.);
#3098=B_SPLINE_CURVE_WITH_KNOTS('',3,(#74530,#74531,#74532,#74533,#74534,
#74535,#74536,#74537,#74538,#74539),.UNSPECIFIED.,.F.,.F.,(4,1,1,1,1,1,
1,4),(367.566340470006,368.31494838402,369.314108658071,370.313268932121,
371.312429206172,372.311589480223,373.310749754273,373.849525777186),
 .UNSPECIFIED.);
#3099=B_SPLINE_CURVE_WITH_KNOTS('',3,(#74540,#74541,#74542,#74543,#74544,
#74545,#74546,#74547,#74548,#74549),.UNSPECIFIED.,.F.,.F.,(4,1,1,1,1,1,
1,4),(367.566340470006,367.993084214887,368.992244488938,369.991404762989,
370.990565037039,371.98972531109,372.988885585141,373.849525777186),
 .UNSPECIFIED.);
#3100=B_SPLINE_CURVE_WITH_KNOTS('',3,(#74554,#74555,#74556,#74557,#74558,
#74559,#74560,#74561,#74562,#74563,#74564),.UNSPECIFIED.,.F.,.F.,(4,1,1,
1,1,1,1,1,4),(361.283155162826,361.320826465665,362.319986739716,363.319147013766,
364.318307287817,365.317467561868,366.316627835919,367.315788109969,367.566340470006),
 .UNSPECIFIED.);
#3101=B_SPLINE_CURVE_WITH_KNOTS('',3,(#74565,#74566,#74567,#74568,#74569,
#74570,#74571,#74572,#74573,#74574),.UNSPECIFIED.,.F.,.F.,(4,1,1,1,1,1,
1,4),(361.283155162827,361.998122570583,362.997282844634,363.996443118684,
364.995603392735,365.994763666786,366.993923940837,367.566340470006),
 .UNSPECIFIED.);
#3102=B_SPLINE_CURVE_WITH_KNOTS('',3,(#74579,#74580,#74581,#74582,#74583,
#74584,#74585,#74586,#74587,#74588),.UNSPECIFIED.,.F.,.F.,(4,1,1,1,1,1,
1,4),(354.999969855647,355.325864821361,356.325025095412,357.324185369462,
358.323345643513,359.322505917564,360.321666191614,361.283155162826),
 .UNSPECIFIED.);
#3103=B_SPLINE_CURVE_WITH_KNOTS('',3,(#74589,#74590,#74591,#74592,#74593,
#74594,#74595,#74596,#74597,#74598,#74599),.UNSPECIFIED.,.F.,.F.,(4,1,1,
1,1,1,1,1,4),(354.999969855647,355.004000652228,356.003160926279,357.00232120033,
358.00148147438,359.000641748431,359.999802022482,360.998962296532,361.283155162827),
 .UNSPECIFIED.);
#3104=B_SPLINE_CURVE_WITH_KNOTS('',3,(#74604,#74605,#74606,#74607,#74608,
#74609,#74610,#74611,#74612,#74613),.UNSPECIFIED.,.F.,.F.,(4,1,1,1,1,1,
1,4),(348.716784548467,349.330903177057,350.330063451108,351.329223725158,
352.328383999209,353.32754427326,354.32670454731,354.999969855647),
 .UNSPECIFIED.);
#3105=B_SPLINE_CURVE_WITH_KNOTS('',3,(#74614,#74615,#74616,#74617,#74618,
#74619,#74620,#74621,#74622,#74623),.UNSPECIFIED.,.F.,.F.,(4,1,1,1,1,1,
1,4),(348.716784548468,349.009039007924,350.008199281975,351.007359556026,
352.006519830076,353.005680104127,354.004840378178,354.999969855647),
 .UNSPECIFIED.);
#3106=B_SPLINE_CURVE_WITH_KNOTS('',3,(#74628,#74629,#74630,#74631,#74632,
#74633,#74634,#74635,#74636,#74637),.UNSPECIFIED.,.F.,.F.,(4,1,1,1,1,1,
1,4),(342.433599241288,343.335941532753,344.335101806803,345.334262080854,
346.333422354905,347.332582628956,348.331742903006,348.716784548467),
 .UNSPECIFIED.);
#3107=B_SPLINE_CURVE_WITH_KNOTS('',3,(#74638,#74639,#74640,#74641,#74642,
#74643,#74644,#74645,#74646,#74647),.UNSPECIFIED.,.F.,.F.,(4,1,1,1,1,1,
1,4),(342.433599241288,343.01407736362,344.013237637671,345.012397911721,
346.011558185772,347.010718459823,348.009878733874,348.716784548468),
 .UNSPECIFIED.);
#3108=B_SPLINE_CURVE_WITH_KNOTS('',3,(#74652,#74653,#74654,#74655,#74656,
#74657,#74658,#74659,#74660,#74661,#74662),.UNSPECIFIED.,.F.,.F.,(4,1,1,
1,1,1,1,1,4),(336.150413934108,336.341819614398,337.340979888449,338.340140162499,
339.33930043655,340.338460710601,341.337620984651,342.336781258702,342.433599241288),
 .UNSPECIFIED.);
#3109=B_SPLINE_CURVE_WITH_KNOTS('',3,(#74663,#74664,#74665,#74666,#74667,
#74668,#74669,#74670,#74671,#74672),.UNSPECIFIED.,.F.,.F.,(4,1,1,1,1,1,
1,4),(336.150413934108,337.019115719316,338.018275993367,339.017436267417,
340.016596541468,341.015756815519,342.014917089569,342.433599241288),
 .UNSPECIFIED.);
#3110=B_SPLINE_CURVE_WITH_KNOTS('',3,(#74677,#74678,#74679,#74680,#74681,
#74682,#74683,#74684,#74685,#74686),.UNSPECIFIED.,.F.,.F.,(4,1,1,1,1,1,
1,4),(329.867228626929,330.346857970094,331.346018244145,332.345178518195,
333.344338792246,334.343499066297,335.342659340347,336.150413934108),
 .UNSPECIFIED.);
#3111=B_SPLINE_CURVE_WITH_KNOTS('',3,(#74687,#74688,#74689,#74690,#74691,
#74692,#74693,#74694,#74695,#74696,#74697),.UNSPECIFIED.,.F.,.F.,(4,1,1,
1,1,1,1,1,4),(329.867228626929,330.024993800961,331.024154075012,332.023314349063,
333.022474623113,334.021634897164,335.020795171215,336.019955445265,336.150413934108),
 .UNSPECIFIED.);
#3112=B_SPLINE_CURVE_WITH_KNOTS('',3,(#74702,#74703,#74704,#74705,#74706,
#74707,#74708,#74709,#74710,#74711),.UNSPECIFIED.,.F.,.F.,(4,1,1,1,1,1,
1,4),(323.584043319749,324.35189632579,325.35105659984,326.350216873891,
327.349377147942,328.348537421993,329.347697696043,329.867228626929),
 .UNSPECIFIED.);
#3113=B_SPLINE_CURVE_WITH_KNOTS('',3,(#74712,#74713,#74714,#74715,#74716,
#74717,#74718,#74719,#74720,#74721),.UNSPECIFIED.,.F.,.F.,(4,1,1,1,1,1,
1,4),(323.584043319749,324.030032156657,325.029192430708,326.028352704758,
327.027512978809,328.02667325286,329.025833526911,329.867228626929),
 .UNSPECIFIED.);
#3114=B_SPLINE_CURVE_WITH_KNOTS('',3,(#74726,#74727,#74728,#74729,#74730,
#74731,#74732,#74733,#74734,#74735,#74736),.UNSPECIFIED.,.F.,.F.,(4,1,1,
1,1,1,1,1,4),(317.30085801257,317.357774407435,318.356934681486,319.356094955536,
320.355255229587,321.354415503638,322.353575777688,323.352736051739,323.584043319749),
 .UNSPECIFIED.);
#3115=B_SPLINE_CURVE_WITH_KNOTS('',3,(#74737,#74738,#74739,#74740,#74741,
#74742,#74743,#74744,#74745,#74746),.UNSPECIFIED.,.F.,.F.,(4,1,1,1,1,1,
1,4),(317.30085801257,318.035070512353,319.034230786404,320.033391060454,
321.032551334505,322.031711608556,323.030871882606,323.584043319749),
 .UNSPECIFIED.);
#3116=B_SPLINE_CURVE_WITH_KNOTS('',3,(#74751,#74752,#74753,#74754,#74755,
#74756,#74757,#74758,#74759,#74760),.UNSPECIFIED.,.F.,.F.,(4,1,1,1,1,1,
1,4),(311.01767270539,311.362812763131,312.361973037182,313.361133311232,
314.360293585283,315.359453859334,316.358614133384,317.30085801257),
 .UNSPECIFIED.);
#3117=B_SPLINE_CURVE_WITH_KNOTS('',3,(#74761,#74762,#74763,#74764,#74765,
#74766,#74767,#74768,#74769,#74770,#74771),.UNSPECIFIED.,.F.,.F.,(4,1,1,
1,1,1,1,1,4),(311.01767270539,311.040948593998,312.040108868049,313.039269142099,
314.03842941615,315.037589690201,316.036749964252,317.035910238302,317.30085801257),
 .UNSPECIFIED.);
#3118=B_SPLINE_CURVE_WITH_KNOTS('',3,(#74776,#74777,#74778,#74779,#74780,
#74781,#74782,#74783,#74784,#74785),.UNSPECIFIED.,.F.,.F.,(4,1,1,1,1,1,
1,4),(304.73448739821,305.367851118827,306.367011392877,307.366171666928,
308.365331940979,309.364492215029,310.36365248908,311.01767270539),
 .UNSPECIFIED.);
#3119=B_SPLINE_CURVE_WITH_KNOTS('',3,(#74786,#74787,#74788,#74789,#74790,
#74791,#74792,#74793,#74794,#74795),.UNSPECIFIED.,.F.,.F.,(4,1,1,1,1,1,
1,4),(304.73448739821,305.045986949694,306.045147223745,307.044307497795,
308.043467771846,309.042628045897,310.041788319947,311.01767270539),
 .UNSPECIFIED.);
#3120=B_SPLINE_CURVE_WITH_KNOTS('',3,(#74800,#74801,#74802,#74803,#74804,
#74805,#74806,#74807,#74808,#74809),.UNSPECIFIED.,.F.,.F.,(4,1,1,1,1,1,
1,4),(298.451302091031,299.372889474523,300.372049748573,301.371210022624,
302.370370296675,303.369530570725,304.368690844776,304.73448739821),
 .UNSPECIFIED.);
#3121=B_SPLINE_CURVE_WITH_KNOTS('',3,(#74810,#74811,#74812,#74813,#74814,
#74815,#74816,#74817,#74818,#74819),.UNSPECIFIED.,.F.,.F.,(4,1,1,1,1,1,
1,4),(298.451302091031,299.05102530539,300.050185579441,301.049345853491,
302.048506127542,303.047666401593,304.046826675643,304.73448739821),
 .UNSPECIFIED.);
#3122=B_SPLINE_CURVE_WITH_KNOTS('',3,(#74824,#74825,#74826,#74827,#74828,
#74829,#74830,#74831,#74832,#74833,#74834),.UNSPECIFIED.,.F.,.F.,(4,1,1,
1,1,1,1,1,4),(292.168116783851,292.378767556168,293.377927830219,294.377088104269,
295.37624837832,296.375408652371,297.374568926421,298.373729200472,298.451302091031),
 .UNSPECIFIED.);
#3123=B_SPLINE_CURVE_WITH_KNOTS('',3,(#74835,#74836,#74837,#74838,#74839,
#74840,#74841,#74842,#74843,#74844),.UNSPECIFIED.,.F.,.F.,(4,1,1,1,1,1,
1,4),(292.168116783851,293.056063661086,294.055223935136,295.054384209187,
296.053544483238,297.052704757289,298.051865031339,298.451302091031),
 .UNSPECIFIED.);
#3124=B_SPLINE_CURVE_WITH_KNOTS('',3,(#74849,#74850,#74851,#74852,#74853,
#74854,#74855,#74856,#74857,#74858),.UNSPECIFIED.,.F.,.F.,(4,1,1,1,1,1,
1,4),(285.884931476672,286.383805911864,287.382966185914,288.382126459965,
289.381286734016,290.380447008066,291.379607282117,292.168116783851),
 .UNSPECIFIED.);
#3125=B_SPLINE_CURVE_WITH_KNOTS('',3,(#74859,#74860,#74861,#74862,#74863,
#74864,#74865,#74866,#74867,#74868,#74869),.UNSPECIFIED.,.F.,.F.,(4,1,1,
1,1,1,1,1,4),(285.884931476672,286.061941742731,287.061102016782,288.060262290832,
289.059422564883,290.058582838934,291.057743112984,292.056903387035,292.168116783851),
 .UNSPECIFIED.);
#3126=B_SPLINE_CURVE_WITH_KNOTS('',3,(#74874,#74875,#74876,#74877,#74878,
#74879,#74880,#74881,#74882,#74883),.UNSPECIFIED.,.F.,.F.,(4,1,1,1,1,1,
1,4),(279.601746169492,280.38884426756,281.38800454161,282.387164815661,
283.386325089712,284.385485363762,285.384645637813,285.884931476672),
 .UNSPECIFIED.);
#3127=B_SPLINE_CURVE_WITH_KNOTS('',3,(#74884,#74885,#74886,#74887,#74888,
#74889,#74890,#74891,#74892,#74893),.UNSPECIFIED.,.F.,.F.,(4,1,1,1,1,1,
1,4),(279.601746169492,280.066980098427,281.066140372478,282.065300646528,
283.064460920579,284.06362119463,285.06278146868,285.884931476672),
 .UNSPECIFIED.);
#3128=B_SPLINE_CURVE_WITH_KNOTS('',3,(#74898,#74899,#74900,#74901,#74902,
#74903,#74904,#74905,#74906,#74907,#74908),.UNSPECIFIED.,.F.,.F.,(4,1,1,
1,1,1,1,1,4),(273.318560862313,273.394722349205,274.393882623256,275.393042897306,
276.392203171357,277.391363445408,278.390523719458,279.389683993509,279.601746169492),
 .UNSPECIFIED.);
#3129=B_SPLINE_CURVE_WITH_KNOTS('',3,(#74909,#74910,#74911,#74912,#74913,
#74914,#74915,#74916,#74917,#74918),.UNSPECIFIED.,.F.,.F.,(4,1,1,1,1,1,
1,4),(273.318560862313,274.072018454123,275.071178728173,276.070339002224,
277.069499276275,278.068659550326,279.067819824376,279.601746169492),
 .UNSPECIFIED.);
#3130=B_SPLINE_CURVE_WITH_KNOTS('',3,(#74923,#74924,#74925,#74926,#74927,
#74928,#74929,#74930,#74931,#74932),.UNSPECIFIED.,.F.,.F.,(4,1,1,1,1,1,
1,4),(267.035375555133,267.399760704901,268.398920978951,269.398081253002,
270.397241527053,271.396401801103,272.395562075154,273.318560862313),
 .UNSPECIFIED.);
#3131=B_SPLINE_CURVE_WITH_KNOTS('',3,(#74933,#74934,#74935,#74936,#74937,
#74938,#74939,#74940,#74941,#74942,#74943),.UNSPECIFIED.,.F.,.F.,(4,1,1,
1,1,1,1,1,4),(267.035375555133,267.077896535768,268.077056809819,269.076217083869,
270.07537735792,271.074537631971,272.073697906021,273.072858180072,273.318560862313),
 .UNSPECIFIED.);
#3132=B_SPLINE_CURVE_WITH_KNOTS('',3,(#74948,#74949,#74950,#74951,#74952,
#74953,#74954,#74955,#74956,#74957),.UNSPECIFIED.,.F.,.F.,(4,1,1,1,1,1,
1,4),(260.752190247953,261.404799060597,262.403959334647,263.403119608698,
264.402279882749,265.401440156799,266.40060043085,267.035375555133),
 .UNSPECIFIED.);
#3133=B_SPLINE_CURVE_WITH_KNOTS('',3,(#74958,#74959,#74960,#74961,#74962,
#74963,#74964,#74965,#74966,#74967),.UNSPECIFIED.,.F.,.F.,(4,1,1,1,1,1,
1,4),(260.752190247954,261.082934891464,262.082095165515,263.081255439565,
264.080415713616,265.079575987667,266.078736261717,267.035375555133),
 .UNSPECIFIED.);
#3134=B_SPLINE_CURVE_WITH_KNOTS('',3,(#74972,#74973,#74974,#74975,#74976,
#74977,#74978,#74979,#74980,#74981),.UNSPECIFIED.,.F.,.F.,(4,1,1,1,1,1,
1,4),(254.469004940774,255.409837416293,256.408997690343,257.408157964394,
258.407318238445,259.406478512495,260.405638786546,260.752190247953),
 .UNSPECIFIED.);
#3135=B_SPLINE_CURVE_WITH_KNOTS('',3,(#74982,#74983,#74984,#74985,#74986,
#74987,#74988,#74989,#74990,#74991),.UNSPECIFIED.,.F.,.F.,(4,1,1,1,1,1,
1,4),(254.469004940774,255.08797324716,256.08713352121,257.086293795261,
258.085454069312,259.084614343362,260.083774617413,260.752190247954),
 .UNSPECIFIED.);
#3136=B_SPLINE_CURVE_WITH_KNOTS('',3,(#74996,#74997,#74998,#74999,#75000,
#75001,#75002,#75003,#75004,#75005,#75006),.UNSPECIFIED.,.F.,.F.,(4,1,1,
1,1,1,1,1,4),(248.185819633594,248.415715497938,249.414875771988,250.414036046039,
251.41319632009,252.41235659414,253.411516868191,254.410677142242,254.469004940774),
 .UNSPECIFIED.);
#3137=B_SPLINE_CURVE_WITH_KNOTS('',3,(#75007,#75008,#75009,#75010,#75011,
#75012,#75013,#75014,#75015,#75016),.UNSPECIFIED.,.F.,.F.,(4,1,1,1,1,1,
1,4),(248.185819633594,249.093011602856,250.092171876906,251.091332150957,
252.090492425008,253.089652699058,254.088812973109,254.469004940774),
 .UNSPECIFIED.);
#3138=B_SPLINE_CURVE_WITH_KNOTS('',3,(#75021,#75022,#75023,#75024,#75025,
#75026,#75027,#75028,#75029,#75030),.UNSPECIFIED.,.F.,.F.,(4,1,1,1,1,1,
1,4),(241.902634326415,242.420753853634,243.419914127684,244.419074401735,
245.418234675786,246.417394949836,247.416555223887,248.185819633594),
 .UNSPECIFIED.);
#3139=B_SPLINE_CURVE_WITH_KNOTS('',3,(#75031,#75032,#75033,#75034,#75035,
#75036,#75037,#75038,#75039,#75040,#75041),.UNSPECIFIED.,.F.,.F.,(4,1,1,
1,1,1,1,1,4),(241.902634326415,242.098889684501,243.098049958552,244.097210232602,
245.096370506653,246.095530780704,247.094691054754,248.093851328805,248.185819633594),
 .UNSPECIFIED.);
#3140=B_SPLINE_CURVE_WITH_KNOTS('',3,(#75046,#75047,#75048,#75049,#75050,
#75051,#75052,#75053,#75054,#75055),.UNSPECIFIED.,.F.,.F.,(4,1,1,1,1,1,
1,4),(235.619449019235,236.42579220933,237.42495248338,238.424112757431,
239.423273031482,240.422433305532,241.421593579583,241.902634326415),
 .UNSPECIFIED.);
#3141=B_SPLINE_CURVE_WITH_KNOTS('',3,(#75056,#75057,#75058,#75059,#75060,
#75061,#75062,#75063,#75064,#75065),.UNSPECIFIED.,.F.,.F.,(4,1,1,1,1,1,
1,4),(235.619449019235,236.103928040197,237.103088314247,238.102248588298,
239.101408862349,240.100569136399,241.09972941045,241.902634326415),
 .UNSPECIFIED.);
#3142=B_SPLINE_CURVE_WITH_KNOTS('',3,(#75070,#75071,#75072,#75073,#75074,
#75075,#75076,#75077,#75078,#75079,#75080),.UNSPECIFIED.,.F.,.F.,(4,1,1,
1,1,1,1,1,4),(229.336263712056,229.431670290975,230.430830565025,231.429990839076,
232.429151113127,233.428311387177,234.427471661228,235.426631935279,235.619449019235),
 .UNSPECIFIED.);
#3143=B_SPLINE_CURVE_WITH_KNOTS('',3,(#75081,#75082,#75083,#75084,#75085,
#75086,#75087,#75088,#75089,#75090),.UNSPECIFIED.,.F.,.F.,(4,1,1,1,1,1,
1,4),(229.336263712056,230.108966395893,231.108126669943,232.107286943994,
233.106447218045,234.105607492095,235.104767766146,235.619449019235),
 .UNSPECIFIED.);
#3144=B_SPLINE_CURVE_WITH_KNOTS('',3,(#75095,#75096,#75097,#75098,#75099,
#75100,#75101,#75102,#75103,#75104),.UNSPECIFIED.,.F.,.F.,(4,1,1,1,1,1,
1,4),(223.053078404876,223.436708646671,224.435868920721,225.435029194772,
226.434189468823,227.433349742873,228.432510016924,229.336263712056),
 .UNSPECIFIED.);
#3145=B_SPLINE_CURVE_WITH_KNOTS('',3,(#75105,#75106,#75107,#75108,#75109,
#75110,#75111,#75112,#75113,#75114,#75115),.UNSPECIFIED.,.F.,.F.,(4,1,1,
1,1,1,1,1,4),(223.053078404876,223.114844477538,224.114004751588,225.113165025639,
226.11232529969,227.111485573741,228.110645847791,229.109806121842,229.336263712056),
 .UNSPECIFIED.);
#3146=B_SPLINE_CURVE_WITH_KNOTS('',3,(#75120,#75121,#75122,#75123,#75124,
#75125,#75126,#75127,#75128,#75129),.UNSPECIFIED.,.F.,.F.,(4,1,1,1,1,1,
1,4),(216.769893097696,217.441747002366,218.440907276417,219.440067550468,
220.439227824519,221.438388098569,222.43754837262,223.053078404876),
 .UNSPECIFIED.);
#3147=B_SPLINE_CURVE_WITH_KNOTS('',3,(#75130,#75131,#75132,#75133,#75134,
#75135,#75136,#75137,#75138,#75139),.UNSPECIFIED.,.F.,.F.,(4,1,1,1,1,1,
1,4),(216.769893097697,217.119882833234,218.119043107284,219.118203381335,
220.117363655386,221.116523929436,222.115684203487,223.053078404876),
 .UNSPECIFIED.);
#3148=B_SPLINE_CURVE_WITH_KNOTS('',3,(#75144,#75145,#75146,#75147,#75148,
#75149,#75150,#75151,#75152,#75153),.UNSPECIFIED.,.F.,.F.,(4,1,1,1,1,1,
1,4),(210.486707790517,211.446785358062,212.445945632113,213.445105906164,
214.444266180214,215.443426454265,216.442586728316,216.769893097696),
 .UNSPECIFIED.);
#3149=B_SPLINE_CURVE_WITH_KNOTS('',3,(#75154,#75155,#75156,#75157,#75158,
#75159,#75160,#75161,#75162,#75163),.UNSPECIFIED.,.F.,.F.,(4,1,1,1,1,1,
1,4),(210.486707790517,211.12492118893,212.12408146298,213.123241737031,
214.122402011082,215.121562285132,216.120722559183,216.769893097697),
 .UNSPECIFIED.);
#3150=B_SPLINE_CURVE_WITH_KNOTS('',3,(#75168,#75169,#75170,#75171,#75172,
#75173,#75174,#75175,#75176,#75177,#75178),.UNSPECIFIED.,.F.,.F.,(4,1,1,
1,1,1,1,1,4),(204.203522483337,204.452663439708,205.451823713758,206.450983987809,
207.45014426186,208.44930453591,209.448464809961,210.447625084012,210.486707790517),
 .UNSPECIFIED.);
#3151=B_SPLINE_CURVE_WITH_KNOTS('',3,(#75179,#75180,#75181,#75182,#75183,
#75184,#75185,#75186,#75187,#75188),.UNSPECIFIED.,.F.,.F.,(4,1,1,1,1,1,
1,4),(204.203522483338,205.129959544625,206.129119818676,207.128280092727,
208.127440366778,209.126600640828,210.125760914879,210.486707790517),
 .UNSPECIFIED.);
#3152=B_SPLINE_CURVE_WITH_KNOTS('',3,(#75193,#75194,#75195,#75196,#75197,
#75198,#75199,#75200,#75201,#75202),.UNSPECIFIED.,.F.,.F.,(4,1,1,1,1,1,
1,4),(197.920337176158,198.457701795403,199.456862069454,200.456022343505,
201.455182617555,202.454342891606,203.453503165657,204.203522483337),
 .UNSPECIFIED.);
#3153=B_SPLINE_CURVE_WITH_KNOTS('',3,(#75203,#75204,#75205,#75206,#75207,
#75208,#75209,#75210,#75211,#75212,#75213),.UNSPECIFIED.,.F.,.F.,(4,1,1,
1,1,1,1,1,4),(197.920337176158,198.135837626271,199.134997900321,200.134158174372,
201.133318448423,202.132478722473,203.131638996524,204.130799270575,204.203522483338),
 .UNSPECIFIED.);
#3154=B_SPLINE_CURVE_WITH_KNOTS('',3,(#75218,#75219,#75220,#75221,#75222,
#75223,#75224,#75225,#75226,#75227),.UNSPECIFIED.,.F.,.F.,(4,1,1,1,1,1,
1,4),(191.637151868978,192.462740151099,193.46190042515,194.461060699201,
195.460220973251,196.459381247302,197.458541521353,197.920337176158),
 .UNSPECIFIED.);
#3155=B_SPLINE_CURVE_WITH_KNOTS('',3,(#75228,#75229,#75230,#75231,#75232,
#75233,#75234,#75235,#75236,#75237),.UNSPECIFIED.,.F.,.F.,(4,1,1,1,1,1,
1,4),(191.637151868978,192.140875981967,193.140036256017,194.139196530068,
195.138356804119,196.137517078169,197.13667735222,197.920337176158),
 .UNSPECIFIED.);
#3156=B_SPLINE_CURVE_WITH_KNOTS('',3,(#75242,#75243,#75244,#75245,#75246,
#75247,#75248,#75249,#75250,#75251,#75252),.UNSPECIFIED.,.F.,.F.,(4,1,1,
1,1,1,1,1,4),(185.353966561799,185.468618232745,186.467778506795,187.466938780846,
188.466099054897,189.465259328947,190.464419602998,191.463579877049,191.637151868978),
 .UNSPECIFIED.);
#3157=B_SPLINE_CURVE_WITH_KNOTS('',3,(#75253,#75254,#75255,#75256,#75257,
#75258,#75259,#75260,#75261,#75262),.UNSPECIFIED.,.F.,.F.,(4,1,1,1,1,1,
1,4),(185.353966561799,186.145914337662,187.145074611713,188.144234885764,
189.143395159815,190.142555433865,191.141715707916,191.637151868978),
 .UNSPECIFIED.);
#3158=B_SPLINE_CURVE_WITH_KNOTS('',3,(#75267,#75268,#75269,#75270,#75271,
#75272,#75273,#75274,#75275,#75276),.UNSPECIFIED.,.F.,.F.,(4,1,1,1,1,1,
1,4),(179.070781254619,179.47365658844,180.472816862491,181.471977136542,
182.471137410592,183.470297684643,184.469457958694,185.353966561799),
 .UNSPECIFIED.);
#3159=B_SPLINE_CURVE_WITH_KNOTS('',3,(#75277,#75278,#75279,#75280,#75281,
#75282,#75283,#75284,#75285,#75286,#75287),.UNSPECIFIED.,.F.,.F.,(4,1,1,
1,1,1,1,1,4),(179.070781254619,179.151792419308,180.150952693358,181.150112967409,
182.14927324146,183.14843351551,184.147593789561,185.146754063612,185.353966561799),
 .UNSPECIFIED.);
#3160=B_SPLINE_CURVE_WITH_KNOTS('',3,(#75292,#75293,#75294,#75295,#75296,
#75297,#75298,#75299,#75300,#75301),.UNSPECIFIED.,.F.,.F.,(4,1,1,1,1,1,
1,4),(172.78759594744,173.478694944136,174.477855218187,175.477015492238,
176.476175766288,177.475336040339,178.47449631439,179.070781254619),
 .UNSPECIFIED.);
#3161=B_SPLINE_CURVE_WITH_KNOTS('',3,(#75302,#75303,#75304,#75305,#75306,
#75307,#75308,#75309,#75310,#75311),.UNSPECIFIED.,.F.,.F.,(4,1,1,1,1,1,
1,4),(172.78759594744,173.156830775004,174.155991049054,175.155151323105,
176.154311597156,177.153471871206,178.152632145257,179.070781254619),
 .UNSPECIFIED.);
#3162=B_SPLINE_CURVE_WITH_KNOTS('',3,(#75316,#75317,#75318,#75319,#75320,
#75321,#75322,#75323,#75324,#75325),.UNSPECIFIED.,.F.,.F.,(4,1,1,1,1,1,
1,4),(166.50441064026,167.483733299832,168.482893573883,169.482053847934,
170.481214121984,171.480374396035,172.479534670086,172.78759594744),
 .UNSPECIFIED.);
#3163=B_SPLINE_CURVE_WITH_KNOTS('',3,(#75326,#75327,#75328,#75329,#75330,
#75331,#75332,#75333,#75334,#75335),.UNSPECIFIED.,.F.,.F.,(4,1,1,1,1,1,
1,4),(166.50441064026,167.161869130699,168.16102940475,169.160189678801,
170.159349952851,171.158510226902,172.157670500953,172.78759594744),
 .UNSPECIFIED.);
#3164=B_SPLINE_CURVE_WITH_KNOTS('',3,(#75340,#75341,#75342,#75343,#75344,
#75345,#75346,#75347,#75348,#75349,#75350),.UNSPECIFIED.,.F.,.F.,(4,1,1,
1,1,1,1,1,4),(160.22122533308,160.489611381477,161.488771655528,162.487931929579,
163.487092203629,164.48625247768,165.485412751731,166.484573025782,166.50441064026),
 .UNSPECIFIED.);
#3165=B_SPLINE_CURVE_WITH_KNOTS('',3,(#75351,#75352,#75353,#75354,#75355,
#75356,#75357,#75358,#75359,#75360),.UNSPECIFIED.,.F.,.F.,(4,1,1,1,1,1,
1,4),(160.221225333081,161.166907486395,162.166067760446,163.165228034497,
164.164388308547,165.163548582598,166.162708856649,166.50441064026),
 .UNSPECIFIED.);
#3166=B_SPLINE_CURVE_WITH_KNOTS('',3,(#75365,#75366,#75367,#75368,#75369,
#75370,#75371,#75372,#75373,#75374),.UNSPECIFIED.,.F.,.F.,(4,1,1,1,1,1,
1,4),(153.938040025901,154.494649737173,155.493810011224,156.492970285275,
157.492130559325,158.491290833376,159.490451107427,160.22122533308),
 .UNSPECIFIED.);
#3167=B_SPLINE_CURVE_WITH_KNOTS('',3,(#75375,#75376,#75377,#75378,#75379,
#75380,#75381,#75382,#75383,#75384,#75385),.UNSPECIFIED.,.F.,.F.,(4,1,1,
1,1,1,1,1,4),(153.938040025901,154.172785568041,155.171945842091,156.171106116142,
157.170266390193,158.169426664243,159.168586938294,160.167747212345,160.221225333081),
 .UNSPECIFIED.);
#3168=B_SPLINE_CURVE_WITH_KNOTS('',3,(#75390,#75391,#75392,#75393,#75394,
#75395,#75396,#75397,#75398,#75399),.UNSPECIFIED.,.F.,.F.,(4,1,1,1,1,1,
1,4),(147.654854718721,148.499688092869,149.49884836692,150.498008640971,
151.497168915021,152.496329189072,153.495489463123,153.938040025901),
 .UNSPECIFIED.);
#3169=B_SPLINE_CURVE_WITH_KNOTS('',3,(#75400,#75401,#75402,#75403,#75404,
#75405,#75406,#75407,#75408,#75409),.UNSPECIFIED.,.F.,.F.,(4,1,1,1,1,1,
1,4),(147.654854718721,148.177823923736,149.176984197787,150.176144471838,
151.175304745888,152.174465019939,153.17362529399,153.938040025901),
 .UNSPECIFIED.);
#3170=B_SPLINE_CURVE_WITH_KNOTS('',3,(#75414,#75415,#75416,#75417,#75418,
#75419,#75420,#75421,#75422,#75423,#75424),.UNSPECIFIED.,.F.,.F.,(4,1,1,
1,1,1,1,1,4),(141.371669411542,141.505566174514,142.504726448565,143.503886722616,
144.503046996666,145.502207270717,146.501367544768,147.500527818819,147.654854718721),
 .UNSPECIFIED.);
#3171=B_SPLINE_CURVE_WITH_KNOTS('',3,(#75425,#75426,#75427,#75428,#75429,
#75430,#75431,#75432,#75433,#75434),.UNSPECIFIED.,.F.,.F.,(4,1,1,1,1,1,
1,4),(141.371669411542,142.182862279432,143.182022553483,144.181182827534,
145.180343101584,146.179503375635,147.178663649686,147.654854718721),
 .UNSPECIFIED.);
#3172=B_SPLINE_CURVE_WITH_KNOTS('',3,(#75439,#75440,#75441,#75442,#75443,
#75444,#75445,#75446,#75447,#75448),.UNSPECIFIED.,.F.,.F.,(4,1,1,1,1,1,
1,4),(135.088484104362,135.51060453021,136.509764804261,137.508925078312,
138.508085352362,139.507245626413,140.506405900464,141.371669411542),
 .UNSPECIFIED.);
#3173=B_SPLINE_CURVE_WITH_KNOTS('',3,(#75449,#75450,#75451,#75452,#75453,
#75454,#75455,#75456,#75457,#75458,#75459),.UNSPECIFIED.,.F.,.F.,(4,1,1,
1,1,1,1,1,4),(135.088484104362,135.188740361078,136.187900635128,137.187060909179,
138.18622118323,139.18538145728,140.184541731331,141.183702005382,141.371669411542),
 .UNSPECIFIED.);
#3174=B_SPLINE_CURVE_WITH_KNOTS('',3,(#75464,#75465,#75466,#75467,#75468,
#75469,#75470,#75471,#75472,#75473),.UNSPECIFIED.,.F.,.F.,(4,1,1,1,1,1,
1,4),(128.805298797183,129.515642885906,130.514803159957,131.513963434008,
132.513123708058,133.512283982109,134.51144425616,135.088484104362),
 .UNSPECIFIED.);
#3175=B_SPLINE_CURVE_WITH_KNOTS('',3,(#75474,#75475,#75476,#75477,#75478,
#75479,#75480,#75481,#75482,#75483),.UNSPECIFIED.,.F.,.F.,(4,1,1,1,1,1,
1,4),(128.805298797183,129.193778716773,130.192938990824,131.192099264875,
132.191259538925,133.190419812976,134.189580087027,135.088484104362),
 .UNSPECIFIED.);
#3176=B_SPLINE_CURVE_WITH_KNOTS('',3,(#75488,#75489,#75490,#75491,#75492,
#75493,#75494,#75495,#75496,#75497),.UNSPECIFIED.,.F.,.F.,(4,1,1,1,1,1,
1,4),(122.522113490003,123.520681241602,124.519841515653,125.519001789703,
126.518162063754,127.517322337805,128.516482611855,128.805298797183),
 .UNSPECIFIED.);
#3177=B_SPLINE_CURVE_WITH_KNOTS('',3,(#75498,#75499,#75500,#75501,#75502,
#75503,#75504,#75505,#75506,#75507),.UNSPECIFIED.,.F.,.F.,(4,1,1,1,1,1,
1,4),(122.522113490003,123.198817072469,124.19797734652,125.197137620571,
126.196297894621,127.195458168672,128.194618442723,128.805298797183),
 .UNSPECIFIED.);
#3178=B_SPLINE_CURVE_WITH_KNOTS('',3,(#75512,#75513,#75514,#75515,#75516,
#75517,#75518,#75519,#75520,#75521,#75522),.UNSPECIFIED.,.F.,.F.,(4,1,1,
1,1,1,1,1,4),(116.238928182823,116.526559323247,117.525719597298,118.524879871349,
119.524040145399,120.52320041945,121.522360693501,122.521520967551,122.522113490003),
 .UNSPECIFIED.);
#3179=B_SPLINE_CURVE_WITH_KNOTS('',3,(#75523,#75524,#75525,#75526,#75527,
#75528,#75529,#75530,#75531,#75532),.UNSPECIFIED.,.F.,.F.,(4,1,1,1,1,1,
1,4),(116.238928182824,117.203855428165,118.203015702216,119.202175976267,
120.201336250317,121.200496524368,122.199656798419,122.522113490003),
 .UNSPECIFIED.);
#3180=B_SPLINE_CURVE_WITH_KNOTS('',3,(#75537,#75538,#75539,#75540,#75541,
#75542,#75543,#75544,#75545,#75546),.UNSPECIFIED.,.F.,.F.,(4,1,1,1,1,1,
1,4),(109.955742875644,110.531597678943,111.530757952994,112.529918227045,
113.529078501095,114.528238775146,115.527399049197,116.238928182823),
 .UNSPECIFIED.);
#3181=B_SPLINE_CURVE_WITH_KNOTS('',3,(#75547,#75548,#75549,#75550,#75551,
#75552,#75553,#75554,#75555,#75556,#75557),.UNSPECIFIED.,.F.,.F.,(4,1,1,
1,1,1,1,1,4),(109.955742875644,110.20973350981,111.208893783861,112.208054057912,
113.207214331962,114.206374606013,115.205534880064,116.204695154114,116.238928182824),
 .UNSPECIFIED.);
#3182=B_SPLINE_CURVE_WITH_KNOTS('',3,(#75562,#75563,#75564,#75565,#75566,
#75567,#75568,#75569,#75570,#75571),.UNSPECIFIED.,.F.,.F.,(4,1,1,1,1,1,
1,4),(103.672557568464,104.536636034639,105.53579630869,106.53495658274,
107.534116856791,108.533277130842,109.532437404892,109.955742875644),
 .UNSPECIFIED.);
#3183=B_SPLINE_CURVE_WITH_KNOTS('',3,(#75572,#75573,#75574,#75575,#75576,
#75577,#75578,#75579,#75580,#75581),.UNSPECIFIED.,.F.,.F.,(4,1,1,1,1,1,
1,4),(103.672557568464,104.214771865506,105.213932139557,106.213092413608,
107.212252687658,108.211412961709,109.21057323576,109.955742875644),
 .UNSPECIFIED.);
#3184=B_SPLINE_CURVE_WITH_KNOTS('',3,(#75586,#75587,#75588,#75589,#75590,
#75591,#75592,#75593,#75594,#75595,#75596),.UNSPECIFIED.,.F.,.F.,(4,1,1,
1,1,1,1,1,4),(97.3893722612846,97.5425141162843,98.5416743903349,99.5408346643856,
100.539994938436,101.539155212487,102.538315486538,103.537475760588,103.672557568464),
 .UNSPECIFIED.);
#3185=B_SPLINE_CURVE_WITH_KNOTS('',3,(#75597,#75598,#75599,#75600,#75601,
#75602,#75603,#75604,#75605,#75606),.UNSPECIFIED.,.F.,.F.,(4,1,1,1,1,1,
1,4),(97.3893722612848,98.2198102212022,99.2189704952528,100.218130769304,
101.217291043354,102.216451317405,103.215611591456,103.672557568464),
 .UNSPECIFIED.);
#3186=B_SPLINE_CURVE_WITH_KNOTS('',3,(#75611,#75612,#75613,#75614,#75615,
#75616,#75617,#75618,#75619,#75620),.UNSPECIFIED.,.F.,.F.,(4,1,1,1,1,1,
1,4),(91.106186954105,91.5475524719801,92.5467127460308,93.5458730200815,
94.5450332941322,95.5441935681829,96.5433538422336,97.3893722612846),
 .UNSPECIFIED.);
#3187=B_SPLINE_CURVE_WITH_KNOTS('',3,(#75621,#75622,#75623,#75624,#75625,
#75626,#75627,#75628,#75629,#75630,#75631),.UNSPECIFIED.,.F.,.F.,(4,1,1,
1,1,1,1,1,4),(91.1061869541051,91.2256883028474,92.2248485768981,93.2240088509487,
94.2231691249994,95.2223293990501,96.2214896731008,97.2206499471515,97.3893722612848),
 .UNSPECIFIED.);
#3188=B_SPLINE_CURVE_WITH_KNOTS('',3,(#75636,#75637,#75638,#75639,#75640,
#75641,#75642,#75643,#75644,#75645),.UNSPECIFIED.,.F.,.F.,(4,1,1,1,1,1,
1,4),(84.8230016469254,85.552590827676,86.5517511017267,87.5509113757774,
88.5500716498281,89.5492319238788,90.5483921979294,91.106186954105),
 .UNSPECIFIED.);
#3189=B_SPLINE_CURVE_WITH_KNOTS('',3,(#75646,#75647,#75648,#75649,#75650,
#75651,#75652,#75653,#75654,#75655),.UNSPECIFIED.,.F.,.F.,(4,1,1,1,1,1,
1,4),(84.8230016469256,85.2307266585432,86.2298869325939,87.2290472066446,
88.2282074806953,89.227367754746,90.2265280287967,91.1061869541051),
 .UNSPECIFIED.);
#3190=B_SPLINE_CURVE_WITH_KNOTS('',3,(#75660,#75661,#75662,#75663,#75664,
#75665,#75666,#75667,#75668,#75669,#75670),.UNSPECIFIED.,.F.,.F.,(4,1,1,
1,1,1,1,1,4),(78.5398163397459,78.5584689093212,79.5576291833719,80.5567894574226,
81.5559497314733,82.555110005524,83.5542702795747,84.5534305536253,84.8230016469254),
 .UNSPECIFIED.);
#3191=B_SPLINE_CURVE_WITH_KNOTS('',3,(#75671,#75672,#75673,#75674,#75675,
#75676,#75677,#75678,#75679,#75680),.UNSPECIFIED.,.F.,.F.,(4,1,1,1,1,1,
1,4),(78.539816339746,79.2357650142391,80.2349252882898,81.2340855623405,
82.2332458363912,83.2324061104419,84.2315663844926,84.8230016469256),
 .UNSPECIFIED.);
#3192=B_SPLINE_CURVE_WITH_KNOTS('',3,(#75685,#75686,#75687,#75688,#75689,
#75690,#75691,#75692,#75693,#75694),.UNSPECIFIED.,.F.,.F.,(4,1,1,1,1,1,
1,4),(72.2566310325663,72.5635072650171,73.5626675390678,74.5618278131185,
75.5609880871692,76.5601483612199,77.5593086352705,78.5398163397459),
 .UNSPECIFIED.);
#3193=B_SPLINE_CURVE_WITH_KNOTS('',3,(#75695,#75696,#75697,#75698,#75699,
#75700,#75701,#75702,#75703,#75704),.UNSPECIFIED.,.F.,.F.,(4,1,1,1,1,1,
1,4),(72.2566310325664,73.240803369935,74.2399636439857,75.2391239180364,
76.2382841920871,77.2374444661378,78.2366047401885,78.539816339746),
 .UNSPECIFIED.);
#3194=B_SPLINE_CURVE_WITH_KNOTS('',3,(#75709,#75710,#75711,#75712,#75713,
#75714,#75715,#75716,#75717,#75718),.UNSPECIFIED.,.F.,.F.,(4,1,1,1,1,1,
1,4),(65.9734457253867,66.568545620713,67.5677058947637,68.5668661688144,
69.5660264428651,70.5651867169157,71.5643469909664,72.2566310325663),
 .UNSPECIFIED.);
#3195=B_SPLINE_CURVE_WITH_KNOTS('',3,(#75719,#75720,#75721,#75722,#75723,
#75724,#75725,#75726,#75727,#75728,#75729),.UNSPECIFIED.,.F.,.F.,(4,1,1,
1,1,1,1,1,4),(65.9734457253868,66.2466814515802,67.2458417256309,68.2450019996816,
69.2441622737323,70.243322547783,71.2424828218336,72.2416430958843,72.2566310325664),
 .UNSPECIFIED.);
#3196=B_SPLINE_CURVE_WITH_KNOTS('',3,(#75734,#75735,#75736,#75737,#75738,
#75739,#75740,#75741,#75742,#75743),.UNSPECIFIED.,.F.,.F.,(4,1,1,1,1,1,
1,4),(59.6902604182071,60.5735839764089,61.5727442504596,62.5719045245103,
63.5710647985609,64.5702250726116,65.5693853466623,65.9734457253867),
 .UNSPECIFIED.);
#3197=B_SPLINE_CURVE_WITH_KNOTS('',3,(#75744,#75745,#75746,#75747,#75748,
#75749,#75750,#75751,#75752,#75753),.UNSPECIFIED.,.F.,.F.,(4,1,1,1,1,1,
1,4),(59.6902604182072,60.2517198072761,61.2508800813268,62.2500403553775,
63.2492006294282,64.2483609034789,65.2475211775295,65.9734457253868),
 .UNSPECIFIED.);
#3198=B_SPLINE_CURVE_WITH_KNOTS('',3,(#75758,#75759,#75760,#75761,#75762,
#75763,#75764,#75765,#75766,#75767,#75768),.UNSPECIFIED.,.F.,.F.,(4,1,1,
1,1,1,1,1,4),(53.4070751110275,53.5794620580541,54.5786223321048,55.5777826061555,
56.5769428802061,57.5761031542568,58.5752634283075,59.5744237023582,59.6902604182071),
 .UNSPECIFIED.);
#3199=B_SPLINE_CURVE_WITH_KNOTS('',3,(#75769,#75770,#75771,#75772,#75773,
#75774,#75775,#75776,#75777,#75778),.UNSPECIFIED.,.F.,.F.,(4,1,1,1,1,1,
1,4),(53.4070751110276,54.256758162972,55.2559184370227,56.2550787110734,
57.2542389851241,58.2533992591747,59.2525595332254,59.6902604182072),
 .UNSPECIFIED.);
#3200=B_SPLINE_CURVE_WITH_KNOTS('',3,(#75783,#75784,#75785,#75786,#75787,
#75788,#75789,#75790,#75791,#75792),.UNSPECIFIED.,.F.,.F.,(4,1,1,1,1,1,
1,4),(47.1238898038479,47.58450041375,48.5836606878007,49.5828209618514,
50.581981235902,51.5811415099527,52.5803017840034,53.4070751110275),
 .UNSPECIFIED.);
#3201=B_SPLINE_CURVE_WITH_KNOTS('',3,(#75793,#75794,#75795,#75796,#75797,
#75798,#75799,#75800,#75801,#75802,#75803),.UNSPECIFIED.,.F.,.F.,(4,1,1,
1,1,1,1,1,4),(47.123889803848,47.2626362446172,48.2617965186679,49.2609567927186,
50.2601170667693,51.2592773408199,52.2584376148706,53.2575978889213,53.4070751110276),
 .UNSPECIFIED.);
#3202=B_SPLINE_CURVE_WITH_KNOTS('',3,(#75808,#75809,#75810,#75811,#75812,
#75813,#75814,#75815,#75816,#75817),.UNSPECIFIED.,.F.,.F.,(4,1,1,1,1,1,
1,4),(40.8407044966683,41.5895387694459,42.5886990434966,43.5878593175472,
44.5870195915979,45.5861798656486,46.5853401396993,47.1238898038479),
 .UNSPECIFIED.);
#3203=B_SPLINE_CURVE_WITH_KNOTS('',3,(#75818,#75819,#75820,#75821,#75822,
#75823,#75824,#75825,#75826,#75827),.UNSPECIFIED.,.F.,.F.,(4,1,1,1,1,1,
1,4),(40.8407044966684,41.2676746003131,42.2668348743638,43.2659951484145,
44.2651554224651,45.2643156965158,46.2634759705665,47.123889803848),
 .UNSPECIFIED.);
#3204=B_SPLINE_CURVE_WITH_KNOTS('',3,(#75832,#75833,#75834,#75835,#75836,
#75837,#75838,#75839,#75840,#75841,#75842),.UNSPECIFIED.,.F.,.F.,(4,1,1,
1,1,1,1,1,4),(34.5575191894887,34.5954168510911,35.5945771251418,36.5937373991924,
37.5928976732431,38.5920579472938,39.5912182213445,40.5903784953952,40.8407044966683),
 .UNSPECIFIED.);
#3205=B_SPLINE_CURVE_WITH_KNOTS('',3,(#75843,#75844,#75845,#75846,#75847,
#75848,#75849,#75850,#75851,#75852),.UNSPECIFIED.,.F.,.F.,(4,1,1,1,1,1,
1,4),(34.5575191894888,35.272712956009,36.2718732300597,37.2710335041103,
38.270193778161,39.2693540522117,40.2685143262624,40.8407044966684),
 .UNSPECIFIED.);
#3206=B_SPLINE_CURVE_WITH_KNOTS('',3,(#75857,#75858,#75859,#75860,#75861,
#75862,#75863,#75864,#75865,#75866),.UNSPECIFIED.,.F.,.F.,(4,1,1,1,1,1,
1,4),(28.2743338823091,28.600455206787,29.5996154808376,30.5987757548883,
31.597936028939,32.5970963029897,33.5962565770404,34.5575191894887),
 .UNSPECIFIED.);
#3207=B_SPLINE_CURVE_WITH_KNOTS('',3,(#75867,#75868,#75869,#75870,#75871,
#75872,#75873,#75874,#75875,#75876,#75877),.UNSPECIFIED.,.F.,.F.,(4,1,1,
1,1,1,1,1,4),(28.2743338823092,28.2785910376542,29.2777513117049,30.2769115857556,
31.2760718598062,32.2752321338569,33.2743924079076,34.2735526819583,34.5575191894888),
 .UNSPECIFIED.);
#3208=B_SPLINE_CURVE_WITH_KNOTS('',3,(#75882,#75883,#75884,#75885,#75886,
#75887,#75888,#75889,#75890,#75891),.UNSPECIFIED.,.F.,.F.,(4,1,1,1,1,1,
1,4),(21.9911485751295,22.6054935624829,23.6046538365335,24.6038141105842,
25.6029743846349,26.6021346586856,27.6012949327363,28.2743338823091),
 .UNSPECIFIED.);
#3209=B_SPLINE_CURVE_WITH_KNOTS('',3,(#75892,#75893,#75894,#75895,#75896,
#75897,#75898,#75899,#75900,#75901),.UNSPECIFIED.,.F.,.F.,(4,1,1,1,1,1,
1,4),(21.9911485751297,22.2836293933501,23.2827896674008,24.2819499414514,
25.2811102155021,26.2802704895528,27.2794307636035,28.2743338823092),
 .UNSPECIFIED.);
#3210=B_SPLINE_CURVE_WITH_KNOTS('',3,(#75906,#75907,#75908,#75909,#75910,
#75911,#75912,#75913,#75914,#75915),.UNSPECIFIED.,.F.,.F.,(4,1,1,1,1,1,
1,4),(15.70796326795,16.6105319181787,17.6096921922294,18.6088524662801,
19.6080127403308,20.6071730143815,21.6063332884322,21.9911485751295),
 .UNSPECIFIED.);
#3211=B_SPLINE_CURVE_WITH_KNOTS('',3,(#75916,#75917,#75918,#75919,#75920,
#75921,#75922,#75923,#75924,#75925),.UNSPECIFIED.,.F.,.F.,(4,1,1,1,1,1,
1,4),(15.7079632679501,16.288667749046,17.2878280230966,18.2869882971473,
19.286148571198,20.2853088452487,21.2844691192994,21.9911485751297),
 .UNSPECIFIED.);
#3212=B_SPLINE_CURVE_WITH_KNOTS('',3,(#75928,#75929,#75930,#75931,#75932,
#75933,#75934,#75935,#75936,#75937,#75938,#75939,#75940,#75941,#75942,#75943,
#75944,#75945,#75946,#75947,#75948,#75949,#75950,#75951,#75952,#75953,#75954,
#75955,#75956,#75957,#75958,#75959,#75960,#75961,#75962,#75963,#75964,#75965,
#75966,#75967,#75968,#75969,#75970,#75971,#75972,#75973,#75974,#75975,#75976,
#75977,#75978,#75979,#75980,#75981,#75982,#75983,#75984,#75985,#75986,#75987,
#75988,#75989,#75990,#75991,#75992,#75993,#75994,#75995,#75996,#75997,#75998,
#75999,#76000,#76001,#76002,#76003,#76004,#76005,#76006,#76007,#76008,#76009,
#76010,#76011,#76012,#76013,#76014,#76015,#76016,#76017,#76018,#76019,#76020,
#76021,#76022,#76023,#76024,#76025,#76026,#76027,#76028,#76029,#76030,#76031,
#76032,#76033),.UNSPECIFIED.,.F.,.F.,(4,3,3,3,3,3,3,3,3,3,3,3,3,3,3,3,3,
3,3,3,3,3,3,3,3,3,3,3,3,3,3,3,3,3,3,4),(-0.990745149397272,-0.953116208297139,
-0.912523111179552,-0.885921211171593,-0.874931108620643,-0.86587654099025,
-0.824728242628866,-0.782498801181784,-0.764023420548686,-0.749177983835952,
-0.743080509582649,-0.700694026797518,-0.657915923258967,-0.615160120207279,
-0.583093267918513,-0.569303123526439,-0.56234430900736,-0.519192848994169,
-0.486892711052215,-0.444701478410969,-0.401945206516134,-0.389788368451242,
-0.382758910740908,-0.376896545121776,-0.334227892709294,-0.290071518416692,
-0.245915144124089,-0.215175751108578,-0.20168695137348,-0.194154816283721,
-0.188100426560717,-0.144404214510165,-0.100314778095157,-0.0563889878319668,
-0.0131683088431834,0.),.UNSPECIFIED.);
#3213=B_SPLINE_CURVE_WITH_KNOTS('',3,(#76038,#76039,#76040,#76041,#76042,
#76043,#76044,#76045,#76046,#76047,#76048,#76049,#76050,#76051,#76052,#76053,
#76054,#76055,#76056,#76057,#76058,#76059,#76060,#76061,#76062,#76063,#76064,
#76065,#76066,#76067,#76068,#76069,#76070,#76071,#76072,#76073,#76074,#76075,
#76076,#76077,#76078,#76079,#76080,#76081,#76082,#76083,#76084,#76085,#76086,
#76087,#76088,#76089,#76090,#76091,#76092,#76093,#76094,#76095,#76096,#76097,
#76098,#76099,#76100,#76101,#76102,#76103,#76104,#76105,#76106,#76107,#76108,
#76109,#76110,#76111,#76112,#76113,#76114,#76115,#76116,#76117,#76118,#76119,
#76120,#76121,#76122,#76123,#76124,#76125,#76126,#76127,#76128,#76129,#76130,
#76131,#76132,#76133,#76134,#76135,#76136,#76137,#76138,#76139,#76140,#76141,
#76142,#76143,#76144,#76145,#76146),.UNSPECIFIED.,.F.,.F.,(4,3,3,3,3,3,
3,3,3,3,3,3,3,3,3,3,3,3,3,3,3,3,3,3,3,3,3,3,3,3,3,3,3,3,3,3,4),(-0.988861763753148,
-0.947944861719371,-0.904266293393393,-0.876752649619069,-0.860521193082487,
-0.854366172475187,-0.810876688531655,-0.767523101590724,-0.747924850769826,
-0.737059406202786,-0.730926332354279,-0.724875966528802,-0.681346469766453,
-0.637840230036599,-0.594392170778502,-0.561806126334929,-0.548626870943788,
-0.543243028328661,-0.500823502880395,-0.46404799300421,-0.421566751277432,
-0.378898569390552,-0.365114758790781,-0.359674607894455,-0.353937374020393,
-0.31200686520388,-0.269901000253992,-0.229433896916033,-0.200754659801529,
-0.187320188163563,-0.179359914434182,-0.174478120366766,-0.130858590275074,
-0.0893323551625696,-0.0481739323171706,-0.00783840924613729,0.),
 .UNSPECIFIED.);
#3214=B_SPLINE_CURVE_WITH_KNOTS('',3,(#78059,#78060,#78061,#78062,#78063,
#78064,#78065,#78066,#78067,#78068,#78069,#78070,#78071,#78072,#78073,#78074),
 .UNSPECIFIED.,.F.,.F.,(4,3,3,3,3,4),(466.085105135419,466.60784798167,
467.607008255721,468.606168529772,469.605328803822,470.521777155409),
 .UNSPECIFIED.);
#3215=B_SPLINE_CURVE_WITH_KNOTS('',3,(#78076,#78077,#78078,#78079,#78080,
#78081,#78082,#78083,#78084,#78085,#78086,#78087,#78088,#78089,#78090,#78091,
#78092,#78093,#78094,#78095,#78096,#78097,#78098,#78099,#78100,#78101,#78102,
#78103,#78104,#78105,#78106,#78107,#78108,#78109,#78110,#78111,#78112,#78113,
#78114,#78115,#78116,#78117,#78118,#78119,#78120,#78121,#78122,#78123,#78124,
#78125,#78126,#78127,#78128,#78129,#78130,#78131,#78132,#78133,#78134,#78135,
#78136,#78137,#78138,#78139,#78140,#78141,#78142,#78143,#78144,#78145,#78146,
#78147,#78148,#78149,#78150,#78151,#78152,#78153,#78154,#78155,#78156,#78157,
#78158,#78159,#78160,#78161,#78162,#78163,#78164,#78165,#78166,#78167,#78168,
#78169,#78170,#78171,#78172,#78173,#78174,#78175,#78176,#78177,#78178,#78179,
#78180,#78181),.UNSPECIFIED.,.F.,.F.,(4,3,3,3,3,3,3,3,3,3,3,3,3,3,3,3,3,
3,3,3,3,3,3,3,3,3,3,3,3,3,3,3,3,3,3,4),(-0.990745149397179,-0.953116208297015,
-0.912523118726293,-0.885921218246659,-0.87493112265529,-0.865876539744951,
-0.824728248358261,-0.782498806194998,-0.76402342524857,-0.749177977734278,
-0.743080507741458,-0.700694026269302,-0.657915914033916,-0.615160113288475,
-0.583093262729394,-0.569303115883233,-0.562344307517487,-0.519192825285289,
-0.486892711052151,-0.444701445163227,-0.401945182425889,-0.389788318046496,
-0.382757232744068,-0.376896437396706,-0.334227749510469,-0.290071446817269,
-0.24591514412407,-0.215175751108561,-0.201686951004493,-0.194154818601853,
-0.188100426670343,-0.144404320209132,-0.100314907674269,-0.0563891000384953,
-0.0131683692741428,0.),.UNSPECIFIED.);
#3216=B_SPLINE_CURVE_WITH_KNOTS('',3,(#78182,#78183,#78184,#78185,#78186,
#78187,#78188,#78189,#78190),.UNSPECIFIED.,.F.,.F.,(4,1,1,1,1,1,4),(10.3764180272052,
11.2928663787925,12.2920266528432,13.2911869268939,14.2903472009446,15.2895074749953,
15.7079632679501),.UNSPECIFIED.);
#3217=B_SPLINE_CURVE_WITH_KNOTS('',3,(#78196,#78197,#78198,#78199,#78200,
#78201,#78202,#78203,#78204,#78205,#78206,#78207,#78208,#78209,#78210,#78211,
#78212,#78213,#78214,#78215,#78216,#78217,#78218,#78219,#78220,#78221,#78222,
#78223,#78224,#78225,#78226,#78227,#78228,#78229,#78230,#78231,#78232,#78233,
#78234,#78235,#78236,#78237,#78238,#78239,#78240,#78241,#78242,#78243,#78244,
#78245,#78246,#78247,#78248,#78249,#78250,#78251,#78252,#78253,#78254,#78255,
#78256,#78257,#78258,#78259,#78260,#78261,#78262,#78263,#78264,#78265,#78266,
#78267,#78268,#78269,#78270,#78271,#78272,#78273,#78274,#78275,#78276,#78277,
#78278,#78279,#78280,#78281,#78282,#78283,#78284,#78285,#78286,#78287,#78288,
#78289,#78290,#78291,#78292,#78293,#78294,#78295,#78296,#78297,#78298,#78299,
#78300,#78301,#78302,#78303,#78304),.UNSPECIFIED.,.F.,.F.,(4,3,3,3,3,3,
3,3,3,3,3,3,3,3,3,3,3,3,3,3,3,3,3,3,3,3,3,3,3,3,3,3,3,3,3,3,4),(-0.988861763753244,
-0.947944861719434,-0.904266288020023,-0.876752644581534,-0.860521185641252,
-0.854366163559061,-0.810876676220037,-0.767523090818058,-0.747924853089199,
-0.737059410276204,-0.730926341162295,-0.724875968929562,-0.681346480687655,
-0.637840262092946,-0.59439219482076,-0.56180614436662,-0.54862689554501,
-0.543243028959436,-0.500823535537494,-0.4640479930042,-0.4215667470188,
-0.378898519968392,-0.365114586359317,-0.359674094222405,-0.353937304897961,
-0.312006788845363,-0.269900865492287,-0.229433896916071,-0.200754659801562,
-0.187320188967778,-0.179359911830878,-0.17447811560387,-0.130858586702903,
-0.0893323660352711,-0.0481739755722922,-0.00783848836599452,0.),
 .UNSPECIFIED.);
#3218=B_SPLINE_CURVE_WITH_KNOTS('',3,(#78307,#78308,#78309,#78310,#78311,
#78312,#78313,#78314,#78315),.UNSPECIFIED.,.F.,.F.,(4,1,1,1,1,1,4),(11.6147305479253,
12.1143106849507,12.613890821976,13.6130510960267,14.6122113700774,15.6113716441281,
15.70796326795),.UNSPECIFIED.);
#3219=B_SPLINE_CURVE_WITH_KNOTS('',3,(#80228,#80229,#80230,#80231,#80232,
#80233,#80234,#80235,#80236,#80237,#80238,#80239,#80240,#80241,#80242,#80243),
 .UNSPECIFIED.,.F.,.F.,(4,3,3,3,3,4),(-472.602809625974,-472.103229488949,
-471.603649351923,-470.604489077873,-469.605328803822,-469.048945451313),
 .UNSPECIFIED.);
#3220=B_SPLINE_CURVE_WITH_KNOTS('',3,(#80296,#80297,#80298,#80299,#80300,
#80301),.UNSPECIFIED.,.F.,.F.,(4,2,4),(0.300223039487565,0.349769627099692,
0.370274237441758),.UNSPECIFIED.);
#3221=B_SPLINE_CURVE_WITH_KNOTS('',3,(#80304,#80305,#80306,#80307,#80308,
#80309),.UNSPECIFIED.,.F.,.F.,(4,2,4),(0.128903119732732,0.149407730074798,
0.198954317686925),.UNSPECIFIED.);
#3222=B_SPLINE_CURVE_WITH_KNOTS('',3,(#80326,#80327,#80328,#80329,#80330,
#80331),.UNSPECIFIED.,.F.,.F.,(4,2,4),(0.128903119732731,0.149407730074798,
0.198954317686925),.UNSPECIFIED.);
#3223=B_SPLINE_CURVE_WITH_KNOTS('',3,(#80461,#80462,#80463,#80464,#80465,
#80466),.UNSPECIFIED.,.F.,.F.,(4,2,4),(0.300223039487565,0.349769627099692,
0.370274237441758),.UNSPECIFIED.);
#3224=B_SPLINE_CURVE_WITH_KNOTS('',3,(#80479,#80480,#80481,#80482,#80483,
#80484),.UNSPECIFIED.,.F.,.F.,(4,2,4),(0.128903119732732,0.149407730074798,
0.198954317686925),.UNSPECIFIED.);
#3225=B_SPLINE_CURVE_WITH_KNOTS('',3,(#80496,#80497,#80498,#80499,#80500,
#80501),.UNSPECIFIED.,.F.,.F.,(4,2,4),(0.300223039487565,0.349769627099692,
0.370274237441758),.UNSPECIFIED.);
#3226=B_SPLINE_CURVE_WITH_KNOTS('',3,(#80514,#80515,#80516,#80517,#80518,
#80519),.UNSPECIFIED.,.F.,.F.,(4,2,4),(0.128903119732732,0.149407730074798,
0.198954317686925),.UNSPECIFIED.);
#3227=B_SPLINE_CURVE_WITH_KNOTS('',3,(#80531,#80532,#80533,#80534,#80535,
#80536),.UNSPECIFIED.,.F.,.F.,(4,2,4),(0.300223039487565,0.349769627099692,
0.370274237441758),.UNSPECIFIED.);
#3228=B_SPLINE_CURVE_WITH_KNOTS('',3,(#80549,#80550,#80551,#80552,#80553,
#80554),.UNSPECIFIED.,.F.,.F.,(4,2,4),(0.128903119732731,0.149407730074798,
0.198954317686925),.UNSPECIFIED.);
#3229=B_SPLINE_CURVE_WITH_KNOTS('',3,(#80566,#80567,#80568,#80569,#80570,
#80571),.UNSPECIFIED.,.F.,.F.,(4,2,4),(0.300223039487565,0.349769627099692,
0.370274237441758),.UNSPECIFIED.);
#3230=B_SPLINE_CURVE_WITH_KNOTS('',3,(#80584,#80585,#80586,#80587,#80588,
#80589),.UNSPECIFIED.,.F.,.F.,(4,2,4),(0.128903119732732,0.149407730074798,
0.198954317686925),.UNSPECIFIED.);
#3231=B_SPLINE_CURVE_WITH_KNOTS('',3,(#80601,#80602,#80603,#80604,#80605,
#80606),.UNSPECIFIED.,.F.,.F.,(4,2,4),(0.300223039487565,0.349769627099692,
0.370274237441759),.UNSPECIFIED.);
#3232=B_SPLINE_CURVE_WITH_KNOTS('',3,(#80619,#80620,#80621,#80622,#80623,
#80624),.UNSPECIFIED.,.F.,.F.,(4,2,4),(0.128903119732732,0.149407730074798,
0.198954317686923),.UNSPECIFIED.);
#3233=B_SPLINE_CURVE_WITH_KNOTS('',3,(#80636,#80637,#80638,#80639,#80640,
#80641),.UNSPECIFIED.,.F.,.F.,(4,2,4),(0.300223039487567,0.349769627099692,
0.370274237441759),.UNSPECIFIED.);
#3234=B_SPLINE_CURVE_WITH_KNOTS('',3,(#80654,#80655,#80656,#80657,#80658,
#80659),.UNSPECIFIED.,.F.,.F.,(4,2,4),(0.128903119732731,0.149407730074798,
0.198954317686924),.UNSPECIFIED.);
#3235=B_SPLINE_CURVE_WITH_KNOTS('',3,(#80671,#80672,#80673,#80674,#80675,
#80676),.UNSPECIFIED.,.F.,.F.,(4,2,4),(0.300223039487565,0.349769627099692,
0.370274237441758),.UNSPECIFIED.);
#3236=B_SPLINE_CURVE_WITH_KNOTS('',3,(#80689,#80690,#80691,#80692,#80693,
#80694),.UNSPECIFIED.,.F.,.F.,(4,2,4),(0.128903119732731,0.149407730074798,
0.198954317686925),.UNSPECIFIED.);
#3237=B_SPLINE_CURVE_WITH_KNOTS('',3,(#80706,#80707,#80708,#80709,#80710,
#80711),.UNSPECIFIED.,.F.,.F.,(4,2,4),(0.300223039487565,0.349769627099692,
0.370274237441758),.UNSPECIFIED.);
#3238=B_SPLINE_CURVE_WITH_KNOTS('',3,(#80724,#80725,#80726,#80727,#80728,
#80729),.UNSPECIFIED.,.F.,.F.,(4,2,4),(0.128903119732732,0.149407730074798,
0.198954317686924),.UNSPECIFIED.);
#3239=B_SPLINE_CURVE_WITH_KNOTS('',3,(#80741,#80742,#80743,#80744,#80745,
#80746),.UNSPECIFIED.,.F.,.F.,(4,2,4),(0.300223039487566,0.349769627099693,
0.370274237441759),.UNSPECIFIED.);
#3240=B_SPLINE_CURVE_WITH_KNOTS('',3,(#80759,#80760,#80761,#80762,#80763,
#80764),.UNSPECIFIED.,.F.,.F.,(4,2,4),(0.128903119732732,0.149407730074798,
0.198954317686925),.UNSPECIFIED.);
#3241=B_SPLINE_CURVE_WITH_KNOTS('',3,(#80776,#80777,#80778,#80779,#80780,
#80781),.UNSPECIFIED.,.F.,.F.,(4,2,4),(0.300223039487566,0.349769627099693,
0.370274237441759),.UNSPECIFIED.);
#3242=B_SPLINE_CURVE_WITH_KNOTS('',3,(#80794,#80795,#80796,#80797,#80798,
#80799),.UNSPECIFIED.,.F.,.F.,(4,2,4),(0.128903119732731,0.149407730074797,
0.198954317686924),.UNSPECIFIED.);
#3243=B_SPLINE_CURVE_WITH_KNOTS('',3,(#80811,#80812,#80813,#80814,#80815,
#80816),.UNSPECIFIED.,.F.,.F.,(4,2,4),(0.300223039487565,0.349769627099692,
0.370274237441758),.UNSPECIFIED.);
#3244=B_SPLINE_CURVE_WITH_KNOTS('',3,(#80829,#80830,#80831,#80832,#80833,
#80834),.UNSPECIFIED.,.F.,.F.,(4,2,4),(0.128903119732732,0.149407730074798,
0.198954317686925),.UNSPECIFIED.);
#3245=B_SPLINE_CURVE_WITH_KNOTS('',3,(#80846,#80847,#80848,#80849,#80850,
#80851),.UNSPECIFIED.,.F.,.F.,(4,2,4),(0.300223039487565,0.349769627099692,
0.370274237441758),.UNSPECIFIED.);
#3246=B_SPLINE_CURVE_WITH_KNOTS('',3,(#80864,#80865,#80866,#80867,#80868,
#80869),.UNSPECIFIED.,.F.,.F.,(4,2,4),(0.128903119732731,0.149407730074798,
0.198954317686925),.UNSPECIFIED.);
#3247=B_SPLINE_CURVE_WITH_KNOTS('',3,(#80881,#80882,#80883,#80884,#80885,
#80886),.UNSPECIFIED.,.F.,.F.,(4,2,4),(0.300223039487565,0.349769627099692,
0.370274237441758),.UNSPECIFIED.);
#3248=B_SPLINE_CURVE_WITH_KNOTS('',3,(#80899,#80900,#80901,#80902,#80903,
#80904),.UNSPECIFIED.,.F.,.F.,(4,2,4),(0.128903119732731,0.149407730074798,
0.198954317686925),.UNSPECIFIED.);
#3249=B_SPLINE_CURVE_WITH_KNOTS('',3,(#80916,#80917,#80918,#80919,#80920,
#80921),.UNSPECIFIED.,.F.,.F.,(4,2,4),(0.300223039487565,0.349769627099692,
0.370274237441759),.UNSPECIFIED.);
#3250=B_SPLINE_CURVE_WITH_KNOTS('',3,(#81027,#81028,#81029,#81030,#81031,
#81032,#81033,#81034,#81035,#81036),.UNSPECIFIED.,.F.,.F.,(4,3,3,4),(-4.09202352044853,
-3.98465656589411,-2.98849242442058,-2.07317267331971),.UNSPECIFIED.);
#3251=B_SPLINE_CURVE_WITH_KNOTS('',3,(#81039,#81040,#81041,#81042,#81043,
#81044,#81045),.UNSPECIFIED.,.F.,.F.,(4,3,4),(0.,0.99616414147353,1.12274180646097),
 .UNSPECIFIED.);
#3252=B_SPLINE_CURVE_WITH_KNOTS('',3,(#81050,#81051,#81052,#81053,#81054,
#81055,#81056,#81057,#81058,#81059,#81060,#81061,#81062,#81063,#81064,#81065,
#81066,#81067,#81068,#81069,#81070,#81071),.UNSPECIFIED.,.F.,.F.,(4,3,3,
3,3,3,3,4),(-10.3752088276281,-9.96164141473529,-8.96547727326176,-7.96931313178823,
-6.9731489903147,-5.97698484884117,-4.98082070736764,-4.09202352044853),
 .UNSPECIFIED.);
#3253=B_SPLINE_CURVE_WITH_KNOTS('',3,(#81072,#81073,#81074,#81075,#81076,
#81077,#81078,#81079,#81080,#81081,#81082,#81083,#81084,#81085,#81086,#81087,
#81088,#81089,#81090,#81091,#81092,#81093),.UNSPECIFIED.,.F.,.F.,(4,3,3,
3,3,3,3,4),(1.12274180646097,1.99232828294706,2.98849242442059,3.98465656589411,
4.98082070736764,5.97698484884117,6.9731489903147,7.40592711364056),
 .UNSPECIFIED.);
#3254=B_SPLINE_CURVE_WITH_KNOTS('',3,(#81098,#81099,#81100,#81101,#81102,
#81103,#81104,#81105,#81106,#81107,#81108,#81109,#81110,#81111,#81112,#81113,
#81114,#81115,#81116,#81117,#81118,#81119),.UNSPECIFIED.,.F.,.F.,(4,3,3,
3,3,3,3,4),(-16.6583941348077,-15.9386262635765,-14.9424621221029,-13.9462979806294,
-12.9501338391559,-11.9539696976823,-10.9578055562088,-10.3752088276281),
 .UNSPECIFIED.);
#3255=B_SPLINE_CURVE_WITH_KNOTS('',3,(#81120,#81121,#81122,#81123,#81124,
#81125,#81126,#81127,#81128,#81129,#81130,#81131,#81132,#81133,#81134,#81135,
#81136,#81137,#81138,#81139,#81140,#81141),.UNSPECIFIED.,.F.,.F.,(4,3,3,
3,3,3,3,4),(7.40592711364056,7.96931313178823,8.96547727326176,9.96164141473529,
10.9578055562088,11.9539696976823,12.9501338391559,13.6891124208201),
 .UNSPECIFIED.);
#3256=B_SPLINE_CURVE_WITH_KNOTS('',3,(#81146,#81147,#81148,#81149,#81150,
#81151,#81152,#81153,#81154,#81155,#81156,#81157,#81158,#81159,#81160,#81161,
#81162,#81163,#81164,#81165,#81166,#81167,#81168,#81169,#81170),
 .UNSPECIFIED.,.F.,.F.,(4,3,3,3,3,3,3,3,4),(-22.9415794419873,-22.9117752538912,
-21.9156111124176,-20.9194469709441,-19.9232828294706,-18.927118687997,
-17.9309545465235,-16.93479040505,-16.6583941348077),.UNSPECIFIED.);
#3257=B_SPLINE_CURVE_WITH_KNOTS('',3,(#81171,#81172,#81173,#81174,#81175,
#81176,#81177,#81178,#81179,#81180,#81181,#81182,#81183,#81184,#81185,#81186,
#81187,#81188,#81189,#81190,#81191,#81192,#81193,#81194,#81195),
 .UNSPECIFIED.,.F.,.F.,(4,3,3,3,3,3,3,3,4),(13.6891124208201,13.9462979806294,
14.9424621221029,15.9386262635765,16.93479040505,17.9309545465235,18.927118687997,
19.9232828294706,19.9722977279997),.UNSPECIFIED.);
#3258=B_SPLINE_CURVE_WITH_KNOTS('',3,(#81200,#81201,#81202,#81203,#81204,
#81205,#81206,#81207,#81208,#81209,#81210,#81211,#81212,#81213,#81214,#81215,
#81216,#81217,#81218,#81219,#81220,#81221),.UNSPECIFIED.,.F.,.F.,(4,3,3,
3,3,3,3,4),(-29.2247647491669,-28.8887601027323,-27.8925959612588,-26.8964318197853,
-25.9002676783117,-24.9041035368382,-23.9079393953647,-22.9415794419873),
 .UNSPECIFIED.);
#3259=B_SPLINE_CURVE_WITH_KNOTS('',3,(#81222,#81223,#81224,#81225,#81226,
#81227,#81228,#81229,#81230,#81231,#81232,#81233,#81234,#81235,#81236,#81237,
#81238,#81239,#81240,#81241,#81242,#81243),.UNSPECIFIED.,.F.,.F.,(4,3,3,
3,3,3,3,4),(19.9722977279997,20.9194469709441,21.9156111124176,22.9117752538912,
23.9079393953647,24.9041035368382,25.9002676783117,26.2554830351793),
 .UNSPECIFIED.);
#3260=B_SPLINE_CURVE_WITH_KNOTS('',3,(#81248,#81249,#81250,#81251,#81252,
#81253,#81254,#81255,#81256,#81257,#81258,#81259,#81260,#81261,#81262,#81263,
#81264,#81265,#81266,#81267,#81268,#81269),.UNSPECIFIED.,.F.,.F.,(4,3,3,
3,3,3,3,4),(-35.5079500563465,-34.8657449515735,-33.8695808101,-32.8734166686264,
-31.8772525271529,-30.8810883856794,-29.8849242442059,-29.2247647491669),
 .UNSPECIFIED.);
#3261=B_SPLINE_CURVE_WITH_KNOTS('',3,(#81270,#81271,#81272,#81273,#81274,
#81275,#81276,#81277,#81278,#81279,#81280,#81281,#81282,#81283,#81284,#81285,
#81286,#81287,#81288,#81289,#81290,#81291),.UNSPECIFIED.,.F.,.F.,(4,3,3,
3,3,3,3,4),(26.2554830351793,26.8964318197853,27.8925959612588,28.8887601027323,
29.8849242442059,30.8810883856794,31.8772525271529,32.5386683423589),
 .UNSPECIFIED.);
#3262=B_SPLINE_CURVE_WITH_KNOTS('',3,(#81296,#81297,#81298,#81299,#81300,
#81301,#81302,#81303,#81304,#81305,#81306,#81307,#81308,#81309,#81310,#81311,
#81312,#81313,#81314,#81315,#81316,#81317),.UNSPECIFIED.,.F.,.F.,(4,3,3,
3,3,3,3,4),(-41.791135363526,-40.8427298004147,-39.8465656589411,-38.8504015174676,
-37.8542373759941,-36.8580732345206,-35.861909093047,-35.5079500563465),
 .UNSPECIFIED.);
#3263=B_SPLINE_CURVE_WITH_KNOTS('',3,(#81318,#81319,#81320,#81321,#81322,
#81323,#81324,#81325,#81326,#81327,#81328,#81329,#81330,#81331,#81332,#81333,
#81334,#81335,#81336,#81337,#81338,#81339),.UNSPECIFIED.,.F.,.F.,(4,3,3,
3,3,3,3,4),(32.5386683423589,32.8734166686265,33.8695808101,34.8657449515735,
35.861909093047,36.8580732345206,37.8542373759941,38.8218536495385),
 .UNSPECIFIED.);
#3264=B_SPLINE_CURVE_WITH_KNOTS('',3,(#81345,#81346,#81347,#81348,#81349,
#81350,#81351,#81352,#81353,#81354),.UNSPECIFIED.,.F.,.F.,(4,1,1,1,1,1,
1,4),(47.1238898038469,47.4778488405475,48.474012982021,49.4701771234945,
50.466341264968,51.4625054064416,52.4586695479151,53.373989299016),
 .UNSPECIFIED.);
#3265=B_SPLINE_CURVE_WITH_KNOTS('',3,(#81357,#81358,#81359,#81360,#81361,
#81362,#81363,#81364,#81365),.UNSPECIFIED.,.F.,.F.,(4,1,1,1,1,1,4),(47.1238898038469,
47.152437671776,48.1486018132495,49.1447659547231,50.1409300961966,51.1370942376701,
52.1332583791436),.UNSPECIFIED.);
#3266=B_SPLINE_CURVE_WITH_KNOTS('',3,(#81370,#81371,#81372,#81373,#81374,
#81375,#81376,#81377,#81378,#81379),.UNSPECIFIED.,.F.,.F.,(4,1,1,1,1,1,
1,4),(40.8407044966673,41.5008639917063,42.4970281331798,43.4931922746533,
44.4893564161269,45.4855205576004,46.4816846990739,47.1238898038469),
 .UNSPECIFIED.);
#3267=B_SPLINE_CURVE_WITH_KNOTS('',3,(#81380,#81381,#81382,#81383,#81384,
#81385,#81386,#81387,#81388,#81389),.UNSPECIFIED.,.F.,.F.,(4,1,1,1,1,1,
1,4),(40.8407044966673,41.1754528229348,42.1716169644084,43.1677811058819,
44.1639452473554,45.1601093888289,46.1562735303025,47.1238898038469),
 .UNSPECIFIED.);
#3268=B_SPLINE_CURVE_WITH_KNOTS('',3,(#81394,#81395,#81396,#81397,#81398,
#81399,#81400,#81401,#81402,#81403),.UNSPECIFIED.,.F.,.F.,(4,1,1,1,1,1,
1,4),(34.5575191894877,35.5238791428651,36.5200432843386,37.5162074258122,
38.5123715672857,39.5085357087592,40.5046998502328,40.8407044966673),
 .UNSPECIFIED.);
#3269=B_SPLINE_CURVE_WITH_KNOTS('',3,(#81404,#81405,#81406,#81407,#81408,
#81409,#81410,#81411,#81412,#81413),.UNSPECIFIED.,.F.,.F.,(4,1,1,1,1,1,
1,4),(34.5575191894877,35.1984679740937,36.1946321155672,37.1907962570407,
38.1869603985142,39.1831245399878,40.1792886814613,40.8407044966673),
 .UNSPECIFIED.);
#3270=B_SPLINE_CURVE_WITH_KNOTS('',3,(#81418,#81419,#81420,#81421,#81422,
#81423,#81424,#81425,#81426,#81427,#81428),.UNSPECIFIED.,.F.,.F.,(4,1,1,
1,1,1,1,1,4),(28.2743338823081,28.5507301525504,29.5468942940239,30.5430584354975,
31.539222576971,32.5353867184445,33.531550859918,34.5277150013916,34.5575191894877),
 .UNSPECIFIED.);
#3271=B_SPLINE_CURVE_WITH_KNOTS('',3,(#81429,#81430,#81431,#81432,#81433,
#81434,#81435,#81436,#81437,#81438),.UNSPECIFIED.,.F.,.F.,(4,1,1,1,1,1,
1,4),(28.2743338823081,29.2214831252525,30.217647266726,31.2138114081995,
32.2099755496731,33.2061396911466,34.2023038326201,34.5575191894877),
 .UNSPECIFIED.);
#3272=B_SPLINE_CURVE_WITH_KNOTS('',3,(#81443,#81444,#81445,#81446,#81447,
#81448,#81449,#81450,#81451,#81452),.UNSPECIFIED.,.F.,.F.,(4,1,1,1,1,1,
1,4),(21.9911485751285,22.5737453037092,23.5699094451828,24.5660735866563,
25.5622377281298,26.5584018696034,27.5545660110769,28.2743338823081),
 .UNSPECIFIED.);
#3273=B_SPLINE_CURVE_WITH_KNOTS('',3,(#81453,#81454,#81455,#81456,#81457,
#81458,#81459,#81460,#81461,#81462,#81463),.UNSPECIFIED.,.F.,.F.,(4,1,1,
1,1,1,1,1,4),(21.9911485751285,22.2483341349378,23.2444982764113,24.2406624178848,
25.2368265593584,26.2329907008319,27.2291548423054,28.225318983779,28.2743338823081),
 .UNSPECIFIED.);
#3274=B_SPLINE_CURVE_WITH_KNOTS('',3,(#81468,#81469,#81470,#81471,#81472,
#81473,#81474,#81475,#81476,#81477),.UNSPECIFIED.,.F.,.F.,(4,1,1,1,1,1,
1,4),(15.707963267949,16.5967604548681,17.5929245963416,18.5890887378151,
19.5852528792886,20.5814170207622,21.5775811622357,21.9911485751285),
 .UNSPECIFIED.);
#3275=B_SPLINE_CURVE_WITH_KNOTS('',3,(#81478,#81479,#81480,#81481,#81482,
#81483,#81484,#81485,#81486,#81487),.UNSPECIFIED.,.F.,.F.,(4,1,1,1,1,1,
1,4),(15.7079632679489,16.2713492860966,17.2675134275701,18.2636775690437,
19.2598417105172,20.2560058519907,21.2521699934642,21.9911485751285),
 .UNSPECIFIED.);
#3276=B_SPLINE_CURVE_WITH_KNOTS('',3,(#81490,#81491,#81492,#81493,#81494,
#81495,#81496,#81497,#81498,#81499,#81500,#81501,#81502,#81503,#81504,#81505,
#81506,#81507,#81508,#81509,#81510,#81511,#81512,#81513,#81514,#81515,#81516,
#81517,#81518,#81519,#81520,#81521,#81522,#81523,#81524,#81525,#81526,#81527,
#81528,#81529,#81530,#81531,#81532,#81533,#81534,#81535,#81536,#81537,#81538,
#81539,#81540,#81541,#81542,#81543,#81544,#81545,#81546,#81547,#81548,#81549,
#81550,#81551,#81552,#81553,#81554,#81555,#81556,#81557,#81558,#81559,#81560,
#81561,#81562,#81563,#81564,#81565,#81566,#81567,#81568,#81569,#81570,#81571,
#81572,#81573,#81574),.UNSPECIFIED.,.F.,.F.,(4,3,3,3,3,3,3,3,3,3,3,3,3,
3,3,3,3,3,3,3,3,3,3,3,3,3,3,3,4),(-0.276631791712725,-0.266952028164814,
-0.252323120380107,-0.245291696267628,-0.242250024468316,-0.226984993323628,
-0.216140129019276,-0.211926830943687,-0.208887036385599,-0.193126552069373,
-0.177076639522004,-0.167863999363706,-0.162681055949887,-0.159693750396033,
-0.143166615227965,-0.140226078888815,-0.124274134827967,-0.116088608730203,
-0.111105706457781,-0.107817001525543,-0.0912655983034208,-0.0743533570119642,
-0.0648492915702117,-0.0586243521231257,-0.055485434306559,-0.0380411261163856,
-0.0205521325003434,-0.00346624990959772,0.),.UNSPECIFIED.);
#3277=B_SPLINE_CURVE_WITH_KNOTS('',3,(#81579,#81580,#81581,#81582,#81583,
#81584,#81585,#81586,#81587,#81588,#81589,#81590,#81591,#81592,#81593,#81594,
#81595,#81596,#81597,#81598,#81599,#81600,#81601,#81602,#81603,#81604,#81605,
#81606,#81607,#81608,#81609,#81610,#81611,#81612,#81613,#81614,#81615,#81616,
#81617,#81618,#81619,#81620,#81621,#81622,#81623,#81624,#81625,#81626,#81627,
#81628,#81629,#81630,#81631,#81632,#81633,#81634,#81635,#81636,#81637,#81638,
#81639,#81640,#81641,#81642,#81643,#81644,#81645,#81646,#81647,#81648,#81649,
#81650,#81651,#81652,#81653,#81654,#81655,#81656,#81657,#81658,#81659,#81660,
#81661,#81662,#81663),.UNSPECIFIED.,.F.,.F.,(4,3,3,3,3,3,3,3,3,3,3,3,3,
3,3,3,3,3,3,3,3,3,3,3,3,3,3,3,4),(-0.275362278356886,-0.263558129214759,
-0.246259601438028,-0.240454824668648,-0.236894340710815,-0.233127676432609,
-0.215926618879135,-0.204582029894356,-0.20054686414582,-0.196717291630079,
-0.179965358204731,-0.163633434810385,-0.154017552858015,-0.14710518062374,
-0.144181207184443,-0.128328561127056,-0.125169907000906,-0.10816649509411,
-0.10086959066255,-0.0956369517540662,-0.0926001968852286,-0.0768321091103029,
-0.0611424409132595,-0.0532927242788775,-0.0475055755195517,-0.0447074663570426,
-0.0295993711118811,-0.0147996855559406,0.),.UNSPECIFIED.);
#3278=B_SPLINE_CURVE_WITH_KNOTS('',3,(#81852,#81853,#81854,#81855,#81856,
#81857,#81858,#81859,#81860,#81861,#81862,#81863,#81864),.UNSPECIFIED.,
 .F.,.F.,(4,3,3,3,4),(38.8218536495385,38.8504015174676,39.8465656589411,
40.8427298004147,41.7580495515155),.UNSPECIFIED.);
#3279=B_SPLINE_CURVE_WITH_KNOTS('',3,(#81866,#81867,#81868,#81869,#81870,
#81871,#81872,#81873,#81874,#81875,#81876,#81877,#81878,#81879,#81880,#81881,
#81882,#81883,#81884,#81885,#81886,#81887,#81888,#81889,#81890,#81891,#81892,
#81893,#81894,#81895,#81896,#81897,#81898,#81899,#81900,#81901,#81902,#81903,
#81904,#81905,#81906,#81907,#81908,#81909,#81910,#81911,#81912,#81913,#81914,
#81915,#81916,#81917,#81918,#81919,#81920,#81921,#81922,#81923,#81924,#81925,
#81926,#81927,#81928,#81929,#81930,#81931,#81932,#81933,#81934,#81935,#81936,
#81937,#81938,#81939,#81940,#81941,#81942,#81943,#81944,#81945,#81946,#81947,
#81948,#81949,#81950),.UNSPECIFIED.,.F.,.F.,(4,3,3,3,3,3,3,3,3,3,3,3,3,
3,3,3,3,3,3,3,3,3,3,3,3,3,3,3,4),(-0.276631791712723,-0.266952028164814,
-0.252323110100293,-0.245291653864685,-0.242249974245191,-0.226984934997862,
-0.216140077984231,-0.211926799186654,-0.208886967893919,-0.193126476631429,
-0.177076564913133,-0.167863943407054,-0.162681030994628,-0.159693742323349,
-0.143166607617838,-0.140226078888816,-0.124274130962391,-0.11608860686451,
-0.111105706623904,-0.10781700186492,-0.0912655940336371,-0.0743533484091529,
-0.0648492894661215,-0.0586243472175359,-0.0554854283171653,-0.0380411167797804,
-0.020552125725747,-0.00346625662044922,0.),.UNSPECIFIED.);
#3280=B_SPLINE_CURVE_WITH_KNOTS('',3,(#81951,#81952,#81953,#81954,#81955,
#81956,#81957,#81958,#81959),.UNSPECIFIED.,.F.,.F.,(4,1,1,1,1,1,4),(10.3752088276281,
11.290528578729,12.2866927202025,13.282856861676,14.2790210031496,15.2751851446231,
15.7079632679489),.UNSPECIFIED.);
#3281=B_SPLINE_CURVE_WITH_KNOTS('',3,(#81965,#81966,#81967,#81968,#81969,
#81970,#81971,#81972,#81973,#81974,#81975,#81976,#81977,#81978,#81979,#81980,
#81981,#81982,#81983,#81984,#81985,#81986,#81987,#81988,#81989,#81990,#81991,
#81992,#81993,#81994,#81995,#81996,#81997,#81998,#81999,#82000,#82001,#82002,
#82003,#82004,#82005,#82006,#82007,#82008,#82009,#82010,#82011,#82012,#82013,
#82014,#82015,#82016,#82017,#82018,#82019,#82020,#82021,#82022,#82023,#82024,
#82025,#82026,#82027,#82028,#82029,#82030,#82031,#82032,#82033,#82034,#82035,
#82036,#82037,#82038,#82039,#82040,#82041,#82042,#82043,#82044,#82045,#82046,
#82047,#82048,#82049),.UNSPECIFIED.,.F.,.F.,(4,3,3,3,3,3,3,3,3,3,3,3,3,
3,3,3,3,3,3,3,3,3,3,3,3,3,3,3,4),(-0.275362278356885,-0.263558129214756,
-0.246259601438024,-0.240454828090957,-0.236894346107961,-0.233127679120847,
-0.215926621847007,-0.204582032491244,-0.200546888044474,-0.196717301354411,
-0.17996536893454,-0.163633454327148,-0.154017567495587,-0.147105232827191,
-0.144181241921046,-0.128328604154869,-0.125169907000904,-0.108166390597872,
-0.100869563000488,-0.0956369336203211,-0.0926001921206514,-0.0768321064508614,
-0.0611424315003572,-0.0532927214375046,-0.0475055703614835,-0.0447074615733897,
-0.0295993573058915,-0.0147996786529457,0.),.UNSPECIFIED.);
#3282=B_SPLINE_CURVE_WITH_KNOTS('',3,(#82052,#82053,#82054,#82055,#82056,
#82057,#82058,#82059),.UNSPECIFIED.,.F.,.F.,(4,1,1,1,1,4),(11.6159397475004,
12.6121038889739,13.6082680304475,14.604432171921,15.6005963133945,15.707963267949),
 .UNSPECIFIED.);
#3283=B_SPLINE_CURVE_WITH_KNOTS('',3,(#82248,#82249,#82250,#82251,#82252,
#82253,#82254,#82255,#82256,#82257),.UNSPECIFIED.,.F.,.F.,(4,3,3,4),(-43.8312222248353,
-42.8350580833617,-41.8388939418882,-41.791135363526),.UNSPECIFIED.);
#3284=FACE_BOUND('',#5341,.T.);
#3285=FACE_BOUND('',#5342,.T.);
#3286=FACE_BOUND('',#5343,.T.);
#3287=FACE_BOUND('',#5344,.T.);
#3288=FACE_BOUND('',#5345,.T.);
#3289=FACE_BOUND('',#5346,.T.);
#3290=FACE_BOUND('',#5347,.T.);
#3291=FACE_BOUND('',#5348,.T.);
#3292=FACE_BOUND('',#5353,.T.);
#3293=FACE_BOUND('',#5354,.T.);
#3294=FACE_BOUND('',#5361,.T.);
#3295=FACE_BOUND('',#5365,.T.);
#3296=FACE_BOUND('',#5369,.T.);
#3297=FACE_BOUND('',#5373,.T.);
#3298=FACE_BOUND('',#5389,.T.);
#3299=FACE_BOUND('',#5390,.T.);
#3300=FACE_BOUND('',#5391,.T.);
#3301=FACE_BOUND('',#5392,.T.);
#3302=FACE_BOUND('',#5393,.T.);
#3303=FACE_BOUND('',#5394,.T.);
#3304=FACE_BOUND('',#5395,.T.);
#3305=FACE_BOUND('',#5396,.T.);
#3306=FACE_BOUND('',#5397,.T.);
#3307=FACE_BOUND('',#5398,.T.);
#3308=FACE_BOUND('',#5399,.T.);
#3309=FACE_BOUND('',#5400,.T.);
#3310=FACE_BOUND('',#5401,.T.);
#3311=FACE_BOUND('',#5402,.T.);
#3312=FACE_BOUND('',#5403,.T.);
#3313=FACE_BOUND('',#5404,.T.);
#3314=FACE_BOUND('',#5405,.T.);
#3315=FACE_BOUND('',#5408,.T.);
#3316=FACE_BOUND('',#5409,.T.);
#3317=FACE_BOUND('',#5410,.T.);
#3318=FACE_BOUND('',#5411,.T.);
#3319=FACE_BOUND('',#5412,.T.);
#3320=FACE_BOUND('',#5633,.T.);
#3321=FACE_BOUND('',#5637,.T.);
#3322=FACE_BOUND('',#5638,.T.);
#3323=FACE_BOUND('',#5639,.T.);
#3324=FACE_BOUND('',#5640,.T.);
#3325=FACE_BOUND('',#5641,.T.);
#3326=FACE_BOUND('',#5642,.T.);
#3327=FACE_BOUND('',#5643,.T.);
#3328=FACE_BOUND('',#5644,.T.);
#3329=FACE_BOUND('',#5645,.T.);
#3330=FACE_BOUND('',#5646,.T.);
#3331=FACE_BOUND('',#5672,.T.);
#3332=FACE_BOUND('',#5673,.T.);
#3333=FACE_BOUND('',#5674,.T.);
#3334=FACE_BOUND('',#5675,.T.);
#3335=FACE_BOUND('',#5705,.T.);
#3336=FACE_BOUND('',#5749,.T.);
#3337=FACE_BOUND('',#5767,.T.);
#3338=FACE_BOUND('',#5771,.T.);
#3339=FACE_BOUND('',#5775,.T.);
#3340=FACE_BOUND('',#5779,.T.);
#3341=FACE_BOUND('',#5783,.T.);
#3342=FACE_BOUND('',#5787,.T.);
#3343=FACE_BOUND('',#5791,.T.);
#3344=FACE_BOUND('',#5795,.T.);
#3345=FACE_BOUND('',#5799,.T.);
#3346=FACE_BOUND('',#5807,.T.);
#3347=FACE_BOUND('',#5811,.T.);
#3348=FACE_BOUND('',#5821,.T.);
#3349=FACE_BOUND('',#5825,.T.);
#3350=FACE_BOUND('',#5828,.T.);
#3351=FACE_BOUND('',#5829,.T.);
#3352=FACE_BOUND('',#5830,.T.);
#3353=FACE_BOUND('',#5831,.T.);
#3354=FACE_BOUND('',#5832,.T.);
#3355=FACE_BOUND('',#5833,.T.);
#3356=FACE_BOUND('',#5834,.T.);
#3357=FACE_BOUND('',#5835,.T.);
#3358=FACE_BOUND('',#5836,.T.);
#3359=FACE_BOUND('',#5837,.T.);
#3360=FACE_BOUND('',#5838,.T.);
#3361=FACE_BOUND('',#5839,.T.);
#3362=FACE_BOUND('',#5840,.T.);
#3363=FACE_BOUND('',#5841,.T.);
#3364=FACE_BOUND('',#5842,.T.);
#3365=FACE_BOUND('',#5843,.T.);
#3366=FACE_BOUND('',#5844,.T.);
#3367=FACE_BOUND('',#5845,.T.);
#3368=FACE_BOUND('',#5846,.T.);
#3369=FACE_BOUND('',#5847,.T.);
#3370=FACE_BOUND('',#5848,.T.);
#3371=FACE_BOUND('',#5849,.T.);
#3372=FACE_BOUND('',#5850,.T.);
#3373=FACE_BOUND('',#5851,.T.);
#3374=FACE_BOUND('',#5852,.T.);
#3375=FACE_BOUND('',#5853,.T.);
#3376=FACE_BOUND('',#5854,.T.);
#3377=FACE_BOUND('',#5855,.T.);
#3378=FACE_BOUND('',#5856,.T.);
#3379=FACE_BOUND('',#5857,.T.);
#3380=FACE_BOUND('',#5858,.T.);
#3381=FACE_BOUND('',#5859,.T.);
#3382=FACE_BOUND('',#5860,.T.);
#3383=FACE_BOUND('',#5861,.T.);
#3384=FACE_BOUND('',#5862,.T.);
#3385=FACE_BOUND('',#5863,.T.);
#3386=FACE_BOUND('',#5864,.T.);
#3387=FACE_BOUND('',#5865,.T.);
#3388=FACE_BOUND('',#5866,.T.);
#3389=FACE_BOUND('',#5867,.T.);
#3390=FACE_BOUND('',#5868,.T.);
#3391=FACE_BOUND('',#5869,.T.);
#3392=FACE_BOUND('',#5945,.T.);
#3393=FACE_BOUND('',#5946,.T.);
#3394=FACE_BOUND('',#5947,.T.);
#3395=FACE_BOUND('',#5948,.T.);
#3396=FACE_BOUND('',#5949,.T.);
#3397=FACE_BOUND('',#5950,.T.);
#3398=FACE_BOUND('',#5951,.T.);
#3399=FACE_BOUND('',#5952,.T.);
#3400=FACE_BOUND('',#5953,.T.);
#3401=FACE_BOUND('',#5954,.T.);
#3402=FACE_BOUND('',#5955,.T.);
#3403=FACE_BOUND('',#5956,.T.);
#3404=FACE_BOUND('',#5957,.T.);
#3405=FACE_BOUND('',#5958,.T.);
#3406=FACE_BOUND('',#5959,.T.);
#3407=FACE_BOUND('',#5960,.T.);
#3408=FACE_BOUND('',#5961,.T.);
#3409=FACE_BOUND('',#5962,.T.);
#3410=FACE_BOUND('',#5963,.T.);
#3411=FACE_BOUND('',#5964,.T.);
#3412=FACE_BOUND('',#5965,.T.);
#3413=FACE_BOUND('',#5966,.T.);
#3414=FACE_BOUND('',#5967,.T.);
#3415=FACE_BOUND('',#5968,.T.);
#3416=FACE_BOUND('',#5969,.T.);
#3417=FACE_BOUND('',#5970,.T.);
#3418=FACE_BOUND('',#5971,.T.);
#3419=FACE_BOUND('',#5972,.T.);
#3420=FACE_BOUND('',#5973,.T.);
#3421=FACE_BOUND('',#5974,.T.);
#3422=FACE_BOUND('',#5975,.T.);
#3423=FACE_BOUND('',#5976,.T.);
#3424=FACE_BOUND('',#5977,.T.);
#3425=FACE_BOUND('',#5978,.T.);
#3426=FACE_BOUND('',#5979,.T.);
#3427=FACE_BOUND('',#5980,.T.);
#3428=FACE_BOUND('',#5981,.T.);
#3429=FACE_BOUND('',#5982,.T.);
#3430=FACE_BOUND('',#5983,.T.);
#3431=FACE_BOUND('',#5984,.T.);
#3432=FACE_BOUND('',#5985,.T.);
#3433=FACE_BOUND('',#5986,.T.);
#3434=FACE_BOUND('',#6058,.T.);
#3435=FACE_BOUND('',#6059,.T.);
#3436=FACE_BOUND('',#6061,.T.);
#3437=FACE_BOUND('',#6062,.T.);
#3438=FACE_BOUND('',#6071,.T.);
#3439=FACE_BOUND('',#6073,.T.);
#3440=FACE_BOUND('',#6075,.T.);
#3441=FACE_BOUND('',#6077,.T.);
#3442=FACE_BOUND('',#6084,.T.);
#3443=FACE_BOUND('',#6091,.T.);
#3444=FACE_BOUND('',#6096,.T.);
#3445=FACE_BOUND('',#6276,.T.);
#3446=FACE_BOUND('',#6280,.T.);
#3447=FACE_BOUND('',#6287,.T.);
#3448=FACE_BOUND('',#6289,.T.);
#3449=FACE_BOUND('',#6290,.T.);
#3450=FACE_BOUND('',#6291,.T.);
#3451=FACE_BOUND('',#6292,.T.);
#3452=FACE_BOUND('',#6293,.T.);
#3453=FACE_BOUND('',#6294,.T.);
#3454=FACE_BOUND('',#6295,.T.);
#3455=FACE_BOUND('',#6296,.T.);
#3456=FACE_BOUND('',#6297,.T.);
#3457=FACE_BOUND('',#6298,.T.);
#3458=FACE_BOUND('',#6299,.T.);
#3459=FACE_BOUND('',#6300,.T.);
#3460=FACE_BOUND('',#6301,.T.);
#3461=FACE_BOUND('',#6302,.T.);
#3462=FACE_BOUND('',#6303,.T.);
#3463=FACE_BOUND('',#6304,.T.);
#3464=FACE_BOUND('',#6305,.T.);
#3465=FACE_BOUND('',#6306,.T.);
#3466=FACE_BOUND('',#6307,.T.);
#3467=FACE_BOUND('',#6308,.T.);
#3468=FACE_BOUND('',#6309,.T.);
#3469=FACE_BOUND('',#6310,.T.);
#3470=FACE_BOUND('',#6311,.T.);
#3471=FACE_BOUND('',#6312,.T.);
#3472=FACE_BOUND('',#6313,.T.);
#3473=FACE_BOUND('',#6314,.T.);
#3474=FACE_BOUND('',#6315,.T.);
#3475=FACE_BOUND('',#6316,.T.);
#3476=FACE_BOUND('',#6317,.T.);
#3477=FACE_BOUND('',#6318,.T.);
#3478=FACE_BOUND('',#6319,.T.);
#3479=FACE_BOUND('',#6320,.T.);
#3480=FACE_BOUND('',#6321,.T.);
#3481=FACE_BOUND('',#6322,.T.);
#3482=FACE_BOUND('',#6323,.T.);
#3483=FACE_BOUND('',#6326,.T.);
#3484=FACE_BOUND('',#6329,.T.);
#3485=FACE_BOUND('',#6332,.T.);
#3486=FACE_BOUND('',#6345,.T.);
#3487=FACE_BOUND('',#6348,.T.);
#3488=FACE_BOUND('',#6442,.T.);
#3489=FACE_BOUND('',#6595,.T.);
#3490=FACE_BOUND('',#6599,.T.);
#3491=FACE_BOUND('',#6600,.T.);
#3492=FACE_BOUND('',#6601,.T.);
#3493=FACE_BOUND('',#6602,.T.);
#3494=FACE_BOUND('',#6603,.T.);
#3495=FACE_BOUND('',#6604,.T.);
#3496=FACE_BOUND('',#6605,.T.);
#3497=FACE_BOUND('',#6606,.T.);
#3498=FACE_BOUND('',#6607,.T.);
#3499=FACE_BOUND('',#6608,.T.);
#3500=FACE_BOUND('',#6609,.T.);
#3501=FACE_BOUND('',#6610,.T.);
#3502=FACE_BOUND('',#6611,.T.);
#3503=FACE_BOUND('',#6612,.T.);
#3504=FACE_BOUND('',#6613,.T.);
#3505=FACE_BOUND('',#6614,.T.);
#3506=FACE_BOUND('',#6615,.T.);
#3507=FACE_BOUND('',#6616,.T.);
#3508=FACE_BOUND('',#6617,.T.);
#3509=FACE_BOUND('',#6618,.T.);
#3510=FACE_BOUND('',#6619,.T.);
#3511=FACE_BOUND('',#6620,.T.);
#3512=FACE_BOUND('',#6621,.T.);
#3513=FACE_BOUND('',#6622,.T.);
#3514=FACE_BOUND('',#6623,.T.);
#3515=FACE_BOUND('',#6624,.T.);
#3516=FACE_BOUND('',#6625,.T.);
#3517=FACE_BOUND('',#6626,.T.);
#3518=FACE_BOUND('',#6627,.T.);
#3519=FACE_BOUND('',#6628,.T.);
#3520=FACE_BOUND('',#6629,.T.);
#3521=FACE_BOUND('',#6630,.T.);
#3522=FACE_BOUND('',#6631,.T.);
#3523=FACE_BOUND('',#6632,.T.);
#3524=FACE_BOUND('',#6633,.T.);
#3525=FACE_BOUND('',#6636,.T.);
#3526=FACE_BOUND('',#6788,.T.);
#3527=FACE_BOUND('',#6941,.T.);
#3528=FACE_BOUND('',#6945,.T.);
#3529=FACE_BOUND('',#6946,.T.);
#3530=FACE_BOUND('',#6947,.T.);
#3531=FACE_BOUND('',#6948,.T.);
#3532=FACE_BOUND('',#6949,.T.);
#3533=FACE_BOUND('',#6950,.T.);
#3534=FACE_BOUND('',#6951,.T.);
#3535=FACE_BOUND('',#6952,.T.);
#3536=FACE_BOUND('',#6953,.T.);
#3537=FACE_BOUND('',#6954,.T.);
#3538=FACE_BOUND('',#6955,.T.);
#3539=FACE_BOUND('',#6956,.T.);
#3540=FACE_BOUND('',#6957,.T.);
#3541=FACE_BOUND('',#6958,.T.);
#3542=FACE_BOUND('',#6959,.T.);
#3543=FACE_BOUND('',#6960,.T.);
#3544=FACE_BOUND('',#6961,.T.);
#3545=FACE_BOUND('',#6962,.T.);
#3546=FACE_BOUND('',#6963,.T.);
#3547=FACE_BOUND('',#6964,.T.);
#3548=FACE_BOUND('',#6965,.T.);
#3549=FACE_BOUND('',#6966,.T.);
#3550=FACE_BOUND('',#6967,.T.);
#3551=FACE_BOUND('',#6968,.T.);
#3552=FACE_BOUND('',#6969,.T.);
#3553=FACE_BOUND('',#6970,.T.);
#3554=FACE_BOUND('',#6971,.T.);
#3555=FACE_BOUND('',#6972,.T.);
#3556=FACE_BOUND('',#6973,.T.);
#3557=FACE_BOUND('',#6974,.T.);
#3558=FACE_BOUND('',#6975,.T.);
#3559=FACE_BOUND('',#6976,.T.);
#3560=FACE_BOUND('',#6977,.T.);
#3561=FACE_BOUND('',#6978,.T.);
#3562=FACE_BOUND('',#6979,.T.);
#3563=FACE_BOUND('',#6982,.T.);
#3564=FACE_BOUND('',#7019,.T.);
#3565=FACE_BOUND('',#7027,.T.);
#3566=FACE_BOUND('',#7062,.T.);
#3567=FACE_BOUND('',#7064,.T.);
#3568=FACE_BOUND('',#7067,.T.);
#3569=FACE_BOUND('',#7071,.T.);
#3570=FACE_BOUND('',#7081,.T.);
#3571=FACE_BOUND('',#7085,.T.);
#3572=FACE_BOUND('',#7249,.T.);
#3573=FACE_BOUND('',#7253,.T.);
#3574=FACE_BOUND('',#7324,.T.);
#3575=FACE_BOUND('',#7348,.T.);
#3576=FACE_BOUND('',#7381,.T.);
#3577=FACE_OUTER_BOUND('',#5333,.T.);
#3578=FACE_OUTER_BOUND('',#5334,.T.);
#3579=FACE_OUTER_BOUND('',#5335,.T.);
#3580=FACE_OUTER_BOUND('',#5336,.T.);
#3581=FACE_OUTER_BOUND('',#5337,.T.);
#3582=FACE_OUTER_BOUND('',#5338,.T.);
#3583=FACE_OUTER_BOUND('',#5339,.T.);
#3584=FACE_OUTER_BOUND('',#5340,.T.);
#3585=FACE_OUTER_BOUND('',#5349,.T.);
#3586=FACE_OUTER_BOUND('',#5350,.T.);
#3587=FACE_OUTER_BOUND('',#5351,.T.);
#3588=FACE_OUTER_BOUND('',#5352,.T.);
#3589=FACE_OUTER_BOUND('',#5355,.T.);
#3590=FACE_OUTER_BOUND('',#5356,.T.);
#3591=FACE_OUTER_BOUND('',#5357,.T.);
#3592=FACE_OUTER_BOUND('',#5358,.T.);
#3593=FACE_OUTER_BOUND('',#5359,.T.);
#3594=FACE_OUTER_BOUND('',#5360,.T.);
#3595=FACE_OUTER_BOUND('',#5362,.T.);
#3596=FACE_OUTER_BOUND('',#5363,.T.);
#3597=FACE_OUTER_BOUND('',#5364,.T.);
#3598=FACE_OUTER_BOUND('',#5366,.T.);
#3599=FACE_OUTER_BOUND('',#5367,.T.);
#3600=FACE_OUTER_BOUND('',#5368,.T.);
#3601=FACE_OUTER_BOUND('',#5370,.T.);
#3602=FACE_OUTER_BOUND('',#5371,.T.);
#3603=FACE_OUTER_BOUND('',#5372,.T.);
#3604=FACE_OUTER_BOUND('',#5374,.T.);
#3605=FACE_OUTER_BOUND('',#5375,.T.);
#3606=FACE_OUTER_BOUND('',#5376,.T.);
#3607=FACE_OUTER_BOUND('',#5377,.T.);
#3608=FACE_OUTER_BOUND('',#5378,.T.);
#3609=FACE_OUTER_BOUND('',#5379,.T.);
#3610=FACE_OUTER_BOUND('',#5380,.T.);
#3611=FACE_OUTER_BOUND('',#5381,.T.);
#3612=FACE_OUTER_BOUND('',#5382,.T.);
#3613=FACE_OUTER_BOUND('',#5383,.T.);
#3614=FACE_OUTER_BOUND('',#5384,.T.);
#3615=FACE_OUTER_BOUND('',#5385,.T.);
#3616=FACE_OUTER_BOUND('',#5386,.T.);
#3617=FACE_OUTER_BOUND('',#5387,.T.);
#3618=FACE_OUTER_BOUND('',#5388,.T.);
#3619=FACE_OUTER_BOUND('',#5406,.T.);
#3620=FACE_OUTER_BOUND('',#5407,.T.);
#3621=FACE_OUTER_BOUND('',#5413,.T.);
#3622=FACE_OUTER_BOUND('',#5414,.T.);
#3623=FACE_OUTER_BOUND('',#5415,.T.);
#3624=FACE_OUTER_BOUND('',#5416,.T.);
#3625=FACE_OUTER_BOUND('',#5417,.T.);
#3626=FACE_OUTER_BOUND('',#5418,.T.);
#3627=FACE_OUTER_BOUND('',#5419,.T.);
#3628=FACE_OUTER_BOUND('',#5420,.T.);
#3629=FACE_OUTER_BOUND('',#5421,.T.);
#3630=FACE_OUTER_BOUND('',#5422,.T.);
#3631=FACE_OUTER_BOUND('',#5423,.T.);
#3632=FACE_OUTER_BOUND('',#5424,.T.);
#3633=FACE_OUTER_BOUND('',#5425,.T.);
#3634=FACE_OUTER_BOUND('',#5426,.T.);
#3635=FACE_OUTER_BOUND('',#5427,.T.);
#3636=FACE_OUTER_BOUND('',#5428,.T.);
#3637=FACE_OUTER_BOUND('',#5429,.T.);
#3638=FACE_OUTER_BOUND('',#5430,.T.);
#3639=FACE_OUTER_BOUND('',#5431,.T.);
#3640=FACE_OUTER_BOUND('',#5432,.T.);
#3641=FACE_OUTER_BOUND('',#5433,.T.);
#3642=FACE_OUTER_BOUND('',#5434,.T.);
#3643=FACE_OUTER_BOUND('',#5435,.T.);
#3644=FACE_OUTER_BOUND('',#5436,.T.);
#3645=FACE_OUTER_BOUND('',#5437,.T.);
#3646=FACE_OUTER_BOUND('',#5438,.T.);
#3647=FACE_OUTER_BOUND('',#5439,.T.);
#3648=FACE_OUTER_BOUND('',#5440,.T.);
#3649=FACE_OUTER_BOUND('',#5441,.T.);
#3650=FACE_OUTER_BOUND('',#5442,.T.);
#3651=FACE_OUTER_BOUND('',#5443,.T.);
#3652=FACE_OUTER_BOUND('',#5444,.T.);
#3653=FACE_OUTER_BOUND('',#5445,.T.);
#3654=FACE_OUTER_BOUND('',#5446,.T.);
#3655=FACE_OUTER_BOUND('',#5447,.T.);
#3656=FACE_OUTER_BOUND('',#5448,.T.);
#3657=FACE_OUTER_BOUND('',#5449,.T.);
#3658=FACE_OUTER_BOUND('',#5450,.T.);
#3659=FACE_OUTER_BOUND('',#5451,.T.);
#3660=FACE_OUTER_BOUND('',#5452,.T.);
#3661=FACE_OUTER_BOUND('',#5453,.T.);
#3662=FACE_OUTER_BOUND('',#5454,.T.);
#3663=FACE_OUTER_BOUND('',#5455,.T.);
#3664=FACE_OUTER_BOUND('',#5456,.T.);
#3665=FACE_OUTER_BOUND('',#5457,.T.);
#3666=FACE_OUTER_BOUND('',#5458,.T.);
#3667=FACE_OUTER_BOUND('',#5459,.T.);
#3668=FACE_OUTER_BOUND('',#5460,.T.);
#3669=FACE_OUTER_BOUND('',#5461,.T.);
#3670=FACE_OUTER_BOUND('',#5462,.T.);
#3671=FACE_OUTER_BOUND('',#5463,.T.);
#3672=FACE_OUTER_BOUND('',#5464,.T.);
#3673=FACE_OUTER_BOUND('',#5465,.T.);
#3674=FACE_OUTER_BOUND('',#5466,.T.);
#3675=FACE_OUTER_BOUND('',#5467,.T.);
#3676=FACE_OUTER_BOUND('',#5468,.T.);
#3677=FACE_OUTER_BOUND('',#5469,.T.);
#3678=FACE_OUTER_BOUND('',#5470,.T.);
#3679=FACE_OUTER_BOUND('',#5471,.T.);
#3680=FACE_OUTER_BOUND('',#5472,.T.);
#3681=FACE_OUTER_BOUND('',#5473,.T.);
#3682=FACE_OUTER_BOUND('',#5474,.T.);
#3683=FACE_OUTER_BOUND('',#5475,.T.);
#3684=FACE_OUTER_BOUND('',#5476,.T.);
#3685=FACE_OUTER_BOUND('',#5477,.T.);
#3686=FACE_OUTER_BOUND('',#5478,.T.);
#3687=FACE_OUTER_BOUND('',#5479,.T.);
#3688=FACE_OUTER_BOUND('',#5480,.T.);
#3689=FACE_OUTER_BOUND('',#5481,.T.);
#3690=FACE_OUTER_BOUND('',#5482,.T.);
#3691=FACE_OUTER_BOUND('',#5483,.T.);
#3692=FACE_OUTER_BOUND('',#5484,.T.);
#3693=FACE_OUTER_BOUND('',#5485,.T.);
#3694=FACE_OUTER_BOUND('',#5486,.T.);
#3695=FACE_OUTER_BOUND('',#5487,.T.);
#3696=FACE_OUTER_BOUND('',#5488,.T.);
#3697=FACE_OUTER_BOUND('',#5489,.T.);
#3698=FACE_OUTER_BOUND('',#5490,.T.);
#3699=FACE_OUTER_BOUND('',#5491,.T.);
#3700=FACE_OUTER_BOUND('',#5492,.T.);
#3701=FACE_OUTER_BOUND('',#5493,.T.);
#3702=FACE_OUTER_BOUND('',#5494,.T.);
#3703=FACE_OUTER_BOUND('',#5495,.T.);
#3704=FACE_OUTER_BOUND('',#5496,.T.);
#3705=FACE_OUTER_BOUND('',#5497,.T.);
#3706=FACE_OUTER_BOUND('',#5498,.T.);
#3707=FACE_OUTER_BOUND('',#5499,.T.);
#3708=FACE_OUTER_BOUND('',#5500,.T.);
#3709=FACE_OUTER_BOUND('',#5501,.T.);
#3710=FACE_OUTER_BOUND('',#5502,.T.);
#3711=FACE_OUTER_BOUND('',#5503,.T.);
#3712=FACE_OUTER_BOUND('',#5504,.T.);
#3713=FACE_OUTER_BOUND('',#5505,.T.);
#3714=FACE_OUTER_BOUND('',#5506,.T.);
#3715=FACE_OUTER_BOUND('',#5507,.T.);
#3716=FACE_OUTER_BOUND('',#5508,.T.);
#3717=FACE_OUTER_BOUND('',#5509,.T.);
#3718=FACE_OUTER_BOUND('',#5510,.T.);
#3719=FACE_OUTER_BOUND('',#5511,.T.);
#3720=FACE_OUTER_BOUND('',#5512,.T.);
#3721=FACE_OUTER_BOUND('',#5513,.T.);
#3722=FACE_OUTER_BOUND('',#5514,.T.);
#3723=FACE_OUTER_BOUND('',#5515,.T.);
#3724=FACE_OUTER_BOUND('',#5516,.T.);
#3725=FACE_OUTER_BOUND('',#5517,.T.);
#3726=FACE_OUTER_BOUND('',#5518,.T.);
#3727=FACE_OUTER_BOUND('',#5519,.T.);
#3728=FACE_OUTER_BOUND('',#5520,.T.);
#3729=FACE_OUTER_BOUND('',#5521,.T.);
#3730=FACE_OUTER_BOUND('',#5522,.T.);
#3731=FACE_OUTER_BOUND('',#5523,.T.);
#3732=FACE_OUTER_BOUND('',#5524,.T.);
#3733=FACE_OUTER_BOUND('',#5525,.T.);
#3734=FACE_OUTER_BOUND('',#5526,.T.);
#3735=FACE_OUTER_BOUND('',#5527,.T.);
#3736=FACE_OUTER_BOUND('',#5528,.T.);
#3737=FACE_OUTER_BOUND('',#5529,.T.);
#3738=FACE_OUTER_BOUND('',#5530,.T.);
#3739=FACE_OUTER_BOUND('',#5531,.T.);
#3740=FACE_OUTER_BOUND('',#5532,.T.);
#3741=FACE_OUTER_BOUND('',#5533,.T.);
#3742=FACE_OUTER_BOUND('',#5534,.T.);
#3743=FACE_OUTER_BOUND('',#5535,.T.);
#3744=FACE_OUTER_BOUND('',#5536,.T.);
#3745=FACE_OUTER_BOUND('',#5537,.T.);
#3746=FACE_OUTER_BOUND('',#5538,.T.);
#3747=FACE_OUTER_BOUND('',#5539,.T.);
#3748=FACE_OUTER_BOUND('',#5540,.T.);
#3749=FACE_OUTER_BOUND('',#5541,.T.);
#3750=FACE_OUTER_BOUND('',#5542,.T.);
#3751=FACE_OUTER_BOUND('',#5543,.T.);
#3752=FACE_OUTER_BOUND('',#5544,.T.);
#3753=FACE_OUTER_BOUND('',#5545,.T.);
#3754=FACE_OUTER_BOUND('',#5546,.T.);
#3755=FACE_OUTER_BOUND('',#5547,.T.);
#3756=FACE_OUTER_BOUND('',#5548,.T.);
#3757=FACE_OUTER_BOUND('',#5549,.T.);
#3758=FACE_OUTER_BOUND('',#5550,.T.);
#3759=FACE_OUTER_BOUND('',#5551,.T.);
#3760=FACE_OUTER_BOUND('',#5552,.T.);
#3761=FACE_OUTER_BOUND('',#5553,.T.);
#3762=FACE_OUTER_BOUND('',#5554,.T.);
#3763=FACE_OUTER_BOUND('',#5555,.T.);
#3764=FACE_OUTER_BOUND('',#5556,.T.);
#3765=FACE_OUTER_BOUND('',#5557,.T.);
#3766=FACE_OUTER_BOUND('',#5558,.T.);
#3767=FACE_OUTER_BOUND('',#5559,.T.);
#3768=FACE_OUTER_BOUND('',#5560,.T.);
#3769=FACE_OUTER_BOUND('',#5561,.T.);
#3770=FACE_OUTER_BOUND('',#5562,.T.);
#3771=FACE_OUTER_BOUND('',#5563,.T.);
#3772=FACE_OUTER_BOUND('',#5564,.T.);
#3773=FACE_OUTER_BOUND('',#5565,.T.);
#3774=FACE_OUTER_BOUND('',#5566,.T.);
#3775=FACE_OUTER_BOUND('',#5567,.T.);
#3776=FACE_OUTER_BOUND('',#5568,.T.);
#3777=FACE_OUTER_BOUND('',#5569,.T.);
#3778=FACE_OUTER_BOUND('',#5570,.T.);
#3779=FACE_OUTER_BOUND('',#5571,.T.);
#3780=FACE_OUTER_BOUND('',#5572,.T.);
#3781=FACE_OUTER_BOUND('',#5573,.T.);
#3782=FACE_OUTER_BOUND('',#5574,.T.);
#3783=FACE_OUTER_BOUND('',#5575,.T.);
#3784=FACE_OUTER_BOUND('',#5576,.T.);
#3785=FACE_OUTER_BOUND('',#5577,.T.);
#3786=FACE_OUTER_BOUND('',#5578,.T.);
#3787=FACE_OUTER_BOUND('',#5579,.T.);
#3788=FACE_OUTER_BOUND('',#5580,.T.);
#3789=FACE_OUTER_BOUND('',#5581,.T.);
#3790=FACE_OUTER_BOUND('',#5582,.T.);
#3791=FACE_OUTER_BOUND('',#5583,.T.);
#3792=FACE_OUTER_BOUND('',#5584,.T.);
#3793=FACE_OUTER_BOUND('',#5585,.T.);
#3794=FACE_OUTER_BOUND('',#5586,.T.);
#3795=FACE_OUTER_BOUND('',#5587,.T.);
#3796=FACE_OUTER_BOUND('',#5588,.T.);
#3797=FACE_OUTER_BOUND('',#5589,.T.);
#3798=FACE_OUTER_BOUND('',#5590,.T.);
#3799=FACE_OUTER_BOUND('',#5591,.T.);
#3800=FACE_OUTER_BOUND('',#5592,.T.);
#3801=FACE_OUTER_BOUND('',#5593,.T.);
#3802=FACE_OUTER_BOUND('',#5594,.T.);
#3803=FACE_OUTER_BOUND('',#5595,.T.);
#3804=FACE_OUTER_BOUND('',#5596,.T.);
#3805=FACE_OUTER_BOUND('',#5597,.T.);
#3806=FACE_OUTER_BOUND('',#5598,.T.);
#3807=FACE_OUTER_BOUND('',#5599,.T.);
#3808=FACE_OUTER_BOUND('',#5600,.T.);
#3809=FACE_OUTER_BOUND('',#5601,.T.);
#3810=FACE_OUTER_BOUND('',#5602,.T.);
#3811=FACE_OUTER_BOUND('',#5603,.T.);
#3812=FACE_OUTER_BOUND('',#5604,.T.);
#3813=FACE_OUTER_BOUND('',#5605,.T.);
#3814=FACE_OUTER_BOUND('',#5606,.T.);
#3815=FACE_OUTER_BOUND('',#5607,.T.);
#3816=FACE_OUTER_BOUND('',#5608,.T.);
#3817=FACE_OUTER_BOUND('',#5609,.T.);
#3818=FACE_OUTER_BOUND('',#5610,.T.);
#3819=FACE_OUTER_BOUND('',#5611,.T.);
#3820=FACE_OUTER_BOUND('',#5612,.T.);
#3821=FACE_OUTER_BOUND('',#5613,.T.);
#3822=FACE_OUTER_BOUND('',#5614,.T.);
#3823=FACE_OUTER_BOUND('',#5615,.T.);
#3824=FACE_OUTER_BOUND('',#5616,.T.);
#3825=FACE_OUTER_BOUND('',#5617,.T.);
#3826=FACE_OUTER_BOUND('',#5618,.T.);
#3827=FACE_OUTER_BOUND('',#5619,.T.);
#3828=FACE_OUTER_BOUND('',#5620,.T.);
#3829=FACE_OUTER_BOUND('',#5621,.T.);
#3830=FACE_OUTER_BOUND('',#5622,.T.);
#3831=FACE_OUTER_BOUND('',#5623,.T.);
#3832=FACE_OUTER_BOUND('',#5624,.T.);
#3833=FACE_OUTER_BOUND('',#5625,.T.);
#3834=FACE_OUTER_BOUND('',#5626,.T.);
#3835=FACE_OUTER_BOUND('',#5627,.T.);
#3836=FACE_OUTER_BOUND('',#5628,.T.);
#3837=FACE_OUTER_BOUND('',#5629,.T.);
#3838=FACE_OUTER_BOUND('',#5630,.T.);
#3839=FACE_OUTER_BOUND('',#5631,.T.);
#3840=FACE_OUTER_BOUND('',#5632,.T.);
#3841=FACE_OUTER_BOUND('',#5634,.T.);
#3842=FACE_OUTER_BOUND('',#5635,.T.);
#3843=FACE_OUTER_BOUND('',#5636,.T.);
#3844=FACE_OUTER_BOUND('',#5647,.T.);
#3845=FACE_OUTER_BOUND('',#5648,.T.);
#3846=FACE_OUTER_BOUND('',#5649,.T.);
#3847=FACE_OUTER_BOUND('',#5650,.T.);
#3848=FACE_OUTER_BOUND('',#5651,.T.);
#3849=FACE_OUTER_BOUND('',#5652,.T.);
#3850=FACE_OUTER_BOUND('',#5653,.T.);
#3851=FACE_OUTER_BOUND('',#5654,.T.);
#3852=FACE_OUTER_BOUND('',#5655,.T.);
#3853=FACE_OUTER_BOUND('',#5656,.T.);
#3854=FACE_OUTER_BOUND('',#5657,.T.);
#3855=FACE_OUTER_BOUND('',#5658,.T.);
#3856=FACE_OUTER_BOUND('',#5659,.T.);
#3857=FACE_OUTER_BOUND('',#5660,.T.);
#3858=FACE_OUTER_BOUND('',#5661,.T.);
#3859=FACE_OUTER_BOUND('',#5662,.T.);
#3860=FACE_OUTER_BOUND('',#5663,.T.);
#3861=FACE_OUTER_BOUND('',#5664,.T.);
#3862=FACE_OUTER_BOUND('',#5665,.T.);
#3863=FACE_OUTER_BOUND('',#5666,.T.);
#3864=FACE_OUTER_BOUND('',#5667,.T.);
#3865=FACE_OUTER_BOUND('',#5668,.T.);
#3866=FACE_OUTER_BOUND('',#5669,.T.);
#3867=FACE_OUTER_BOUND('',#5670,.T.);
#3868=FACE_OUTER_BOUND('',#5671,.T.);
#3869=FACE_OUTER_BOUND('',#5676,.T.);
#3870=FACE_OUTER_BOUND('',#5677,.T.);
#3871=FACE_OUTER_BOUND('',#5678,.T.);
#3872=FACE_OUTER_BOUND('',#5679,.T.);
#3873=FACE_OUTER_BOUND('',#5680,.T.);
#3874=FACE_OUTER_BOUND('',#5681,.T.);
#3875=FACE_OUTER_BOUND('',#5682,.T.);
#3876=FACE_OUTER_BOUND('',#5683,.T.);
#3877=FACE_OUTER_BOUND('',#5684,.T.);
#3878=FACE_OUTER_BOUND('',#5685,.T.);
#3879=FACE_OUTER_BOUND('',#5686,.T.);
#3880=FACE_OUTER_BOUND('',#5687,.T.);
#3881=FACE_OUTER_BOUND('',#5688,.T.);
#3882=FACE_OUTER_BOUND('',#5689,.T.);
#3883=FACE_OUTER_BOUND('',#5690,.T.);
#3884=FACE_OUTER_BOUND('',#5691,.T.);
#3885=FACE_OUTER_BOUND('',#5692,.T.);
#3886=FACE_OUTER_BOUND('',#5693,.T.);
#3887=FACE_OUTER_BOUND('',#5694,.T.);
#3888=FACE_OUTER_BOUND('',#5695,.T.);
#3889=FACE_OUTER_BOUND('',#5696,.T.);
#3890=FACE_OUTER_BOUND('',#5697,.T.);
#3891=FACE_OUTER_BOUND('',#5698,.T.);
#3892=FACE_OUTER_BOUND('',#5699,.T.);
#3893=FACE_OUTER_BOUND('',#5700,.T.);
#3894=FACE_OUTER_BOUND('',#5701,.T.);
#3895=FACE_OUTER_BOUND('',#5702,.T.);
#3896=FACE_OUTER_BOUND('',#5703,.T.);
#3897=FACE_OUTER_BOUND('',#5704,.T.);
#3898=FACE_OUTER_BOUND('',#5706,.T.);
#3899=FACE_OUTER_BOUND('',#5707,.T.);
#3900=FACE_OUTER_BOUND('',#5708,.T.);
#3901=FACE_OUTER_BOUND('',#5709,.T.);
#3902=FACE_OUTER_BOUND('',#5710,.T.);
#3903=FACE_OUTER_BOUND('',#5711,.T.);
#3904=FACE_OUTER_BOUND('',#5712,.T.);
#3905=FACE_OUTER_BOUND('',#5713,.T.);
#3906=FACE_OUTER_BOUND('',#5714,.T.);
#3907=FACE_OUTER_BOUND('',#5715,.T.);
#3908=FACE_OUTER_BOUND('',#5716,.T.);
#3909=FACE_OUTER_BOUND('',#5717,.T.);
#3910=FACE_OUTER_BOUND('',#5718,.T.);
#3911=FACE_OUTER_BOUND('',#5719,.T.);
#3912=FACE_OUTER_BOUND('',#5720,.T.);
#3913=FACE_OUTER_BOUND('',#5721,.T.);
#3914=FACE_OUTER_BOUND('',#5722,.T.);
#3915=FACE_OUTER_BOUND('',#5723,.T.);
#3916=FACE_OUTER_BOUND('',#5724,.T.);
#3917=FACE_OUTER_BOUND('',#5725,.T.);
#3918=FACE_OUTER_BOUND('',#5726,.T.);
#3919=FACE_OUTER_BOUND('',#5727,.T.);
#3920=FACE_OUTER_BOUND('',#5728,.T.);
#3921=FACE_OUTER_BOUND('',#5729,.T.);
#3922=FACE_OUTER_BOUND('',#5730,.T.);
#3923=FACE_OUTER_BOUND('',#5731,.T.);
#3924=FACE_OUTER_BOUND('',#5732,.T.);
#3925=FACE_OUTER_BOUND('',#5733,.T.);
#3926=FACE_OUTER_BOUND('',#5734,.T.);
#3927=FACE_OUTER_BOUND('',#5735,.T.);
#3928=FACE_OUTER_BOUND('',#5736,.T.);
#3929=FACE_OUTER_BOUND('',#5737,.T.);
#3930=FACE_OUTER_BOUND('',#5738,.T.);
#3931=FACE_OUTER_BOUND('',#5739,.T.);
#3932=FACE_OUTER_BOUND('',#5740,.T.);
#3933=FACE_OUTER_BOUND('',#5741,.T.);
#3934=FACE_OUTER_BOUND('',#5742,.T.);
#3935=FACE_OUTER_BOUND('',#5743,.T.);
#3936=FACE_OUTER_BOUND('',#5744,.T.);
#3937=FACE_OUTER_BOUND('',#5745,.T.);
#3938=FACE_OUTER_BOUND('',#5746,.T.);
#3939=FACE_OUTER_BOUND('',#5747,.T.);
#3940=FACE_OUTER_BOUND('',#5748,.T.);
#3941=FACE_OUTER_BOUND('',#5750,.T.);
#3942=FACE_OUTER_BOUND('',#5751,.T.);
#3943=FACE_OUTER_BOUND('',#5752,.T.);
#3944=FACE_OUTER_BOUND('',#5753,.T.);
#3945=FACE_OUTER_BOUND('',#5754,.T.);
#3946=FACE_OUTER_BOUND('',#5755,.T.);
#3947=FACE_OUTER_BOUND('',#5756,.T.);
#3948=FACE_OUTER_BOUND('',#5757,.T.);
#3949=FACE_OUTER_BOUND('',#5758,.T.);
#3950=FACE_OUTER_BOUND('',#5759,.T.);
#3951=FACE_OUTER_BOUND('',#5760,.T.);
#3952=FACE_OUTER_BOUND('',#5761,.T.);
#3953=FACE_OUTER_BOUND('',#5762,.T.);
#3954=FACE_OUTER_BOUND('',#5763,.T.);
#3955=FACE_OUTER_BOUND('',#5764,.T.);
#3956=FACE_OUTER_BOUND('',#5765,.T.);
#3957=FACE_OUTER_BOUND('',#5766,.T.);
#3958=FACE_OUTER_BOUND('',#5768,.T.);
#3959=FACE_OUTER_BOUND('',#5769,.T.);
#3960=FACE_OUTER_BOUND('',#5770,.T.);
#3961=FACE_OUTER_BOUND('',#5772,.T.);
#3962=FACE_OUTER_BOUND('',#5773,.T.);
#3963=FACE_OUTER_BOUND('',#5774,.T.);
#3964=FACE_OUTER_BOUND('',#5776,.T.);
#3965=FACE_OUTER_BOUND('',#5777,.T.);
#3966=FACE_OUTER_BOUND('',#5778,.T.);
#3967=FACE_OUTER_BOUND('',#5780,.T.);
#3968=FACE_OUTER_BOUND('',#5781,.T.);
#3969=FACE_OUTER_BOUND('',#5782,.T.);
#3970=FACE_OUTER_BOUND('',#5784,.T.);
#3971=FACE_OUTER_BOUND('',#5785,.T.);
#3972=FACE_OUTER_BOUND('',#5786,.T.);
#3973=FACE_OUTER_BOUND('',#5788,.T.);
#3974=FACE_OUTER_BOUND('',#5789,.T.);
#3975=FACE_OUTER_BOUND('',#5790,.T.);
#3976=FACE_OUTER_BOUND('',#5792,.T.);
#3977=FACE_OUTER_BOUND('',#5793,.T.);
#3978=FACE_OUTER_BOUND('',#5794,.T.);
#3979=FACE_OUTER_BOUND('',#5796,.T.);
#3980=FACE_OUTER_BOUND('',#5797,.T.);
#3981=FACE_OUTER_BOUND('',#5798,.T.);
#3982=FACE_OUTER_BOUND('',#5800,.T.);
#3983=FACE_OUTER_BOUND('',#5801,.T.);
#3984=FACE_OUTER_BOUND('',#5802,.T.);
#3985=FACE_OUTER_BOUND('',#5803,.T.);
#3986=FACE_OUTER_BOUND('',#5804,.T.);
#3987=FACE_OUTER_BOUND('',#5805,.T.);
#3988=FACE_OUTER_BOUND('',#5806,.T.);
#3989=FACE_OUTER_BOUND('',#5808,.T.);
#3990=FACE_OUTER_BOUND('',#5809,.T.);
#3991=FACE_OUTER_BOUND('',#5810,.T.);
#3992=FACE_OUTER_BOUND('',#5812,.T.);
#3993=FACE_OUTER_BOUND('',#5813,.T.);
#3994=FACE_OUTER_BOUND('',#5814,.T.);
#3995=FACE_OUTER_BOUND('',#5815,.T.);
#3996=FACE_OUTER_BOUND('',#5816,.T.);
#3997=FACE_OUTER_BOUND('',#5817,.T.);
#3998=FACE_OUTER_BOUND('',#5818,.T.);
#3999=FACE_OUTER_BOUND('',#5819,.T.);
#4000=FACE_OUTER_BOUND('',#5820,.T.);
#4001=FACE_OUTER_BOUND('',#5822,.T.);
#4002=FACE_OUTER_BOUND('',#5823,.T.);
#4003=FACE_OUTER_BOUND('',#5824,.T.);
#4004=FACE_OUTER_BOUND('',#5826,.T.);
#4005=FACE_OUTER_BOUND('',#5827,.T.);
#4006=FACE_OUTER_BOUND('',#5870,.T.);
#4007=FACE_OUTER_BOUND('',#5871,.T.);
#4008=FACE_OUTER_BOUND('',#5872,.T.);
#4009=FACE_OUTER_BOUND('',#5873,.T.);
#4010=FACE_OUTER_BOUND('',#5874,.T.);
#4011=FACE_OUTER_BOUND('',#5875,.T.);
#4012=FACE_OUTER_BOUND('',#5876,.T.);
#4013=FACE_OUTER_BOUND('',#5877,.T.);
#4014=FACE_OUTER_BOUND('',#5878,.T.);
#4015=FACE_OUTER_BOUND('',#5879,.T.);
#4016=FACE_OUTER_BOUND('',#5880,.T.);
#4017=FACE_OUTER_BOUND('',#5881,.T.);
#4018=FACE_OUTER_BOUND('',#5882,.T.);
#4019=FACE_OUTER_BOUND('',#5883,.T.);
#4020=FACE_OUTER_BOUND('',#5884,.T.);
#4021=FACE_OUTER_BOUND('',#5885,.T.);
#4022=FACE_OUTER_BOUND('',#5886,.T.);
#4023=FACE_OUTER_BOUND('',#5887,.T.);
#4024=FACE_OUTER_BOUND('',#5888,.T.);
#4025=FACE_OUTER_BOUND('',#5889,.T.);
#4026=FACE_OUTER_BOUND('',#5890,.T.);
#4027=FACE_OUTER_BOUND('',#5891,.T.);
#4028=FACE_OUTER_BOUND('',#5892,.T.);
#4029=FACE_OUTER_BOUND('',#5893,.T.);
#4030=FACE_OUTER_BOUND('',#5894,.T.);
#4031=FACE_OUTER_BOUND('',#5895,.T.);
#4032=FACE_OUTER_BOUND('',#5896,.T.);
#4033=FACE_OUTER_BOUND('',#5897,.T.);
#4034=FACE_OUTER_BOUND('',#5898,.T.);
#4035=FACE_OUTER_BOUND('',#5899,.T.);
#4036=FACE_OUTER_BOUND('',#5900,.T.);
#4037=FACE_OUTER_BOUND('',#5901,.T.);
#4038=FACE_OUTER_BOUND('',#5902,.T.);
#4039=FACE_OUTER_BOUND('',#5903,.T.);
#4040=FACE_OUTER_BOUND('',#5904,.T.);
#4041=FACE_OUTER_BOUND('',#5905,.T.);
#4042=FACE_OUTER_BOUND('',#5906,.T.);
#4043=FACE_OUTER_BOUND('',#5907,.T.);
#4044=FACE_OUTER_BOUND('',#5908,.T.);
#4045=FACE_OUTER_BOUND('',#5909,.T.);
#4046=FACE_OUTER_BOUND('',#5910,.T.);
#4047=FACE_OUTER_BOUND('',#5911,.T.);
#4048=FACE_OUTER_BOUND('',#5912,.T.);
#4049=FACE_OUTER_BOUND('',#5913,.T.);
#4050=FACE_OUTER_BOUND('',#5914,.T.);
#4051=FACE_OUTER_BOUND('',#5915,.T.);
#4052=FACE_OUTER_BOUND('',#5916,.T.);
#4053=FACE_OUTER_BOUND('',#5917,.T.);
#4054=FACE_OUTER_BOUND('',#5918,.T.);
#4055=FACE_OUTER_BOUND('',#5919,.T.);
#4056=FACE_OUTER_BOUND('',#5920,.T.);
#4057=FACE_OUTER_BOUND('',#5921,.T.);
#4058=FACE_OUTER_BOUND('',#5922,.T.);
#4059=FACE_OUTER_BOUND('',#5923,.T.);
#4060=FACE_OUTER_BOUND('',#5924,.T.);
#4061=FACE_OUTER_BOUND('',#5925,.T.);
#4062=FACE_OUTER_BOUND('',#5926,.T.);
#4063=FACE_OUTER_BOUND('',#5927,.T.);
#4064=FACE_OUTER_BOUND('',#5928,.T.);
#4065=FACE_OUTER_BOUND('',#5929,.T.);
#4066=FACE_OUTER_BOUND('',#5930,.T.);
#4067=FACE_OUTER_BOUND('',#5931,.T.);
#4068=FACE_OUTER_BOUND('',#5932,.T.);
#4069=FACE_OUTER_BOUND('',#5933,.T.);
#4070=FACE_OUTER_BOUND('',#5934,.T.);
#4071=FACE_OUTER_BOUND('',#5935,.T.);
#4072=FACE_OUTER_BOUND('',#5936,.T.);
#4073=FACE_OUTER_BOUND('',#5937,.T.);
#4074=FACE_OUTER_BOUND('',#5938,.T.);
#4075=FACE_OUTER_BOUND('',#5939,.T.);
#4076=FACE_OUTER_BOUND('',#5940,.T.);
#4077=FACE_OUTER_BOUND('',#5941,.T.);
#4078=FACE_OUTER_BOUND('',#5942,.T.);
#4079=FACE_OUTER_BOUND('',#5943,.T.);
#4080=FACE_OUTER_BOUND('',#5944,.T.);
#4081=FACE_OUTER_BOUND('',#5987,.T.);
#4082=FACE_OUTER_BOUND('',#5988,.T.);
#4083=FACE_OUTER_BOUND('',#5989,.T.);
#4084=FACE_OUTER_BOUND('',#5990,.T.);
#4085=FACE_OUTER_BOUND('',#5991,.T.);
#4086=FACE_OUTER_BOUND('',#5992,.T.);
#4087=FACE_OUTER_BOUND('',#5993,.T.);
#4088=FACE_OUTER_BOUND('',#5994,.T.);
#4089=FACE_OUTER_BOUND('',#5995,.T.);
#4090=FACE_OUTER_BOUND('',#5996,.T.);
#4091=FACE_OUTER_BOUND('',#5997,.T.);
#4092=FACE_OUTER_BOUND('',#5998,.T.);
#4093=FACE_OUTER_BOUND('',#5999,.T.);
#4094=FACE_OUTER_BOUND('',#6000,.T.);
#4095=FACE_OUTER_BOUND('',#6001,.T.);
#4096=FACE_OUTER_BOUND('',#6002,.T.);
#4097=FACE_OUTER_BOUND('',#6003,.T.);
#4098=FACE_OUTER_BOUND('',#6004,.T.);
#4099=FACE_OUTER_BOUND('',#6005,.T.);
#4100=FACE_OUTER_BOUND('',#6006,.T.);
#4101=FACE_OUTER_BOUND('',#6007,.T.);
#4102=FACE_OUTER_BOUND('',#6008,.T.);
#4103=FACE_OUTER_BOUND('',#6009,.T.);
#4104=FACE_OUTER_BOUND('',#6010,.T.);
#4105=FACE_OUTER_BOUND('',#6011,.T.);
#4106=FACE_OUTER_BOUND('',#6012,.T.);
#4107=FACE_OUTER_BOUND('',#6013,.T.);
#4108=FACE_OUTER_BOUND('',#6014,.T.);
#4109=FACE_OUTER_BOUND('',#6015,.T.);
#4110=FACE_OUTER_BOUND('',#6016,.T.);
#4111=FACE_OUTER_BOUND('',#6017,.T.);
#4112=FACE_OUTER_BOUND('',#6018,.T.);
#4113=FACE_OUTER_BOUND('',#6019,.T.);
#4114=FACE_OUTER_BOUND('',#6020,.T.);
#4115=FACE_OUTER_BOUND('',#6021,.T.);
#4116=FACE_OUTER_BOUND('',#6022,.T.);
#4117=FACE_OUTER_BOUND('',#6023,.T.);
#4118=FACE_OUTER_BOUND('',#6024,.T.);
#4119=FACE_OUTER_BOUND('',#6025,.T.);
#4120=FACE_OUTER_BOUND('',#6026,.T.);
#4121=FACE_OUTER_BOUND('',#6027,.T.);
#4122=FACE_OUTER_BOUND('',#6028,.T.);
#4123=FACE_OUTER_BOUND('',#6029,.T.);
#4124=FACE_OUTER_BOUND('',#6030,.T.);
#4125=FACE_OUTER_BOUND('',#6031,.T.);
#4126=FACE_OUTER_BOUND('',#6032,.T.);
#4127=FACE_OUTER_BOUND('',#6033,.T.);
#4128=FACE_OUTER_BOUND('',#6034,.T.);
#4129=FACE_OUTER_BOUND('',#6035,.T.);
#4130=FACE_OUTER_BOUND('',#6036,.T.);
#4131=FACE_OUTER_BOUND('',#6037,.T.);
#4132=FACE_OUTER_BOUND('',#6038,.T.);
#4133=FACE_OUTER_BOUND('',#6039,.T.);
#4134=FACE_OUTER_BOUND('',#6040,.T.);
#4135=FACE_OUTER_BOUND('',#6041,.T.);
#4136=FACE_OUTER_BOUND('',#6042,.T.);
#4137=FACE_OUTER_BOUND('',#6043,.T.);
#4138=FACE_OUTER_BOUND('',#6044,.T.);
#4139=FACE_OUTER_BOUND('',#6045,.T.);
#4140=FACE_OUTER_BOUND('',#6046,.T.);
#4141=FACE_OUTER_BOUND('',#6047,.T.);
#4142=FACE_OUTER_BOUND('',#6048,.T.);
#4143=FACE_OUTER_BOUND('',#6049,.T.);
#4144=FACE_OUTER_BOUND('',#6050,.T.);
#4145=FACE_OUTER_BOUND('',#6051,.T.);
#4146=FACE_OUTER_BOUND('',#6052,.T.);
#4147=FACE_OUTER_BOUND('',#6053,.T.);
#4148=FACE_OUTER_BOUND('',#6054,.T.);
#4149=FACE_OUTER_BOUND('',#6055,.T.);
#4150=FACE_OUTER_BOUND('',#6056,.T.);
#4151=FACE_OUTER_BOUND('',#6057,.T.);
#4152=FACE_OUTER_BOUND('',#6060,.T.);
#4153=FACE_OUTER_BOUND('',#6063,.T.);
#4154=FACE_OUTER_BOUND('',#6064,.T.);
#4155=FACE_OUTER_BOUND('',#6065,.T.);
#4156=FACE_OUTER_BOUND('',#6066,.T.);
#4157=FACE_OUTER_BOUND('',#6067,.T.);
#4158=FACE_OUTER_BOUND('',#6068,.T.);
#4159=FACE_OUTER_BOUND('',#6069,.T.);
#4160=FACE_OUTER_BOUND('',#6070,.T.);
#4161=FACE_OUTER_BOUND('',#6072,.T.);
#4162=FACE_OUTER_BOUND('',#6074,.T.);
#4163=FACE_OUTER_BOUND('',#6076,.T.);
#4164=FACE_OUTER_BOUND('',#6078,.T.);
#4165=FACE_OUTER_BOUND('',#6079,.T.);
#4166=FACE_OUTER_BOUND('',#6080,.T.);
#4167=FACE_OUTER_BOUND('',#6081,.T.);
#4168=FACE_OUTER_BOUND('',#6082,.T.);
#4169=FACE_OUTER_BOUND('',#6083,.T.);
#4170=FACE_OUTER_BOUND('',#6085,.T.);
#4171=FACE_OUTER_BOUND('',#6086,.T.);
#4172=FACE_OUTER_BOUND('',#6087,.T.);
#4173=FACE_OUTER_BOUND('',#6088,.T.);
#4174=FACE_OUTER_BOUND('',#6089,.T.);
#4175=FACE_OUTER_BOUND('',#6090,.T.);
#4176=FACE_OUTER_BOUND('',#6092,.T.);
#4177=FACE_OUTER_BOUND('',#6093,.T.);
#4178=FACE_OUTER_BOUND('',#6094,.T.);
#4179=FACE_OUTER_BOUND('',#6095,.T.);
#4180=FACE_OUTER_BOUND('',#6097,.T.);
#4181=FACE_OUTER_BOUND('',#6098,.T.);
#4182=FACE_OUTER_BOUND('',#6099,.T.);
#4183=FACE_OUTER_BOUND('',#6100,.T.);
#4184=FACE_OUTER_BOUND('',#6101,.T.);
#4185=FACE_OUTER_BOUND('',#6102,.T.);
#4186=FACE_OUTER_BOUND('',#6103,.T.);
#4187=FACE_OUTER_BOUND('',#6104,.T.);
#4188=FACE_OUTER_BOUND('',#6105,.T.);
#4189=FACE_OUTER_BOUND('',#6106,.T.);
#4190=FACE_OUTER_BOUND('',#6107,.T.);
#4191=FACE_OUTER_BOUND('',#6108,.T.);
#4192=FACE_OUTER_BOUND('',#6109,.T.);
#4193=FACE_OUTER_BOUND('',#6110,.T.);
#4194=FACE_OUTER_BOUND('',#6111,.T.);
#4195=FACE_OUTER_BOUND('',#6112,.T.);
#4196=FACE_OUTER_BOUND('',#6113,.T.);
#4197=FACE_OUTER_BOUND('',#6114,.T.);
#4198=FACE_OUTER_BOUND('',#6115,.T.);
#4199=FACE_OUTER_BOUND('',#6116,.T.);
#4200=FACE_OUTER_BOUND('',#6117,.T.);
#4201=FACE_OUTER_BOUND('',#6118,.T.);
#4202=FACE_OUTER_BOUND('',#6119,.T.);
#4203=FACE_OUTER_BOUND('',#6120,.T.);
#4204=FACE_OUTER_BOUND('',#6121,.T.);
#4205=FACE_OUTER_BOUND('',#6122,.T.);
#4206=FACE_OUTER_BOUND('',#6123,.T.);
#4207=FACE_OUTER_BOUND('',#6124,.T.);
#4208=FACE_OUTER_BOUND('',#6125,.T.);
#4209=FACE_OUTER_BOUND('',#6126,.T.);
#4210=FACE_OUTER_BOUND('',#6127,.T.);
#4211=FACE_OUTER_BOUND('',#6128,.T.);
#4212=FACE_OUTER_BOUND('',#6129,.T.);
#4213=FACE_OUTER_BOUND('',#6130,.T.);
#4214=FACE_OUTER_BOUND('',#6131,.T.);
#4215=FACE_OUTER_BOUND('',#6132,.T.);
#4216=FACE_OUTER_BOUND('',#6133,.T.);
#4217=FACE_OUTER_BOUND('',#6134,.T.);
#4218=FACE_OUTER_BOUND('',#6135,.T.);
#4219=FACE_OUTER_BOUND('',#6136,.T.);
#4220=FACE_OUTER_BOUND('',#6137,.T.);
#4221=FACE_OUTER_BOUND('',#6138,.T.);
#4222=FACE_OUTER_BOUND('',#6139,.T.);
#4223=FACE_OUTER_BOUND('',#6140,.T.);
#4224=FACE_OUTER_BOUND('',#6141,.T.);
#4225=FACE_OUTER_BOUND('',#6142,.T.);
#4226=FACE_OUTER_BOUND('',#6143,.T.);
#4227=FACE_OUTER_BOUND('',#6144,.T.);
#4228=FACE_OUTER_BOUND('',#6145,.T.);
#4229=FACE_OUTER_BOUND('',#6146,.T.);
#4230=FACE_OUTER_BOUND('',#6147,.T.);
#4231=FACE_OUTER_BOUND('',#6148,.T.);
#4232=FACE_OUTER_BOUND('',#6149,.T.);
#4233=FACE_OUTER_BOUND('',#6150,.T.);
#4234=FACE_OUTER_BOUND('',#6151,.T.);
#4235=FACE_OUTER_BOUND('',#6152,.T.);
#4236=FACE_OUTER_BOUND('',#6153,.T.);
#4237=FACE_OUTER_BOUND('',#6154,.T.);
#4238=FACE_OUTER_BOUND('',#6155,.T.);
#4239=FACE_OUTER_BOUND('',#6156,.T.);
#4240=FACE_OUTER_BOUND('',#6157,.T.);
#4241=FACE_OUTER_BOUND('',#6158,.T.);
#4242=FACE_OUTER_BOUND('',#6159,.T.);
#4243=FACE_OUTER_BOUND('',#6160,.T.);
#4244=FACE_OUTER_BOUND('',#6161,.T.);
#4245=FACE_OUTER_BOUND('',#6162,.T.);
#4246=FACE_OUTER_BOUND('',#6163,.T.);
#4247=FACE_OUTER_BOUND('',#6164,.T.);
#4248=FACE_OUTER_BOUND('',#6165,.T.);
#4249=FACE_OUTER_BOUND('',#6166,.T.);
#4250=FACE_OUTER_BOUND('',#6167,.T.);
#4251=FACE_OUTER_BOUND('',#6168,.T.);
#4252=FACE_OUTER_BOUND('',#6169,.T.);
#4253=FACE_OUTER_BOUND('',#6170,.T.);
#4254=FACE_OUTER_BOUND('',#6171,.T.);
#4255=FACE_OUTER_BOUND('',#6172,.T.);
#4256=FACE_OUTER_BOUND('',#6173,.T.);
#4257=FACE_OUTER_BOUND('',#6174,.T.);
#4258=FACE_OUTER_BOUND('',#6175,.T.);
#4259=FACE_OUTER_BOUND('',#6176,.T.);
#4260=FACE_OUTER_BOUND('',#6177,.T.);
#4261=FACE_OUTER_BOUND('',#6178,.T.);
#4262=FACE_OUTER_BOUND('',#6179,.T.);
#4263=FACE_OUTER_BOUND('',#6180,.T.);
#4264=FACE_OUTER_BOUND('',#6181,.T.);
#4265=FACE_OUTER_BOUND('',#6182,.T.);
#4266=FACE_OUTER_BOUND('',#6183,.T.);
#4267=FACE_OUTER_BOUND('',#6184,.T.);
#4268=FACE_OUTER_BOUND('',#6185,.T.);
#4269=FACE_OUTER_BOUND('',#6186,.T.);
#4270=FACE_OUTER_BOUND('',#6187,.T.);
#4271=FACE_OUTER_BOUND('',#6188,.T.);
#4272=FACE_OUTER_BOUND('',#6189,.T.);
#4273=FACE_OUTER_BOUND('',#6190,.T.);
#4274=FACE_OUTER_BOUND('',#6191,.T.);
#4275=FACE_OUTER_BOUND('',#6192,.T.);
#4276=FACE_OUTER_BOUND('',#6193,.T.);
#4277=FACE_OUTER_BOUND('',#6194,.T.);
#4278=FACE_OUTER_BOUND('',#6195,.T.);
#4279=FACE_OUTER_BOUND('',#6196,.T.);
#4280=FACE_OUTER_BOUND('',#6197,.T.);
#4281=FACE_OUTER_BOUND('',#6198,.T.);
#4282=FACE_OUTER_BOUND('',#6199,.T.);
#4283=FACE_OUTER_BOUND('',#6200,.T.);
#4284=FACE_OUTER_BOUND('',#6201,.T.);
#4285=FACE_OUTER_BOUND('',#6202,.T.);
#4286=FACE_OUTER_BOUND('',#6203,.T.);
#4287=FACE_OUTER_BOUND('',#6204,.T.);
#4288=FACE_OUTER_BOUND('',#6205,.T.);
#4289=FACE_OUTER_BOUND('',#6206,.T.);
#4290=FACE_OUTER_BOUND('',#6207,.T.);
#4291=FACE_OUTER_BOUND('',#6208,.T.);
#4292=FACE_OUTER_BOUND('',#6209,.T.);
#4293=FACE_OUTER_BOUND('',#6210,.T.);
#4294=FACE_OUTER_BOUND('',#6211,.T.);
#4295=FACE_OUTER_BOUND('',#6212,.T.);
#4296=FACE_OUTER_BOUND('',#6213,.T.);
#4297=FACE_OUTER_BOUND('',#6214,.T.);
#4298=FACE_OUTER_BOUND('',#6215,.T.);
#4299=FACE_OUTER_BOUND('',#6216,.T.);
#4300=FACE_OUTER_BOUND('',#6217,.T.);
#4301=FACE_OUTER_BOUND('',#6218,.T.);
#4302=FACE_OUTER_BOUND('',#6219,.T.);
#4303=FACE_OUTER_BOUND('',#6220,.T.);
#4304=FACE_OUTER_BOUND('',#6221,.T.);
#4305=FACE_OUTER_BOUND('',#6222,.T.);
#4306=FACE_OUTER_BOUND('',#6223,.T.);
#4307=FACE_OUTER_BOUND('',#6224,.T.);
#4308=FACE_OUTER_BOUND('',#6225,.T.);
#4309=FACE_OUTER_BOUND('',#6226,.T.);
#4310=FACE_OUTER_BOUND('',#6227,.T.);
#4311=FACE_OUTER_BOUND('',#6228,.T.);
#4312=FACE_OUTER_BOUND('',#6229,.T.);
#4313=FACE_OUTER_BOUND('',#6230,.T.);
#4314=FACE_OUTER_BOUND('',#6231,.T.);
#4315=FACE_OUTER_BOUND('',#6232,.T.);
#4316=FACE_OUTER_BOUND('',#6233,.T.);
#4317=FACE_OUTER_BOUND('',#6234,.T.);
#4318=FACE_OUTER_BOUND('',#6235,.T.);
#4319=FACE_OUTER_BOUND('',#6236,.T.);
#4320=FACE_OUTER_BOUND('',#6237,.T.);
#4321=FACE_OUTER_BOUND('',#6238,.T.);
#4322=FACE_OUTER_BOUND('',#6239,.T.);
#4323=FACE_OUTER_BOUND('',#6240,.T.);
#4324=FACE_OUTER_BOUND('',#6241,.T.);
#4325=FACE_OUTER_BOUND('',#6242,.T.);
#4326=FACE_OUTER_BOUND('',#6243,.T.);
#4327=FACE_OUTER_BOUND('',#6244,.T.);
#4328=FACE_OUTER_BOUND('',#6245,.T.);
#4329=FACE_OUTER_BOUND('',#6246,.T.);
#4330=FACE_OUTER_BOUND('',#6247,.T.);
#4331=FACE_OUTER_BOUND('',#6248,.T.);
#4332=FACE_OUTER_BOUND('',#6249,.T.);
#4333=FACE_OUTER_BOUND('',#6250,.T.);
#4334=FACE_OUTER_BOUND('',#6251,.T.);
#4335=FACE_OUTER_BOUND('',#6252,.T.);
#4336=FACE_OUTER_BOUND('',#6253,.T.);
#4337=FACE_OUTER_BOUND('',#6254,.T.);
#4338=FACE_OUTER_BOUND('',#6255,.T.);
#4339=FACE_OUTER_BOUND('',#6256,.T.);
#4340=FACE_OUTER_BOUND('',#6257,.T.);
#4341=FACE_OUTER_BOUND('',#6258,.T.);
#4342=FACE_OUTER_BOUND('',#6259,.T.);
#4343=FACE_OUTER_BOUND('',#6260,.T.);
#4344=FACE_OUTER_BOUND('',#6261,.T.);
#4345=FACE_OUTER_BOUND('',#6262,.T.);
#4346=FACE_OUTER_BOUND('',#6263,.T.);
#4347=FACE_OUTER_BOUND('',#6264,.T.);
#4348=FACE_OUTER_BOUND('',#6265,.T.);
#4349=FACE_OUTER_BOUND('',#6266,.T.);
#4350=FACE_OUTER_BOUND('',#6267,.T.);
#4351=FACE_OUTER_BOUND('',#6268,.T.);
#4352=FACE_OUTER_BOUND('',#6269,.T.);
#4353=FACE_OUTER_BOUND('',#6270,.T.);
#4354=FACE_OUTER_BOUND('',#6271,.T.);
#4355=FACE_OUTER_BOUND('',#6272,.T.);
#4356=FACE_OUTER_BOUND('',#6273,.T.);
#4357=FACE_OUTER_BOUND('',#6274,.T.);
#4358=FACE_OUTER_BOUND('',#6275,.T.);
#4359=FACE_OUTER_BOUND('',#6277,.T.);
#4360=FACE_OUTER_BOUND('',#6278,.T.);
#4361=FACE_OUTER_BOUND('',#6279,.T.);
#4362=FACE_OUTER_BOUND('',#6281,.T.);
#4363=FACE_OUTER_BOUND('',#6282,.T.);
#4364=FACE_OUTER_BOUND('',#6283,.T.);
#4365=FACE_OUTER_BOUND('',#6284,.T.);
#4366=FACE_OUTER_BOUND('',#6285,.T.);
#4367=FACE_OUTER_BOUND('',#6286,.T.);
#4368=FACE_OUTER_BOUND('',#6288,.T.);
#4369=FACE_OUTER_BOUND('',#6324,.T.);
#4370=FACE_OUTER_BOUND('',#6325,.T.);
#4371=FACE_OUTER_BOUND('',#6327,.T.);
#4372=FACE_OUTER_BOUND('',#6328,.T.);
#4373=FACE_OUTER_BOUND('',#6330,.T.);
#4374=FACE_OUTER_BOUND('',#6331,.T.);
#4375=FACE_OUTER_BOUND('',#6333,.T.);
#4376=FACE_OUTER_BOUND('',#6334,.T.);
#4377=FACE_OUTER_BOUND('',#6335,.T.);
#4378=FACE_OUTER_BOUND('',#6336,.T.);
#4379=FACE_OUTER_BOUND('',#6337,.T.);
#4380=FACE_OUTER_BOUND('',#6338,.T.);
#4381=FACE_OUTER_BOUND('',#6339,.T.);
#4382=FACE_OUTER_BOUND('',#6340,.T.);
#4383=FACE_OUTER_BOUND('',#6341,.T.);
#4384=FACE_OUTER_BOUND('',#6342,.T.);
#4385=FACE_OUTER_BOUND('',#6343,.T.);
#4386=FACE_OUTER_BOUND('',#6344,.T.);
#4387=FACE_OUTER_BOUND('',#6346,.T.);
#4388=FACE_OUTER_BOUND('',#6347,.T.);
#4389=FACE_OUTER_BOUND('',#6349,.T.);
#4390=FACE_OUTER_BOUND('',#6350,.T.);
#4391=FACE_OUTER_BOUND('',#6351,.T.);
#4392=FACE_OUTER_BOUND('',#6352,.T.);
#4393=FACE_OUTER_BOUND('',#6353,.T.);
#4394=FACE_OUTER_BOUND('',#6354,.T.);
#4395=FACE_OUTER_BOUND('',#6355,.T.);
#4396=FACE_OUTER_BOUND('',#6356,.T.);
#4397=FACE_OUTER_BOUND('',#6357,.T.);
#4398=FACE_OUTER_BOUND('',#6358,.T.);
#4399=FACE_OUTER_BOUND('',#6359,.T.);
#4400=FACE_OUTER_BOUND('',#6360,.T.);
#4401=FACE_OUTER_BOUND('',#6361,.T.);
#4402=FACE_OUTER_BOUND('',#6362,.T.);
#4403=FACE_OUTER_BOUND('',#6363,.T.);
#4404=FACE_OUTER_BOUND('',#6364,.T.);
#4405=FACE_OUTER_BOUND('',#6365,.T.);
#4406=FACE_OUTER_BOUND('',#6366,.T.);
#4407=FACE_OUTER_BOUND('',#6367,.T.);
#4408=FACE_OUTER_BOUND('',#6368,.T.);
#4409=FACE_OUTER_BOUND('',#6369,.T.);
#4410=FACE_OUTER_BOUND('',#6370,.T.);
#4411=FACE_OUTER_BOUND('',#6371,.T.);
#4412=FACE_OUTER_BOUND('',#6372,.T.);
#4413=FACE_OUTER_BOUND('',#6373,.T.);
#4414=FACE_OUTER_BOUND('',#6374,.T.);
#4415=FACE_OUTER_BOUND('',#6375,.T.);
#4416=FACE_OUTER_BOUND('',#6376,.T.);
#4417=FACE_OUTER_BOUND('',#6377,.T.);
#4418=FACE_OUTER_BOUND('',#6378,.T.);
#4419=FACE_OUTER_BOUND('',#6379,.T.);
#4420=FACE_OUTER_BOUND('',#6380,.T.);
#4421=FACE_OUTER_BOUND('',#6381,.T.);
#4422=FACE_OUTER_BOUND('',#6382,.T.);
#4423=FACE_OUTER_BOUND('',#6383,.T.);
#4424=FACE_OUTER_BOUND('',#6384,.T.);
#4425=FACE_OUTER_BOUND('',#6385,.T.);
#4426=FACE_OUTER_BOUND('',#6386,.T.);
#4427=FACE_OUTER_BOUND('',#6387,.T.);
#4428=FACE_OUTER_BOUND('',#6388,.T.);
#4429=FACE_OUTER_BOUND('',#6389,.T.);
#4430=FACE_OUTER_BOUND('',#6390,.T.);
#4431=FACE_OUTER_BOUND('',#6391,.T.);
#4432=FACE_OUTER_BOUND('',#6392,.T.);
#4433=FACE_OUTER_BOUND('',#6393,.T.);
#4434=FACE_OUTER_BOUND('',#6394,.T.);
#4435=FACE_OUTER_BOUND('',#6395,.T.);
#4436=FACE_OUTER_BOUND('',#6396,.T.);
#4437=FACE_OUTER_BOUND('',#6397,.T.);
#4438=FACE_OUTER_BOUND('',#6398,.T.);
#4439=FACE_OUTER_BOUND('',#6399,.T.);
#4440=FACE_OUTER_BOUND('',#6400,.T.);
#4441=FACE_OUTER_BOUND('',#6401,.T.);
#4442=FACE_OUTER_BOUND('',#6402,.T.);
#4443=FACE_OUTER_BOUND('',#6403,.T.);
#4444=FACE_OUTER_BOUND('',#6404,.T.);
#4445=FACE_OUTER_BOUND('',#6405,.T.);
#4446=FACE_OUTER_BOUND('',#6406,.T.);
#4447=FACE_OUTER_BOUND('',#6407,.T.);
#4448=FACE_OUTER_BOUND('',#6408,.T.);
#4449=FACE_OUTER_BOUND('',#6409,.T.);
#4450=FACE_OUTER_BOUND('',#6410,.T.);
#4451=FACE_OUTER_BOUND('',#6411,.T.);
#4452=FACE_OUTER_BOUND('',#6412,.T.);
#4453=FACE_OUTER_BOUND('',#6413,.T.);
#4454=FACE_OUTER_BOUND('',#6414,.T.);
#4455=FACE_OUTER_BOUND('',#6415,.T.);
#4456=FACE_OUTER_BOUND('',#6416,.T.);
#4457=FACE_OUTER_BOUND('',#6417,.T.);
#4458=FACE_OUTER_BOUND('',#6418,.T.);
#4459=FACE_OUTER_BOUND('',#6419,.T.);
#4460=FACE_OUTER_BOUND('',#6420,.T.);
#4461=FACE_OUTER_BOUND('',#6421,.T.);
#4462=FACE_OUTER_BOUND('',#6422,.T.);
#4463=FACE_OUTER_BOUND('',#6423,.T.);
#4464=FACE_OUTER_BOUND('',#6424,.T.);
#4465=FACE_OUTER_BOUND('',#6425,.T.);
#4466=FACE_OUTER_BOUND('',#6426,.T.);
#4467=FACE_OUTER_BOUND('',#6427,.T.);
#4468=FACE_OUTER_BOUND('',#6428,.T.);
#4469=FACE_OUTER_BOUND('',#6429,.T.);
#4470=FACE_OUTER_BOUND('',#6430,.T.);
#4471=FACE_OUTER_BOUND('',#6431,.T.);
#4472=FACE_OUTER_BOUND('',#6432,.T.);
#4473=FACE_OUTER_BOUND('',#6433,.T.);
#4474=FACE_OUTER_BOUND('',#6434,.T.);
#4475=FACE_OUTER_BOUND('',#6435,.T.);
#4476=FACE_OUTER_BOUND('',#6436,.T.);
#4477=FACE_OUTER_BOUND('',#6437,.T.);
#4478=FACE_OUTER_BOUND('',#6438,.T.);
#4479=FACE_OUTER_BOUND('',#6439,.T.);
#4480=FACE_OUTER_BOUND('',#6440,.T.);
#4481=FACE_OUTER_BOUND('',#6441,.T.);
#4482=FACE_OUTER_BOUND('',#6443,.T.);
#4483=FACE_OUTER_BOUND('',#6444,.T.);
#4484=FACE_OUTER_BOUND('',#6445,.T.);
#4485=FACE_OUTER_BOUND('',#6446,.T.);
#4486=FACE_OUTER_BOUND('',#6447,.T.);
#4487=FACE_OUTER_BOUND('',#6448,.T.);
#4488=FACE_OUTER_BOUND('',#6449,.T.);
#4489=FACE_OUTER_BOUND('',#6450,.T.);
#4490=FACE_OUTER_BOUND('',#6451,.T.);
#4491=FACE_OUTER_BOUND('',#6452,.T.);
#4492=FACE_OUTER_BOUND('',#6453,.T.);
#4493=FACE_OUTER_BOUND('',#6454,.T.);
#4494=FACE_OUTER_BOUND('',#6455,.T.);
#4495=FACE_OUTER_BOUND('',#6456,.T.);
#4496=FACE_OUTER_BOUND('',#6457,.T.);
#4497=FACE_OUTER_BOUND('',#6458,.T.);
#4498=FACE_OUTER_BOUND('',#6459,.T.);
#4499=FACE_OUTER_BOUND('',#6460,.T.);
#4500=FACE_OUTER_BOUND('',#6461,.T.);
#4501=FACE_OUTER_BOUND('',#6462,.T.);
#4502=FACE_OUTER_BOUND('',#6463,.T.);
#4503=FACE_OUTER_BOUND('',#6464,.T.);
#4504=FACE_OUTER_BOUND('',#6465,.T.);
#4505=FACE_OUTER_BOUND('',#6466,.T.);
#4506=FACE_OUTER_BOUND('',#6467,.T.);
#4507=FACE_OUTER_BOUND('',#6468,.T.);
#4508=FACE_OUTER_BOUND('',#6469,.T.);
#4509=FACE_OUTER_BOUND('',#6470,.T.);
#4510=FACE_OUTER_BOUND('',#6471,.T.);
#4511=FACE_OUTER_BOUND('',#6472,.T.);
#4512=FACE_OUTER_BOUND('',#6473,.T.);
#4513=FACE_OUTER_BOUND('',#6474,.T.);
#4514=FACE_OUTER_BOUND('',#6475,.T.);
#4515=FACE_OUTER_BOUND('',#6476,.T.);
#4516=FACE_OUTER_BOUND('',#6477,.T.);
#4517=FACE_OUTER_BOUND('',#6478,.T.);
#4518=FACE_OUTER_BOUND('',#6479,.T.);
#4519=FACE_OUTER_BOUND('',#6480,.T.);
#4520=FACE_OUTER_BOUND('',#6481,.T.);
#4521=FACE_OUTER_BOUND('',#6482,.T.);
#4522=FACE_OUTER_BOUND('',#6483,.T.);
#4523=FACE_OUTER_BOUND('',#6484,.T.);
#4524=FACE_OUTER_BOUND('',#6485,.T.);
#4525=FACE_OUTER_BOUND('',#6486,.T.);
#4526=FACE_OUTER_BOUND('',#6487,.T.);
#4527=FACE_OUTER_BOUND('',#6488,.T.);
#4528=FACE_OUTER_BOUND('',#6489,.T.);
#4529=FACE_OUTER_BOUND('',#6490,.T.);
#4530=FACE_OUTER_BOUND('',#6491,.T.);
#4531=FACE_OUTER_BOUND('',#6492,.T.);
#4532=FACE_OUTER_BOUND('',#6493,.T.);
#4533=FACE_OUTER_BOUND('',#6494,.T.);
#4534=FACE_OUTER_BOUND('',#6495,.T.);
#4535=FACE_OUTER_BOUND('',#6496,.T.);
#4536=FACE_OUTER_BOUND('',#6497,.T.);
#4537=FACE_OUTER_BOUND('',#6498,.T.);
#4538=FACE_OUTER_BOUND('',#6499,.T.);
#4539=FACE_OUTER_BOUND('',#6500,.T.);
#4540=FACE_OUTER_BOUND('',#6501,.T.);
#4541=FACE_OUTER_BOUND('',#6502,.T.);
#4542=FACE_OUTER_BOUND('',#6503,.T.);
#4543=FACE_OUTER_BOUND('',#6504,.T.);
#4544=FACE_OUTER_BOUND('',#6505,.T.);
#4545=FACE_OUTER_BOUND('',#6506,.T.);
#4546=FACE_OUTER_BOUND('',#6507,.T.);
#4547=FACE_OUTER_BOUND('',#6508,.T.);
#4548=FACE_OUTER_BOUND('',#6509,.T.);
#4549=FACE_OUTER_BOUND('',#6510,.T.);
#4550=FACE_OUTER_BOUND('',#6511,.T.);
#4551=FACE_OUTER_BOUND('',#6512,.T.);
#4552=FACE_OUTER_BOUND('',#6513,.T.);
#4553=FACE_OUTER_BOUND('',#6514,.T.);
#4554=FACE_OUTER_BOUND('',#6515,.T.);
#4555=FACE_OUTER_BOUND('',#6516,.T.);
#4556=FACE_OUTER_BOUND('',#6517,.T.);
#4557=FACE_OUTER_BOUND('',#6518,.T.);
#4558=FACE_OUTER_BOUND('',#6519,.T.);
#4559=FACE_OUTER_BOUND('',#6520,.T.);
#4560=FACE_OUTER_BOUND('',#6521,.T.);
#4561=FACE_OUTER_BOUND('',#6522,.T.);
#4562=FACE_OUTER_BOUND('',#6523,.T.);
#4563=FACE_OUTER_BOUND('',#6524,.T.);
#4564=FACE_OUTER_BOUND('',#6525,.T.);
#4565=FACE_OUTER_BOUND('',#6526,.T.);
#4566=FACE_OUTER_BOUND('',#6527,.T.);
#4567=FACE_OUTER_BOUND('',#6528,.T.);
#4568=FACE_OUTER_BOUND('',#6529,.T.);
#4569=FACE_OUTER_BOUND('',#6530,.T.);
#4570=FACE_OUTER_BOUND('',#6531,.T.);
#4571=FACE_OUTER_BOUND('',#6532,.T.);
#4572=FACE_OUTER_BOUND('',#6533,.T.);
#4573=FACE_OUTER_BOUND('',#6534,.T.);
#4574=FACE_OUTER_BOUND('',#6535,.T.);
#4575=FACE_OUTER_BOUND('',#6536,.T.);
#4576=FACE_OUTER_BOUND('',#6537,.T.);
#4577=FACE_OUTER_BOUND('',#6538,.T.);
#4578=FACE_OUTER_BOUND('',#6539,.T.);
#4579=FACE_OUTER_BOUND('',#6540,.T.);
#4580=FACE_OUTER_BOUND('',#6541,.T.);
#4581=FACE_OUTER_BOUND('',#6542,.T.);
#4582=FACE_OUTER_BOUND('',#6543,.T.);
#4583=FACE_OUTER_BOUND('',#6544,.T.);
#4584=FACE_OUTER_BOUND('',#6545,.T.);
#4585=FACE_OUTER_BOUND('',#6546,.T.);
#4586=FACE_OUTER_BOUND('',#6547,.T.);
#4587=FACE_OUTER_BOUND('',#6548,.T.);
#4588=FACE_OUTER_BOUND('',#6549,.T.);
#4589=FACE_OUTER_BOUND('',#6550,.T.);
#4590=FACE_OUTER_BOUND('',#6551,.T.);
#4591=FACE_OUTER_BOUND('',#6552,.T.);
#4592=FACE_OUTER_BOUND('',#6553,.T.);
#4593=FACE_OUTER_BOUND('',#6554,.T.);
#4594=FACE_OUTER_BOUND('',#6555,.T.);
#4595=FACE_OUTER_BOUND('',#6556,.T.);
#4596=FACE_OUTER_BOUND('',#6557,.T.);
#4597=FACE_OUTER_BOUND('',#6558,.T.);
#4598=FACE_OUTER_BOUND('',#6559,.T.);
#4599=FACE_OUTER_BOUND('',#6560,.T.);
#4600=FACE_OUTER_BOUND('',#6561,.T.);
#4601=FACE_OUTER_BOUND('',#6562,.T.);
#4602=FACE_OUTER_BOUND('',#6563,.T.);
#4603=FACE_OUTER_BOUND('',#6564,.T.);
#4604=FACE_OUTER_BOUND('',#6565,.T.);
#4605=FACE_OUTER_BOUND('',#6566,.T.);
#4606=FACE_OUTER_BOUND('',#6567,.T.);
#4607=FACE_OUTER_BOUND('',#6568,.T.);
#4608=FACE_OUTER_BOUND('',#6569,.T.);
#4609=FACE_OUTER_BOUND('',#6570,.T.);
#4610=FACE_OUTER_BOUND('',#6571,.T.);
#4611=FACE_OUTER_BOUND('',#6572,.T.);
#4612=FACE_OUTER_BOUND('',#6573,.T.);
#4613=FACE_OUTER_BOUND('',#6574,.T.);
#4614=FACE_OUTER_BOUND('',#6575,.T.);
#4615=FACE_OUTER_BOUND('',#6576,.T.);
#4616=FACE_OUTER_BOUND('',#6577,.T.);
#4617=FACE_OUTER_BOUND('',#6578,.T.);
#4618=FACE_OUTER_BOUND('',#6579,.T.);
#4619=FACE_OUTER_BOUND('',#6580,.T.);
#4620=FACE_OUTER_BOUND('',#6581,.T.);
#4621=FACE_OUTER_BOUND('',#6582,.T.);
#4622=FACE_OUTER_BOUND('',#6583,.T.);
#4623=FACE_OUTER_BOUND('',#6584,.T.);
#4624=FACE_OUTER_BOUND('',#6585,.T.);
#4625=FACE_OUTER_BOUND('',#6586,.T.);
#4626=FACE_OUTER_BOUND('',#6587,.T.);
#4627=FACE_OUTER_BOUND('',#6588,.T.);
#4628=FACE_OUTER_BOUND('',#6589,.T.);
#4629=FACE_OUTER_BOUND('',#6590,.T.);
#4630=FACE_OUTER_BOUND('',#6591,.T.);
#4631=FACE_OUTER_BOUND('',#6592,.T.);
#4632=FACE_OUTER_BOUND('',#6593,.T.);
#4633=FACE_OUTER_BOUND('',#6594,.T.);
#4634=FACE_OUTER_BOUND('',#6596,.T.);
#4635=FACE_OUTER_BOUND('',#6597,.T.);
#4636=FACE_OUTER_BOUND('',#6598,.T.);
#4637=FACE_OUTER_BOUND('',#6634,.T.);
#4638=FACE_OUTER_BOUND('',#6635,.T.);
#4639=FACE_OUTER_BOUND('',#6637,.T.);
#4640=FACE_OUTER_BOUND('',#6638,.T.);
#4641=FACE_OUTER_BOUND('',#6639,.T.);
#4642=FACE_OUTER_BOUND('',#6640,.T.);
#4643=FACE_OUTER_BOUND('',#6641,.T.);
#4644=FACE_OUTER_BOUND('',#6642,.T.);
#4645=FACE_OUTER_BOUND('',#6643,.T.);
#4646=FACE_OUTER_BOUND('',#6644,.T.);
#4647=FACE_OUTER_BOUND('',#6645,.T.);
#4648=FACE_OUTER_BOUND('',#6646,.T.);
#4649=FACE_OUTER_BOUND('',#6647,.T.);
#4650=FACE_OUTER_BOUND('',#6648,.T.);
#4651=FACE_OUTER_BOUND('',#6649,.T.);
#4652=FACE_OUTER_BOUND('',#6650,.T.);
#4653=FACE_OUTER_BOUND('',#6651,.T.);
#4654=FACE_OUTER_BOUND('',#6652,.T.);
#4655=FACE_OUTER_BOUND('',#6653,.T.);
#4656=FACE_OUTER_BOUND('',#6654,.T.);
#4657=FACE_OUTER_BOUND('',#6655,.T.);
#4658=FACE_OUTER_BOUND('',#6656,.T.);
#4659=FACE_OUTER_BOUND('',#6657,.T.);
#4660=FACE_OUTER_BOUND('',#6658,.T.);
#4661=FACE_OUTER_BOUND('',#6659,.T.);
#4662=FACE_OUTER_BOUND('',#6660,.T.);
#4663=FACE_OUTER_BOUND('',#6661,.T.);
#4664=FACE_OUTER_BOUND('',#6662,.T.);
#4665=FACE_OUTER_BOUND('',#6663,.T.);
#4666=FACE_OUTER_BOUND('',#6664,.T.);
#4667=FACE_OUTER_BOUND('',#6665,.T.);
#4668=FACE_OUTER_BOUND('',#6666,.T.);
#4669=FACE_OUTER_BOUND('',#6667,.T.);
#4670=FACE_OUTER_BOUND('',#6668,.T.);
#4671=FACE_OUTER_BOUND('',#6669,.T.);
#4672=FACE_OUTER_BOUND('',#6670,.T.);
#4673=FACE_OUTER_BOUND('',#6671,.T.);
#4674=FACE_OUTER_BOUND('',#6672,.T.);
#4675=FACE_OUTER_BOUND('',#6673,.T.);
#4676=FACE_OUTER_BOUND('',#6674,.T.);
#4677=FACE_OUTER_BOUND('',#6675,.T.);
#4678=FACE_OUTER_BOUND('',#6676,.T.);
#4679=FACE_OUTER_BOUND('',#6677,.T.);
#4680=FACE_OUTER_BOUND('',#6678,.T.);
#4681=FACE_OUTER_BOUND('',#6679,.T.);
#4682=FACE_OUTER_BOUND('',#6680,.T.);
#4683=FACE_OUTER_BOUND('',#6681,.T.);
#4684=FACE_OUTER_BOUND('',#6682,.T.);
#4685=FACE_OUTER_BOUND('',#6683,.T.);
#4686=FACE_OUTER_BOUND('',#6684,.T.);
#4687=FACE_OUTER_BOUND('',#6685,.T.);
#4688=FACE_OUTER_BOUND('',#6686,.T.);
#4689=FACE_OUTER_BOUND('',#6687,.T.);
#4690=FACE_OUTER_BOUND('',#6688,.T.);
#4691=FACE_OUTER_BOUND('',#6689,.T.);
#4692=FACE_OUTER_BOUND('',#6690,.T.);
#4693=FACE_OUTER_BOUND('',#6691,.T.);
#4694=FACE_OUTER_BOUND('',#6692,.T.);
#4695=FACE_OUTER_BOUND('',#6693,.T.);
#4696=FACE_OUTER_BOUND('',#6694,.T.);
#4697=FACE_OUTER_BOUND('',#6695,.T.);
#4698=FACE_OUTER_BOUND('',#6696,.T.);
#4699=FACE_OUTER_BOUND('',#6697,.T.);
#4700=FACE_OUTER_BOUND('',#6698,.T.);
#4701=FACE_OUTER_BOUND('',#6699,.T.);
#4702=FACE_OUTER_BOUND('',#6700,.T.);
#4703=FACE_OUTER_BOUND('',#6701,.T.);
#4704=FACE_OUTER_BOUND('',#6702,.T.);
#4705=FACE_OUTER_BOUND('',#6703,.T.);
#4706=FACE_OUTER_BOUND('',#6704,.T.);
#4707=FACE_OUTER_BOUND('',#6705,.T.);
#4708=FACE_OUTER_BOUND('',#6706,.T.);
#4709=FACE_OUTER_BOUND('',#6707,.T.);
#4710=FACE_OUTER_BOUND('',#6708,.T.);
#4711=FACE_OUTER_BOUND('',#6709,.T.);
#4712=FACE_OUTER_BOUND('',#6710,.T.);
#4713=FACE_OUTER_BOUND('',#6711,.T.);
#4714=FACE_OUTER_BOUND('',#6712,.T.);
#4715=FACE_OUTER_BOUND('',#6713,.T.);
#4716=FACE_OUTER_BOUND('',#6714,.T.);
#4717=FACE_OUTER_BOUND('',#6715,.T.);
#4718=FACE_OUTER_BOUND('',#6716,.T.);
#4719=FACE_OUTER_BOUND('',#6717,.T.);
#4720=FACE_OUTER_BOUND('',#6718,.T.);
#4721=FACE_OUTER_BOUND('',#6719,.T.);
#4722=FACE_OUTER_BOUND('',#6720,.T.);
#4723=FACE_OUTER_BOUND('',#6721,.T.);
#4724=FACE_OUTER_BOUND('',#6722,.T.);
#4725=FACE_OUTER_BOUND('',#6723,.T.);
#4726=FACE_OUTER_BOUND('',#6724,.T.);
#4727=FACE_OUTER_BOUND('',#6725,.T.);
#4728=FACE_OUTER_BOUND('',#6726,.T.);
#4729=FACE_OUTER_BOUND('',#6727,.T.);
#4730=FACE_OUTER_BOUND('',#6728,.T.);
#4731=FACE_OUTER_BOUND('',#6729,.T.);
#4732=FACE_OUTER_BOUND('',#6730,.T.);
#4733=FACE_OUTER_BOUND('',#6731,.T.);
#4734=FACE_OUTER_BOUND('',#6732,.T.);
#4735=FACE_OUTER_BOUND('',#6733,.T.);
#4736=FACE_OUTER_BOUND('',#6734,.T.);
#4737=FACE_OUTER_BOUND('',#6735,.T.);
#4738=FACE_OUTER_BOUND('',#6736,.T.);
#4739=FACE_OUTER_BOUND('',#6737,.T.);
#4740=FACE_OUTER_BOUND('',#6738,.T.);
#4741=FACE_OUTER_BOUND('',#6739,.T.);
#4742=FACE_OUTER_BOUND('',#6740,.T.);
#4743=FACE_OUTER_BOUND('',#6741,.T.);
#4744=FACE_OUTER_BOUND('',#6742,.T.);
#4745=FACE_OUTER_BOUND('',#6743,.T.);
#4746=FACE_OUTER_BOUND('',#6744,.T.);
#4747=FACE_OUTER_BOUND('',#6745,.T.);
#4748=FACE_OUTER_BOUND('',#6746,.T.);
#4749=FACE_OUTER_BOUND('',#6747,.T.);
#4750=FACE_OUTER_BOUND('',#6748,.T.);
#4751=FACE_OUTER_BOUND('',#6749,.T.);
#4752=FACE_OUTER_BOUND('',#6750,.T.);
#4753=FACE_OUTER_BOUND('',#6751,.T.);
#4754=FACE_OUTER_BOUND('',#6752,.T.);
#4755=FACE_OUTER_BOUND('',#6753,.T.);
#4756=FACE_OUTER_BOUND('',#6754,.T.);
#4757=FACE_OUTER_BOUND('',#6755,.T.);
#4758=FACE_OUTER_BOUND('',#6756,.T.);
#4759=FACE_OUTER_BOUND('',#6757,.T.);
#4760=FACE_OUTER_BOUND('',#6758,.T.);
#4761=FACE_OUTER_BOUND('',#6759,.T.);
#4762=FACE_OUTER_BOUND('',#6760,.T.);
#4763=FACE_OUTER_BOUND('',#6761,.T.);
#4764=FACE_OUTER_BOUND('',#6762,.T.);
#4765=FACE_OUTER_BOUND('',#6763,.T.);
#4766=FACE_OUTER_BOUND('',#6764,.T.);
#4767=FACE_OUTER_BOUND('',#6765,.T.);
#4768=FACE_OUTER_BOUND('',#6766,.T.);
#4769=FACE_OUTER_BOUND('',#6767,.T.);
#4770=FACE_OUTER_BOUND('',#6768,.T.);
#4771=FACE_OUTER_BOUND('',#6769,.T.);
#4772=FACE_OUTER_BOUND('',#6770,.T.);
#4773=FACE_OUTER_BOUND('',#6771,.T.);
#4774=FACE_OUTER_BOUND('',#6772,.T.);
#4775=FACE_OUTER_BOUND('',#6773,.T.);
#4776=FACE_OUTER_BOUND('',#6774,.T.);
#4777=FACE_OUTER_BOUND('',#6775,.T.);
#4778=FACE_OUTER_BOUND('',#6776,.T.);
#4779=FACE_OUTER_BOUND('',#6777,.T.);
#4780=FACE_OUTER_BOUND('',#6778,.T.);
#4781=FACE_OUTER_BOUND('',#6779,.T.);
#4782=FACE_OUTER_BOUND('',#6780,.T.);
#4783=FACE_OUTER_BOUND('',#6781,.T.);
#4784=FACE_OUTER_BOUND('',#6782,.T.);
#4785=FACE_OUTER_BOUND('',#6783,.T.);
#4786=FACE_OUTER_BOUND('',#6784,.T.);
#4787=FACE_OUTER_BOUND('',#6785,.T.);
#4788=FACE_OUTER_BOUND('',#6786,.T.);
#4789=FACE_OUTER_BOUND('',#6787,.T.);
#4790=FACE_OUTER_BOUND('',#6789,.T.);
#4791=FACE_OUTER_BOUND('',#6790,.T.);
#4792=FACE_OUTER_BOUND('',#6791,.T.);
#4793=FACE_OUTER_BOUND('',#6792,.T.);
#4794=FACE_OUTER_BOUND('',#6793,.T.);
#4795=FACE_OUTER_BOUND('',#6794,.T.);
#4796=FACE_OUTER_BOUND('',#6795,.T.);
#4797=FACE_OUTER_BOUND('',#6796,.T.);
#4798=FACE_OUTER_BOUND('',#6797,.T.);
#4799=FACE_OUTER_BOUND('',#6798,.T.);
#4800=FACE_OUTER_BOUND('',#6799,.T.);
#4801=FACE_OUTER_BOUND('',#6800,.T.);
#4802=FACE_OUTER_BOUND('',#6801,.T.);
#4803=FACE_OUTER_BOUND('',#6802,.T.);
#4804=FACE_OUTER_BOUND('',#6803,.T.);
#4805=FACE_OUTER_BOUND('',#6804,.T.);
#4806=FACE_OUTER_BOUND('',#6805,.T.);
#4807=FACE_OUTER_BOUND('',#6806,.T.);
#4808=FACE_OUTER_BOUND('',#6807,.T.);
#4809=FACE_OUTER_BOUND('',#6808,.T.);
#4810=FACE_OUTER_BOUND('',#6809,.T.);
#4811=FACE_OUTER_BOUND('',#6810,.T.);
#4812=FACE_OUTER_BOUND('',#6811,.T.);
#4813=FACE_OUTER_BOUND('',#6812,.T.);
#4814=FACE_OUTER_BOUND('',#6813,.T.);
#4815=FACE_OUTER_BOUND('',#6814,.T.);
#4816=FACE_OUTER_BOUND('',#6815,.T.);
#4817=FACE_OUTER_BOUND('',#6816,.T.);
#4818=FACE_OUTER_BOUND('',#6817,.T.);
#4819=FACE_OUTER_BOUND('',#6818,.T.);
#4820=FACE_OUTER_BOUND('',#6819,.T.);
#4821=FACE_OUTER_BOUND('',#6820,.T.);
#4822=FACE_OUTER_BOUND('',#6821,.T.);
#4823=FACE_OUTER_BOUND('',#6822,.T.);
#4824=FACE_OUTER_BOUND('',#6823,.T.);
#4825=FACE_OUTER_BOUND('',#6824,.T.);
#4826=FACE_OUTER_BOUND('',#6825,.T.);
#4827=FACE_OUTER_BOUND('',#6826,.T.);
#4828=FACE_OUTER_BOUND('',#6827,.T.);
#4829=FACE_OUTER_BOUND('',#6828,.T.);
#4830=FACE_OUTER_BOUND('',#6829,.T.);
#4831=FACE_OUTER_BOUND('',#6830,.T.);
#4832=FACE_OUTER_BOUND('',#6831,.T.);
#4833=FACE_OUTER_BOUND('',#6832,.T.);
#4834=FACE_OUTER_BOUND('',#6833,.T.);
#4835=FACE_OUTER_BOUND('',#6834,.T.);
#4836=FACE_OUTER_BOUND('',#6835,.T.);
#4837=FACE_OUTER_BOUND('',#6836,.T.);
#4838=FACE_OUTER_BOUND('',#6837,.T.);
#4839=FACE_OUTER_BOUND('',#6838,.T.);
#4840=FACE_OUTER_BOUND('',#6839,.T.);
#4841=FACE_OUTER_BOUND('',#6840,.T.);
#4842=FACE_OUTER_BOUND('',#6841,.T.);
#4843=FACE_OUTER_BOUND('',#6842,.T.);
#4844=FACE_OUTER_BOUND('',#6843,.T.);
#4845=FACE_OUTER_BOUND('',#6844,.T.);
#4846=FACE_OUTER_BOUND('',#6845,.T.);
#4847=FACE_OUTER_BOUND('',#6846,.T.);
#4848=FACE_OUTER_BOUND('',#6847,.T.);
#4849=FACE_OUTER_BOUND('',#6848,.T.);
#4850=FACE_OUTER_BOUND('',#6849,.T.);
#4851=FACE_OUTER_BOUND('',#6850,.T.);
#4852=FACE_OUTER_BOUND('',#6851,.T.);
#4853=FACE_OUTER_BOUND('',#6852,.T.);
#4854=FACE_OUTER_BOUND('',#6853,.T.);
#4855=FACE_OUTER_BOUND('',#6854,.T.);
#4856=FACE_OUTER_BOUND('',#6855,.T.);
#4857=FACE_OUTER_BOUND('',#6856,.T.);
#4858=FACE_OUTER_BOUND('',#6857,.T.);
#4859=FACE_OUTER_BOUND('',#6858,.T.);
#4860=FACE_OUTER_BOUND('',#6859,.T.);
#4861=FACE_OUTER_BOUND('',#6860,.T.);
#4862=FACE_OUTER_BOUND('',#6861,.T.);
#4863=FACE_OUTER_BOUND('',#6862,.T.);
#4864=FACE_OUTER_BOUND('',#6863,.T.);
#4865=FACE_OUTER_BOUND('',#6864,.T.);
#4866=FACE_OUTER_BOUND('',#6865,.T.);
#4867=FACE_OUTER_BOUND('',#6866,.T.);
#4868=FACE_OUTER_BOUND('',#6867,.T.);
#4869=FACE_OUTER_BOUND('',#6868,.T.);
#4870=FACE_OUTER_BOUND('',#6869,.T.);
#4871=FACE_OUTER_BOUND('',#6870,.T.);
#4872=FACE_OUTER_BOUND('',#6871,.T.);
#4873=FACE_OUTER_BOUND('',#6872,.T.);
#4874=FACE_OUTER_BOUND('',#6873,.T.);
#4875=FACE_OUTER_BOUND('',#6874,.T.);
#4876=FACE_OUTER_BOUND('',#6875,.T.);
#4877=FACE_OUTER_BOUND('',#6876,.T.);
#4878=FACE_OUTER_BOUND('',#6877,.T.);
#4879=FACE_OUTER_BOUND('',#6878,.T.);
#4880=FACE_OUTER_BOUND('',#6879,.T.);
#4881=FACE_OUTER_BOUND('',#6880,.T.);
#4882=FACE_OUTER_BOUND('',#6881,.T.);
#4883=FACE_OUTER_BOUND('',#6882,.T.);
#4884=FACE_OUTER_BOUND('',#6883,.T.);
#4885=FACE_OUTER_BOUND('',#6884,.T.);
#4886=FACE_OUTER_BOUND('',#6885,.T.);
#4887=FACE_OUTER_BOUND('',#6886,.T.);
#4888=FACE_OUTER_BOUND('',#6887,.T.);
#4889=FACE_OUTER_BOUND('',#6888,.T.);
#4890=FACE_OUTER_BOUND('',#6889,.T.);
#4891=FACE_OUTER_BOUND('',#6890,.T.);
#4892=FACE_OUTER_BOUND('',#6891,.T.);
#4893=FACE_OUTER_BOUND('',#6892,.T.);
#4894=FACE_OUTER_BOUND('',#6893,.T.);
#4895=FACE_OUTER_BOUND('',#6894,.T.);
#4896=FACE_OUTER_BOUND('',#6895,.T.);
#4897=FACE_OUTER_BOUND('',#6896,.T.);
#4898=FACE_OUTER_BOUND('',#6897,.T.);
#4899=FACE_OUTER_BOUND('',#6898,.T.);
#4900=FACE_OUTER_BOUND('',#6899,.T.);
#4901=FACE_OUTER_BOUND('',#6900,.T.);
#4902=FACE_OUTER_BOUND('',#6901,.T.);
#4903=FACE_OUTER_BOUND('',#6902,.T.);
#4904=FACE_OUTER_BOUND('',#6903,.T.);
#4905=FACE_OUTER_BOUND('',#6904,.T.);
#4906=FACE_OUTER_BOUND('',#6905,.T.);
#4907=FACE_OUTER_BOUND('',#6906,.T.);
#4908=FACE_OUTER_BOUND('',#6907,.T.);
#4909=FACE_OUTER_BOUND('',#6908,.T.);
#4910=FACE_OUTER_BOUND('',#6909,.T.);
#4911=FACE_OUTER_BOUND('',#6910,.T.);
#4912=FACE_OUTER_BOUND('',#6911,.T.);
#4913=FACE_OUTER_BOUND('',#6912,.T.);
#4914=FACE_OUTER_BOUND('',#6913,.T.);
#4915=FACE_OUTER_BOUND('',#6914,.T.);
#4916=FACE_OUTER_BOUND('',#6915,.T.);
#4917=FACE_OUTER_BOUND('',#6916,.T.);
#4918=FACE_OUTER_BOUND('',#6917,.T.);
#4919=FACE_OUTER_BOUND('',#6918,.T.);
#4920=FACE_OUTER_BOUND('',#6919,.T.);
#4921=FACE_OUTER_BOUND('',#6920,.T.);
#4922=FACE_OUTER_BOUND('',#6921,.T.);
#4923=FACE_OUTER_BOUND('',#6922,.T.);
#4924=FACE_OUTER_BOUND('',#6923,.T.);
#4925=FACE_OUTER_BOUND('',#6924,.T.);
#4926=FACE_OUTER_BOUND('',#6925,.T.);
#4927=FACE_OUTER_BOUND('',#6926,.T.);
#4928=FACE_OUTER_BOUND('',#6927,.T.);
#4929=FACE_OUTER_BOUND('',#6928,.T.);
#4930=FACE_OUTER_BOUND('',#6929,.T.);
#4931=FACE_OUTER_BOUND('',#6930,.T.);
#4932=FACE_OUTER_BOUND('',#6931,.T.);
#4933=FACE_OUTER_BOUND('',#6932,.T.);
#4934=FACE_OUTER_BOUND('',#6933,.T.);
#4935=FACE_OUTER_BOUND('',#6934,.T.);
#4936=FACE_OUTER_BOUND('',#6935,.T.);
#4937=FACE_OUTER_BOUND('',#6936,.T.);
#4938=FACE_OUTER_BOUND('',#6937,.T.);
#4939=FACE_OUTER_BOUND('',#6938,.T.);
#4940=FACE_OUTER_BOUND('',#6939,.T.);
#4941=FACE_OUTER_BOUND('',#6940,.T.);
#4942=FACE_OUTER_BOUND('',#6942,.T.);
#4943=FACE_OUTER_BOUND('',#6943,.T.);
#4944=FACE_OUTER_BOUND('',#6944,.T.);
#4945=FACE_OUTER_BOUND('',#6980,.T.);
#4946=FACE_OUTER_BOUND('',#6981,.T.);
#4947=FACE_OUTER_BOUND('',#6983,.T.);
#4948=FACE_OUTER_BOUND('',#6984,.T.);
#4949=FACE_OUTER_BOUND('',#6985,.T.);
#4950=FACE_OUTER_BOUND('',#6986,.T.);
#4951=FACE_OUTER_BOUND('',#6987,.T.);
#4952=FACE_OUTER_BOUND('',#6988,.T.);
#4953=FACE_OUTER_BOUND('',#6989,.T.);
#4954=FACE_OUTER_BOUND('',#6990,.T.);
#4955=FACE_OUTER_BOUND('',#6991,.T.);
#4956=FACE_OUTER_BOUND('',#6992,.T.);
#4957=FACE_OUTER_BOUND('',#6993,.T.);
#4958=FACE_OUTER_BOUND('',#6994,.T.);
#4959=FACE_OUTER_BOUND('',#6995,.T.);
#4960=FACE_OUTER_BOUND('',#6996,.T.);
#4961=FACE_OUTER_BOUND('',#6997,.T.);
#4962=FACE_OUTER_BOUND('',#6998,.T.);
#4963=FACE_OUTER_BOUND('',#6999,.T.);
#4964=FACE_OUTER_BOUND('',#7000,.T.);
#4965=FACE_OUTER_BOUND('',#7001,.T.);
#4966=FACE_OUTER_BOUND('',#7002,.T.);
#4967=FACE_OUTER_BOUND('',#7003,.T.);
#4968=FACE_OUTER_BOUND('',#7004,.T.);
#4969=FACE_OUTER_BOUND('',#7005,.T.);
#4970=FACE_OUTER_BOUND('',#7006,.T.);
#4971=FACE_OUTER_BOUND('',#7007,.T.);
#4972=FACE_OUTER_BOUND('',#7008,.T.);
#4973=FACE_OUTER_BOUND('',#7009,.T.);
#4974=FACE_OUTER_BOUND('',#7010,.T.);
#4975=FACE_OUTER_BOUND('',#7011,.T.);
#4976=FACE_OUTER_BOUND('',#7012,.T.);
#4977=FACE_OUTER_BOUND('',#7013,.T.);
#4978=FACE_OUTER_BOUND('',#7014,.T.);
#4979=FACE_OUTER_BOUND('',#7015,.T.);
#4980=FACE_OUTER_BOUND('',#7016,.T.);
#4981=FACE_OUTER_BOUND('',#7017,.T.);
#4982=FACE_OUTER_BOUND('',#7018,.T.);
#4983=FACE_OUTER_BOUND('',#7020,.T.);
#4984=FACE_OUTER_BOUND('',#7021,.T.);
#4985=FACE_OUTER_BOUND('',#7022,.T.);
#4986=FACE_OUTER_BOUND('',#7023,.T.);
#4987=FACE_OUTER_BOUND('',#7024,.T.);
#4988=FACE_OUTER_BOUND('',#7025,.T.);
#4989=FACE_OUTER_BOUND('',#7026,.T.);
#4990=FACE_OUTER_BOUND('',#7028,.T.);
#4991=FACE_OUTER_BOUND('',#7029,.T.);
#4992=FACE_OUTER_BOUND('',#7030,.T.);
#4993=FACE_OUTER_BOUND('',#7031,.T.);
#4994=FACE_OUTER_BOUND('',#7032,.T.);
#4995=FACE_OUTER_BOUND('',#7033,.T.);
#4996=FACE_OUTER_BOUND('',#7034,.T.);
#4997=FACE_OUTER_BOUND('',#7035,.T.);
#4998=FACE_OUTER_BOUND('',#7036,.T.);
#4999=FACE_OUTER_BOUND('',#7037,.T.);
#5000=FACE_OUTER_BOUND('',#7038,.T.);
#5001=FACE_OUTER_BOUND('',#7039,.T.);
#5002=FACE_OUTER_BOUND('',#7040,.T.);
#5003=FACE_OUTER_BOUND('',#7041,.T.);
#5004=FACE_OUTER_BOUND('',#7042,.T.);
#5005=FACE_OUTER_BOUND('',#7043,.T.);
#5006=FACE_OUTER_BOUND('',#7044,.T.);
#5007=FACE_OUTER_BOUND('',#7045,.T.);
#5008=FACE_OUTER_BOUND('',#7046,.T.);
#5009=FACE_OUTER_BOUND('',#7047,.T.);
#5010=FACE_OUTER_BOUND('',#7048,.T.);
#5011=FACE_OUTER_BOUND('',#7049,.T.);
#5012=FACE_OUTER_BOUND('',#7050,.T.);
#5013=FACE_OUTER_BOUND('',#7051,.T.);
#5014=FACE_OUTER_BOUND('',#7052,.T.);
#5015=FACE_OUTER_BOUND('',#7053,.T.);
#5016=FACE_OUTER_BOUND('',#7054,.T.);
#5017=FACE_OUTER_BOUND('',#7055,.T.);
#5018=FACE_OUTER_BOUND('',#7056,.T.);
#5019=FACE_OUTER_BOUND('',#7057,.T.);
#5020=FACE_OUTER_BOUND('',#7058,.T.);
#5021=FACE_OUTER_BOUND('',#7059,.T.);
#5022=FACE_OUTER_BOUND('',#7060,.T.);
#5023=FACE_OUTER_BOUND('',#7061,.T.);
#5024=FACE_OUTER_BOUND('',#7063,.T.);
#5025=FACE_OUTER_BOUND('',#7065,.T.);
#5026=FACE_OUTER_BOUND('',#7066,.T.);
#5027=FACE_OUTER_BOUND('',#7068,.T.);
#5028=FACE_OUTER_BOUND('',#7069,.T.);
#5029=FACE_OUTER_BOUND('',#7070,.T.);
#5030=FACE_OUTER_BOUND('',#7072,.T.);
#5031=FACE_OUTER_BOUND('',#7073,.T.);
#5032=FACE_OUTER_BOUND('',#7074,.T.);
#5033=FACE_OUTER_BOUND('',#7075,.T.);
#5034=FACE_OUTER_BOUND('',#7076,.T.);
#5035=FACE_OUTER_BOUND('',#7077,.T.);
#5036=FACE_OUTER_BOUND('',#7078,.T.);
#5037=FACE_OUTER_BOUND('',#7079,.T.);
#5038=FACE_OUTER_BOUND('',#7080,.T.);
#5039=FACE_OUTER_BOUND('',#7082,.T.);
#5040=FACE_OUTER_BOUND('',#7083,.T.);
#5041=FACE_OUTER_BOUND('',#7084,.T.);
#5042=FACE_OUTER_BOUND('',#7086,.T.);
#5043=FACE_OUTER_BOUND('',#7087,.T.);
#5044=FACE_OUTER_BOUND('',#7088,.T.);
#5045=FACE_OUTER_BOUND('',#7089,.T.);
#5046=FACE_OUTER_BOUND('',#7090,.T.);
#5047=FACE_OUTER_BOUND('',#7091,.T.);
#5048=FACE_OUTER_BOUND('',#7092,.T.);
#5049=FACE_OUTER_BOUND('',#7093,.T.);
#5050=FACE_OUTER_BOUND('',#7094,.T.);
#5051=FACE_OUTER_BOUND('',#7095,.T.);
#5052=FACE_OUTER_BOUND('',#7096,.T.);
#5053=FACE_OUTER_BOUND('',#7097,.T.);
#5054=FACE_OUTER_BOUND('',#7098,.T.);
#5055=FACE_OUTER_BOUND('',#7099,.T.);
#5056=FACE_OUTER_BOUND('',#7100,.T.);
#5057=FACE_OUTER_BOUND('',#7101,.T.);
#5058=FACE_OUTER_BOUND('',#7102,.T.);
#5059=FACE_OUTER_BOUND('',#7103,.T.);
#5060=FACE_OUTER_BOUND('',#7104,.T.);
#5061=FACE_OUTER_BOUND('',#7105,.T.);
#5062=FACE_OUTER_BOUND('',#7106,.T.);
#5063=FACE_OUTER_BOUND('',#7107,.T.);
#5064=FACE_OUTER_BOUND('',#7108,.T.);
#5065=FACE_OUTER_BOUND('',#7109,.T.);
#5066=FACE_OUTER_BOUND('',#7110,.T.);
#5067=FACE_OUTER_BOUND('',#7111,.T.);
#5068=FACE_OUTER_BOUND('',#7112,.T.);
#5069=FACE_OUTER_BOUND('',#7113,.T.);
#5070=FACE_OUTER_BOUND('',#7114,.T.);
#5071=FACE_OUTER_BOUND('',#7115,.T.);
#5072=FACE_OUTER_BOUND('',#7116,.T.);
#5073=FACE_OUTER_BOUND('',#7117,.T.);
#5074=FACE_OUTER_BOUND('',#7118,.T.);
#5075=FACE_OUTER_BOUND('',#7119,.T.);
#5076=FACE_OUTER_BOUND('',#7120,.T.);
#5077=FACE_OUTER_BOUND('',#7121,.T.);
#5078=FACE_OUTER_BOUND('',#7122,.T.);
#5079=FACE_OUTER_BOUND('',#7123,.T.);
#5080=FACE_OUTER_BOUND('',#7124,.T.);
#5081=FACE_OUTER_BOUND('',#7125,.T.);
#5082=FACE_OUTER_BOUND('',#7126,.T.);
#5083=FACE_OUTER_BOUND('',#7127,.T.);
#5084=FACE_OUTER_BOUND('',#7128,.T.);
#5085=FACE_OUTER_BOUND('',#7129,.T.);
#5086=FACE_OUTER_BOUND('',#7130,.T.);
#5087=FACE_OUTER_BOUND('',#7131,.T.);
#5088=FACE_OUTER_BOUND('',#7132,.T.);
#5089=FACE_OUTER_BOUND('',#7133,.T.);
#5090=FACE_OUTER_BOUND('',#7134,.T.);
#5091=FACE_OUTER_BOUND('',#7135,.T.);
#5092=FACE_OUTER_BOUND('',#7136,.T.);
#5093=FACE_OUTER_BOUND('',#7137,.T.);
#5094=FACE_OUTER_BOUND('',#7138,.T.);
#5095=FACE_OUTER_BOUND('',#7139,.T.);
#5096=FACE_OUTER_BOUND('',#7140,.T.);
#5097=FACE_OUTER_BOUND('',#7141,.T.);
#5098=FACE_OUTER_BOUND('',#7142,.T.);
#5099=FACE_OUTER_BOUND('',#7143,.T.);
#5100=FACE_OUTER_BOUND('',#7144,.T.);
#5101=FACE_OUTER_BOUND('',#7145,.T.);
#5102=FACE_OUTER_BOUND('',#7146,.T.);
#5103=FACE_OUTER_BOUND('',#7147,.T.);
#5104=FACE_OUTER_BOUND('',#7148,.T.);
#5105=FACE_OUTER_BOUND('',#7149,.T.);
#5106=FACE_OUTER_BOUND('',#7150,.T.);
#5107=FACE_OUTER_BOUND('',#7151,.T.);
#5108=FACE_OUTER_BOUND('',#7152,.T.);
#5109=FACE_OUTER_BOUND('',#7153,.T.);
#5110=FACE_OUTER_BOUND('',#7154,.T.);
#5111=FACE_OUTER_BOUND('',#7155,.T.);
#5112=FACE_OUTER_BOUND('',#7156,.T.);
#5113=FACE_OUTER_BOUND('',#7157,.T.);
#5114=FACE_OUTER_BOUND('',#7158,.T.);
#5115=FACE_OUTER_BOUND('',#7159,.T.);
#5116=FACE_OUTER_BOUND('',#7160,.T.);
#5117=FACE_OUTER_BOUND('',#7161,.T.);
#5118=FACE_OUTER_BOUND('',#7162,.T.);
#5119=FACE_OUTER_BOUND('',#7163,.T.);
#5120=FACE_OUTER_BOUND('',#7164,.T.);
#5121=FACE_OUTER_BOUND('',#7165,.T.);
#5122=FACE_OUTER_BOUND('',#7166,.T.);
#5123=FACE_OUTER_BOUND('',#7167,.T.);
#5124=FACE_OUTER_BOUND('',#7168,.T.);
#5125=FACE_OUTER_BOUND('',#7169,.T.);
#5126=FACE_OUTER_BOUND('',#7170,.T.);
#5127=FACE_OUTER_BOUND('',#7171,.T.);
#5128=FACE_OUTER_BOUND('',#7172,.T.);
#5129=FACE_OUTER_BOUND('',#7173,.T.);
#5130=FACE_OUTER_BOUND('',#7174,.T.);
#5131=FACE_OUTER_BOUND('',#7175,.T.);
#5132=FACE_OUTER_BOUND('',#7176,.T.);
#5133=FACE_OUTER_BOUND('',#7177,.T.);
#5134=FACE_OUTER_BOUND('',#7178,.T.);
#5135=FACE_OUTER_BOUND('',#7179,.T.);
#5136=FACE_OUTER_BOUND('',#7180,.T.);
#5137=FACE_OUTER_BOUND('',#7181,.T.);
#5138=FACE_OUTER_BOUND('',#7182,.T.);
#5139=FACE_OUTER_BOUND('',#7183,.T.);
#5140=FACE_OUTER_BOUND('',#7184,.T.);
#5141=FACE_OUTER_BOUND('',#7185,.T.);
#5142=FACE_OUTER_BOUND('',#7186,.T.);
#5143=FACE_OUTER_BOUND('',#7187,.T.);
#5144=FACE_OUTER_BOUND('',#7188,.T.);
#5145=FACE_OUTER_BOUND('',#7189,.T.);
#5146=FACE_OUTER_BOUND('',#7190,.T.);
#5147=FACE_OUTER_BOUND('',#7191,.T.);
#5148=FACE_OUTER_BOUND('',#7192,.T.);
#5149=FACE_OUTER_BOUND('',#7193,.T.);
#5150=FACE_OUTER_BOUND('',#7194,.T.);
#5151=FACE_OUTER_BOUND('',#7195,.T.);
#5152=FACE_OUTER_BOUND('',#7196,.T.);
#5153=FACE_OUTER_BOUND('',#7197,.T.);
#5154=FACE_OUTER_BOUND('',#7198,.T.);
#5155=FACE_OUTER_BOUND('',#7199,.T.);
#5156=FACE_OUTER_BOUND('',#7200,.T.);
#5157=FACE_OUTER_BOUND('',#7201,.T.);
#5158=FACE_OUTER_BOUND('',#7202,.T.);
#5159=FACE_OUTER_BOUND('',#7203,.T.);
#5160=FACE_OUTER_BOUND('',#7204,.T.);
#5161=FACE_OUTER_BOUND('',#7205,.T.);
#5162=FACE_OUTER_BOUND('',#7206,.T.);
#5163=FACE_OUTER_BOUND('',#7207,.T.);
#5164=FACE_OUTER_BOUND('',#7208,.T.);
#5165=FACE_OUTER_BOUND('',#7209,.T.);
#5166=FACE_OUTER_BOUND('',#7210,.T.);
#5167=FACE_OUTER_BOUND('',#7211,.T.);
#5168=FACE_OUTER_BOUND('',#7212,.T.);
#5169=FACE_OUTER_BOUND('',#7213,.T.);
#5170=FACE_OUTER_BOUND('',#7214,.T.);
#5171=FACE_OUTER_BOUND('',#7215,.T.);
#5172=FACE_OUTER_BOUND('',#7216,.T.);
#5173=FACE_OUTER_BOUND('',#7217,.T.);
#5174=FACE_OUTER_BOUND('',#7218,.T.);
#5175=FACE_OUTER_BOUND('',#7219,.T.);
#5176=FACE_OUTER_BOUND('',#7220,.T.);
#5177=FACE_OUTER_BOUND('',#7221,.T.);
#5178=FACE_OUTER_BOUND('',#7222,.T.);
#5179=FACE_OUTER_BOUND('',#7223,.T.);
#5180=FACE_OUTER_BOUND('',#7224,.T.);
#5181=FACE_OUTER_BOUND('',#7225,.T.);
#5182=FACE_OUTER_BOUND('',#7226,.T.);
#5183=FACE_OUTER_BOUND('',#7227,.T.);
#5184=FACE_OUTER_BOUND('',#7228,.T.);
#5185=FACE_OUTER_BOUND('',#7229,.T.);
#5186=FACE_OUTER_BOUND('',#7230,.T.);
#5187=FACE_OUTER_BOUND('',#7231,.T.);
#5188=FACE_OUTER_BOUND('',#7232,.T.);
#5189=FACE_OUTER_BOUND('',#7233,.T.);
#5190=FACE_OUTER_BOUND('',#7234,.T.);
#5191=FACE_OUTER_BOUND('',#7235,.T.);
#5192=FACE_OUTER_BOUND('',#7236,.T.);
#5193=FACE_OUTER_BOUND('',#7237,.T.);
#5194=FACE_OUTER_BOUND('',#7238,.T.);
#5195=FACE_OUTER_BOUND('',#7239,.T.);
#5196=FACE_OUTER_BOUND('',#7240,.T.);
#5197=FACE_OUTER_BOUND('',#7241,.T.);
#5198=FACE_OUTER_BOUND('',#7242,.T.);
#5199=FACE_OUTER_BOUND('',#7243,.T.);
#5200=FACE_OUTER_BOUND('',#7244,.T.);
#5201=FACE_OUTER_BOUND('',#7245,.T.);
#5202=FACE_OUTER_BOUND('',#7246,.T.);
#5203=FACE_OUTER_BOUND('',#7247,.T.);
#5204=FACE_OUTER_BOUND('',#7248,.T.);
#5205=FACE_OUTER_BOUND('',#7250,.T.);
#5206=FACE_OUTER_BOUND('',#7251,.T.);
#5207=FACE_OUTER_BOUND('',#7252,.T.);
#5208=FACE_OUTER_BOUND('',#7254,.T.);
#5209=FACE_OUTER_BOUND('',#7255,.T.);
#5210=FACE_OUTER_BOUND('',#7256,.T.);
#5211=FACE_OUTER_BOUND('',#7257,.T.);
#5212=FACE_OUTER_BOUND('',#7258,.T.);
#5213=FACE_OUTER_BOUND('',#7259,.T.);
#5214=FACE_OUTER_BOUND('',#7260,.T.);
#5215=FACE_OUTER_BOUND('',#7261,.T.);
#5216=FACE_OUTER_BOUND('',#7262,.T.);
#5217=FACE_OUTER_BOUND('',#7263,.T.);
#5218=FACE_OUTER_BOUND('',#7264,.T.);
#5219=FACE_OUTER_BOUND('',#7265,.T.);
#5220=FACE_OUTER_BOUND('',#7266,.T.);
#5221=FACE_OUTER_BOUND('',#7267,.T.);
#5222=FACE_OUTER_BOUND('',#7268,.T.);
#5223=FACE_OUTER_BOUND('',#7269,.T.);
#5224=FACE_OUTER_BOUND('',#7270,.T.);
#5225=FACE_OUTER_BOUND('',#7271,.T.);
#5226=FACE_OUTER_BOUND('',#7272,.T.);
#5227=FACE_OUTER_BOUND('',#7273,.T.);
#5228=FACE_OUTER_BOUND('',#7274,.T.);
#5229=FACE_OUTER_BOUND('',#7275,.T.);
#5230=FACE_OUTER_BOUND('',#7276,.T.);
#5231=FACE_OUTER_BOUND('',#7277,.T.);
#5232=FACE_OUTER_BOUND('',#7278,.T.);
#5233=FACE_OUTER_BOUND('',#7279,.T.);
#5234=FACE_OUTER_BOUND('',#7280,.T.);
#5235=FACE_OUTER_BOUND('',#7281,.T.);
#5236=FACE_OUTER_BOUND('',#7282,.T.);
#5237=FACE_OUTER_BOUND('',#7283,.T.);
#5238=FACE_OUTER_BOUND('',#7284,.T.);
#5239=FACE_OUTER_BOUND('',#7285,.T.);
#5240=FACE_OUTER_BOUND('',#7286,.T.);
#5241=FACE_OUTER_BOUND('',#7287,.T.);
#5242=FACE_OUTER_BOUND('',#7288,.T.);
#5243=FACE_OUTER_BOUND('',#7289,.T.);
#5244=FACE_OUTER_BOUND('',#7290,.T.);
#5245=FACE_OUTER_BOUND('',#7291,.T.);
#5246=FACE_OUTER_BOUND('',#7292,.T.);
#5247=FACE_OUTER_BOUND('',#7293,.T.);
#5248=FACE_OUTER_BOUND('',#7294,.T.);
#5249=FACE_OUTER_BOUND('',#7295,.T.);
#5250=FACE_OUTER_BOUND('',#7296,.T.);
#5251=FACE_OUTER_BOUND('',#7297,.T.);
#5252=FACE_OUTER_BOUND('',#7298,.T.);
#5253=FACE_OUTER_BOUND('',#7299,.T.);
#5254=FACE_OUTER_BOUND('',#7300,.T.);
#5255=FACE_OUTER_BOUND('',#7301,.T.);
#5256=FACE_OUTER_BOUND('',#7302,.T.);
#5257=FACE_OUTER_BOUND('',#7303,.T.);
#5258=FACE_OUTER_BOUND('',#7304,.T.);
#5259=FACE_OUTER_BOUND('',#7305,.T.);
#5260=FACE_OUTER_BOUND('',#7306,.T.);
#5261=FACE_OUTER_BOUND('',#7307,.T.);
#5262=FACE_OUTER_BOUND('',#7308,.T.);
#5263=FACE_OUTER_BOUND('',#7309,.T.);
#5264=FACE_OUTER_BOUND('',#7310,.T.);
#5265=FACE_OUTER_BOUND('',#7311,.T.);
#5266=FACE_OUTER_BOUND('',#7312,.T.);
#5267=FACE_OUTER_BOUND('',#7313,.T.);
#5268=FACE_OUTER_BOUND('',#7314,.T.);
#5269=FACE_OUTER_BOUND('',#7315,.T.);
#5270=FACE_OUTER_BOUND('',#7316,.T.);
#5271=FACE_OUTER_BOUND('',#7317,.T.);
#5272=FACE_OUTER_BOUND('',#7318,.T.);
#5273=FACE_OUTER_BOUND('',#7319,.T.);
#5274=FACE_OUTER_BOUND('',#7320,.T.);
#5275=FACE_OUTER_BOUND('',#7321,.T.);
#5276=FACE_OUTER_BOUND('',#7322,.T.);
#5277=FACE_OUTER_BOUND('',#7323,.T.);
#5278=FACE_OUTER_BOUND('',#7325,.T.);
#5279=FACE_OUTER_BOUND('',#7326,.T.);
#5280=FACE_OUTER_BOUND('',#7327,.T.);
#5281=FACE_OUTER_BOUND('',#7328,.T.);
#5282=FACE_OUTER_BOUND('',#7329,.T.);
#5283=FACE_OUTER_BOUND('',#7330,.T.);
#5284=FACE_OUTER_BOUND('',#7331,.T.);
#5285=FACE_OUTER_BOUND('',#7332,.T.);
#5286=FACE_OUTER_BOUND('',#7333,.T.);
#5287=FACE_OUTER_BOUND('',#7334,.T.);
#5288=FACE_OUTER_BOUND('',#7335,.T.);
#5289=FACE_OUTER_BOUND('',#7336,.T.);
#5290=FACE_OUTER_BOUND('',#7337,.T.);
#5291=FACE_OUTER_BOUND('',#7338,.T.);
#5292=FACE_OUTER_BOUND('',#7339,.T.);
#5293=FACE_OUTER_BOUND('',#7340,.T.);
#5294=FACE_OUTER_BOUND('',#7341,.T.);
#5295=FACE_OUTER_BOUND('',#7342,.T.);
#5296=FACE_OUTER_BOUND('',#7343,.T.);
#5297=FACE_OUTER_BOUND('',#7344,.T.);
#5298=FACE_OUTER_BOUND('',#7345,.T.);
#5299=FACE_OUTER_BOUND('',#7346,.T.);
#5300=FACE_OUTER_BOUND('',#7347,.T.);
#5301=FACE_OUTER_BOUND('',#7349,.T.);
#5302=FACE_OUTER_BOUND('',#7350,.T.);
#5303=FACE_OUTER_BOUND('',#7351,.T.);
#5304=FACE_OUTER_BOUND('',#7352,.T.);
#5305=FACE_OUTER_BOUND('',#7353,.T.);
#5306=FACE_OUTER_BOUND('',#7354,.T.);
#5307=FACE_OUTER_BOUND('',#7355,.T.);
#5308=FACE_OUTER_BOUND('',#7356,.T.);
#5309=FACE_OUTER_BOUND('',#7357,.T.);
#5310=FACE_OUTER_BOUND('',#7358,.T.);
#5311=FACE_OUTER_BOUND('',#7359,.T.);
#5312=FACE_OUTER_BOUND('',#7360,.T.);
#5313=FACE_OUTER_BOUND('',#7361,.T.);
#5314=FACE_OUTER_BOUND('',#7362,.T.);
#5315=FACE_OUTER_BOUND('',#7363,.T.);
#5316=FACE_OUTER_BOUND('',#7364,.T.);
#5317=FACE_OUTER_BOUND('',#7365,.T.);
#5318=FACE_OUTER_BOUND('',#7366,.T.);
#5319=FACE_OUTER_BOUND('',#7367,.T.);
#5320=FACE_OUTER_BOUND('',#7368,.T.);
#5321=FACE_OUTER_BOUND('',#7369,.T.);
#5322=FACE_OUTER_BOUND('',#7370,.T.);
#5323=FACE_OUTER_BOUND('',#7371,.T.);
#5324=FACE_OUTER_BOUND('',#7372,.T.);
#5325=FACE_OUTER_BOUND('',#7373,.T.);
#5326=FACE_OUTER_BOUND('',#7374,.T.);
#5327=FACE_OUTER_BOUND('',#7375,.T.);
#5328=FACE_OUTER_BOUND('',#7376,.T.);
#5329=FACE_OUTER_BOUND('',#7377,.T.);
#5330=FACE_OUTER_BOUND('',#7378,.T.);
#5331=FACE_OUTER_BOUND('',#7379,.T.);
#5332=FACE_OUTER_BOUND('',#7380,.T.);
#5333=EDGE_LOOP('',(#19269,#19270,#19271,#19272,#19273,#19274));
#5334=EDGE_LOOP('',(#19275,#19276,#19277,#19278));
#5335=EDGE_LOOP('',(#19279,#19280,#19281,#19282,#19283,#19284));
#5336=EDGE_LOOP('',(#19285,#19286,#19287,#19288,#19289));
#5337=EDGE_LOOP('',(#19290,#19291,#19292,#19293,#19294,#19295));
#5338=EDGE_LOOP('',(#19296,#19297,#19298,#19299,#19300,#19301));
#5339=EDGE_LOOP('',(#19302,#19303,#19304,#19305,#19306,#19307));
#5340=EDGE_LOOP('',(#19308,#19309,#19310,#19311));
#5341=EDGE_LOOP('',(#19312,#19313,#19314,#19315,#19316,#19317,#19318,#19319,
#19320,#19321,#19322,#19323));
#5342=EDGE_LOOP('',(#19324,#19325,#19326,#19327,#19328,#19329,#19330,#19331,
#19332,#19333,#19334,#19335,#19336,#19337,#19338,#19339,#19340,#19341,#19342));
#5343=EDGE_LOOP('',(#19343,#19344,#19345,#19346,#19347,#19348,#19349,#19350,
#19351,#19352,#19353,#19354));
#5344=EDGE_LOOP('',(#19355,#19356,#19357,#19358,#19359,#19360,#19361,#19362,
#19363,#19364,#19365));
#5345=EDGE_LOOP('',(#19366,#19367,#19368,#19369,#19370,#19371,#19372,#19373,
#19374,#19375,#19376,#19377,#19378,#19379,#19380,#19381,#19382,#19383,#19384,
#19385,#19386,#19387,#19388,#19389,#19390,#19391,#19392,#19393,#19394,#19395,
#19396,#19397,#19398,#19399,#19400));
#5346=EDGE_LOOP('',(#19401,#19402,#19403,#19404,#19405,#19406,#19407,#19408,
#19409,#19410,#19411,#19412,#19413,#19414,#19415,#19416,#19417,#19418,#19419,
#19420,#19421,#19422,#19423,#19424,#19425,#19426,#19427,#19428,#19429,#19430));
#5347=EDGE_LOOP('',(#19431,#19432,#19433,#19434));
#5348=EDGE_LOOP('',(#19435,#19436,#19437,#19438,#19439,#19440,#19441,#19442,
#19443,#19444,#19445,#19446,#19447,#19448,#19449,#19450,#19451,#19452,#19453,
#19454,#19455,#19456,#19457,#19458,#19459,#19460,#19461,#19462,#19463,#19464,
#19465,#19466,#19467,#19468,#19469));
#5349=EDGE_LOOP('',(#19470,#19471,#19472,#19473,#19474,#19475));
#5350=EDGE_LOOP('',(#19476,#19477,#19478,#19479,#19480));
#5351=EDGE_LOOP('',(#19481,#19482,#19483,#19484));
#5352=EDGE_LOOP('',(#19485,#19486,#19487,#19488));
#5353=EDGE_LOOP('',(#19489));
#5354=EDGE_LOOP('',(#19490));
#5355=EDGE_LOOP('',(#19491,#19492,#19493,#19494));
#5356=EDGE_LOOP('',(#19495,#19496,#19497,#19498));
#5357=EDGE_LOOP('',(#19499,#19500,#19501,#19502));
#5358=EDGE_LOOP('',(#19503,#19504,#19505,#19506));
#5359=EDGE_LOOP('',(#19507,#19508,#19509,#19510));
#5360=EDGE_LOOP('',(#19511));
#5361=EDGE_LOOP('',(#19512));
#5362=EDGE_LOOP('',(#19513,#19514,#19515,#19516));
#5363=EDGE_LOOP('',(#19517,#19518,#19519,#19520));
#5364=EDGE_LOOP('',(#19521));
#5365=EDGE_LOOP('',(#19522));
#5366=EDGE_LOOP('',(#19523,#19524,#19525,#19526));
#5367=EDGE_LOOP('',(#19527,#19528,#19529,#19530));
#5368=EDGE_LOOP('',(#19531));
#5369=EDGE_LOOP('',(#19532));
#5370=EDGE_LOOP('',(#19533,#19534,#19535,#19536));
#5371=EDGE_LOOP('',(#19537,#19538,#19539,#19540));
#5372=EDGE_LOOP('',(#19541));
#5373=EDGE_LOOP('',(#19542));
#5374=EDGE_LOOP('',(#19543,#19544,#19545,#19546,#19547,#19548));
#5375=EDGE_LOOP('',(#19549,#19550,#19551,#19552,#19553));
#5376=EDGE_LOOP('',(#19554,#19555,#19556));
#5377=EDGE_LOOP('',(#19557,#19558,#19559));
#5378=EDGE_LOOP('',(#19560,#19561,#19562));
#5379=EDGE_LOOP('',(#19563,#19564,#19565));
#5380=EDGE_LOOP('',(#19566,#19567,#19568,#19569));
#5381=EDGE_LOOP('',(#19570,#19571,#19572,#19573));
#5382=EDGE_LOOP('',(#19574,#19575,#19576,#19577));
#5383=EDGE_LOOP('',(#19578,#19579,#19580,#19581,#19582));
#5384=EDGE_LOOP('',(#19583,#19584,#19585,#19586));
#5385=EDGE_LOOP('',(#19587,#19588,#19589,#19590));
#5386=EDGE_LOOP('',(#19591,#19592,#19593,#19594));
#5387=EDGE_LOOP('',(#19595,#19596,#19597,#19598));
#5388=EDGE_LOOP('',(#19599,#19600,#19601,#19602,#19603,#19604));
#5389=EDGE_LOOP('',(#19605));
#5390=EDGE_LOOP('',(#19606));
#5391=EDGE_LOOP('',(#19607));
#5392=EDGE_LOOP('',(#19608));
#5393=EDGE_LOOP('',(#19609));
#5394=EDGE_LOOP('',(#19610));
#5395=EDGE_LOOP('',(#19611));
#5396=EDGE_LOOP('',(#19612));
#5397=EDGE_LOOP('',(#19613));
#5398=EDGE_LOOP('',(#19614));
#5399=EDGE_LOOP('',(#19615));
#5400=EDGE_LOOP('',(#19616));
#5401=EDGE_LOOP('',(#19617));
#5402=EDGE_LOOP('',(#19618));
#5403=EDGE_LOOP('',(#19619));
#5404=EDGE_LOOP('',(#19620));
#5405=EDGE_LOOP('',(#19621));
#5406=EDGE_LOOP('',(#19622,#19623,#19624,#19625));
#5407=EDGE_LOOP('',(#19626,#19627,#19628,#19629,#19630,#19631));
#5408=EDGE_LOOP('',(#19632));
#5409=EDGE_LOOP('',(#19633));
#5410=EDGE_LOOP('',(#19634));
#5411=EDGE_LOOP('',(#19635));
#5412=EDGE_LOOP('',(#19636));
#5413=EDGE_LOOP('',(#19637,#19638,#19639,#19640));
#5414=EDGE_LOOP('',(#19641,#19642,#19643,#19644));
#5415=EDGE_LOOP('',(#19645,#19646,#19647,#19648));
#5416=EDGE_LOOP('',(#19649,#19650,#19651,#19652));
#5417=EDGE_LOOP('',(#19653,#19654,#19655,#19656));
#5418=EDGE_LOOP('',(#19657,#19658,#19659,#19660));
#5419=EDGE_LOOP('',(#19661,#19662,#19663,#19664));
#5420=EDGE_LOOP('',(#19665,#19666,#19667,#19668));
#5421=EDGE_LOOP('',(#19669,#19670,#19671,#19672));
#5422=EDGE_LOOP('',(#19673,#19674,#19675,#19676));
#5423=EDGE_LOOP('',(#19677,#19678,#19679,#19680));
#5424=EDGE_LOOP('',(#19681,#19682,#19683,#19684));
#5425=EDGE_LOOP('',(#19685,#19686,#19687,#19688,#19689,#19690,#19691,#19692,
#19693,#19694,#19695,#19696));
#5426=EDGE_LOOP('',(#19697,#19698,#19699,#19700));
#5427=EDGE_LOOP('',(#19701,#19702,#19703,#19704));
#5428=EDGE_LOOP('',(#19705,#19706,#19707,#19708));
#5429=EDGE_LOOP('',(#19709,#19710,#19711,#19712));
#5430=EDGE_LOOP('',(#19713,#19714,#19715,#19716));
#5431=EDGE_LOOP('',(#19717,#19718,#19719,#19720));
#5432=EDGE_LOOP('',(#19721,#19722,#19723,#19724));
#5433=EDGE_LOOP('',(#19725,#19726,#19727,#19728));
#5434=EDGE_LOOP('',(#19729,#19730,#19731,#19732));
#5435=EDGE_LOOP('',(#19733,#19734,#19735,#19736));
#5436=EDGE_LOOP('',(#19737,#19738,#19739,#19740));
#5437=EDGE_LOOP('',(#19741,#19742,#19743,#19744));
#5438=EDGE_LOOP('',(#19745,#19746,#19747,#19748));
#5439=EDGE_LOOP('',(#19749,#19750,#19751,#19752));
#5440=EDGE_LOOP('',(#19753,#19754,#19755,#19756));
#5441=EDGE_LOOP('',(#19757,#19758,#19759,#19760));
#5442=EDGE_LOOP('',(#19761,#19762,#19763,#19764));
#5443=EDGE_LOOP('',(#19765,#19766,#19767,#19768));
#5444=EDGE_LOOP('',(#19769,#19770,#19771,#19772));
#5445=EDGE_LOOP('',(#19773,#19774,#19775,#19776,#19777,#19778,#19779,#19780,
#19781,#19782,#19783,#19784,#19785,#19786,#19787,#19788,#19789,#19790,#19791));
#5446=EDGE_LOOP('',(#19792,#19793,#19794,#19795));
#5447=EDGE_LOOP('',(#19796,#19797,#19798,#19799));
#5448=EDGE_LOOP('',(#19800,#19801,#19802,#19803));
#5449=EDGE_LOOP('',(#19804,#19805,#19806,#19807));
#5450=EDGE_LOOP('',(#19808,#19809,#19810,#19811));
#5451=EDGE_LOOP('',(#19812,#19813,#19814,#19815));
#5452=EDGE_LOOP('',(#19816,#19817,#19818,#19819));
#5453=EDGE_LOOP('',(#19820,#19821,#19822,#19823));
#5454=EDGE_LOOP('',(#19824,#19825,#19826,#19827));
#5455=EDGE_LOOP('',(#19828,#19829,#19830,#19831));
#5456=EDGE_LOOP('',(#19832,#19833,#19834,#19835));
#5457=EDGE_LOOP('',(#19836,#19837,#19838,#19839));
#5458=EDGE_LOOP('',(#19840,#19841,#19842,#19843,#19844,#19845,#19846,#19847,
#19848,#19849,#19850,#19851));
#5459=EDGE_LOOP('',(#19852,#19853,#19854,#19855));
#5460=EDGE_LOOP('',(#19856,#19857,#19858,#19859));
#5461=EDGE_LOOP('',(#19860,#19861,#19862,#19863));
#5462=EDGE_LOOP('',(#19864,#19865,#19866,#19867));
#5463=EDGE_LOOP('',(#19868,#19869,#19870,#19871));
#5464=EDGE_LOOP('',(#19872,#19873,#19874,#19875));
#5465=EDGE_LOOP('',(#19876,#19877,#19878,#19879));
#5466=EDGE_LOOP('',(#19880,#19881,#19882,#19883));
#5467=EDGE_LOOP('',(#19884,#19885,#19886,#19887));
#5468=EDGE_LOOP('',(#19888,#19889,#19890,#19891));
#5469=EDGE_LOOP('',(#19892,#19893,#19894,#19895));
#5470=EDGE_LOOP('',(#19896,#19897,#19898,#19899,#19900,#19901,#19902,#19903,
#19904,#19905,#19906));
#5471=EDGE_LOOP('',(#19907,#19908,#19909,#19910));
#5472=EDGE_LOOP('',(#19911,#19912,#19913,#19914));
#5473=EDGE_LOOP('',(#19915,#19916,#19917,#19918));
#5474=EDGE_LOOP('',(#19919,#19920,#19921,#19922));
#5475=EDGE_LOOP('',(#19923,#19924,#19925,#19926));
#5476=EDGE_LOOP('',(#19927,#19928,#19929,#19930));
#5477=EDGE_LOOP('',(#19931,#19932,#19933,#19934));
#5478=EDGE_LOOP('',(#19935,#19936,#19937,#19938));
#5479=EDGE_LOOP('',(#19939,#19940,#19941,#19942));
#5480=EDGE_LOOP('',(#19943,#19944,#19945,#19946));
#5481=EDGE_LOOP('',(#19947,#19948,#19949,#19950));
#5482=EDGE_LOOP('',(#19951,#19952,#19953,#19954));
#5483=EDGE_LOOP('',(#19955,#19956,#19957,#19958));
#5484=EDGE_LOOP('',(#19959,#19960,#19961,#19962));
#5485=EDGE_LOOP('',(#19963,#19964,#19965,#19966));
#5486=EDGE_LOOP('',(#19967,#19968,#19969,#19970));
#5487=EDGE_LOOP('',(#19971,#19972,#19973,#19974));
#5488=EDGE_LOOP('',(#19975,#19976,#19977,#19978));
#5489=EDGE_LOOP('',(#19979,#19980,#19981,#19982));
#5490=EDGE_LOOP('',(#19983,#19984,#19985,#19986));
#5491=EDGE_LOOP('',(#19987,#19988,#19989,#19990));
#5492=EDGE_LOOP('',(#19991,#19992,#19993,#19994));
#5493=EDGE_LOOP('',(#19995,#19996,#19997,#19998));
#5494=EDGE_LOOP('',(#19999,#20000,#20001,#20002));
#5495=EDGE_LOOP('',(#20003,#20004,#20005,#20006));
#5496=EDGE_LOOP('',(#20007,#20008,#20009,#20010));
#5497=EDGE_LOOP('',(#20011,#20012,#20013,#20014));
#5498=EDGE_LOOP('',(#20015,#20016,#20017,#20018));
#5499=EDGE_LOOP('',(#20019,#20020,#20021,#20022));
#5500=EDGE_LOOP('',(#20023,#20024,#20025,#20026));
#5501=EDGE_LOOP('',(#20027,#20028,#20029,#20030));
#5502=EDGE_LOOP('',(#20031,#20032,#20033,#20034));
#5503=EDGE_LOOP('',(#20035,#20036,#20037,#20038));
#5504=EDGE_LOOP('',(#20039,#20040,#20041,#20042));
#5505=EDGE_LOOP('',(#20043,#20044,#20045,#20046));
#5506=EDGE_LOOP('',(#20047,#20048,#20049,#20050,#20051,#20052,#20053,#20054,
#20055,#20056,#20057,#20058,#20059,#20060,#20061,#20062,#20063,#20064,#20065,
#20066,#20067,#20068,#20069,#20070,#20071,#20072,#20073,#20074,#20075,#20076,
#20077,#20078,#20079,#20080,#20081));
#5507=EDGE_LOOP('',(#20082,#20083,#20084,#20085));
#5508=EDGE_LOOP('',(#20086,#20087,#20088,#20089));
#5509=EDGE_LOOP('',(#20090,#20091,#20092,#20093));
#5510=EDGE_LOOP('',(#20094,#20095,#20096,#20097));
#5511=EDGE_LOOP('',(#20098,#20099,#20100,#20101));
#5512=EDGE_LOOP('',(#20102,#20103,#20104,#20105));
#5513=EDGE_LOOP('',(#20106,#20107,#20108,#20109));
#5514=EDGE_LOOP('',(#20110,#20111,#20112,#20113));
#5515=EDGE_LOOP('',(#20114,#20115,#20116,#20117));
#5516=EDGE_LOOP('',(#20118,#20119,#20120,#20121));
#5517=EDGE_LOOP('',(#20122,#20123,#20124,#20125));
#5518=EDGE_LOOP('',(#20126,#20127,#20128,#20129));
#5519=EDGE_LOOP('',(#20130,#20131,#20132,#20133));
#5520=EDGE_LOOP('',(#20134,#20135,#20136,#20137));
#5521=EDGE_LOOP('',(#20138,#20139,#20140,#20141));
#5522=EDGE_LOOP('',(#20142,#20143,#20144,#20145));
#5523=EDGE_LOOP('',(#20146,#20147,#20148,#20149));
#5524=EDGE_LOOP('',(#20150,#20151,#20152,#20153));
#5525=EDGE_LOOP('',(#20154,#20155,#20156,#20157));
#5526=EDGE_LOOP('',(#20158,#20159,#20160,#20161));
#5527=EDGE_LOOP('',(#20162,#20163,#20164,#20165));
#5528=EDGE_LOOP('',(#20166,#20167,#20168,#20169));
#5529=EDGE_LOOP('',(#20170,#20171,#20172,#20173));
#5530=EDGE_LOOP('',(#20174,#20175,#20176,#20177));
#5531=EDGE_LOOP('',(#20178,#20179,#20180,#20181));
#5532=EDGE_LOOP('',(#20182,#20183,#20184,#20185));
#5533=EDGE_LOOP('',(#20186,#20187,#20188,#20189));
#5534=EDGE_LOOP('',(#20190,#20191,#20192,#20193));
#5535=EDGE_LOOP('',(#20194,#20195,#20196,#20197));
#5536=EDGE_LOOP('',(#20198,#20199,#20200,#20201));
#5537=EDGE_LOOP('',(#20202,#20203,#20204,#20205,#20206,#20207,#20208,#20209,
#20210,#20211,#20212,#20213,#20214,#20215,#20216,#20217,#20218,#20219,#20220,
#20221,#20222,#20223,#20224,#20225,#20226,#20227,#20228,#20229,#20230,#20231));
#5538=EDGE_LOOP('',(#20232,#20233,#20234,#20235));
#5539=EDGE_LOOP('',(#20236,#20237,#20238,#20239));
#5540=EDGE_LOOP('',(#20240,#20241,#20242,#20243));
#5541=EDGE_LOOP('',(#20244,#20245,#20246,#20247));
#5542=EDGE_LOOP('',(#20248,#20249,#20250,#20251));
#5543=EDGE_LOOP('',(#20252,#20253,#20254,#20255));
#5544=EDGE_LOOP('',(#20256,#20257,#20258,#20259));
#5545=EDGE_LOOP('',(#20260,#20261,#20262,#20263));
#5546=EDGE_LOOP('',(#20264,#20265,#20266,#20267));
#5547=EDGE_LOOP('',(#20268,#20269,#20270,#20271));
#5548=EDGE_LOOP('',(#20272,#20273,#20274,#20275));
#5549=EDGE_LOOP('',(#20276,#20277,#20278,#20279));
#5550=EDGE_LOOP('',(#20280,#20281,#20282,#20283));
#5551=EDGE_LOOP('',(#20284,#20285,#20286,#20287));
#5552=EDGE_LOOP('',(#20288,#20289,#20290,#20291));
#5553=EDGE_LOOP('',(#20292,#20293,#20294,#20295));
#5554=EDGE_LOOP('',(#20296,#20297,#20298,#20299));
#5555=EDGE_LOOP('',(#20300,#20301,#20302,#20303));
#5556=EDGE_LOOP('',(#20304,#20305,#20306,#20307));
#5557=EDGE_LOOP('',(#20308,#20309,#20310,#20311));
#5558=EDGE_LOOP('',(#20312,#20313,#20314,#20315));
#5559=EDGE_LOOP('',(#20316,#20317,#20318,#20319));
#5560=EDGE_LOOP('',(#20320,#20321,#20322,#20323));
#5561=EDGE_LOOP('',(#20324,#20325,#20326,#20327));
#5562=EDGE_LOOP('',(#20328,#20329,#20330,#20331));
#5563=EDGE_LOOP('',(#20332,#20333,#20334,#20335));
#5564=EDGE_LOOP('',(#20336,#20337,#20338,#20339));
#5565=EDGE_LOOP('',(#20340,#20341,#20342,#20343));
#5566=EDGE_LOOP('',(#20344,#20345,#20346,#20347));
#5567=EDGE_LOOP('',(#20348,#20349,#20350,#20351));
#5568=EDGE_LOOP('',(#20352,#20353,#20354,#20355));
#5569=EDGE_LOOP('',(#20356,#20357,#20358,#20359));
#5570=EDGE_LOOP('',(#20360,#20361,#20362,#20363));
#5571=EDGE_LOOP('',(#20364,#20365,#20366,#20367));
#5572=EDGE_LOOP('',(#20368,#20369,#20370,#20371));
#5573=EDGE_LOOP('',(#20372,#20373,#20374,#20375));
#5574=EDGE_LOOP('',(#20376,#20377,#20378,#20379));
#5575=EDGE_LOOP('',(#20380,#20381,#20382,#20383));
#5576=EDGE_LOOP('',(#20384,#20385,#20386,#20387));
#5577=EDGE_LOOP('',(#20388,#20389,#20390,#20391));
#5578=EDGE_LOOP('',(#20392,#20393,#20394,#20395,#20396,#20397,#20398,#20399,
#20400,#20401,#20402,#20403,#20404,#20405,#20406,#20407,#20408,#20409,#20410,
#20411,#20412,#20413,#20414,#20415,#20416,#20417,#20418,#20419,#20420,#20421,
#20422,#20423,#20424,#20425,#20426));
#5579=EDGE_LOOP('',(#20427,#20428,#20429,#20430));
#5580=EDGE_LOOP('',(#20431,#20432,#20433,#20434));
#5581=EDGE_LOOP('',(#20435,#20436,#20437,#20438));
#5582=EDGE_LOOP('',(#20439,#20440,#20441,#20442));
#5583=EDGE_LOOP('',(#20443,#20444,#20445,#20446));
#5584=EDGE_LOOP('',(#20447,#20448,#20449,#20450));
#5585=EDGE_LOOP('',(#20451,#20452,#20453,#20454));
#5586=EDGE_LOOP('',(#20455,#20456,#20457,#20458));
#5587=EDGE_LOOP('',(#20459,#20460,#20461,#20462));
#5588=EDGE_LOOP('',(#20463,#20464,#20465,#20466));
#5589=EDGE_LOOP('',(#20467,#20468,#20469,#20470));
#5590=EDGE_LOOP('',(#20471,#20472,#20473,#20474));
#5591=EDGE_LOOP('',(#20475,#20476,#20477,#20478));
#5592=EDGE_LOOP('',(#20479,#20480,#20481,#20482));
#5593=EDGE_LOOP('',(#20483,#20484,#20485,#20486));
#5594=EDGE_LOOP('',(#20487,#20488,#20489,#20490));
#5595=EDGE_LOOP('',(#20491,#20492,#20493,#20494));
#5596=EDGE_LOOP('',(#20495,#20496,#20497,#20498));
#5597=EDGE_LOOP('',(#20499,#20500,#20501,#20502));
#5598=EDGE_LOOP('',(#20503,#20504,#20505,#20506));
#5599=EDGE_LOOP('',(#20507,#20508,#20509,#20510));
#5600=EDGE_LOOP('',(#20511,#20512,#20513,#20514));
#5601=EDGE_LOOP('',(#20515,#20516,#20517,#20518));
#5602=EDGE_LOOP('',(#20519,#20520,#20521,#20522));
#5603=EDGE_LOOP('',(#20523,#20524,#20525,#20526));
#5604=EDGE_LOOP('',(#20527,#20528,#20529,#20530));
#5605=EDGE_LOOP('',(#20531,#20532,#20533,#20534));
#5606=EDGE_LOOP('',(#20535,#20536,#20537,#20538));
#5607=EDGE_LOOP('',(#20539,#20540,#20541,#20542));
#5608=EDGE_LOOP('',(#20543,#20544,#20545,#20546));
#5609=EDGE_LOOP('',(#20547,#20548,#20549,#20550));
#5610=EDGE_LOOP('',(#20551,#20552,#20553,#20554));
#5611=EDGE_LOOP('',(#20555,#20556,#20557,#20558));
#5612=EDGE_LOOP('',(#20559,#20560,#20561,#20562));
#5613=EDGE_LOOP('',(#20563,#20564,#20565,#20566));
#5614=EDGE_LOOP('',(#20567,#20568,#20569,#20570));
#5615=EDGE_LOOP('',(#20571,#20572,#20573,#20574));
#5616=EDGE_LOOP('',(#20575,#20576,#20577,#20578));
#5617=EDGE_LOOP('',(#20579));
#5618=EDGE_LOOP('',(#20580));
#5619=EDGE_LOOP('',(#20581));
#5620=EDGE_LOOP('',(#20582));
#5621=EDGE_LOOP('',(#20583));
#5622=EDGE_LOOP('',(#20584));
#5623=EDGE_LOOP('',(#20585));
#5624=EDGE_LOOP('',(#20586));
#5625=EDGE_LOOP('',(#20587));
#5626=EDGE_LOOP('',(#20588));
#5627=EDGE_LOOP('',(#20589));
#5628=EDGE_LOOP('',(#20590));
#5629=EDGE_LOOP('',(#20591));
#5630=EDGE_LOOP('',(#20592));
#5631=EDGE_LOOP('',(#20593,#20594,#20595,#20596));
#5632=EDGE_LOOP('',(#20597));
#5633=EDGE_LOOP('',(#20598));
#5634=EDGE_LOOP('',(#20599,#20600,#20601,#20602));
#5635=EDGE_LOOP('',(#20603,#20604,#20605,#20606));
#5636=EDGE_LOOP('',(#20607,#20608,#20609,#20610,#20611,#20612,#20613,#20614,
#20615,#20616,#20617,#20618,#20619,#20620,#20621,#20622,#20623,#20624,#20625,
#20626,#20627,#20628,#20629,#20630,#20631));
#5637=EDGE_LOOP('',(#20632));
#5638=EDGE_LOOP('',(#20633));
#5639=EDGE_LOOP('',(#20634));
#5640=EDGE_LOOP('',(#20635));
#5641=EDGE_LOOP('',(#20636));
#5642=EDGE_LOOP('',(#20637));
#5643=EDGE_LOOP('',(#20638));
#5644=EDGE_LOOP('',(#20639));
#5645=EDGE_LOOP('',(#20640));
#5646=EDGE_LOOP('',(#20641));
#5647=EDGE_LOOP('',(#20642,#20643,#20644,#20645));
#5648=EDGE_LOOP('',(#20646,#20647,#20648,#20649));
#5649=EDGE_LOOP('',(#20650,#20651,#20652,#20653));
#5650=EDGE_LOOP('',(#20654,#20655,#20656,#20657));
#5651=EDGE_LOOP('',(#20658,#20659,#20660,#20661));
#5652=EDGE_LOOP('',(#20662,#20663,#20664,#20665));
#5653=EDGE_LOOP('',(#20666,#20667,#20668,#20669));
#5654=EDGE_LOOP('',(#20670,#20671,#20672,#20673,#20674));
#5655=EDGE_LOOP('',(#20675,#20676,#20677,#20678,#20679,#20680));
#5656=EDGE_LOOP('',(#20681,#20682,#20683,#20684,#20685));
#5657=EDGE_LOOP('',(#20686,#20687,#20688));
#5658=EDGE_LOOP('',(#20689,#20690,#20691,#20692));
#5659=EDGE_LOOP('',(#20693,#20694,#20695,#20696));
#5660=EDGE_LOOP('',(#20697,#20698,#20699,#20700));
#5661=EDGE_LOOP('',(#20701,#20702,#20703,#20704));
#5662=EDGE_LOOP('',(#20705,#20706,#20707,#20708));
#5663=EDGE_LOOP('',(#20709,#20710,#20711,#20712,#20713));
#5664=EDGE_LOOP('',(#20714,#20715,#20716,#20717));
#5665=EDGE_LOOP('',(#20718,#20719,#20720,#20721));
#5666=EDGE_LOOP('',(#20722,#20723,#20724,#20725));
#5667=EDGE_LOOP('',(#20726,#20727,#20728,#20729));
#5668=EDGE_LOOP('',(#20730,#20731,#20732,#20733,#20734,#20735));
#5669=EDGE_LOOP('',(#20736,#20737,#20738,#20739,#20740));
#5670=EDGE_LOOP('',(#20741,#20742,#20743,#20744));
#5671=EDGE_LOOP('',(#20745,#20746,#20747,#20748,#20749,#20750,#20751,#20752,
#20753,#20754,#20755,#20756,#20757,#20758,#20759,#20760,#20761,#20762,#20763,
#20764,#20765));
#5672=EDGE_LOOP('',(#20766));
#5673=EDGE_LOOP('',(#20767));
#5674=EDGE_LOOP('',(#20768));
#5675=EDGE_LOOP('',(#20769));
#5676=EDGE_LOOP('',(#20770,#20771,#20772,#20773));
#5677=EDGE_LOOP('',(#20774,#20775,#20776,#20777));
#5678=EDGE_LOOP('',(#20778,#20779,#20780,#20781));
#5679=EDGE_LOOP('',(#20782,#20783,#20784,#20785));
#5680=EDGE_LOOP('',(#20786,#20787,#20788,#20789));
#5681=EDGE_LOOP('',(#20790,#20791,#20792,#20793));
#5682=EDGE_LOOP('',(#20794,#20795,#20796,#20797));
#5683=EDGE_LOOP('',(#20798,#20799,#20800,#20801));
#5684=EDGE_LOOP('',(#20802,#20803,#20804,#20805));
#5685=EDGE_LOOP('',(#20806,#20807,#20808,#20809));
#5686=EDGE_LOOP('',(#20810,#20811,#20812,#20813));
#5687=EDGE_LOOP('',(#20814,#20815,#20816,#20817));
#5688=EDGE_LOOP('',(#20818,#20819,#20820,#20821));
#5689=EDGE_LOOP('',(#20822,#20823,#20824,#20825));
#5690=EDGE_LOOP('',(#20826,#20827,#20828,#20829));
#5691=EDGE_LOOP('',(#20830,#20831,#20832,#20833));
#5692=EDGE_LOOP('',(#20834,#20835,#20836,#20837,#20838));
#5693=EDGE_LOOP('',(#20839,#20840,#20841,#20842));
#5694=EDGE_LOOP('',(#20843,#20844,#20845,#20846));
#5695=EDGE_LOOP('',(#20847,#20848,#20849,#20850));
#5696=EDGE_LOOP('',(#20851,#20852,#20853,#20854));
#5697=EDGE_LOOP('',(#20855,#20856,#20857,#20858));
#5698=EDGE_LOOP('',(#20859,#20860,#20861,#20862));
#5699=EDGE_LOOP('',(#20863,#20864,#20865,#20866));
#5700=EDGE_LOOP('',(#20867,#20868,#20869,#20870));
#5701=EDGE_LOOP('',(#20871,#20872,#20873,#20874));
#5702=EDGE_LOOP('',(#20875,#20876,#20877,#20878));
#5703=EDGE_LOOP('',(#20879,#20880,#20881,#20882,#20883,#20884));
#5704=EDGE_LOOP('',(#20885,#20886,#20887,#20888,#20889,#20890,#20891,#20892,
#20893,#20894));
#5705=EDGE_LOOP('',(#20895));
#5706=EDGE_LOOP('',(#20896,#20897,#20898,#20899,#20900,#20901,#20902,#20903));
#5707=EDGE_LOOP('',(#20904,#20905,#20906,#20907));
#5708=EDGE_LOOP('',(#20908,#20909,#20910,#20911));
#5709=EDGE_LOOP('',(#20912,#20913,#20914,#20915));
#5710=EDGE_LOOP('',(#20916,#20917,#20918,#20919));
#5711=EDGE_LOOP('',(#20920,#20921,#20922,#20923));
#5712=EDGE_LOOP('',(#20924,#20925,#20926,#20927));
#5713=EDGE_LOOP('',(#20928,#20929,#20930,#20931));
#5714=EDGE_LOOP('',(#20932,#20933,#20934,#20935));
#5715=EDGE_LOOP('',(#20936,#20937,#20938,#20939));
#5716=EDGE_LOOP('',(#20940,#20941,#20942,#20943));
#5717=EDGE_LOOP('',(#20944,#20945,#20946,#20947));
#5718=EDGE_LOOP('',(#20948,#20949,#20950,#20951));
#5719=EDGE_LOOP('',(#20952,#20953,#20954,#20955));
#5720=EDGE_LOOP('',(#20956,#20957,#20958,#20959));
#5721=EDGE_LOOP('',(#20960,#20961,#20962,#20963));
#5722=EDGE_LOOP('',(#20964,#20965,#20966,#20967));
#5723=EDGE_LOOP('',(#20968,#20969,#20970,#20971));
#5724=EDGE_LOOP('',(#20972,#20973,#20974,#20975));
#5725=EDGE_LOOP('',(#20976,#20977,#20978,#20979));
#5726=EDGE_LOOP('',(#20980,#20981,#20982,#20983));
#5727=EDGE_LOOP('',(#20984,#20985,#20986,#20987,#20988,#20989,#20990));
#5728=EDGE_LOOP('',(#20991,#20992,#20993,#20994));
#5729=EDGE_LOOP('',(#20995,#20996,#20997,#20998));
#5730=EDGE_LOOP('',(#20999,#21000,#21001,#21002));
#5731=EDGE_LOOP('',(#21003,#21004,#21005,#21006));
#5732=EDGE_LOOP('',(#21007,#21008,#21009,#21010));
#5733=EDGE_LOOP('',(#21011,#21012,#21013,#21014));
#5734=EDGE_LOOP('',(#21015,#21016,#21017,#21018));
#5735=EDGE_LOOP('',(#21019,#21020,#21021,#21022));
#5736=EDGE_LOOP('',(#21023,#21024,#21025,#21026));
#5737=EDGE_LOOP('',(#21027,#21028,#21029,#21030));
#5738=EDGE_LOOP('',(#21031,#21032,#21033,#21034));
#5739=EDGE_LOOP('',(#21035,#21036,#21037,#21038));
#5740=EDGE_LOOP('',(#21039,#21040,#21041,#21042));
#5741=EDGE_LOOP('',(#21043,#21044,#21045,#21046));
#5742=EDGE_LOOP('',(#21047,#21048,#21049,#21050));
#5743=EDGE_LOOP('',(#21051,#21052,#21053,#21054));
#5744=EDGE_LOOP('',(#21055,#21056,#21057,#21058));
#5745=EDGE_LOOP('',(#21059,#21060,#21061,#21062,#21063,#21064));
#5746=EDGE_LOOP('',(#21065,#21066,#21067,#21068,#21069));
#5747=EDGE_LOOP('',(#21070));
#5748=EDGE_LOOP('',(#21071,#21072,#21073,#21074,#21075,#21076,#21077,#21078,
#21079,#21080,#21081));
#5749=EDGE_LOOP('',(#21082,#21083));
#5750=EDGE_LOOP('',(#21084));
#5751=EDGE_LOOP('',(#21085,#21086,#21087,#21088));
#5752=EDGE_LOOP('',(#21089));
#5753=EDGE_LOOP('',(#21090));
#5754=EDGE_LOOP('',(#21091));
#5755=EDGE_LOOP('',(#21092,#21093,#21094,#21095));
#5756=EDGE_LOOP('',(#21096));
#5757=EDGE_LOOP('',(#21097,#21098,#21099,#21100));
#5758=EDGE_LOOP('',(#21101));
#5759=EDGE_LOOP('',(#21102,#21103,#21104,#21105));
#5760=EDGE_LOOP('',(#21106));
#5761=EDGE_LOOP('',(#21107,#21108,#21109,#21110));
#5762=EDGE_LOOP('',(#21111,#21112,#21113,#21114));
#5763=EDGE_LOOP('',(#21115,#21116,#21117,#21118));
#5764=EDGE_LOOP('',(#21119,#21120,#21121,#21122));
#5765=EDGE_LOOP('',(#21123,#21124,#21125,#21126));
#5766=EDGE_LOOP('',(#21127));
#5767=EDGE_LOOP('',(#21128));
#5768=EDGE_LOOP('',(#21129,#21130,#21131,#21132));
#5769=EDGE_LOOP('',(#21133,#21134,#21135,#21136));
#5770=EDGE_LOOP('',(#21137));
#5771=EDGE_LOOP('',(#21138));
#5772=EDGE_LOOP('',(#21139,#21140,#21141,#21142));
#5773=EDGE_LOOP('',(#21143,#21144,#21145,#21146));
#5774=EDGE_LOOP('',(#21147));
#5775=EDGE_LOOP('',(#21148));
#5776=EDGE_LOOP('',(#21149,#21150,#21151,#21152));
#5777=EDGE_LOOP('',(#21153,#21154,#21155,#21156));
#5778=EDGE_LOOP('',(#21157));
#5779=EDGE_LOOP('',(#21158));
#5780=EDGE_LOOP('',(#21159,#21160,#21161,#21162));
#5781=EDGE_LOOP('',(#21163,#21164,#21165,#21166));
#5782=EDGE_LOOP('',(#21167));
#5783=EDGE_LOOP('',(#21168));
#5784=EDGE_LOOP('',(#21169,#21170,#21171,#21172));
#5785=EDGE_LOOP('',(#21173,#21174,#21175,#21176));
#5786=EDGE_LOOP('',(#21177));
#5787=EDGE_LOOP('',(#21178));
#5788=EDGE_LOOP('',(#21179,#21180,#21181,#21182));
#5789=EDGE_LOOP('',(#21183,#21184,#21185,#21186));
#5790=EDGE_LOOP('',(#21187));
#5791=EDGE_LOOP('',(#21188));
#5792=EDGE_LOOP('',(#21189,#21190,#21191,#21192));
#5793=EDGE_LOOP('',(#21193,#21194,#21195,#21196));
#5794=EDGE_LOOP('',(#21197));
#5795=EDGE_LOOP('',(#21198));
#5796=EDGE_LOOP('',(#21199,#21200,#21201,#21202));
#5797=EDGE_LOOP('',(#21203,#21204,#21205,#21206));
#5798=EDGE_LOOP('',(#21207));
#5799=EDGE_LOOP('',(#21208));
#5800=EDGE_LOOP('',(#21209,#21210,#21211,#21212,#21213,#21214));
#5801=EDGE_LOOP('',(#21215,#21216,#21217,#21218,#21219,#21220));
#5802=EDGE_LOOP('',(#21221,#21222,#21223,#21224));
#5803=EDGE_LOOP('',(#21225,#21226,#21227,#21228,#21229,#21230));
#5804=EDGE_LOOP('',(#21231,#21232,#21233,#21234));
#5805=EDGE_LOOP('',(#21235,#21236,#21237,#21238));
#5806=EDGE_LOOP('',(#21239));
#5807=EDGE_LOOP('',(#21240));
#5808=EDGE_LOOP('',(#21241,#21242,#21243,#21244));
#5809=EDGE_LOOP('',(#21245,#21246,#21247,#21248));
#5810=EDGE_LOOP('',(#21249));
#5811=EDGE_LOOP('',(#21250));
#5812=EDGE_LOOP('',(#21251,#21252,#21253,#21254,#21255,#21256));
#5813=EDGE_LOOP('',(#21257,#21258,#21259,#21260,#21261,#21262));
#5814=EDGE_LOOP('',(#21263,#21264,#21265,#21266));
#5815=EDGE_LOOP('',(#21267,#21268,#21269,#21270,#21271,#21272));
#5816=EDGE_LOOP('',(#21273,#21274,#21275,#21276,#21277,#21278));
#5817=EDGE_LOOP('',(#21279,#21280,#21281,#21282,#21283,#21284));
#5818=EDGE_LOOP('',(#21285,#21286,#21287,#21288));
#5819=EDGE_LOOP('',(#21289,#21290,#21291,#21292));
#5820=EDGE_LOOP('',(#21293));
#5821=EDGE_LOOP('',(#21294));
#5822=EDGE_LOOP('',(#21295,#21296,#21297,#21298));
#5823=EDGE_LOOP('',(#21299,#21300,#21301,#21302));
#5824=EDGE_LOOP('',(#21303));
#5825=EDGE_LOOP('',(#21304));
#5826=EDGE_LOOP('',(#21305,#21306,#21307,#21308));
#5827=EDGE_LOOP('',(#21309,#21310,#21311,#21312));
#5828=EDGE_LOOP('',(#21313));
#5829=EDGE_LOOP('',(#21314));
#5830=EDGE_LOOP('',(#21315));
#5831=EDGE_LOOP('',(#21316));
#5832=EDGE_LOOP('',(#21317));
#5833=EDGE_LOOP('',(#21318));
#5834=EDGE_LOOP('',(#21319));
#5835=EDGE_LOOP('',(#21320));
#5836=EDGE_LOOP('',(#21321));
#5837=EDGE_LOOP('',(#21322));
#5838=EDGE_LOOP('',(#21323));
#5839=EDGE_LOOP('',(#21324));
#5840=EDGE_LOOP('',(#21325));
#5841=EDGE_LOOP('',(#21326));
#5842=EDGE_LOOP('',(#21327));
#5843=EDGE_LOOP('',(#21328));
#5844=EDGE_LOOP('',(#21329));
#5845=EDGE_LOOP('',(#21330));
#5846=EDGE_LOOP('',(#21331));
#5847=EDGE_LOOP('',(#21332));
#5848=EDGE_LOOP('',(#21333));
#5849=EDGE_LOOP('',(#21334));
#5850=EDGE_LOOP('',(#21335));
#5851=EDGE_LOOP('',(#21336));
#5852=EDGE_LOOP('',(#21337));
#5853=EDGE_LOOP('',(#21338));
#5854=EDGE_LOOP('',(#21339));
#5855=EDGE_LOOP('',(#21340));
#5856=EDGE_LOOP('',(#21341));
#5857=EDGE_LOOP('',(#21342));
#5858=EDGE_LOOP('',(#21343));
#5859=EDGE_LOOP('',(#21344));
#5860=EDGE_LOOP('',(#21345));
#5861=EDGE_LOOP('',(#21346));
#5862=EDGE_LOOP('',(#21347));
#5863=EDGE_LOOP('',(#21348));
#5864=EDGE_LOOP('',(#21349));
#5865=EDGE_LOOP('',(#21350));
#5866=EDGE_LOOP('',(#21351));
#5867=EDGE_LOOP('',(#21352));
#5868=EDGE_LOOP('',(#21353));
#5869=EDGE_LOOP('',(#21354));
#5870=EDGE_LOOP('',(#21355,#21356,#21357,#21358));
#5871=EDGE_LOOP('',(#21359,#21360,#21361,#21362));
#5872=EDGE_LOOP('',(#21363,#21364,#21365,#21366));
#5873=EDGE_LOOP('',(#21367,#21368,#21369,#21370));
#5874=EDGE_LOOP('',(#21371,#21372,#21373,#21374));
#5875=EDGE_LOOP('',(#21375,#21376,#21377,#21378));
#5876=EDGE_LOOP('',(#21379,#21380,#21381,#21382));
#5877=EDGE_LOOP('',(#21383,#21384,#21385,#21386));
#5878=EDGE_LOOP('',(#21387,#21388,#21389,#21390));
#5879=EDGE_LOOP('',(#21391,#21392,#21393,#21394));
#5880=EDGE_LOOP('',(#21395,#21396,#21397,#21398));
#5881=EDGE_LOOP('',(#21399,#21400,#21401,#21402));
#5882=EDGE_LOOP('',(#21403,#21404,#21405,#21406));
#5883=EDGE_LOOP('',(#21407,#21408,#21409,#21410,#21411,#21412));
#5884=EDGE_LOOP('',(#21413,#21414,#21415,#21416,#21417,#21418));
#5885=EDGE_LOOP('',(#21419,#21420,#21421,#21422));
#5886=EDGE_LOOP('',(#21423,#21424,#21425,#21426));
#5887=EDGE_LOOP('',(#21427,#21428,#21429,#21430));
#5888=EDGE_LOOP('',(#21431,#21432,#21433,#21434));
#5889=EDGE_LOOP('',(#21435,#21436,#21437,#21438));
#5890=EDGE_LOOP('',(#21439,#21440,#21441,#21442));
#5891=EDGE_LOOP('',(#21443,#21444,#21445,#21446));
#5892=EDGE_LOOP('',(#21447,#21448,#21449,#21450));
#5893=EDGE_LOOP('',(#21451,#21452,#21453,#21454));
#5894=EDGE_LOOP('',(#21455,#21456,#21457,#21458));
#5895=EDGE_LOOP('',(#21459,#21460,#21461,#21462));
#5896=EDGE_LOOP('',(#21463,#21464,#21465,#21466));
#5897=EDGE_LOOP('',(#21467,#21468,#21469,#21470));
#5898=EDGE_LOOP('',(#21471,#21472,#21473,#21474));
#5899=EDGE_LOOP('',(#21475,#21476,#21477,#21478));
#5900=EDGE_LOOP('',(#21479,#21480,#21481,#21482));
#5901=EDGE_LOOP('',(#21483,#21484,#21485,#21486));
#5902=EDGE_LOOP('',(#21487,#21488,#21489,#21490));
#5903=EDGE_LOOP('',(#21491,#21492,#21493,#21494));
#5904=EDGE_LOOP('',(#21495,#21496,#21497,#21498));
#5905=EDGE_LOOP('',(#21499,#21500,#21501,#21502));
#5906=EDGE_LOOP('',(#21503,#21504,#21505,#21506));
#5907=EDGE_LOOP('',(#21507,#21508,#21509,#21510));
#5908=EDGE_LOOP('',(#21511,#21512,#21513,#21514));
#5909=EDGE_LOOP('',(#21515,#21516,#21517,#21518));
#5910=EDGE_LOOP('',(#21519,#21520,#21521,#21522));
#5911=EDGE_LOOP('',(#21523,#21524,#21525,#21526));
#5912=EDGE_LOOP('',(#21527,#21528,#21529,#21530));
#5913=EDGE_LOOP('',(#21531,#21532,#21533,#21534));
#5914=EDGE_LOOP('',(#21535,#21536,#21537,#21538));
#5915=EDGE_LOOP('',(#21539,#21540,#21541,#21542));
#5916=EDGE_LOOP('',(#21543,#21544,#21545,#21546));
#5917=EDGE_LOOP('',(#21547,#21548,#21549,#21550));
#5918=EDGE_LOOP('',(#21551,#21552,#21553,#21554));
#5919=EDGE_LOOP('',(#21555,#21556,#21557,#21558));
#5920=EDGE_LOOP('',(#21559,#21560,#21561,#21562));
#5921=EDGE_LOOP('',(#21563,#21564,#21565,#21566));
#5922=EDGE_LOOP('',(#21567,#21568,#21569,#21570));
#5923=EDGE_LOOP('',(#21571,#21572,#21573,#21574));
#5924=EDGE_LOOP('',(#21575,#21576,#21577,#21578));
#5925=EDGE_LOOP('',(#21579,#21580,#21581,#21582));
#5926=EDGE_LOOP('',(#21583,#21584,#21585,#21586));
#5927=EDGE_LOOP('',(#21587,#21588,#21589,#21590));
#5928=EDGE_LOOP('',(#21591,#21592,#21593,#21594));
#5929=EDGE_LOOP('',(#21595,#21596,#21597,#21598));
#5930=EDGE_LOOP('',(#21599,#21600,#21601,#21602));
#5931=EDGE_LOOP('',(#21603,#21604,#21605,#21606));
#5932=EDGE_LOOP('',(#21607,#21608,#21609,#21610));
#5933=EDGE_LOOP('',(#21611,#21612,#21613,#21614));
#5934=EDGE_LOOP('',(#21615,#21616,#21617,#21618));
#5935=EDGE_LOOP('',(#21619,#21620,#21621,#21622));
#5936=EDGE_LOOP('',(#21623,#21624,#21625,#21626));
#5937=EDGE_LOOP('',(#21627,#21628,#21629,#21630));
#5938=EDGE_LOOP('',(#21631,#21632,#21633,#21634));
#5939=EDGE_LOOP('',(#21635,#21636,#21637,#21638));
#5940=EDGE_LOOP('',(#21639,#21640,#21641,#21642));
#5941=EDGE_LOOP('',(#21643,#21644,#21645,#21646));
#5942=EDGE_LOOP('',(#21647,#21648,#21649,#21650,#21651,#21652));
#5943=EDGE_LOOP('',(#21653,#21654,#21655,#21656,#21657,#21658));
#5944=EDGE_LOOP('',(#21659,#21660,#21661,#21662));
#5945=EDGE_LOOP('',(#21663));
#5946=EDGE_LOOP('',(#21664));
#5947=EDGE_LOOP('',(#21665));
#5948=EDGE_LOOP('',(#21666));
#5949=EDGE_LOOP('',(#21667));
#5950=EDGE_LOOP('',(#21668));
#5951=EDGE_LOOP('',(#21669));
#5952=EDGE_LOOP('',(#21670));
#5953=EDGE_LOOP('',(#21671));
#5954=EDGE_LOOP('',(#21672));
#5955=EDGE_LOOP('',(#21673));
#5956=EDGE_LOOP('',(#21674));
#5957=EDGE_LOOP('',(#21675));
#5958=EDGE_LOOP('',(#21676));
#5959=EDGE_LOOP('',(#21677));
#5960=EDGE_LOOP('',(#21678));
#5961=EDGE_LOOP('',(#21679));
#5962=EDGE_LOOP('',(#21680));
#5963=EDGE_LOOP('',(#21681));
#5964=EDGE_LOOP('',(#21682));
#5965=EDGE_LOOP('',(#21683));
#5966=EDGE_LOOP('',(#21684));
#5967=EDGE_LOOP('',(#21685));
#5968=EDGE_LOOP('',(#21686));
#5969=EDGE_LOOP('',(#21687));
#5970=EDGE_LOOP('',(#21688));
#5971=EDGE_LOOP('',(#21689));
#5972=EDGE_LOOP('',(#21690));
#5973=EDGE_LOOP('',(#21691));
#5974=EDGE_LOOP('',(#21692));
#5975=EDGE_LOOP('',(#21693));
#5976=EDGE_LOOP('',(#21694));
#5977=EDGE_LOOP('',(#21695));
#5978=EDGE_LOOP('',(#21696));
#5979=EDGE_LOOP('',(#21697));
#5980=EDGE_LOOP('',(#21698));
#5981=EDGE_LOOP('',(#21699));
#5982=EDGE_LOOP('',(#21700));
#5983=EDGE_LOOP('',(#21701));
#5984=EDGE_LOOP('',(#21702));
#5985=EDGE_LOOP('',(#21703));
#5986=EDGE_LOOP('',(#21704));
#5987=EDGE_LOOP('',(#21705,#21706,#21707,#21708));
#5988=EDGE_LOOP('',(#21709,#21710,#21711,#21712));
#5989=EDGE_LOOP('',(#21713,#21714,#21715,#21716));
#5990=EDGE_LOOP('',(#21717,#21718,#21719,#21720));
#5991=EDGE_LOOP('',(#21721,#21722,#21723,#21724));
#5992=EDGE_LOOP('',(#21725,#21726,#21727,#21728));
#5993=EDGE_LOOP('',(#21729,#21730,#21731,#21732));
#5994=EDGE_LOOP('',(#21733,#21734,#21735,#21736));
#5995=EDGE_LOOP('',(#21737,#21738,#21739,#21740));
#5996=EDGE_LOOP('',(#21741,#21742,#21743,#21744));
#5997=EDGE_LOOP('',(#21745,#21746,#21747,#21748));
#5998=EDGE_LOOP('',(#21749,#21750,#21751,#21752));
#5999=EDGE_LOOP('',(#21753,#21754,#21755,#21756));
#6000=EDGE_LOOP('',(#21757,#21758,#21759,#21760));
#6001=EDGE_LOOP('',(#21761,#21762,#21763,#21764));
#6002=EDGE_LOOP('',(#21765,#21766,#21767,#21768));
#6003=EDGE_LOOP('',(#21769,#21770,#21771,#21772));
#6004=EDGE_LOOP('',(#21773,#21774,#21775,#21776));
#6005=EDGE_LOOP('',(#21777,#21778,#21779,#21780));
#6006=EDGE_LOOP('',(#21781,#21782,#21783,#21784));
#6007=EDGE_LOOP('',(#21785,#21786,#21787,#21788));
#6008=EDGE_LOOP('',(#21789,#21790,#21791,#21792));
#6009=EDGE_LOOP('',(#21793,#21794,#21795,#21796));
#6010=EDGE_LOOP('',(#21797,#21798,#21799,#21800));
#6011=EDGE_LOOP('',(#21801,#21802,#21803,#21804));
#6012=EDGE_LOOP('',(#21805,#21806,#21807,#21808));
#6013=EDGE_LOOP('',(#21809,#21810,#21811,#21812));
#6014=EDGE_LOOP('',(#21813,#21814,#21815,#21816));
#6015=EDGE_LOOP('',(#21817,#21818,#21819,#21820));
#6016=EDGE_LOOP('',(#21821,#21822,#21823,#21824));
#6017=EDGE_LOOP('',(#21825,#21826,#21827,#21828));
#6018=EDGE_LOOP('',(#21829,#21830,#21831,#21832));
#6019=EDGE_LOOP('',(#21833,#21834,#21835,#21836));
#6020=EDGE_LOOP('',(#21837,#21838,#21839,#21840));
#6021=EDGE_LOOP('',(#21841,#21842,#21843,#21844));
#6022=EDGE_LOOP('',(#21845,#21846,#21847,#21848));
#6023=EDGE_LOOP('',(#21849,#21850,#21851,#21852));
#6024=EDGE_LOOP('',(#21853,#21854,#21855,#21856));
#6025=EDGE_LOOP('',(#21857,#21858,#21859,#21860));
#6026=EDGE_LOOP('',(#21861,#21862,#21863,#21864));
#6027=EDGE_LOOP('',(#21865,#21866,#21867,#21868));
#6028=EDGE_LOOP('',(#21869,#21870,#21871,#21872));
#6029=EDGE_LOOP('',(#21873,#21874,#21875,#21876));
#6030=EDGE_LOOP('',(#21877,#21878,#21879,#21880));
#6031=EDGE_LOOP('',(#21881,#21882,#21883,#21884));
#6032=EDGE_LOOP('',(#21885,#21886,#21887,#21888));
#6033=EDGE_LOOP('',(#21889,#21890,#21891,#21892));
#6034=EDGE_LOOP('',(#21893,#21894,#21895,#21896));
#6035=EDGE_LOOP('',(#21897,#21898,#21899,#21900));
#6036=EDGE_LOOP('',(#21901,#21902,#21903,#21904));
#6037=EDGE_LOOP('',(#21905,#21906,#21907,#21908));
#6038=EDGE_LOOP('',(#21909,#21910,#21911,#21912));
#6039=EDGE_LOOP('',(#21913,#21914,#21915,#21916));
#6040=EDGE_LOOP('',(#21917,#21918,#21919,#21920));
#6041=EDGE_LOOP('',(#21921,#21922,#21923,#21924));
#6042=EDGE_LOOP('',(#21925,#21926,#21927,#21928));
#6043=EDGE_LOOP('',(#21929,#21930,#21931,#21932,#21933,#21934));
#6044=EDGE_LOOP('',(#21935,#21936,#21937,#21938,#21939,#21940,#21941,#21942));
#6045=EDGE_LOOP('',(#21943,#21944,#21945,#21946));
#6046=EDGE_LOOP('',(#21947,#21948,#21949,#21950,#21951,#21952,#21953));
#6047=EDGE_LOOP('',(#21954,#21955,#21956,#21957));
#6048=EDGE_LOOP('',(#21958,#21959,#21960));
#6049=EDGE_LOOP('',(#21961,#21962,#21963));
#6050=EDGE_LOOP('',(#21964,#21965,#21966,#21967));
#6051=EDGE_LOOP('',(#21968,#21969,#21970,#21971,#21972));
#6052=EDGE_LOOP('',(#21973,#21974,#21975));
#6053=EDGE_LOOP('',(#21976,#21977,#21978,#21979,#21980));
#6054=EDGE_LOOP('',(#21981,#21982,#21983,#21984));
#6055=EDGE_LOOP('',(#21985,#21986,#21987,#21988,#21989));
#6056=EDGE_LOOP('',(#21990,#21991,#21992,#21993,#21994));
#6057=EDGE_LOOP('',(#21995,#21996,#21997,#21998));
#6058=EDGE_LOOP('',(#21999));
#6059=EDGE_LOOP('',(#22000));
#6060=EDGE_LOOP('',(#22001,#22002,#22003,#22004));
#6061=EDGE_LOOP('',(#22005));
#6062=EDGE_LOOP('',(#22006));
#6063=EDGE_LOOP('',(#22007,#22008,#22009,#22010,#22011,#22012));
#6064=EDGE_LOOP('',(#22013,#22014,#22015,#22016,#22017));
#6065=EDGE_LOOP('',(#22018,#22019,#22020,#22021));
#6066=EDGE_LOOP('',(#22022,#22023,#22024));
#6067=EDGE_LOOP('',(#22025,#22026,#22027,#22028,#22029));
#6068=EDGE_LOOP('',(#22030,#22031,#22032,#22033,#22034,#22035));
#6069=EDGE_LOOP('',(#22036,#22037,#22038,#22039,#22040));
#6070=EDGE_LOOP('',(#22041,#22042,#22043,#22044));
#6071=EDGE_LOOP('',(#22045));
#6072=EDGE_LOOP('',(#22046,#22047,#22048,#22049));
#6073=EDGE_LOOP('',(#22050));
#6074=EDGE_LOOP('',(#22051));
#6075=EDGE_LOOP('',(#22052));
#6076=EDGE_LOOP('',(#22053));
#6077=EDGE_LOOP('',(#22054));
#6078=EDGE_LOOP('',(#22055,#22056,#22057,#22058));
#6079=EDGE_LOOP('',(#22059,#22060,#22061,#22062));
#6080=EDGE_LOOP('',(#22063,#22064,#22065,#22066,#22067,#22068));
#6081=EDGE_LOOP('',(#22069,#22070,#22071,#22072,#22073));
#6082=EDGE_LOOP('',(#22074));
#6083=EDGE_LOOP('',(#22075,#22076,#22077,#22078,#22079,#22080,#22081,#22082,
#22083));
#6084=EDGE_LOOP('',(#22084,#22085));
#6085=EDGE_LOOP('',(#22086));
#6086=EDGE_LOOP('',(#22087,#22088,#22089,#22090));
#6087=EDGE_LOOP('',(#22091,#22092,#22093,#22094,#22095,#22096,#22097,#22098,
#22099,#22100));
#6088=EDGE_LOOP('',(#22101,#22102,#22103,#22104,#22105,#22106,#22107,#22108));
#6089=EDGE_LOOP('',(#22109,#22110,#22111));
#6090=EDGE_LOOP('',(#22112,#22113,#22114,#22115));
#6091=EDGE_LOOP('',(#22116,#22117));
#6092=EDGE_LOOP('',(#22118,#22119));
#6093=EDGE_LOOP('',(#22120,#22121,#22122,#22123,#22124,#22125,#22126,#22127));
#6094=EDGE_LOOP('',(#22128,#22129));
#6095=EDGE_LOOP('',(#22130,#22131,#22132,#22133));
#6096=EDGE_LOOP('',(#22134,#22135));
#6097=EDGE_LOOP('',(#22136,#22137));
#6098=EDGE_LOOP('',(#22138,#22139,#22140,#22141,#22142,#22143,#22144,#22145,
#22146));
#6099=EDGE_LOOP('',(#22147,#22148,#22149,#22150));
#6100=EDGE_LOOP('',(#22151,#22152,#22153,#22154));
#6101=EDGE_LOOP('',(#22155,#22156,#22157,#22158));
#6102=EDGE_LOOP('',(#22159,#22160,#22161,#22162));
#6103=EDGE_LOOP('',(#22163,#22164,#22165,#22166));
#6104=EDGE_LOOP('',(#22167,#22168,#22169,#22170));
#6105=EDGE_LOOP('',(#22171,#22172,#22173,#22174));
#6106=EDGE_LOOP('',(#22175,#22176,#22177,#22178));
#6107=EDGE_LOOP('',(#22179,#22180,#22181,#22182));
#6108=EDGE_LOOP('',(#22183,#22184,#22185,#22186));
#6109=EDGE_LOOP('',(#22187,#22188,#22189,#22190));
#6110=EDGE_LOOP('',(#22191,#22192,#22193,#22194));
#6111=EDGE_LOOP('',(#22195,#22196,#22197,#22198));
#6112=EDGE_LOOP('',(#22199,#22200,#22201,#22202));
#6113=EDGE_LOOP('',(#22203,#22204,#22205,#22206));
#6114=EDGE_LOOP('',(#22207,#22208,#22209,#22210));
#6115=EDGE_LOOP('',(#22211,#22212,#22213,#22214));
#6116=EDGE_LOOP('',(#22215,#22216,#22217,#22218));
#6117=EDGE_LOOP('',(#22219,#22220,#22221,#22222));
#6118=EDGE_LOOP('',(#22223,#22224,#22225,#22226));
#6119=EDGE_LOOP('',(#22227,#22228,#22229,#22230,#22231));
#6120=EDGE_LOOP('',(#22232,#22233,#22234,#22235,#22236,#22237,#22238,#22239,
#22240,#22241,#22242,#22243,#22244,#22245,#22246,#22247,#22248,#22249,#22250,
#22251,#22252,#22253,#22254,#22255));
#6121=EDGE_LOOP('',(#22256,#22257,#22258,#22259,#22260));
#6122=EDGE_LOOP('',(#22261,#22262,#22263,#22264));
#6123=EDGE_LOOP('',(#22265,#22266,#22267,#22268,#22269,#22270,#22271,#22272,
#22273,#22274,#22275,#22276,#22277,#22278,#22279,#22280,#22281,#22282,#22283,
#22284,#22285,#22286,#22287,#22288));
#6124=EDGE_LOOP('',(#22289,#22290,#22291,#22292));
#6125=EDGE_LOOP('',(#22293,#22294,#22295));
#6126=EDGE_LOOP('',(#22296,#22297,#22298,#22299));
#6127=EDGE_LOOP('',(#22300,#22301,#22302));
#6128=EDGE_LOOP('',(#22303,#22304,#22305,#22306));
#6129=EDGE_LOOP('',(#22307,#22308,#22309));
#6130=EDGE_LOOP('',(#22310,#22311,#22312,#22313));
#6131=EDGE_LOOP('',(#22314,#22315,#22316));
#6132=EDGE_LOOP('',(#22317,#22318,#22319,#22320));
#6133=EDGE_LOOP('',(#22321,#22322,#22323));
#6134=EDGE_LOOP('',(#22324,#22325,#22326,#22327));
#6135=EDGE_LOOP('',(#22328,#22329,#22330));
#6136=EDGE_LOOP('',(#22331,#22332,#22333,#22334));
#6137=EDGE_LOOP('',(#22335,#22336,#22337));
#6138=EDGE_LOOP('',(#22338,#22339,#22340,#22341));
#6139=EDGE_LOOP('',(#22342,#22343,#22344));
#6140=EDGE_LOOP('',(#22345,#22346,#22347,#22348));
#6141=EDGE_LOOP('',(#22349,#22350,#22351));
#6142=EDGE_LOOP('',(#22352,#22353,#22354,#22355));
#6143=EDGE_LOOP('',(#22356,#22357,#22358));
#6144=EDGE_LOOP('',(#22359,#22360,#22361,#22362));
#6145=EDGE_LOOP('',(#22363,#22364,#22365));
#6146=EDGE_LOOP('',(#22366,#22367,#22368,#22369));
#6147=EDGE_LOOP('',(#22370,#22371,#22372));
#6148=EDGE_LOOP('',(#22373,#22374,#22375,#22376));
#6149=EDGE_LOOP('',(#22377,#22378,#22379));
#6150=EDGE_LOOP('',(#22380,#22381,#22382,#22383));
#6151=EDGE_LOOP('',(#22384,#22385,#22386));
#6152=EDGE_LOOP('',(#22387,#22388,#22389,#22390));
#6153=EDGE_LOOP('',(#22391,#22392,#22393));
#6154=EDGE_LOOP('',(#22394,#22395,#22396,#22397));
#6155=EDGE_LOOP('',(#22398,#22399,#22400));
#6156=EDGE_LOOP('',(#22401,#22402,#22403,#22404));
#6157=EDGE_LOOP('',(#22405,#22406,#22407));
#6158=EDGE_LOOP('',(#22408,#22409,#22410,#22411));
#6159=EDGE_LOOP('',(#22412,#22413,#22414));
#6160=EDGE_LOOP('',(#22415,#22416,#22417,#22418));
#6161=EDGE_LOOP('',(#22419,#22420,#22421));
#6162=EDGE_LOOP('',(#22422,#22423,#22424,#22425));
#6163=EDGE_LOOP('',(#22426,#22427,#22428));
#6164=EDGE_LOOP('',(#22429,#22430,#22431,#22432));
#6165=EDGE_LOOP('',(#22433,#22434,#22435));
#6166=EDGE_LOOP('',(#22436,#22437,#22438,#22439));
#6167=EDGE_LOOP('',(#22440,#22441,#22442));
#6168=EDGE_LOOP('',(#22443,#22444,#22445,#22446));
#6169=EDGE_LOOP('',(#22447,#22448,#22449));
#6170=EDGE_LOOP('',(#22450,#22451,#22452,#22453));
#6171=EDGE_LOOP('',(#22454,#22455,#22456));
#6172=EDGE_LOOP('',(#22457,#22458,#22459,#22460));
#6173=EDGE_LOOP('',(#22461,#22462,#22463));
#6174=EDGE_LOOP('',(#22464,#22465,#22466,#22467));
#6175=EDGE_LOOP('',(#22468,#22469,#22470));
#6176=EDGE_LOOP('',(#22471,#22472,#22473,#22474));
#6177=EDGE_LOOP('',(#22475,#22476,#22477));
#6178=EDGE_LOOP('',(#22478,#22479,#22480,#22481));
#6179=EDGE_LOOP('',(#22482,#22483,#22484));
#6180=EDGE_LOOP('',(#22485,#22486,#22487,#22488));
#6181=EDGE_LOOP('',(#22489,#22490,#22491));
#6182=EDGE_LOOP('',(#22492,#22493,#22494,#22495));
#6183=EDGE_LOOP('',(#22496,#22497,#22498));
#6184=EDGE_LOOP('',(#22499,#22500,#22501,#22502));
#6185=EDGE_LOOP('',(#22503,#22504,#22505));
#6186=EDGE_LOOP('',(#22506,#22507,#22508,#22509));
#6187=EDGE_LOOP('',(#22510,#22511,#22512));
#6188=EDGE_LOOP('',(#22513,#22514,#22515,#22516));
#6189=EDGE_LOOP('',(#22517,#22518,#22519));
#6190=EDGE_LOOP('',(#22520,#22521,#22522,#22523));
#6191=EDGE_LOOP('',(#22524,#22525,#22526));
#6192=EDGE_LOOP('',(#22527,#22528,#22529,#22530));
#6193=EDGE_LOOP('',(#22531,#22532,#22533,#22534));
#6194=EDGE_LOOP('',(#22535,#22536,#22537,#22538));
#6195=EDGE_LOOP('',(#22539,#22540,#22541,#22542));
#6196=EDGE_LOOP('',(#22543,#22544,#22545,#22546));
#6197=EDGE_LOOP('',(#22547,#22548,#22549));
#6198=EDGE_LOOP('',(#22550,#22551,#22552,#22553));
#6199=EDGE_LOOP('',(#22554,#22555,#22556));
#6200=EDGE_LOOP('',(#22557,#22558,#22559,#22560));
#6201=EDGE_LOOP('',(#22561,#22562,#22563));
#6202=EDGE_LOOP('',(#22564,#22565,#22566,#22567));
#6203=EDGE_LOOP('',(#22568,#22569,#22570));
#6204=EDGE_LOOP('',(#22571,#22572,#22573,#22574));
#6205=EDGE_LOOP('',(#22575,#22576,#22577));
#6206=EDGE_LOOP('',(#22578,#22579,#22580,#22581));
#6207=EDGE_LOOP('',(#22582,#22583,#22584));
#6208=EDGE_LOOP('',(#22585,#22586,#22587,#22588));
#6209=EDGE_LOOP('',(#22589,#22590,#22591));
#6210=EDGE_LOOP('',(#22592,#22593,#22594,#22595));
#6211=EDGE_LOOP('',(#22596,#22597,#22598));
#6212=EDGE_LOOP('',(#22599,#22600,#22601,#22602));
#6213=EDGE_LOOP('',(#22603,#22604,#22605));
#6214=EDGE_LOOP('',(#22606,#22607,#22608,#22609));
#6215=EDGE_LOOP('',(#22610,#22611,#22612));
#6216=EDGE_LOOP('',(#22613,#22614,#22615,#22616));
#6217=EDGE_LOOP('',(#22617,#22618,#22619));
#6218=EDGE_LOOP('',(#22620,#22621,#22622,#22623));
#6219=EDGE_LOOP('',(#22624,#22625,#22626));
#6220=EDGE_LOOP('',(#22627,#22628,#22629,#22630));
#6221=EDGE_LOOP('',(#22631,#22632,#22633));
#6222=EDGE_LOOP('',(#22634,#22635,#22636,#22637));
#6223=EDGE_LOOP('',(#22638,#22639,#22640));
#6224=EDGE_LOOP('',(#22641,#22642,#22643,#22644));
#6225=EDGE_LOOP('',(#22645,#22646,#22647));
#6226=EDGE_LOOP('',(#22648,#22649,#22650,#22651));
#6227=EDGE_LOOP('',(#22652,#22653,#22654));
#6228=EDGE_LOOP('',(#22655,#22656,#22657,#22658));
#6229=EDGE_LOOP('',(#22659,#22660,#22661));
#6230=EDGE_LOOP('',(#22662,#22663,#22664,#22665));
#6231=EDGE_LOOP('',(#22666,#22667,#22668));
#6232=EDGE_LOOP('',(#22669,#22670,#22671,#22672));
#6233=EDGE_LOOP('',(#22673,#22674,#22675));
#6234=EDGE_LOOP('',(#22676,#22677,#22678,#22679));
#6235=EDGE_LOOP('',(#22680,#22681,#22682));
#6236=EDGE_LOOP('',(#22683,#22684,#22685,#22686));
#6237=EDGE_LOOP('',(#22687,#22688,#22689));
#6238=EDGE_LOOP('',(#22690,#22691,#22692,#22693));
#6239=EDGE_LOOP('',(#22694,#22695,#22696));
#6240=EDGE_LOOP('',(#22697,#22698,#22699,#22700));
#6241=EDGE_LOOP('',(#22701,#22702,#22703));
#6242=EDGE_LOOP('',(#22704,#22705,#22706,#22707));
#6243=EDGE_LOOP('',(#22708,#22709,#22710));
#6244=EDGE_LOOP('',(#22711,#22712,#22713,#22714));
#6245=EDGE_LOOP('',(#22715,#22716,#22717));
#6246=EDGE_LOOP('',(#22718,#22719,#22720,#22721));
#6247=EDGE_LOOP('',(#22722,#22723,#22724));
#6248=EDGE_LOOP('',(#22725,#22726,#22727,#22728));
#6249=EDGE_LOOP('',(#22729,#22730,#22731));
#6250=EDGE_LOOP('',(#22732,#22733,#22734,#22735));
#6251=EDGE_LOOP('',(#22736,#22737,#22738));
#6252=EDGE_LOOP('',(#22739,#22740,#22741,#22742));
#6253=EDGE_LOOP('',(#22743,#22744,#22745));
#6254=EDGE_LOOP('',(#22746,#22747,#22748,#22749));
#6255=EDGE_LOOP('',(#22750,#22751,#22752));
#6256=EDGE_LOOP('',(#22753,#22754,#22755,#22756));
#6257=EDGE_LOOP('',(#22757,#22758,#22759));
#6258=EDGE_LOOP('',(#22760,#22761,#22762,#22763));
#6259=EDGE_LOOP('',(#22764,#22765,#22766));
#6260=EDGE_LOOP('',(#22767,#22768,#22769,#22770));
#6261=EDGE_LOOP('',(#22771,#22772,#22773));
#6262=EDGE_LOOP('',(#22774,#22775,#22776,#22777));
#6263=EDGE_LOOP('',(#22778,#22779,#22780));
#6264=EDGE_LOOP('',(#22781,#22782,#22783,#22784));
#6265=EDGE_LOOP('',(#22785,#22786,#22787));
#6266=EDGE_LOOP('',(#22788,#22789,#22790,#22791));
#6267=EDGE_LOOP('',(#22792,#22793,#22794));
#6268=EDGE_LOOP('',(#22795,#22796,#22797));
#6269=EDGE_LOOP('',(#22798,#22799,#22800,#22801));
#6270=EDGE_LOOP('',(#22802,#22803,#22804,#22805));
#6271=EDGE_LOOP('',(#22806,#22807,#22808,#22809));
#6272=EDGE_LOOP('',(#22810,#22811,#22812,#22813));
#6273=EDGE_LOOP('',(#22814,#22815,#22816,#22817));
#6274=EDGE_LOOP('',(#22818,#22819,#22820,#22821));
#6275=EDGE_LOOP('',(#22822,#22823,#22824,#22825,#22826,#22827));
#6276=EDGE_LOOP('',(#22828));
#6277=EDGE_LOOP('',(#22829,#22830,#22831,#22832,#22833));
#6278=EDGE_LOOP('',(#22834,#22835,#22836,#22837,#22838));
#6279=EDGE_LOOP('',(#22839));
#6280=EDGE_LOOP('',(#22840));
#6281=EDGE_LOOP('',(#22841));
#6282=EDGE_LOOP('',(#22842,#22843,#22844,#22845,#22846,#22847));
#6283=EDGE_LOOP('',(#22848,#22849,#22850,#22851));
#6284=EDGE_LOOP('',(#22852,#22853,#22854,#22855,#22856,#22857));
#6285=EDGE_LOOP('',(#22858,#22859,#22860,#22861));
#6286=EDGE_LOOP('',(#22862));
#6287=EDGE_LOOP('',(#22863));
#6288=EDGE_LOOP('',(#22864,#22865,#22866,#22867,#22868,#22869,#22870,#22871,
#22872,#22873,#22874,#22875));
#6289=EDGE_LOOP('',(#22876,#22877,#22878,#22879));
#6290=EDGE_LOOP('',(#22880,#22881,#22882,#22883));
#6291=EDGE_LOOP('',(#22884,#22885,#22886,#22887));
#6292=EDGE_LOOP('',(#22888,#22889,#22890,#22891));
#6293=EDGE_LOOP('',(#22892,#22893,#22894,#22895));
#6294=EDGE_LOOP('',(#22896,#22897,#22898,#22899));
#6295=EDGE_LOOP('',(#22900,#22901,#22902,#22903));
#6296=EDGE_LOOP('',(#22904,#22905,#22906,#22907));
#6297=EDGE_LOOP('',(#22908,#22909,#22910,#22911));
#6298=EDGE_LOOP('',(#22912,#22913,#22914,#22915));
#6299=EDGE_LOOP('',(#22916,#22917,#22918,#22919));
#6300=EDGE_LOOP('',(#22920,#22921,#22922,#22923));
#6301=EDGE_LOOP('',(#22924,#22925,#22926,#22927));
#6302=EDGE_LOOP('',(#22928,#22929,#22930,#22931));
#6303=EDGE_LOOP('',(#22932,#22933,#22934,#22935));
#6304=EDGE_LOOP('',(#22936,#22937,#22938,#22939));
#6305=EDGE_LOOP('',(#22940,#22941,#22942,#22943));
#6306=EDGE_LOOP('',(#22944,#22945,#22946,#22947));
#6307=EDGE_LOOP('',(#22948,#22949,#22950,#22951));
#6308=EDGE_LOOP('',(#22952,#22953,#22954,#22955));
#6309=EDGE_LOOP('',(#22956,#22957,#22958,#22959));
#6310=EDGE_LOOP('',(#22960,#22961,#22962,#22963));
#6311=EDGE_LOOP('',(#22964,#22965,#22966,#22967));
#6312=EDGE_LOOP('',(#22968,#22969,#22970,#22971));
#6313=EDGE_LOOP('',(#22972,#22973,#22974,#22975));
#6314=EDGE_LOOP('',(#22976,#22977,#22978,#22979));
#6315=EDGE_LOOP('',(#22980,#22981,#22982,#22983));
#6316=EDGE_LOOP('',(#22984,#22985,#22986,#22987));
#6317=EDGE_LOOP('',(#22988,#22989,#22990,#22991));
#6318=EDGE_LOOP('',(#22992,#22993,#22994,#22995));
#6319=EDGE_LOOP('',(#22996,#22997,#22998,#22999));
#6320=EDGE_LOOP('',(#23000,#23001,#23002,#23003));
#6321=EDGE_LOOP('',(#23004,#23005,#23006,#23007));
#6322=EDGE_LOOP('',(#23008,#23009,#23010,#23011));
#6323=EDGE_LOOP('',(#23012,#23013,#23014,#23015));
#6324=EDGE_LOOP('',(#23016,#23017,#23018,#23019));
#6325=EDGE_LOOP('',(#23020));
#6326=EDGE_LOOP('',(#23021,#23022,#23023,#23024,#23025,#23026));
#6327=EDGE_LOOP('',(#23027,#23028,#23029,#23030));
#6328=EDGE_LOOP('',(#23031));
#6329=EDGE_LOOP('',(#23032));
#6330=EDGE_LOOP('',(#23033,#23034,#23035,#23036));
#6331=EDGE_LOOP('',(#23037));
#6332=EDGE_LOOP('',(#23038));
#6333=EDGE_LOOP('',(#23039,#23040));
#6334=EDGE_LOOP('',(#23041));
#6335=EDGE_LOOP('',(#23042,#23043,#23044,#23045));
#6336=EDGE_LOOP('',(#23046,#23047,#23048,#23049));
#6337=EDGE_LOOP('',(#23050,#23051,#23052,#23053));
#6338=EDGE_LOOP('',(#23054));
#6339=EDGE_LOOP('',(#23055,#23056,#23057,#23058));
#6340=EDGE_LOOP('',(#23059));
#6341=EDGE_LOOP('',(#23060));
#6342=EDGE_LOOP('',(#23061,#23062,#23063,#23064,#23065));
#6343=EDGE_LOOP('',(#23066,#23067,#23068,#23069,#23070));
#6344=EDGE_LOOP('',(#23071));
#6345=EDGE_LOOP('',(#23072));
#6346=EDGE_LOOP('',(#23073,#23074,#23075,#23076));
#6347=EDGE_LOOP('',(#23077));
#6348=EDGE_LOOP('',(#23078));
#6349=EDGE_LOOP('',(#23079,#23080,#23081,#23082));
#6350=EDGE_LOOP('',(#23083,#23084,#23085,#23086));
#6351=EDGE_LOOP('',(#23087,#23088,#23089,#23090));
#6352=EDGE_LOOP('',(#23091,#23092,#23093,#23094));
#6353=EDGE_LOOP('',(#23095,#23096,#23097,#23098));
#6354=EDGE_LOOP('',(#23099,#23100,#23101,#23102));
#6355=EDGE_LOOP('',(#23103,#23104,#23105,#23106));
#6356=EDGE_LOOP('',(#23107,#23108,#23109,#23110));
#6357=EDGE_LOOP('',(#23111,#23112,#23113,#23114));
#6358=EDGE_LOOP('',(#23115,#23116,#23117,#23118));
#6359=EDGE_LOOP('',(#23119,#23120,#23121,#23122));
#6360=EDGE_LOOP('',(#23123,#23124,#23125,#23126));
#6361=EDGE_LOOP('',(#23127,#23128,#23129,#23130));
#6362=EDGE_LOOP('',(#23131,#23132,#23133,#23134));
#6363=EDGE_LOOP('',(#23135,#23136,#23137,#23138));
#6364=EDGE_LOOP('',(#23139,#23140,#23141,#23142));
#6365=EDGE_LOOP('',(#23143,#23144,#23145,#23146));
#6366=EDGE_LOOP('',(#23147,#23148,#23149,#23150));
#6367=EDGE_LOOP('',(#23151,#23152,#23153,#23154));
#6368=EDGE_LOOP('',(#23155,#23156,#23157,#23158));
#6369=EDGE_LOOP('',(#23159,#23160,#23161,#23162));
#6370=EDGE_LOOP('',(#23163,#23164,#23165,#23166));
#6371=EDGE_LOOP('',(#23167,#23168,#23169,#23170));
#6372=EDGE_LOOP('',(#23171,#23172,#23173,#23174));
#6373=EDGE_LOOP('',(#23175,#23176,#23177,#23178));
#6374=EDGE_LOOP('',(#23179,#23180,#23181,#23182));
#6375=EDGE_LOOP('',(#23183,#23184,#23185,#23186));
#6376=EDGE_LOOP('',(#23187,#23188,#23189,#23190));
#6377=EDGE_LOOP('',(#23191,#23192,#23193,#23194));
#6378=EDGE_LOOP('',(#23195,#23196,#23197,#23198));
#6379=EDGE_LOOP('',(#23199,#23200,#23201,#23202));
#6380=EDGE_LOOP('',(#23203,#23204,#23205,#23206));
#6381=EDGE_LOOP('',(#23207,#23208,#23209,#23210));
#6382=EDGE_LOOP('',(#23211,#23212,#23213,#23214));
#6383=EDGE_LOOP('',(#23215,#23216,#23217,#23218));
#6384=EDGE_LOOP('',(#23219,#23220,#23221,#23222));
#6385=EDGE_LOOP('',(#23223,#23224,#23225,#23226));
#6386=EDGE_LOOP('',(#23227,#23228,#23229,#23230));
#6387=EDGE_LOOP('',(#23231,#23232,#23233,#23234));
#6388=EDGE_LOOP('',(#23235,#23236,#23237,#23238));
#6389=EDGE_LOOP('',(#23239,#23240,#23241,#23242));
#6390=EDGE_LOOP('',(#23243,#23244,#23245,#23246));
#6391=EDGE_LOOP('',(#23247,#23248,#23249,#23250));
#6392=EDGE_LOOP('',(#23251,#23252,#23253,#23254));
#6393=EDGE_LOOP('',(#23255,#23256,#23257,#23258));
#6394=EDGE_LOOP('',(#23259,#23260,#23261,#23262));
#6395=EDGE_LOOP('',(#23263,#23264,#23265,#23266));
#6396=EDGE_LOOP('',(#23267,#23268,#23269,#23270));
#6397=EDGE_LOOP('',(#23271,#23272,#23273,#23274));
#6398=EDGE_LOOP('',(#23275,#23276,#23277,#23278));
#6399=EDGE_LOOP('',(#23279,#23280,#23281,#23282));
#6400=EDGE_LOOP('',(#23283,#23284,#23285,#23286));
#6401=EDGE_LOOP('',(#23287,#23288,#23289,#23290));
#6402=EDGE_LOOP('',(#23291,#23292,#23293,#23294));
#6403=EDGE_LOOP('',(#23295,#23296,#23297,#23298));
#6404=EDGE_LOOP('',(#23299,#23300,#23301,#23302));
#6405=EDGE_LOOP('',(#23303,#23304,#23305,#23306));
#6406=EDGE_LOOP('',(#23307,#23308,#23309,#23310));
#6407=EDGE_LOOP('',(#23311,#23312,#23313,#23314));
#6408=EDGE_LOOP('',(#23315,#23316,#23317,#23318));
#6409=EDGE_LOOP('',(#23319,#23320,#23321,#23322));
#6410=EDGE_LOOP('',(#23323,#23324,#23325,#23326));
#6411=EDGE_LOOP('',(#23327,#23328,#23329,#23330));
#6412=EDGE_LOOP('',(#23331,#23332,#23333,#23334));
#6413=EDGE_LOOP('',(#23335,#23336,#23337,#23338));
#6414=EDGE_LOOP('',(#23339,#23340,#23341,#23342));
#6415=EDGE_LOOP('',(#23343,#23344,#23345,#23346));
#6416=EDGE_LOOP('',(#23347,#23348,#23349,#23350));
#6417=EDGE_LOOP('',(#23351,#23352,#23353,#23354));
#6418=EDGE_LOOP('',(#23355,#23356,#23357,#23358));
#6419=EDGE_LOOP('',(#23359,#23360,#23361,#23362));
#6420=EDGE_LOOP('',(#23363,#23364,#23365,#23366));
#6421=EDGE_LOOP('',(#23367,#23368,#23369,#23370));
#6422=EDGE_LOOP('',(#23371,#23372,#23373,#23374));
#6423=EDGE_LOOP('',(#23375,#23376,#23377,#23378));
#6424=EDGE_LOOP('',(#23379,#23380,#23381,#23382));
#6425=EDGE_LOOP('',(#23383,#23384,#23385,#23386));
#6426=EDGE_LOOP('',(#23387,#23388,#23389,#23390));
#6427=EDGE_LOOP('',(#23391,#23392,#23393,#23394));
#6428=EDGE_LOOP('',(#23395,#23396,#23397,#23398));
#6429=EDGE_LOOP('',(#23399,#23400,#23401,#23402));
#6430=EDGE_LOOP('',(#23403,#23404,#23405,#23406));
#6431=EDGE_LOOP('',(#23407,#23408,#23409,#23410));
#6432=EDGE_LOOP('',(#23411,#23412,#23413,#23414));
#6433=EDGE_LOOP('',(#23415,#23416,#23417,#23418));
#6434=EDGE_LOOP('',(#23419,#23420,#23421,#23422));
#6435=EDGE_LOOP('',(#23423,#23424,#23425,#23426,#23427,#23428,#23429,#23430,
#23431,#23432,#23433,#23434,#23435,#23436,#23437,#23438,#23439,#23440,#23441,
#23442,#23443,#23444,#23445,#23446,#23447,#23448,#23449,#23450,#23451,#23452,
#23453,#23454,#23455,#23456,#23457,#23458,#23459,#23460,#23461,#23462,#23463,
#23464,#23465,#23466,#23467,#23468,#23469,#23470,#23471,#23472,#23473,#23474,
#23475,#23476,#23477,#23478,#23479,#23480,#23481,#23482,#23483,#23484,#23485,
#23486,#23487,#23488,#23489,#23490,#23491,#23492,#23493,#23494,#23495,#23496,
#23497,#23498,#23499,#23500,#23501,#23502,#23503,#23504,#23505,#23506,#23507,
#23508,#23509,#23510));
#6436=EDGE_LOOP('',(#23511,#23512,#23513,#23514,#23515));
#6437=EDGE_LOOP('',(#23516,#23517,#23518,#23519));
#6438=EDGE_LOOP('',(#23520,#23521,#23522,#23523,#23524,#23525,#23526,#23527,
#23528,#23529,#23530,#23531,#23532,#23533,#23534,#23535,#23536,#23537,#23538,
#23539,#23540,#23541,#23542,#23543,#23544,#23545,#23546,#23547,#23548,#23549,
#23550,#23551,#23552,#23553,#23554,#23555,#23556,#23557,#23558,#23559,#23560,
#23561,#23562,#23563,#23564,#23565,#23566,#23567,#23568,#23569,#23570,#23571,
#23572,#23573,#23574,#23575,#23576,#23577,#23578,#23579,#23580,#23581,#23582,
#23583,#23584,#23585,#23586,#23587,#23588,#23589,#23590,#23591,#23592,#23593,
#23594,#23595,#23596,#23597,#23598,#23599,#23600,#23601,#23602,#23603,#23604,
#23605,#23606,#23607));
#6439=EDGE_LOOP('',(#23608,#23609,#23610,#23611,#23612,#23613));
#6440=EDGE_LOOP('',(#23614,#23615,#23616,#23617,#23618));
#6441=EDGE_LOOP('',(#23619));
#6442=EDGE_LOOP('',(#23620));
#6443=EDGE_LOOP('',(#23621,#23622,#23623,#23624));
#6444=EDGE_LOOP('',(#23625,#23626,#23627));
#6445=EDGE_LOOP('',(#23628,#23629,#23630,#23631));
#6446=EDGE_LOOP('',(#23632,#23633,#23634));
#6447=EDGE_LOOP('',(#23635,#23636,#23637,#23638));
#6448=EDGE_LOOP('',(#23639,#23640,#23641));
#6449=EDGE_LOOP('',(#23642,#23643,#23644,#23645));
#6450=EDGE_LOOP('',(#23646,#23647,#23648));
#6451=EDGE_LOOP('',(#23649,#23650,#23651,#23652));
#6452=EDGE_LOOP('',(#23653,#23654,#23655));
#6453=EDGE_LOOP('',(#23656,#23657,#23658,#23659));
#6454=EDGE_LOOP('',(#23660,#23661,#23662));
#6455=EDGE_LOOP('',(#23663,#23664,#23665,#23666));
#6456=EDGE_LOOP('',(#23667,#23668,#23669));
#6457=EDGE_LOOP('',(#23670,#23671,#23672,#23673));
#6458=EDGE_LOOP('',(#23674,#23675,#23676));
#6459=EDGE_LOOP('',(#23677,#23678,#23679,#23680));
#6460=EDGE_LOOP('',(#23681,#23682,#23683));
#6461=EDGE_LOOP('',(#23684,#23685,#23686,#23687));
#6462=EDGE_LOOP('',(#23688,#23689,#23690));
#6463=EDGE_LOOP('',(#23691,#23692,#23693,#23694));
#6464=EDGE_LOOP('',(#23695,#23696,#23697));
#6465=EDGE_LOOP('',(#23698,#23699,#23700,#23701));
#6466=EDGE_LOOP('',(#23702,#23703,#23704));
#6467=EDGE_LOOP('',(#23705,#23706,#23707,#23708));
#6468=EDGE_LOOP('',(#23709,#23710,#23711));
#6469=EDGE_LOOP('',(#23712,#23713,#23714,#23715));
#6470=EDGE_LOOP('',(#23716,#23717,#23718));
#6471=EDGE_LOOP('',(#23719,#23720,#23721,#23722));
#6472=EDGE_LOOP('',(#23723,#23724,#23725));
#6473=EDGE_LOOP('',(#23726,#23727,#23728,#23729));
#6474=EDGE_LOOP('',(#23730,#23731,#23732));
#6475=EDGE_LOOP('',(#23733,#23734,#23735,#23736));
#6476=EDGE_LOOP('',(#23737,#23738,#23739));
#6477=EDGE_LOOP('',(#23740,#23741,#23742,#23743));
#6478=EDGE_LOOP('',(#23744,#23745,#23746));
#6479=EDGE_LOOP('',(#23747,#23748,#23749,#23750));
#6480=EDGE_LOOP('',(#23751,#23752,#23753));
#6481=EDGE_LOOP('',(#23754,#23755,#23756,#23757));
#6482=EDGE_LOOP('',(#23758,#23759,#23760));
#6483=EDGE_LOOP('',(#23761,#23762,#23763,#23764));
#6484=EDGE_LOOP('',(#23765,#23766,#23767));
#6485=EDGE_LOOP('',(#23768,#23769,#23770,#23771));
#6486=EDGE_LOOP('',(#23772,#23773,#23774));
#6487=EDGE_LOOP('',(#23775,#23776,#23777,#23778));
#6488=EDGE_LOOP('',(#23779,#23780,#23781));
#6489=EDGE_LOOP('',(#23782,#23783,#23784,#23785));
#6490=EDGE_LOOP('',(#23786,#23787,#23788));
#6491=EDGE_LOOP('',(#23789,#23790,#23791,#23792));
#6492=EDGE_LOOP('',(#23793,#23794,#23795));
#6493=EDGE_LOOP('',(#23796,#23797,#23798,#23799));
#6494=EDGE_LOOP('',(#23800,#23801,#23802));
#6495=EDGE_LOOP('',(#23803,#23804,#23805,#23806));
#6496=EDGE_LOOP('',(#23807,#23808,#23809));
#6497=EDGE_LOOP('',(#23810,#23811,#23812,#23813));
#6498=EDGE_LOOP('',(#23814,#23815,#23816));
#6499=EDGE_LOOP('',(#23817,#23818,#23819,#23820));
#6500=EDGE_LOOP('',(#23821,#23822,#23823));
#6501=EDGE_LOOP('',(#23824,#23825,#23826,#23827));
#6502=EDGE_LOOP('',(#23828,#23829,#23830));
#6503=EDGE_LOOP('',(#23831,#23832,#23833,#23834));
#6504=EDGE_LOOP('',(#23835,#23836,#23837));
#6505=EDGE_LOOP('',(#23838,#23839,#23840,#23841));
#6506=EDGE_LOOP('',(#23842,#23843,#23844));
#6507=EDGE_LOOP('',(#23845,#23846,#23847,#23848));
#6508=EDGE_LOOP('',(#23849,#23850,#23851));
#6509=EDGE_LOOP('',(#23852,#23853,#23854,#23855));
#6510=EDGE_LOOP('',(#23856,#23857,#23858));
#6511=EDGE_LOOP('',(#23859,#23860,#23861,#23862));
#6512=EDGE_LOOP('',(#23863,#23864,#23865,#23866));
#6513=EDGE_LOOP('',(#23867,#23868,#23869,#23870));
#6514=EDGE_LOOP('',(#23871,#23872,#23873,#23874));
#6515=EDGE_LOOP('',(#23875,#23876,#23877,#23878));
#6516=EDGE_LOOP('',(#23879,#23880,#23881));
#6517=EDGE_LOOP('',(#23882,#23883,#23884,#23885));
#6518=EDGE_LOOP('',(#23886,#23887,#23888));
#6519=EDGE_LOOP('',(#23889,#23890,#23891,#23892));
#6520=EDGE_LOOP('',(#23893,#23894,#23895));
#6521=EDGE_LOOP('',(#23896,#23897,#23898,#23899));
#6522=EDGE_LOOP('',(#23900,#23901,#23902));
#6523=EDGE_LOOP('',(#23903,#23904,#23905,#23906));
#6524=EDGE_LOOP('',(#23907,#23908,#23909));
#6525=EDGE_LOOP('',(#23910,#23911,#23912,#23913));
#6526=EDGE_LOOP('',(#23914,#23915,#23916));
#6527=EDGE_LOOP('',(#23917,#23918,#23919,#23920));
#6528=EDGE_LOOP('',(#23921,#23922,#23923));
#6529=EDGE_LOOP('',(#23924,#23925,#23926,#23927));
#6530=EDGE_LOOP('',(#23928,#23929,#23930));
#6531=EDGE_LOOP('',(#23931,#23932,#23933,#23934));
#6532=EDGE_LOOP('',(#23935,#23936,#23937));
#6533=EDGE_LOOP('',(#23938,#23939,#23940,#23941));
#6534=EDGE_LOOP('',(#23942,#23943,#23944));
#6535=EDGE_LOOP('',(#23945,#23946,#23947,#23948));
#6536=EDGE_LOOP('',(#23949,#23950,#23951));
#6537=EDGE_LOOP('',(#23952,#23953,#23954,#23955));
#6538=EDGE_LOOP('',(#23956,#23957,#23958));
#6539=EDGE_LOOP('',(#23959,#23960,#23961,#23962));
#6540=EDGE_LOOP('',(#23963,#23964,#23965));
#6541=EDGE_LOOP('',(#23966,#23967,#23968,#23969));
#6542=EDGE_LOOP('',(#23970,#23971,#23972));
#6543=EDGE_LOOP('',(#23973,#23974,#23975,#23976));
#6544=EDGE_LOOP('',(#23977,#23978,#23979));
#6545=EDGE_LOOP('',(#23980,#23981,#23982,#23983));
#6546=EDGE_LOOP('',(#23984,#23985,#23986));
#6547=EDGE_LOOP('',(#23987,#23988,#23989,#23990));
#6548=EDGE_LOOP('',(#23991,#23992,#23993));
#6549=EDGE_LOOP('',(#23994,#23995,#23996,#23997));
#6550=EDGE_LOOP('',(#23998,#23999,#24000));
#6551=EDGE_LOOP('',(#24001,#24002,#24003,#24004));
#6552=EDGE_LOOP('',(#24005,#24006,#24007));
#6553=EDGE_LOOP('',(#24008,#24009,#24010,#24011));
#6554=EDGE_LOOP('',(#24012,#24013,#24014));
#6555=EDGE_LOOP('',(#24015,#24016,#24017,#24018));
#6556=EDGE_LOOP('',(#24019,#24020,#24021));
#6557=EDGE_LOOP('',(#24022,#24023,#24024,#24025));
#6558=EDGE_LOOP('',(#24026,#24027,#24028));
#6559=EDGE_LOOP('',(#24029,#24030,#24031,#24032));
#6560=EDGE_LOOP('',(#24033,#24034,#24035));
#6561=EDGE_LOOP('',(#24036,#24037,#24038,#24039));
#6562=EDGE_LOOP('',(#24040,#24041,#24042));
#6563=EDGE_LOOP('',(#24043,#24044,#24045,#24046));
#6564=EDGE_LOOP('',(#24047,#24048,#24049));
#6565=EDGE_LOOP('',(#24050,#24051,#24052,#24053));
#6566=EDGE_LOOP('',(#24054,#24055,#24056));
#6567=EDGE_LOOP('',(#24057,#24058,#24059,#24060));
#6568=EDGE_LOOP('',(#24061,#24062,#24063));
#6569=EDGE_LOOP('',(#24064,#24065,#24066,#24067));
#6570=EDGE_LOOP('',(#24068,#24069,#24070));
#6571=EDGE_LOOP('',(#24071,#24072,#24073,#24074));
#6572=EDGE_LOOP('',(#24075,#24076,#24077));
#6573=EDGE_LOOP('',(#24078,#24079,#24080,#24081));
#6574=EDGE_LOOP('',(#24082,#24083,#24084));
#6575=EDGE_LOOP('',(#24085,#24086,#24087,#24088));
#6576=EDGE_LOOP('',(#24089,#24090,#24091));
#6577=EDGE_LOOP('',(#24092,#24093,#24094,#24095));
#6578=EDGE_LOOP('',(#24096,#24097,#24098));
#6579=EDGE_LOOP('',(#24099,#24100,#24101,#24102));
#6580=EDGE_LOOP('',(#24103,#24104,#24105));
#6581=EDGE_LOOP('',(#24106,#24107,#24108,#24109));
#6582=EDGE_LOOP('',(#24110,#24111,#24112));
#6583=EDGE_LOOP('',(#24113,#24114,#24115,#24116));
#6584=EDGE_LOOP('',(#24117,#24118,#24119));
#6585=EDGE_LOOP('',(#24120,#24121,#24122,#24123));
#6586=EDGE_LOOP('',(#24124,#24125,#24126));
#6587=EDGE_LOOP('',(#24127,#24128,#24129));
#6588=EDGE_LOOP('',(#24130,#24131,#24132,#24133));
#6589=EDGE_LOOP('',(#24134,#24135,#24136,#24137));
#6590=EDGE_LOOP('',(#24138,#24139,#24140,#24141));
#6591=EDGE_LOOP('',(#24142,#24143,#24144,#24145));
#6592=EDGE_LOOP('',(#24146,#24147,#24148,#24149));
#6593=EDGE_LOOP('',(#24150,#24151,#24152,#24153));
#6594=EDGE_LOOP('',(#24154,#24155,#24156,#24157,#24158,#24159));
#6595=EDGE_LOOP('',(#24160));
#6596=EDGE_LOOP('',(#24161));
#6597=EDGE_LOOP('',(#24162,#24163,#24164,#24165,#24166,#24167));
#6598=EDGE_LOOP('',(#24168,#24169,#24170,#24171,#24172,#24173,#24174,#24175,
#24176,#24177,#24178,#24179));
#6599=EDGE_LOOP('',(#24180,#24181,#24182,#24183));
#6600=EDGE_LOOP('',(#24184,#24185,#24186,#24187));
#6601=EDGE_LOOP('',(#24188,#24189,#24190,#24191));
#6602=EDGE_LOOP('',(#24192,#24193,#24194,#24195));
#6603=EDGE_LOOP('',(#24196,#24197,#24198,#24199));
#6604=EDGE_LOOP('',(#24200,#24201,#24202,#24203));
#6605=EDGE_LOOP('',(#24204,#24205,#24206,#24207));
#6606=EDGE_LOOP('',(#24208,#24209,#24210,#24211));
#6607=EDGE_LOOP('',(#24212,#24213,#24214,#24215));
#6608=EDGE_LOOP('',(#24216,#24217,#24218,#24219));
#6609=EDGE_LOOP('',(#24220,#24221,#24222,#24223));
#6610=EDGE_LOOP('',(#24224,#24225,#24226,#24227));
#6611=EDGE_LOOP('',(#24228,#24229,#24230,#24231));
#6612=EDGE_LOOP('',(#24232,#24233,#24234,#24235));
#6613=EDGE_LOOP('',(#24236,#24237,#24238,#24239));
#6614=EDGE_LOOP('',(#24240,#24241,#24242,#24243));
#6615=EDGE_LOOP('',(#24244,#24245,#24246,#24247));
#6616=EDGE_LOOP('',(#24248,#24249,#24250,#24251));
#6617=EDGE_LOOP('',(#24252,#24253,#24254,#24255));
#6618=EDGE_LOOP('',(#24256,#24257,#24258,#24259));
#6619=EDGE_LOOP('',(#24260,#24261,#24262,#24263));
#6620=EDGE_LOOP('',(#24264,#24265,#24266,#24267));
#6621=EDGE_LOOP('',(#24268,#24269,#24270,#24271));
#6622=EDGE_LOOP('',(#24272,#24273,#24274,#24275));
#6623=EDGE_LOOP('',(#24276,#24277,#24278,#24279));
#6624=EDGE_LOOP('',(#24280,#24281,#24282,#24283));
#6625=EDGE_LOOP('',(#24284,#24285,#24286,#24287));
#6626=EDGE_LOOP('',(#24288,#24289,#24290,#24291));
#6627=EDGE_LOOP('',(#24292,#24293,#24294,#24295));
#6628=EDGE_LOOP('',(#24296,#24297,#24298,#24299));
#6629=EDGE_LOOP('',(#24300,#24301,#24302,#24303));
#6630=EDGE_LOOP('',(#24304,#24305,#24306,#24307));
#6631=EDGE_LOOP('',(#24308,#24309,#24310,#24311));
#6632=EDGE_LOOP('',(#24312,#24313,#24314,#24315));
#6633=EDGE_LOOP('',(#24316,#24317,#24318,#24319));
#6634=EDGE_LOOP('',(#24320,#24321,#24322,#24323));
#6635=EDGE_LOOP('',(#24324));
#6636=EDGE_LOOP('',(#24325,#24326,#24327,#24328,#24329,#24330));
#6637=EDGE_LOOP('',(#24331));
#6638=EDGE_LOOP('',(#24332,#24333,#24334,#24335));
#6639=EDGE_LOOP('',(#24336,#24337,#24338,#24339));
#6640=EDGE_LOOP('',(#24340,#24341,#24342,#24343));
#6641=EDGE_LOOP('',(#24344));
#6642=EDGE_LOOP('',(#24345,#24346,#24347,#24348));
#6643=EDGE_LOOP('',(#24349,#24350,#24351,#24352));
#6644=EDGE_LOOP('',(#24353,#24354,#24355,#24356));
#6645=EDGE_LOOP('',(#24357,#24358,#24359,#24360));
#6646=EDGE_LOOP('',(#24361,#24362,#24363,#24364));
#6647=EDGE_LOOP('',(#24365,#24366,#24367,#24368));
#6648=EDGE_LOOP('',(#24369,#24370,#24371,#24372));
#6649=EDGE_LOOP('',(#24373,#24374,#24375,#24376));
#6650=EDGE_LOOP('',(#24377,#24378,#24379,#24380));
#6651=EDGE_LOOP('',(#24381,#24382,#24383,#24384));
#6652=EDGE_LOOP('',(#24385,#24386,#24387,#24388));
#6653=EDGE_LOOP('',(#24389,#24390,#24391,#24392));
#6654=EDGE_LOOP('',(#24393,#24394,#24395,#24396));
#6655=EDGE_LOOP('',(#24397,#24398,#24399,#24400));
#6656=EDGE_LOOP('',(#24401,#24402,#24403,#24404));
#6657=EDGE_LOOP('',(#24405,#24406,#24407,#24408));
#6658=EDGE_LOOP('',(#24409,#24410,#24411,#24412));
#6659=EDGE_LOOP('',(#24413,#24414,#24415,#24416));
#6660=EDGE_LOOP('',(#24417,#24418,#24419,#24420));
#6661=EDGE_LOOP('',(#24421,#24422,#24423,#24424));
#6662=EDGE_LOOP('',(#24425,#24426,#24427,#24428));
#6663=EDGE_LOOP('',(#24429,#24430,#24431,#24432));
#6664=EDGE_LOOP('',(#24433,#24434,#24435,#24436));
#6665=EDGE_LOOP('',(#24437,#24438,#24439,#24440));
#6666=EDGE_LOOP('',(#24441,#24442,#24443,#24444));
#6667=EDGE_LOOP('',(#24445,#24446,#24447,#24448));
#6668=EDGE_LOOP('',(#24449,#24450,#24451,#24452));
#6669=EDGE_LOOP('',(#24453,#24454,#24455,#24456));
#6670=EDGE_LOOP('',(#24457,#24458,#24459,#24460));
#6671=EDGE_LOOP('',(#24461,#24462,#24463,#24464));
#6672=EDGE_LOOP('',(#24465,#24466,#24467,#24468));
#6673=EDGE_LOOP('',(#24469,#24470,#24471,#24472));
#6674=EDGE_LOOP('',(#24473,#24474,#24475,#24476));
#6675=EDGE_LOOP('',(#24477,#24478,#24479,#24480));
#6676=EDGE_LOOP('',(#24481,#24482,#24483,#24484));
#6677=EDGE_LOOP('',(#24485,#24486,#24487,#24488));
#6678=EDGE_LOOP('',(#24489,#24490,#24491,#24492));
#6679=EDGE_LOOP('',(#24493,#24494,#24495,#24496));
#6680=EDGE_LOOP('',(#24497,#24498,#24499,#24500));
#6681=EDGE_LOOP('',(#24501,#24502,#24503,#24504));
#6682=EDGE_LOOP('',(#24505,#24506,#24507,#24508));
#6683=EDGE_LOOP('',(#24509,#24510,#24511,#24512));
#6684=EDGE_LOOP('',(#24513,#24514,#24515,#24516));
#6685=EDGE_LOOP('',(#24517,#24518,#24519,#24520));
#6686=EDGE_LOOP('',(#24521,#24522,#24523,#24524));
#6687=EDGE_LOOP('',(#24525,#24526,#24527,#24528));
#6688=EDGE_LOOP('',(#24529,#24530,#24531,#24532));
#6689=EDGE_LOOP('',(#24533,#24534,#24535,#24536));
#6690=EDGE_LOOP('',(#24537,#24538,#24539,#24540));
#6691=EDGE_LOOP('',(#24541,#24542,#24543,#24544));
#6692=EDGE_LOOP('',(#24545,#24546,#24547,#24548));
#6693=EDGE_LOOP('',(#24549,#24550,#24551,#24552));
#6694=EDGE_LOOP('',(#24553,#24554,#24555,#24556));
#6695=EDGE_LOOP('',(#24557,#24558,#24559,#24560));
#6696=EDGE_LOOP('',(#24561,#24562,#24563,#24564));
#6697=EDGE_LOOP('',(#24565,#24566,#24567,#24568));
#6698=EDGE_LOOP('',(#24569,#24570,#24571,#24572));
#6699=EDGE_LOOP('',(#24573,#24574,#24575,#24576));
#6700=EDGE_LOOP('',(#24577,#24578,#24579,#24580));
#6701=EDGE_LOOP('',(#24581,#24582,#24583,#24584));
#6702=EDGE_LOOP('',(#24585,#24586,#24587,#24588));
#6703=EDGE_LOOP('',(#24589,#24590,#24591,#24592));
#6704=EDGE_LOOP('',(#24593,#24594,#24595,#24596));
#6705=EDGE_LOOP('',(#24597,#24598,#24599,#24600));
#6706=EDGE_LOOP('',(#24601,#24602,#24603,#24604));
#6707=EDGE_LOOP('',(#24605,#24606,#24607,#24608));
#6708=EDGE_LOOP('',(#24609,#24610,#24611,#24612));
#6709=EDGE_LOOP('',(#24613,#24614,#24615,#24616));
#6710=EDGE_LOOP('',(#24617,#24618,#24619,#24620));
#6711=EDGE_LOOP('',(#24621,#24622,#24623,#24624));
#6712=EDGE_LOOP('',(#24625,#24626,#24627,#24628));
#6713=EDGE_LOOP('',(#24629,#24630,#24631,#24632));
#6714=EDGE_LOOP('',(#24633,#24634,#24635,#24636));
#6715=EDGE_LOOP('',(#24637,#24638,#24639,#24640));
#6716=EDGE_LOOP('',(#24641,#24642,#24643,#24644));
#6717=EDGE_LOOP('',(#24645,#24646,#24647,#24648));
#6718=EDGE_LOOP('',(#24649,#24650,#24651,#24652));
#6719=EDGE_LOOP('',(#24653,#24654,#24655,#24656));
#6720=EDGE_LOOP('',(#24657,#24658,#24659,#24660));
#6721=EDGE_LOOP('',(#24661,#24662,#24663,#24664));
#6722=EDGE_LOOP('',(#24665,#24666,#24667,#24668));
#6723=EDGE_LOOP('',(#24669,#24670,#24671,#24672));
#6724=EDGE_LOOP('',(#24673,#24674,#24675,#24676));
#6725=EDGE_LOOP('',(#24677,#24678,#24679,#24680));
#6726=EDGE_LOOP('',(#24681,#24682,#24683,#24684));
#6727=EDGE_LOOP('',(#24685,#24686,#24687,#24688));
#6728=EDGE_LOOP('',(#24689,#24690,#24691,#24692));
#6729=EDGE_LOOP('',(#24693,#24694,#24695,#24696));
#6730=EDGE_LOOP('',(#24697,#24698,#24699,#24700));
#6731=EDGE_LOOP('',(#24701,#24702,#24703,#24704));
#6732=EDGE_LOOP('',(#24705,#24706,#24707,#24708));
#6733=EDGE_LOOP('',(#24709,#24710,#24711,#24712));
#6734=EDGE_LOOP('',(#24713,#24714,#24715,#24716));
#6735=EDGE_LOOP('',(#24717,#24718,#24719,#24720));
#6736=EDGE_LOOP('',(#24721,#24722,#24723,#24724));
#6737=EDGE_LOOP('',(#24725,#24726,#24727,#24728));
#6738=EDGE_LOOP('',(#24729,#24730,#24731,#24732));
#6739=EDGE_LOOP('',(#24733,#24734,#24735,#24736));
#6740=EDGE_LOOP('',(#24737,#24738,#24739,#24740));
#6741=EDGE_LOOP('',(#24741,#24742,#24743,#24744));
#6742=EDGE_LOOP('',(#24745,#24746,#24747,#24748));
#6743=EDGE_LOOP('',(#24749,#24750,#24751,#24752));
#6744=EDGE_LOOP('',(#24753,#24754,#24755,#24756));
#6745=EDGE_LOOP('',(#24757,#24758,#24759,#24760));
#6746=EDGE_LOOP('',(#24761,#24762,#24763,#24764));
#6747=EDGE_LOOP('',(#24765,#24766,#24767,#24768));
#6748=EDGE_LOOP('',(#24769,#24770,#24771,#24772));
#6749=EDGE_LOOP('',(#24773,#24774,#24775,#24776));
#6750=EDGE_LOOP('',(#24777,#24778,#24779,#24780));
#6751=EDGE_LOOP('',(#24781,#24782,#24783,#24784));
#6752=EDGE_LOOP('',(#24785,#24786,#24787,#24788));
#6753=EDGE_LOOP('',(#24789,#24790,#24791,#24792));
#6754=EDGE_LOOP('',(#24793,#24794,#24795,#24796));
#6755=EDGE_LOOP('',(#24797,#24798,#24799,#24800));
#6756=EDGE_LOOP('',(#24801,#24802,#24803,#24804));
#6757=EDGE_LOOP('',(#24805,#24806,#24807,#24808));
#6758=EDGE_LOOP('',(#24809,#24810,#24811,#24812));
#6759=EDGE_LOOP('',(#24813,#24814,#24815,#24816));
#6760=EDGE_LOOP('',(#24817,#24818,#24819,#24820));
#6761=EDGE_LOOP('',(#24821,#24822,#24823,#24824));
#6762=EDGE_LOOP('',(#24825,#24826,#24827,#24828));
#6763=EDGE_LOOP('',(#24829,#24830,#24831,#24832));
#6764=EDGE_LOOP('',(#24833,#24834,#24835,#24836));
#6765=EDGE_LOOP('',(#24837,#24838,#24839,#24840));
#6766=EDGE_LOOP('',(#24841,#24842,#24843,#24844));
#6767=EDGE_LOOP('',(#24845,#24846,#24847,#24848));
#6768=EDGE_LOOP('',(#24849,#24850,#24851,#24852));
#6769=EDGE_LOOP('',(#24853,#24854,#24855,#24856));
#6770=EDGE_LOOP('',(#24857,#24858,#24859,#24860));
#6771=EDGE_LOOP('',(#24861,#24862,#24863,#24864));
#6772=EDGE_LOOP('',(#24865,#24866,#24867,#24868));
#6773=EDGE_LOOP('',(#24869,#24870,#24871,#24872));
#6774=EDGE_LOOP('',(#24873,#24874,#24875,#24876));
#6775=EDGE_LOOP('',(#24877,#24878,#24879,#24880));
#6776=EDGE_LOOP('',(#24881,#24882,#24883,#24884));
#6777=EDGE_LOOP('',(#24885,#24886,#24887,#24888));
#6778=EDGE_LOOP('',(#24889,#24890,#24891,#24892));
#6779=EDGE_LOOP('',(#24893,#24894,#24895,#24896));
#6780=EDGE_LOOP('',(#24897,#24898,#24899,#24900,#24901));
#6781=EDGE_LOOP('',(#24902,#24903,#24904,#24905,#24906,#24907,#24908,#24909,
#24910,#24911,#24912,#24913,#24914,#24915,#24916,#24917,#24918,#24919,#24920,
#24921,#24922,#24923,#24924,#24925,#24926,#24927,#24928,#24929,#24930,#24931,
#24932,#24933,#24934,#24935,#24936,#24937,#24938,#24939,#24940,#24941,#24942,
#24943,#24944,#24945,#24946,#24947,#24948,#24949,#24950,#24951,#24952,#24953,
#24954,#24955,#24956,#24957,#24958,#24959,#24960,#24961,#24962,#24963,#24964,
#24965,#24966,#24967,#24968,#24969,#24970,#24971,#24972,#24973,#24974,#24975,
#24976,#24977,#24978,#24979,#24980,#24981,#24982,#24983,#24984,#24985,#24986,
#24987,#24988,#24989,#24990,#24991,#24992,#24993,#24994,#24995,#24996,#24997,
#24998,#24999,#25000,#25001,#25002,#25003,#25004,#25005,#25006,#25007,#25008,
#25009,#25010,#25011,#25012,#25013,#25014,#25015,#25016,#25017,#25018,#25019,
#25020,#25021,#25022,#25023,#25024,#25025,#25026,#25027,#25028,#25029,#25030,
#25031,#25032,#25033,#25034,#25035,#25036,#25037,#25038,#25039,#25040,#25041,
#25042,#25043));
#6782=EDGE_LOOP('',(#25044,#25045,#25046,#25047,#25048));
#6783=EDGE_LOOP('',(#25049,#25050,#25051,#25052));
#6784=EDGE_LOOP('',(#25053,#25054,#25055,#25056,#25057,#25058,#25059,#25060,
#25061,#25062,#25063,#25064,#25065,#25066,#25067,#25068,#25069,#25070,#25071,
#25072,#25073,#25074,#25075,#25076,#25077,#25078,#25079,#25080,#25081,#25082,
#25083,#25084,#25085,#25086,#25087,#25088,#25089,#25090,#25091,#25092,#25093,
#25094,#25095,#25096,#25097,#25098,#25099,#25100,#25101,#25102,#25103,#25104,
#25105,#25106,#25107,#25108,#25109,#25110,#25111,#25112,#25113,#25114,#25115,
#25116,#25117,#25118,#25119,#25120,#25121,#25122,#25123,#25124,#25125,#25126,
#25127,#25128,#25129,#25130,#25131,#25132,#25133,#25134,#25135,#25136,#25137,
#25138,#25139,#25140,#25141,#25142,#25143,#25144,#25145,#25146,#25147,#25148,
#25149,#25150,#25151,#25152,#25153,#25154,#25155,#25156,#25157,#25158,#25159,
#25160,#25161,#25162,#25163,#25164,#25165,#25166,#25167,#25168,#25169,#25170,
#25171,#25172,#25173,#25174,#25175,#25176,#25177,#25178,#25179,#25180,#25181,
#25182,#25183,#25184,#25185,#25186,#25187,#25188,#25189,#25190,#25191,#25192,
#25193,#25194));
#6785=EDGE_LOOP('',(#25195,#25196,#25197,#25198,#25199,#25200));
#6786=EDGE_LOOP('',(#25201,#25202,#25203,#25204));
#6787=EDGE_LOOP('',(#25205));
#6788=EDGE_LOOP('',(#25206));
#6789=EDGE_LOOP('',(#25207,#25208,#25209,#25210));
#6790=EDGE_LOOP('',(#25211,#25212,#25213));
#6791=EDGE_LOOP('',(#25214,#25215,#25216,#25217));
#6792=EDGE_LOOP('',(#25218,#25219,#25220));
#6793=EDGE_LOOP('',(#25221,#25222,#25223,#25224));
#6794=EDGE_LOOP('',(#25225,#25226,#25227));
#6795=EDGE_LOOP('',(#25228,#25229,#25230,#25231));
#6796=EDGE_LOOP('',(#25232,#25233,#25234));
#6797=EDGE_LOOP('',(#25235,#25236,#25237,#25238));
#6798=EDGE_LOOP('',(#25239,#25240,#25241));
#6799=EDGE_LOOP('',(#25242,#25243,#25244,#25245));
#6800=EDGE_LOOP('',(#25246,#25247,#25248));
#6801=EDGE_LOOP('',(#25249,#25250,#25251,#25252));
#6802=EDGE_LOOP('',(#25253,#25254,#25255));
#6803=EDGE_LOOP('',(#25256,#25257,#25258,#25259));
#6804=EDGE_LOOP('',(#25260,#25261,#25262));
#6805=EDGE_LOOP('',(#25263,#25264,#25265,#25266));
#6806=EDGE_LOOP('',(#25267,#25268,#25269));
#6807=EDGE_LOOP('',(#25270,#25271,#25272,#25273));
#6808=EDGE_LOOP('',(#25274,#25275,#25276));
#6809=EDGE_LOOP('',(#25277,#25278,#25279,#25280));
#6810=EDGE_LOOP('',(#25281,#25282,#25283));
#6811=EDGE_LOOP('',(#25284,#25285,#25286,#25287));
#6812=EDGE_LOOP('',(#25288,#25289,#25290));
#6813=EDGE_LOOP('',(#25291,#25292,#25293,#25294));
#6814=EDGE_LOOP('',(#25295,#25296,#25297));
#6815=EDGE_LOOP('',(#25298,#25299,#25300,#25301));
#6816=EDGE_LOOP('',(#25302,#25303,#25304));
#6817=EDGE_LOOP('',(#25305,#25306,#25307,#25308));
#6818=EDGE_LOOP('',(#25309,#25310,#25311));
#6819=EDGE_LOOP('',(#25312,#25313,#25314,#25315));
#6820=EDGE_LOOP('',(#25316,#25317,#25318));
#6821=EDGE_LOOP('',(#25319,#25320,#25321,#25322));
#6822=EDGE_LOOP('',(#25323,#25324,#25325));
#6823=EDGE_LOOP('',(#25326,#25327,#25328,#25329));
#6824=EDGE_LOOP('',(#25330,#25331,#25332));
#6825=EDGE_LOOP('',(#25333,#25334,#25335,#25336));
#6826=EDGE_LOOP('',(#25337,#25338,#25339));
#6827=EDGE_LOOP('',(#25340,#25341,#25342,#25343));
#6828=EDGE_LOOP('',(#25344,#25345,#25346));
#6829=EDGE_LOOP('',(#25347,#25348,#25349,#25350));
#6830=EDGE_LOOP('',(#25351,#25352,#25353));
#6831=EDGE_LOOP('',(#25354,#25355,#25356,#25357));
#6832=EDGE_LOOP('',(#25358,#25359,#25360));
#6833=EDGE_LOOP('',(#25361,#25362,#25363,#25364));
#6834=EDGE_LOOP('',(#25365,#25366,#25367));
#6835=EDGE_LOOP('',(#25368,#25369,#25370,#25371));
#6836=EDGE_LOOP('',(#25372,#25373,#25374));
#6837=EDGE_LOOP('',(#25375,#25376,#25377,#25378));
#6838=EDGE_LOOP('',(#25379,#25380,#25381));
#6839=EDGE_LOOP('',(#25382,#25383,#25384,#25385));
#6840=EDGE_LOOP('',(#25386,#25387,#25388));
#6841=EDGE_LOOP('',(#25389,#25390,#25391,#25392));
#6842=EDGE_LOOP('',(#25393,#25394,#25395));
#6843=EDGE_LOOP('',(#25396,#25397,#25398,#25399));
#6844=EDGE_LOOP('',(#25400,#25401,#25402));
#6845=EDGE_LOOP('',(#25403,#25404,#25405,#25406));
#6846=EDGE_LOOP('',(#25407,#25408,#25409));
#6847=EDGE_LOOP('',(#25410,#25411,#25412,#25413));
#6848=EDGE_LOOP('',(#25414,#25415,#25416));
#6849=EDGE_LOOP('',(#25417,#25418,#25419,#25420));
#6850=EDGE_LOOP('',(#25421,#25422,#25423));
#6851=EDGE_LOOP('',(#25424,#25425,#25426,#25427));
#6852=EDGE_LOOP('',(#25428,#25429,#25430));
#6853=EDGE_LOOP('',(#25431,#25432,#25433,#25434));
#6854=EDGE_LOOP('',(#25435,#25436,#25437));
#6855=EDGE_LOOP('',(#25438,#25439,#25440,#25441));
#6856=EDGE_LOOP('',(#25442,#25443,#25444));
#6857=EDGE_LOOP('',(#25445,#25446,#25447,#25448));
#6858=EDGE_LOOP('',(#25449,#25450,#25451,#25452));
#6859=EDGE_LOOP('',(#25453,#25454,#25455,#25456));
#6860=EDGE_LOOP('',(#25457,#25458,#25459,#25460));
#6861=EDGE_LOOP('',(#25461,#25462,#25463,#25464));
#6862=EDGE_LOOP('',(#25465,#25466,#25467));
#6863=EDGE_LOOP('',(#25468,#25469,#25470,#25471));
#6864=EDGE_LOOP('',(#25472,#25473,#25474));
#6865=EDGE_LOOP('',(#25475,#25476,#25477,#25478));
#6866=EDGE_LOOP('',(#25479,#25480,#25481));
#6867=EDGE_LOOP('',(#25482,#25483,#25484,#25485));
#6868=EDGE_LOOP('',(#25486,#25487,#25488));
#6869=EDGE_LOOP('',(#25489,#25490,#25491,#25492));
#6870=EDGE_LOOP('',(#25493,#25494,#25495));
#6871=EDGE_LOOP('',(#25496,#25497,#25498,#25499));
#6872=EDGE_LOOP('',(#25500,#25501,#25502));
#6873=EDGE_LOOP('',(#25503,#25504,#25505,#25506));
#6874=EDGE_LOOP('',(#25507,#25508,#25509));
#6875=EDGE_LOOP('',(#25510,#25511,#25512,#25513));
#6876=EDGE_LOOP('',(#25514,#25515,#25516));
#6877=EDGE_LOOP('',(#25517,#25518,#25519,#25520));
#6878=EDGE_LOOP('',(#25521,#25522,#25523));
#6879=EDGE_LOOP('',(#25524,#25525,#25526,#25527));
#6880=EDGE_LOOP('',(#25528,#25529,#25530));
#6881=EDGE_LOOP('',(#25531,#25532,#25533,#25534));
#6882=EDGE_LOOP('',(#25535,#25536,#25537));
#6883=EDGE_LOOP('',(#25538,#25539,#25540,#25541));
#6884=EDGE_LOOP('',(#25542,#25543,#25544));
#6885=EDGE_LOOP('',(#25545,#25546,#25547,#25548));
#6886=EDGE_LOOP('',(#25549,#25550,#25551));
#6887=EDGE_LOOP('',(#25552,#25553,#25554,#25555));
#6888=EDGE_LOOP('',(#25556,#25557,#25558));
#6889=EDGE_LOOP('',(#25559,#25560,#25561,#25562));
#6890=EDGE_LOOP('',(#25563,#25564,#25565));
#6891=EDGE_LOOP('',(#25566,#25567,#25568,#25569));
#6892=EDGE_LOOP('',(#25570,#25571,#25572));
#6893=EDGE_LOOP('',(#25573,#25574,#25575,#25576));
#6894=EDGE_LOOP('',(#25577,#25578,#25579));
#6895=EDGE_LOOP('',(#25580,#25581,#25582,#25583));
#6896=EDGE_LOOP('',(#25584,#25585,#25586));
#6897=EDGE_LOOP('',(#25587,#25588,#25589,#25590));
#6898=EDGE_LOOP('',(#25591,#25592,#25593));
#6899=EDGE_LOOP('',(#25594,#25595,#25596,#25597));
#6900=EDGE_LOOP('',(#25598,#25599,#25600));
#6901=EDGE_LOOP('',(#25601,#25602,#25603,#25604));
#6902=EDGE_LOOP('',(#25605,#25606,#25607));
#6903=EDGE_LOOP('',(#25608,#25609,#25610,#25611));
#6904=EDGE_LOOP('',(#25612,#25613,#25614));
#6905=EDGE_LOOP('',(#25615,#25616,#25617,#25618));
#6906=EDGE_LOOP('',(#25619,#25620,#25621));
#6907=EDGE_LOOP('',(#25622,#25623,#25624,#25625));
#6908=EDGE_LOOP('',(#25626,#25627,#25628));
#6909=EDGE_LOOP('',(#25629,#25630,#25631,#25632));
#6910=EDGE_LOOP('',(#25633,#25634,#25635));
#6911=EDGE_LOOP('',(#25636,#25637,#25638,#25639));
#6912=EDGE_LOOP('',(#25640,#25641,#25642));
#6913=EDGE_LOOP('',(#25643,#25644,#25645,#25646));
#6914=EDGE_LOOP('',(#25647,#25648,#25649));
#6915=EDGE_LOOP('',(#25650,#25651,#25652,#25653));
#6916=EDGE_LOOP('',(#25654,#25655,#25656));
#6917=EDGE_LOOP('',(#25657,#25658,#25659,#25660));
#6918=EDGE_LOOP('',(#25661,#25662,#25663));
#6919=EDGE_LOOP('',(#25664,#25665,#25666,#25667));
#6920=EDGE_LOOP('',(#25668,#25669,#25670));
#6921=EDGE_LOOP('',(#25671,#25672,#25673,#25674));
#6922=EDGE_LOOP('',(#25675,#25676,#25677));
#6923=EDGE_LOOP('',(#25678,#25679,#25680,#25681));
#6924=EDGE_LOOP('',(#25682,#25683,#25684));
#6925=EDGE_LOOP('',(#25685,#25686,#25687,#25688));
#6926=EDGE_LOOP('',(#25689,#25690,#25691));
#6927=EDGE_LOOP('',(#25692,#25693,#25694,#25695));
#6928=EDGE_LOOP('',(#25696,#25697,#25698));
#6929=EDGE_LOOP('',(#25699,#25700,#25701,#25702));
#6930=EDGE_LOOP('',(#25703,#25704,#25705));
#6931=EDGE_LOOP('',(#25706,#25707,#25708,#25709));
#6932=EDGE_LOOP('',(#25710,#25711,#25712));
#6933=EDGE_LOOP('',(#25713,#25714,#25715));
#6934=EDGE_LOOP('',(#25716,#25717,#25718,#25719));
#6935=EDGE_LOOP('',(#25720,#25721,#25722,#25723));
#6936=EDGE_LOOP('',(#25724,#25725,#25726,#25727));
#6937=EDGE_LOOP('',(#25728,#25729,#25730,#25731));
#6938=EDGE_LOOP('',(#25732,#25733,#25734,#25735));
#6939=EDGE_LOOP('',(#25736,#25737,#25738,#25739));
#6940=EDGE_LOOP('',(#25740,#25741,#25742,#25743,#25744,#25745));
#6941=EDGE_LOOP('',(#25746));
#6942=EDGE_LOOP('',(#25747));
#6943=EDGE_LOOP('',(#25748,#25749,#25750,#25751,#25752,#25753));
#6944=EDGE_LOOP('',(#25754,#25755,#25756,#25757,#25758,#25759,#25760,#25761,
#25762,#25763,#25764,#25765));
#6945=EDGE_LOOP('',(#25766,#25767,#25768,#25769));
#6946=EDGE_LOOP('',(#25770,#25771,#25772,#25773));
#6947=EDGE_LOOP('',(#25774,#25775,#25776,#25777));
#6948=EDGE_LOOP('',(#25778,#25779,#25780,#25781));
#6949=EDGE_LOOP('',(#25782,#25783,#25784,#25785));
#6950=EDGE_LOOP('',(#25786,#25787,#25788,#25789));
#6951=EDGE_LOOP('',(#25790,#25791,#25792,#25793));
#6952=EDGE_LOOP('',(#25794,#25795,#25796,#25797));
#6953=EDGE_LOOP('',(#25798,#25799,#25800,#25801));
#6954=EDGE_LOOP('',(#25802,#25803,#25804,#25805));
#6955=EDGE_LOOP('',(#25806,#25807,#25808,#25809));
#6956=EDGE_LOOP('',(#25810,#25811,#25812,#25813));
#6957=EDGE_LOOP('',(#25814,#25815,#25816,#25817));
#6958=EDGE_LOOP('',(#25818,#25819,#25820,#25821));
#6959=EDGE_LOOP('',(#25822,#25823,#25824,#25825));
#6960=EDGE_LOOP('',(#25826,#25827,#25828,#25829));
#6961=EDGE_LOOP('',(#25830,#25831,#25832,#25833));
#6962=EDGE_LOOP('',(#25834,#25835,#25836,#25837));
#6963=EDGE_LOOP('',(#25838,#25839,#25840,#25841));
#6964=EDGE_LOOP('',(#25842,#25843,#25844,#25845));
#6965=EDGE_LOOP('',(#25846,#25847,#25848,#25849));
#6966=EDGE_LOOP('',(#25850,#25851,#25852,#25853));
#6967=EDGE_LOOP('',(#25854,#25855,#25856,#25857));
#6968=EDGE_LOOP('',(#25858,#25859,#25860,#25861));
#6969=EDGE_LOOP('',(#25862,#25863,#25864,#25865));
#6970=EDGE_LOOP('',(#25866,#25867,#25868,#25869));
#6971=EDGE_LOOP('',(#25870,#25871,#25872,#25873));
#6972=EDGE_LOOP('',(#25874,#25875,#25876,#25877));
#6973=EDGE_LOOP('',(#25878,#25879,#25880,#25881));
#6974=EDGE_LOOP('',(#25882,#25883,#25884,#25885));
#6975=EDGE_LOOP('',(#25886,#25887,#25888,#25889));
#6976=EDGE_LOOP('',(#25890,#25891,#25892,#25893));
#6977=EDGE_LOOP('',(#25894,#25895,#25896,#25897));
#6978=EDGE_LOOP('',(#25898,#25899,#25900,#25901));
#6979=EDGE_LOOP('',(#25902,#25903,#25904,#25905));
#6980=EDGE_LOOP('',(#25906,#25907,#25908,#25909));
#6981=EDGE_LOOP('',(#25910));
#6982=EDGE_LOOP('',(#25911,#25912,#25913,#25914,#25915,#25916));
#6983=EDGE_LOOP('',(#25917,#25918,#25919,#25920));
#6984=EDGE_LOOP('',(#25921,#25922,#25923,#25924));
#6985=EDGE_LOOP('',(#25925,#25926,#25927,#25928));
#6986=EDGE_LOOP('',(#25929,#25930,#25931,#25932));
#6987=EDGE_LOOP('',(#25933,#25934,#25935,#25936,#25937,#25938));
#6988=EDGE_LOOP('',(#25939,#25940,#25941,#25942));
#6989=EDGE_LOOP('',(#25943,#25944,#25945,#25946,#25947,#25948,#25949,#25950));
#6990=EDGE_LOOP('',(#25951,#25952,#25953,#25954,#25955,#25956));
#6991=EDGE_LOOP('',(#25957,#25958,#25959,#25960));
#6992=EDGE_LOOP('',(#25961,#25962,#25963,#25964));
#6993=EDGE_LOOP('',(#25965,#25966,#25967,#25968));
#6994=EDGE_LOOP('',(#25969,#25970,#25971,#25972,#25973,#25974,#25975,#25976));
#6995=EDGE_LOOP('',(#25977,#25978,#25979,#25980));
#6996=EDGE_LOOP('',(#25981,#25982,#25983,#25984));
#6997=EDGE_LOOP('',(#25985,#25986,#25987,#25988,#25989,#25990));
#6998=EDGE_LOOP('',(#25991,#25992,#25993,#25994));
#6999=EDGE_LOOP('',(#25995,#25996,#25997,#25998));
#7000=EDGE_LOOP('',(#25999,#26000,#26001,#26002));
#7001=EDGE_LOOP('',(#26003,#26004,#26005,#26006,#26007,#26008));
#7002=EDGE_LOOP('',(#26009,#26010,#26011,#26012,#26013,#26014,#26015,#26016));
#7003=EDGE_LOOP('',(#26017,#26018,#26019,#26020));
#7004=EDGE_LOOP('',(#26021,#26022,#26023,#26024));
#7005=EDGE_LOOP('',(#26025,#26026,#26027,#26028,#26029,#26030));
#7006=EDGE_LOOP('',(#26031,#26032,#26033,#26034));
#7007=EDGE_LOOP('',(#26035,#26036,#26037,#26038));
#7008=EDGE_LOOP('',(#26039,#26040,#26041,#26042));
#7009=EDGE_LOOP('',(#26043,#26044,#26045,#26046));
#7010=EDGE_LOOP('',(#26047,#26048,#26049,#26050));
#7011=EDGE_LOOP('',(#26051,#26052,#26053,#26054));
#7012=EDGE_LOOP('',(#26055,#26056,#26057,#26058));
#7013=EDGE_LOOP('',(#26059,#26060,#26061,#26062,#26063,#26064));
#7014=EDGE_LOOP('',(#26065,#26066,#26067,#26068,#26069,#26070,#26071,#26072));
#7015=EDGE_LOOP('',(#26073,#26074,#26075,#26076));
#7016=EDGE_LOOP('',(#26077,#26078,#26079,#26080,#26081,#26082));
#7017=EDGE_LOOP('',(#26083,#26084,#26085,#26086,#26087,#26088,#26089,#26090));
#7018=EDGE_LOOP('',(#26091,#26092,#26093,#26094,#26095,#26096,#26097,#26098,
#26099,#26100,#26101,#26102,#26103,#26104,#26105,#26106));
#7019=EDGE_LOOP('',(#26107));
#7020=EDGE_LOOP('',(#26108,#26109,#26110,#26111,#26112,#26113,#26114,#26115));
#7021=EDGE_LOOP('',(#26116,#26117,#26118,#26119,#26120,#26121,#26122,#26123));
#7022=EDGE_LOOP('',(#26124,#26125,#26126,#26127));
#7023=EDGE_LOOP('',(#26128,#26129,#26130,#26131,#26132,#26133));
#7024=EDGE_LOOP('',(#26134,#26135,#26136,#26137,#26138,#26139,#26140,#26141));
#7025=EDGE_LOOP('',(#26142,#26143,#26144,#26145));
#7026=EDGE_LOOP('',(#26146,#26147,#26148,#26149,#26150,#26151,#26152,#26153,
#26154,#26155,#26156,#26157,#26158,#26159,#26160,#26161));
#7027=EDGE_LOOP('',(#26162));
#7028=EDGE_LOOP('',(#26163,#26164,#26165,#26166));
#7029=EDGE_LOOP('',(#26167,#26168,#26169,#26170));
#7030=EDGE_LOOP('',(#26171,#26172,#26173,#26174));
#7031=EDGE_LOOP('',(#26175,#26176,#26177,#26178));
#7032=EDGE_LOOP('',(#26179,#26180,#26181,#26182));
#7033=EDGE_LOOP('',(#26183,#26184,#26185,#26186));
#7034=EDGE_LOOP('',(#26187,#26188,#26189,#26190));
#7035=EDGE_LOOP('',(#26191,#26192,#26193,#26194));
#7036=EDGE_LOOP('',(#26195,#26196,#26197,#26198));
#7037=EDGE_LOOP('',(#26199,#26200,#26201,#26202));
#7038=EDGE_LOOP('',(#26203,#26204,#26205,#26206));
#7039=EDGE_LOOP('',(#26207,#26208,#26209,#26210));
#7040=EDGE_LOOP('',(#26211,#26212,#26213,#26214));
#7041=EDGE_LOOP('',(#26215,#26216,#26217,#26218));
#7042=EDGE_LOOP('',(#26219,#26220,#26221,#26222));
#7043=EDGE_LOOP('',(#26223,#26224,#26225,#26226));
#7044=EDGE_LOOP('',(#26227,#26228,#26229));
#7045=EDGE_LOOP('',(#26230,#26231,#26232,#26233,#26234));
#7046=EDGE_LOOP('',(#26235,#26236,#26237,#26238));
#7047=EDGE_LOOP('',(#26239,#26240,#26241,#26242));
#7048=EDGE_LOOP('',(#26243,#26244,#26245,#26246));
#7049=EDGE_LOOP('',(#26247,#26248,#26249,#26250));
#7050=EDGE_LOOP('',(#26251,#26252,#26253,#26254));
#7051=EDGE_LOOP('',(#26255,#26256,#26257,#26258));
#7052=EDGE_LOOP('',(#26259,#26260,#26261,#26262));
#7053=EDGE_LOOP('',(#26263,#26264,#26265,#26266));
#7054=EDGE_LOOP('',(#26267,#26268,#26269,#26270));
#7055=EDGE_LOOP('',(#26271,#26272,#26273,#26274));
#7056=EDGE_LOOP('',(#26275,#26276,#26277,#26278));
#7057=EDGE_LOOP('',(#26279,#26280,#26281,#26282));
#7058=EDGE_LOOP('',(#26283,#26284,#26285,#26286));
#7059=EDGE_LOOP('',(#26287,#26288,#26289,#26290));
#7060=EDGE_LOOP('',(#26291,#26292,#26293,#26294,#26295));
#7061=EDGE_LOOP('',(#26296,#26297,#26298,#26299,#26300,#26301));
#7062=EDGE_LOOP('',(#26302,#26303,#26304,#26305,#26306));
#7063=EDGE_LOOP('',(#26307));
#7064=EDGE_LOOP('',(#26308));
#7065=EDGE_LOOP('',(#26309,#26310,#26311,#26312,#26313));
#7066=EDGE_LOOP('',(#26314));
#7067=EDGE_LOOP('',(#26315));
#7068=EDGE_LOOP('',(#26316,#26317,#26318,#26319,#26320));
#7069=EDGE_LOOP('',(#26321,#26322,#26323,#26324,#26325,#26326,#26327,#26328,
#26329));
#7070=EDGE_LOOP('',(#26330,#26331,#26332,#26333));
#7071=EDGE_LOOP('',(#26334));
#7072=EDGE_LOOP('',(#26335,#26336,#26337,#26338,#26339,#26340,#26341,#26342,
#26343,#26344,#26345,#26346,#26347,#26348,#26349,#26350,#26351,#26352,#26353,
#26354,#26355,#26356,#26357,#26358,#26359,#26360,#26361,#26362,#26363,#26364,
#26365,#26366,#26367,#26368,#26369));
#7073=EDGE_LOOP('',(#26370,#26371,#26372,#26373,#26374));
#7074=EDGE_LOOP('',(#26375,#26376,#26377,#26378));
#7075=EDGE_LOOP('',(#26379,#26380,#26381,#26382,#26383,#26384,#26385,#26386,
#26387,#26388,#26389,#26390,#26391,#26392,#26393,#26394,#26395,#26396,#26397,
#26398,#26399,#26400,#26401,#26402,#26403,#26404,#26405,#26406,#26407,#26408,
#26409,#26410,#26411,#26412,#26413,#26414));
#7076=EDGE_LOOP('',(#26415,#26416));
#7077=EDGE_LOOP('',(#26417,#26418));
#7078=EDGE_LOOP('',(#26419,#26420,#26421,#26422,#26423,#26424));
#7079=EDGE_LOOP('',(#26425,#26426,#26427,#26428));
#7080=EDGE_LOOP('',(#26429));
#7081=EDGE_LOOP('',(#26430,#26431,#26432,#26433,#26434));
#7082=EDGE_LOOP('',(#26435,#26436,#26437,#26438));
#7083=EDGE_LOOP('',(#26439,#26440,#26441,#26442));
#7084=EDGE_LOOP('',(#26443));
#7085=EDGE_LOOP('',(#26444));
#7086=EDGE_LOOP('',(#26445,#26446,#26447,#26448));
#7087=EDGE_LOOP('',(#26449,#26450,#26451,#26452));
#7088=EDGE_LOOP('',(#26453,#26454,#26455,#26456));
#7089=EDGE_LOOP('',(#26457,#26458,#26459,#26460));
#7090=EDGE_LOOP('',(#26461,#26462,#26463,#26464));
#7091=EDGE_LOOP('',(#26465,#26466,#26467,#26468));
#7092=EDGE_LOOP('',(#26469,#26470,#26471,#26472));
#7093=EDGE_LOOP('',(#26473,#26474,#26475,#26476));
#7094=EDGE_LOOP('',(#26477,#26478,#26479,#26480));
#7095=EDGE_LOOP('',(#26481,#26482,#26483,#26484));
#7096=EDGE_LOOP('',(#26485,#26486,#26487,#26488));
#7097=EDGE_LOOP('',(#26489,#26490,#26491,#26492));
#7098=EDGE_LOOP('',(#26493,#26494,#26495,#26496));
#7099=EDGE_LOOP('',(#26497,#26498,#26499,#26500));
#7100=EDGE_LOOP('',(#26501,#26502,#26503,#26504));
#7101=EDGE_LOOP('',(#26505,#26506,#26507,#26508));
#7102=EDGE_LOOP('',(#26509,#26510,#26511,#26512));
#7103=EDGE_LOOP('',(#26513,#26514,#26515,#26516));
#7104=EDGE_LOOP('',(#26517,#26518,#26519,#26520));
#7105=EDGE_LOOP('',(#26521,#26522,#26523,#26524));
#7106=EDGE_LOOP('',(#26525,#26526,#26527,#26528));
#7107=EDGE_LOOP('',(#26529,#26530,#26531,#26532));
#7108=EDGE_LOOP('',(#26533,#26534,#26535,#26536));
#7109=EDGE_LOOP('',(#26537,#26538,#26539,#26540));
#7110=EDGE_LOOP('',(#26541,#26542,#26543,#26544));
#7111=EDGE_LOOP('',(#26545,#26546,#26547,#26548));
#7112=EDGE_LOOP('',(#26549,#26550,#26551,#26552));
#7113=EDGE_LOOP('',(#26553,#26554,#26555,#26556));
#7114=EDGE_LOOP('',(#26557,#26558,#26559,#26560));
#7115=EDGE_LOOP('',(#26561,#26562,#26563,#26564));
#7116=EDGE_LOOP('',(#26565,#26566,#26567,#26568));
#7117=EDGE_LOOP('',(#26569,#26570,#26571,#26572));
#7118=EDGE_LOOP('',(#26573,#26574,#26575,#26576));
#7119=EDGE_LOOP('',(#26577,#26578,#26579,#26580));
#7120=EDGE_LOOP('',(#26581,#26582,#26583,#26584));
#7121=EDGE_LOOP('',(#26585,#26586,#26587,#26588));
#7122=EDGE_LOOP('',(#26589,#26590,#26591,#26592));
#7123=EDGE_LOOP('',(#26593,#26594,#26595,#26596));
#7124=EDGE_LOOP('',(#26597,#26598,#26599,#26600));
#7125=EDGE_LOOP('',(#26601,#26602,#26603,#26604));
#7126=EDGE_LOOP('',(#26605,#26606,#26607,#26608));
#7127=EDGE_LOOP('',(#26609,#26610,#26611,#26612));
#7128=EDGE_LOOP('',(#26613,#26614,#26615,#26616));
#7129=EDGE_LOOP('',(#26617,#26618,#26619,#26620));
#7130=EDGE_LOOP('',(#26621,#26622,#26623,#26624));
#7131=EDGE_LOOP('',(#26625,#26626,#26627,#26628));
#7132=EDGE_LOOP('',(#26629,#26630,#26631,#26632));
#7133=EDGE_LOOP('',(#26633,#26634,#26635,#26636));
#7134=EDGE_LOOP('',(#26637,#26638,#26639,#26640));
#7135=EDGE_LOOP('',(#26641,#26642,#26643,#26644));
#7136=EDGE_LOOP('',(#26645,#26646,#26647,#26648));
#7137=EDGE_LOOP('',(#26649,#26650,#26651,#26652));
#7138=EDGE_LOOP('',(#26653,#26654,#26655,#26656));
#7139=EDGE_LOOP('',(#26657,#26658,#26659,#26660));
#7140=EDGE_LOOP('',(#26661,#26662,#26663,#26664));
#7141=EDGE_LOOP('',(#26665,#26666,#26667,#26668));
#7142=EDGE_LOOP('',(#26669,#26670,#26671,#26672));
#7143=EDGE_LOOP('',(#26673,#26674,#26675,#26676));
#7144=EDGE_LOOP('',(#26677,#26678,#26679,#26680));
#7145=EDGE_LOOP('',(#26681,#26682,#26683,#26684));
#7146=EDGE_LOOP('',(#26685,#26686,#26687,#26688));
#7147=EDGE_LOOP('',(#26689,#26690,#26691,#26692));
#7148=EDGE_LOOP('',(#26693,#26694,#26695,#26696));
#7149=EDGE_LOOP('',(#26697,#26698,#26699,#26700));
#7150=EDGE_LOOP('',(#26701,#26702,#26703,#26704));
#7151=EDGE_LOOP('',(#26705,#26706,#26707,#26708));
#7152=EDGE_LOOP('',(#26709,#26710,#26711,#26712));
#7153=EDGE_LOOP('',(#26713,#26714,#26715,#26716));
#7154=EDGE_LOOP('',(#26717,#26718,#26719,#26720));
#7155=EDGE_LOOP('',(#26721,#26722,#26723,#26724));
#7156=EDGE_LOOP('',(#26725,#26726,#26727,#26728));
#7157=EDGE_LOOP('',(#26729,#26730,#26731,#26732));
#7158=EDGE_LOOP('',(#26733,#26734,#26735,#26736));
#7159=EDGE_LOOP('',(#26737,#26738,#26739,#26740));
#7160=EDGE_LOOP('',(#26741,#26742,#26743,#26744));
#7161=EDGE_LOOP('',(#26745,#26746,#26747,#26748));
#7162=EDGE_LOOP('',(#26749,#26750,#26751,#26752));
#7163=EDGE_LOOP('',(#26753,#26754,#26755,#26756));
#7164=EDGE_LOOP('',(#26757,#26758,#26759,#26760));
#7165=EDGE_LOOP('',(#26761,#26762,#26763,#26764));
#7166=EDGE_LOOP('',(#26765,#26766,#26767,#26768));
#7167=EDGE_LOOP('',(#26769,#26770,#26771,#26772));
#7168=EDGE_LOOP('',(#26773,#26774,#26775,#26776));
#7169=EDGE_LOOP('',(#26777,#26778,#26779,#26780));
#7170=EDGE_LOOP('',(#26781,#26782,#26783,#26784));
#7171=EDGE_LOOP('',(#26785,#26786,#26787,#26788));
#7172=EDGE_LOOP('',(#26789,#26790,#26791,#26792));
#7173=EDGE_LOOP('',(#26793,#26794,#26795,#26796));
#7174=EDGE_LOOP('',(#26797,#26798,#26799,#26800));
#7175=EDGE_LOOP('',(#26801,#26802,#26803,#26804));
#7176=EDGE_LOOP('',(#26805,#26806,#26807,#26808));
#7177=EDGE_LOOP('',(#26809,#26810,#26811,#26812));
#7178=EDGE_LOOP('',(#26813,#26814,#26815,#26816));
#7179=EDGE_LOOP('',(#26817,#26818,#26819,#26820));
#7180=EDGE_LOOP('',(#26821,#26822,#26823,#26824));
#7181=EDGE_LOOP('',(#26825,#26826,#26827,#26828));
#7182=EDGE_LOOP('',(#26829,#26830,#26831,#26832));
#7183=EDGE_LOOP('',(#26833,#26834,#26835,#26836));
#7184=EDGE_LOOP('',(#26837,#26838,#26839,#26840));
#7185=EDGE_LOOP('',(#26841,#26842,#26843,#26844));
#7186=EDGE_LOOP('',(#26845,#26846,#26847,#26848));
#7187=EDGE_LOOP('',(#26849,#26850,#26851,#26852));
#7188=EDGE_LOOP('',(#26853,#26854,#26855,#26856));
#7189=EDGE_LOOP('',(#26857,#26858,#26859,#26860));
#7190=EDGE_LOOP('',(#26861,#26862,#26863,#26864));
#7191=EDGE_LOOP('',(#26865,#26866,#26867,#26868));
#7192=EDGE_LOOP('',(#26869,#26870,#26871,#26872));
#7193=EDGE_LOOP('',(#26873,#26874,#26875,#26876));
#7194=EDGE_LOOP('',(#26877,#26878,#26879,#26880));
#7195=EDGE_LOOP('',(#26881,#26882,#26883,#26884));
#7196=EDGE_LOOP('',(#26885,#26886,#26887,#26888));
#7197=EDGE_LOOP('',(#26889,#26890,#26891,#26892));
#7198=EDGE_LOOP('',(#26893,#26894,#26895,#26896));
#7199=EDGE_LOOP('',(#26897,#26898,#26899,#26900));
#7200=EDGE_LOOP('',(#26901,#26902,#26903,#26904));
#7201=EDGE_LOOP('',(#26905,#26906,#26907,#26908));
#7202=EDGE_LOOP('',(#26909,#26910,#26911,#26912));
#7203=EDGE_LOOP('',(#26913,#26914,#26915,#26916));
#7204=EDGE_LOOP('',(#26917,#26918,#26919,#26920));
#7205=EDGE_LOOP('',(#26921,#26922,#26923,#26924));
#7206=EDGE_LOOP('',(#26925,#26926,#26927,#26928));
#7207=EDGE_LOOP('',(#26929,#26930,#26931,#26932));
#7208=EDGE_LOOP('',(#26933,#26934,#26935,#26936));
#7209=EDGE_LOOP('',(#26937,#26938,#26939,#26940));
#7210=EDGE_LOOP('',(#26941,#26942,#26943,#26944));
#7211=EDGE_LOOP('',(#26945,#26946,#26947,#26948));
#7212=EDGE_LOOP('',(#26949,#26950,#26951,#26952));
#7213=EDGE_LOOP('',(#26953,#26954,#26955,#26956));
#7214=EDGE_LOOP('',(#26957,#26958,#26959,#26960));
#7215=EDGE_LOOP('',(#26961,#26962,#26963,#26964));
#7216=EDGE_LOOP('',(#26965,#26966,#26967,#26968));
#7217=EDGE_LOOP('',(#26969,#26970,#26971,#26972));
#7218=EDGE_LOOP('',(#26973,#26974,#26975,#26976));
#7219=EDGE_LOOP('',(#26977,#26978,#26979,#26980));
#7220=EDGE_LOOP('',(#26981,#26982,#26983,#26984));
#7221=EDGE_LOOP('',(#26985,#26986,#26987,#26988));
#7222=EDGE_LOOP('',(#26989,#26990,#26991,#26992));
#7223=EDGE_LOOP('',(#26993,#26994,#26995,#26996));
#7224=EDGE_LOOP('',(#26997,#26998,#26999,#27000));
#7225=EDGE_LOOP('',(#27001,#27002,#27003,#27004));
#7226=EDGE_LOOP('',(#27005,#27006,#27007,#27008));
#7227=EDGE_LOOP('',(#27009,#27010,#27011,#27012));
#7228=EDGE_LOOP('',(#27013,#27014,#27015,#27016));
#7229=EDGE_LOOP('',(#27017,#27018,#27019,#27020));
#7230=EDGE_LOOP('',(#27021,#27022,#27023,#27024));
#7231=EDGE_LOOP('',(#27025,#27026,#27027,#27028));
#7232=EDGE_LOOP('',(#27029,#27030,#27031,#27032));
#7233=EDGE_LOOP('',(#27033,#27034,#27035,#27036));
#7234=EDGE_LOOP('',(#27037,#27038,#27039,#27040));
#7235=EDGE_LOOP('',(#27041,#27042,#27043,#27044));
#7236=EDGE_LOOP('',(#27045,#27046,#27047,#27048));
#7237=EDGE_LOOP('',(#27049,#27050,#27051,#27052));
#7238=EDGE_LOOP('',(#27053,#27054,#27055,#27056,#27057));
#7239=EDGE_LOOP('',(#27058,#27059,#27060,#27061,#27062,#27063,#27064,#27065,
#27066,#27067,#27068,#27069,#27070,#27071,#27072,#27073,#27074,#27075,#27076,
#27077,#27078,#27079,#27080,#27081,#27082,#27083,#27084,#27085,#27086,#27087,
#27088,#27089,#27090,#27091,#27092,#27093,#27094,#27095,#27096,#27097,#27098,
#27099,#27100,#27101,#27102,#27103,#27104,#27105,#27106,#27107,#27108,#27109,
#27110,#27111,#27112,#27113,#27114,#27115,#27116,#27117,#27118,#27119,#27120,
#27121,#27122,#27123,#27124,#27125,#27126,#27127,#27128,#27129,#27130,#27131,
#27132,#27133,#27134,#27135,#27136,#27137,#27138,#27139,#27140,#27141,#27142,
#27143,#27144,#27145,#27146,#27147,#27148,#27149,#27150,#27151,#27152,#27153,
#27154,#27155,#27156,#27157,#27158,#27159,#27160,#27161,#27162,#27163,#27164,
#27165,#27166,#27167,#27168,#27169,#27170,#27171,#27172,#27173,#27174,#27175,
#27176,#27177,#27178,#27179,#27180,#27181,#27182,#27183,#27184,#27185,#27186,
#27187,#27188,#27189,#27190,#27191,#27192,#27193,#27194,#27195,#27196,#27197,
#27198,#27199,#27200,#27201,#27202,#27203,#27204,#27205,#27206,#27207,#27208,
#27209,#27210,#27211));
#7240=EDGE_LOOP('',(#27212,#27213,#27214,#27215,#27216));
#7241=EDGE_LOOP('',(#27217,#27218,#27219,#27220));
#7242=EDGE_LOOP('',(#27221,#27222,#27223,#27224,#27225,#27226,#27227,#27228,
#27229,#27230,#27231,#27232,#27233,#27234,#27235,#27236,#27237,#27238,#27239,
#27240,#27241,#27242,#27243,#27244,#27245,#27246,#27247,#27248,#27249,#27250,
#27251,#27252,#27253,#27254,#27255,#27256,#27257,#27258,#27259,#27260,#27261,
#27262,#27263,#27264,#27265,#27266,#27267,#27268,#27269,#27270,#27271,#27272,
#27273,#27274,#27275,#27276,#27277,#27278,#27279,#27280,#27281,#27282,#27283,
#27284,#27285,#27286,#27287,#27288,#27289,#27290,#27291,#27292,#27293,#27294,
#27295,#27296,#27297,#27298,#27299,#27300,#27301,#27302,#27303,#27304,#27305,
#27306,#27307,#27308,#27309,#27310,#27311,#27312,#27313,#27314,#27315,#27316,
#27317,#27318,#27319,#27320,#27321,#27322,#27323,#27324,#27325,#27326,#27327,
#27328,#27329,#27330,#27331,#27332,#27333,#27334,#27335,#27336,#27337,#27338,
#27339,#27340,#27341,#27342,#27343,#27344,#27345,#27346,#27347,#27348,#27349,
#27350,#27351,#27352,#27353,#27354,#27355,#27356,#27357,#27358,#27359,#27360,
#27361,#27362,#27363,#27364,#27365,#27366,#27367,#27368,#27369,#27370,#27371,
#27372,#27373,#27374));
#7243=EDGE_LOOP('',(#27375,#27376,#27377,#27378));
#7244=EDGE_LOOP('',(#27379,#27380,#27381,#27382,#27383,#27384));
#7245=EDGE_LOOP('',(#27385,#27386,#27387,#27388));
#7246=EDGE_LOOP('',(#27389,#27390,#27391,#27392,#27393,#27394));
#7247=EDGE_LOOP('',(#27395));
#7248=EDGE_LOOP('',(#27396,#27397));
#7249=EDGE_LOOP('',(#27398));
#7250=EDGE_LOOP('',(#27399,#27400,#27401,#27402,#27403));
#7251=EDGE_LOOP('',(#27404,#27405,#27406,#27407,#27408));
#7252=EDGE_LOOP('',(#27409));
#7253=EDGE_LOOP('',(#27410));
#7254=EDGE_LOOP('',(#27411,#27412,#27413,#27414));
#7255=EDGE_LOOP('',(#27415,#27416,#27417,#27418,#27419,#27420));
#7256=EDGE_LOOP('',(#27421,#27422,#27423,#27424));
#7257=EDGE_LOOP('',(#27425,#27426,#27427,#27428,#27429,#27430));
#7258=EDGE_LOOP('',(#27431,#27432,#27433,#27434,#27435,#27436,#27437,#27438,
#27439,#27440,#27441,#27442,#27443,#27444,#27445,#27446,#27447,#27448,#27449,
#27450,#27451,#27452,#27453,#27454,#27455,#27456,#27457,#27458,#27459,#27460,
#27461,#27462,#27463,#27464,#27465,#27466,#27467,#27468,#27469,#27470,#27471,
#27472,#27473,#27474,#27475,#27476,#27477,#27478,#27479,#27480,#27481,#27482,
#27483,#27484,#27485,#27486,#27487,#27488,#27489,#27490,#27491,#27492,#27493,
#27494));
#7259=EDGE_LOOP('',(#27495,#27496,#27497,#27498));
#7260=EDGE_LOOP('',(#27499,#27500,#27501,#27502,#27503,#27504));
#7261=EDGE_LOOP('',(#27505,#27506,#27507,#27508));
#7262=EDGE_LOOP('',(#27509,#27510,#27511,#27512,#27513,#27514));
#7263=EDGE_LOOP('',(#27515,#27516,#27517,#27518));
#7264=EDGE_LOOP('',(#27519,#27520,#27521,#27522,#27523,#27524));
#7265=EDGE_LOOP('',(#27525,#27526,#27527,#27528));
#7266=EDGE_LOOP('',(#27529,#27530,#27531,#27532,#27533,#27534));
#7267=EDGE_LOOP('',(#27535,#27536,#27537,#27538));
#7268=EDGE_LOOP('',(#27539,#27540,#27541,#27542,#27543,#27544));
#7269=EDGE_LOOP('',(#27545,#27546,#27547,#27548));
#7270=EDGE_LOOP('',(#27549,#27550,#27551,#27552,#27553,#27554));
#7271=EDGE_LOOP('',(#27555,#27556,#27557,#27558));
#7272=EDGE_LOOP('',(#27559,#27560,#27561,#27562,#27563,#27564));
#7273=EDGE_LOOP('',(#27565,#27566,#27567,#27568));
#7274=EDGE_LOOP('',(#27569,#27570,#27571,#27572,#27573,#27574));
#7275=EDGE_LOOP('',(#27575,#27576,#27577,#27578));
#7276=EDGE_LOOP('',(#27579,#27580,#27581,#27582,#27583,#27584));
#7277=EDGE_LOOP('',(#27585,#27586,#27587,#27588));
#7278=EDGE_LOOP('',(#27589,#27590,#27591,#27592,#27593,#27594));
#7279=EDGE_LOOP('',(#27595,#27596,#27597,#27598));
#7280=EDGE_LOOP('',(#27599,#27600,#27601,#27602,#27603,#27604));
#7281=EDGE_LOOP('',(#27605,#27606,#27607,#27608));
#7282=EDGE_LOOP('',(#27609,#27610,#27611,#27612,#27613,#27614));
#7283=EDGE_LOOP('',(#27615,#27616,#27617,#27618));
#7284=EDGE_LOOP('',(#27619,#27620,#27621,#27622,#27623,#27624));
#7285=EDGE_LOOP('',(#27625,#27626,#27627,#27628));
#7286=EDGE_LOOP('',(#27629,#27630,#27631,#27632,#27633,#27634,#27635));
#7287=EDGE_LOOP('',(#27636,#27637,#27638,#27639));
#7288=EDGE_LOOP('',(#27640,#27641,#27642,#27643,#27644,#27645));
#7289=EDGE_LOOP('',(#27646,#27647,#27648,#27649));
#7290=EDGE_LOOP('',(#27650,#27651,#27652,#27653,#27654,#27655));
#7291=EDGE_LOOP('',(#27656,#27657,#27658,#27659));
#7292=EDGE_LOOP('',(#27660,#27661,#27662,#27663,#27664,#27665));
#7293=EDGE_LOOP('',(#27666,#27667,#27668,#27669));
#7294=EDGE_LOOP('',(#27670,#27671,#27672,#27673,#27674,#27675));
#7295=EDGE_LOOP('',(#27676,#27677,#27678,#27679));
#7296=EDGE_LOOP('',(#27680,#27681,#27682,#27683,#27684,#27685));
#7297=EDGE_LOOP('',(#27686,#27687,#27688,#27689));
#7298=EDGE_LOOP('',(#27690,#27691,#27692,#27693,#27694,#27695));
#7299=EDGE_LOOP('',(#27696,#27697,#27698,#27699));
#7300=EDGE_LOOP('',(#27700,#27701,#27702,#27703,#27704,#27705));
#7301=EDGE_LOOP('',(#27706,#27707,#27708,#27709));
#7302=EDGE_LOOP('',(#27710,#27711,#27712,#27713,#27714,#27715));
#7303=EDGE_LOOP('',(#27716,#27717,#27718,#27719));
#7304=EDGE_LOOP('',(#27720,#27721,#27722,#27723,#27724,#27725));
#7305=EDGE_LOOP('',(#27726,#27727,#27728,#27729));
#7306=EDGE_LOOP('',(#27730,#27731,#27732,#27733,#27734,#27735));
#7307=EDGE_LOOP('',(#27736,#27737,#27738,#27739));
#7308=EDGE_LOOP('',(#27740,#27741,#27742,#27743,#27744,#27745));
#7309=EDGE_LOOP('',(#27746,#27747,#27748,#27749));
#7310=EDGE_LOOP('',(#27750,#27751,#27752,#27753,#27754,#27755));
#7311=EDGE_LOOP('',(#27756,#27757,#27758,#27759));
#7312=EDGE_LOOP('',(#27760,#27761,#27762,#27763,#27764,#27765));
#7313=EDGE_LOOP('',(#27766,#27767,#27768,#27769));
#7314=EDGE_LOOP('',(#27770,#27771,#27772,#27773));
#7315=EDGE_LOOP('',(#27774,#27775,#27776,#27777));
#7316=EDGE_LOOP('',(#27778,#27779,#27780,#27781));
#7317=EDGE_LOOP('',(#27782,#27783,#27784,#27785));
#7318=EDGE_LOOP('',(#27786,#27787,#27788,#27789));
#7319=EDGE_LOOP('',(#27790,#27791,#27792,#27793));
#7320=EDGE_LOOP('',(#27794,#27795,#27796,#27797));
#7321=EDGE_LOOP('',(#27798,#27799,#27800,#27801));
#7322=EDGE_LOOP('',(#27802,#27803,#27804,#27805));
#7323=EDGE_LOOP('',(#27806,#27807,#27808,#27809,#27810,#27811,#27812,#27813,
#27814,#27815,#27816,#27817,#27818,#27819,#27820,#27821,#27822,#27823,#27824,
#27825,#27826,#27827,#27828,#27829,#27830,#27831,#27832,#27833,#27834,#27835));
#7324=EDGE_LOOP('',(#27836,#27837,#27838,#27839,#27840,#27841));
#7325=EDGE_LOOP('',(#27842,#27843,#27844,#27845));
#7326=EDGE_LOOP('',(#27846,#27847,#27848,#27849));
#7327=EDGE_LOOP('',(#27850,#27851,#27852,#27853));
#7328=EDGE_LOOP('',(#27854,#27855,#27856,#27857,#27858,#27859));
#7329=EDGE_LOOP('',(#27860,#27861,#27862,#27863));
#7330=EDGE_LOOP('',(#27864,#27865,#27866,#27867));
#7331=EDGE_LOOP('',(#27868,#27869,#27870,#27871));
#7332=EDGE_LOOP('',(#27872,#27873,#27874,#27875));
#7333=EDGE_LOOP('',(#27876,#27877,#27878,#27879));
#7334=EDGE_LOOP('',(#27880,#27881,#27882,#27883));
#7335=EDGE_LOOP('',(#27884,#27885,#27886,#27887));
#7336=EDGE_LOOP('',(#27888,#27889,#27890,#27891));
#7337=EDGE_LOOP('',(#27892,#27893,#27894,#27895));
#7338=EDGE_LOOP('',(#27896,#27897,#27898,#27899));
#7339=EDGE_LOOP('',(#27900,#27901,#27902,#27903));
#7340=EDGE_LOOP('',(#27904,#27905,#27906,#27907));
#7341=EDGE_LOOP('',(#27908,#27909,#27910,#27911));
#7342=EDGE_LOOP('',(#27912,#27913,#27914,#27915));
#7343=EDGE_LOOP('',(#27916,#27917,#27918,#27919));
#7344=EDGE_LOOP('',(#27920,#27921,#27922,#27923,#27924,#27925));
#7345=EDGE_LOOP('',(#27926,#27927,#27928,#27929));
#7346=EDGE_LOOP('',(#27930,#27931,#27932,#27933));
#7347=EDGE_LOOP('',(#27934));
#7348=EDGE_LOOP('',(#27935));
#7349=EDGE_LOOP('',(#27936,#27937,#27938,#27939));
#7350=EDGE_LOOP('',(#27940));
#7351=EDGE_LOOP('',(#27941,#27942,#27943,#27944));
#7352=EDGE_LOOP('',(#27945,#27946,#27947,#27948));
#7353=EDGE_LOOP('',(#27949,#27950,#27951,#27952));
#7354=EDGE_LOOP('',(#27953,#27954,#27955,#27956));
#7355=EDGE_LOOP('',(#27957,#27958,#27959,#27960));
#7356=EDGE_LOOP('',(#27961,#27962,#27963,#27964));
#7357=EDGE_LOOP('',(#27965,#27966,#27967,#27968));
#7358=EDGE_LOOP('',(#27969,#27970,#27971,#27972));
#7359=EDGE_LOOP('',(#27973,#27974,#27975,#27976));
#7360=EDGE_LOOP('',(#27977,#27978,#27979,#27980));
#7361=EDGE_LOOP('',(#27981,#27982,#27983,#27984));
#7362=EDGE_LOOP('',(#27985,#27986,#27987,#27988));
#7363=EDGE_LOOP('',(#27989,#27990,#27991,#27992));
#7364=EDGE_LOOP('',(#27993,#27994,#27995,#27996,#27997));
#7365=EDGE_LOOP('',(#27998,#27999,#28000,#28001,#28002,#28003,#28004,#28005,
#28006,#28007,#28008,#28009,#28010,#28011,#28012,#28013,#28014));
#7366=EDGE_LOOP('',(#28015,#28016,#28017,#28018,#28019));
#7367=EDGE_LOOP('',(#28020,#28021,#28022,#28023));
#7368=EDGE_LOOP('',(#28024,#28025,#28026,#28027,#28028,#28029,#28030,#28031,
#28032,#28033,#28034,#28035,#28036,#28037,#28038,#28039,#28040));
#7369=EDGE_LOOP('',(#28041,#28042,#28043,#28044));
#7370=EDGE_LOOP('',(#28045,#28046,#28047,#28048));
#7371=EDGE_LOOP('',(#28049,#28050,#28051,#28052));
#7372=EDGE_LOOP('',(#28053,#28054,#28055,#28056));
#7373=EDGE_LOOP('',(#28057,#28058,#28059,#28060));
#7374=EDGE_LOOP('',(#28061,#28062,#28063,#28064));
#7375=EDGE_LOOP('',(#28065,#28066,#28067,#28068,#28069,#28070));
#7376=EDGE_LOOP('',(#28071));
#7377=EDGE_LOOP('',(#28072,#28073,#28074,#28075,#28076,#28077));
#7378=EDGE_LOOP('',(#28078,#28079,#28080,#28081));
#7379=EDGE_LOOP('',(#28082,#28083,#28084,#28085,#28086,#28087));
#7380=EDGE_LOOP('',(#28088));
#7381=EDGE_LOOP('',(#28089,#28090,#28091,#28092,#28093,#28094));
#7382=LINE('',#40770,#9688);
#7383=LINE('',#40772,#9689);
#7384=LINE('',#40774,#9690);
#7385=LINE('',#40776,#9691);
#7386=LINE('',#40778,#9692);
#7387=LINE('',#40779,#9693);
#7388=LINE('',#40782,#9694);
#7389=LINE('',#40784,#9695);
#7390=LINE('',#40785,#9696);
#7391=LINE('',#40788,#9697);
#7392=LINE('',#40790,#9698);
#7393=LINE('',#40792,#9699);
#7394=LINE('',#40793,#9700);
#7395=LINE('',#40796,#9701);
#7396=LINE('',#40798,#9702);
#7397=LINE('',#40799,#9703);
#7398=LINE('',#40802,#9704);
#7399=LINE('',#40804,#9705);
#7400=LINE('',#40806,#9706);
#7401=LINE('',#40807,#9707);
#7402=LINE('',#40810,#9708);
#7403=LINE('',#40812,#9709);
#7404=LINE('',#40813,#9710);
#7405=LINE('',#40816,#9711);
#7406=LINE('',#40818,#9712);
#7407=LINE('',#40820,#9713);
#7408=LINE('',#40821,#9714);
#7409=LINE('',#40824,#9715);
#7410=LINE('',#40825,#9716);
#7411=LINE('',#40828,#9717);
#7412=LINE('',#40830,#9718);
#7413=LINE('',#40832,#9719);
#7414=LINE('',#40834,#9720);
#7415=LINE('',#40836,#9721);
#7416=LINE('',#40838,#9722);
#7417=LINE('',#40840,#9723);
#7418=LINE('',#40842,#9724);
#7419=LINE('',#40844,#9725);
#7420=LINE('',#40846,#9726);
#7421=LINE('',#40848,#9727);
#7422=LINE('',#40849,#9728);
#7423=LINE('',#40852,#9729);
#7424=LINE('',#40854,#9730);
#7425=LINE('',#40856,#9731);
#7426=LINE('',#40858,#9732);
#7427=LINE('',#40860,#9733);
#7428=LINE('',#40890,#9734);
#7429=LINE('',#40892,#9735);
#7430=LINE('',#40894,#9736);
#7431=LINE('',#40912,#9737);
#7432=LINE('',#40914,#9738);
#7433=LINE('',#40916,#9739);
#7434=LINE('',#40918,#9740);
#7435=LINE('',#40920,#9741);
#7436=LINE('',#40922,#9742);
#7437=LINE('',#40924,#9743);
#7438=LINE('',#40926,#9744);
#7439=LINE('',#40928,#9745);
#7440=LINE('',#40930,#9746);
#7441=LINE('',#40932,#9747);
#7442=LINE('',#40933,#9748);
#7443=LINE('',#40944,#9749);
#7444=LINE('',#40946,#9750);
#7445=LINE('',#40948,#9751);
#7446=LINE('',#40950,#9752);
#7447=LINE('',#40964,#9753);
#7448=LINE('',#40982,#9754);
#7449=LINE('',#41056,#9755);
#7450=LINE('',#41118,#9756);
#7451=LINE('',#41148,#9757);
#7452=LINE('',#41178,#9758);
#7453=LINE('',#41220,#9759);
#7454=LINE('',#41222,#9760);
#7455=LINE('',#41224,#9761);
#7456=LINE('',#41225,#9762);
#7457=LINE('',#41240,#9763);
#7458=LINE('',#41314,#9764);
#7459=LINE('',#41365,#9765);
#7460=LINE('',#41367,#9766);
#7461=LINE('',#41368,#9767);
#7462=LINE('',#41369,#9768);
#7463=LINE('',#41372,#9769);
#7464=LINE('',#41374,#9770);
#7465=LINE('',#41375,#9771);
#7466=LINE('',#41380,#9772);
#7467=LINE('',#41385,#9773);
#7468=LINE('',#41387,#9774);
#7469=LINE('',#41388,#9775);
#7470=LINE('',#41389,#9776);
#7471=LINE('',#41394,#9777);
#7472=LINE('',#41398,#9778);
#7473=LINE('',#41402,#9779);
#7474=LINE('',#41408,#9780);
#7475=LINE('',#41412,#9781);
#7476=LINE('',#41421,#9782);
#7477=LINE('',#41425,#9783);
#7478=LINE('',#41434,#9784);
#7479=LINE('',#41438,#9785);
#7480=LINE('',#41447,#9786);
#7481=LINE('',#41451,#9787);
#7482=LINE('',#41458,#9788);
#7483=LINE('',#41459,#9789);
#7484=LINE('',#41462,#9790);
#7485=LINE('',#41463,#9791);
#7486=LINE('',#41464,#9792);
#7487=LINE('',#41467,#9793);
#7488=LINE('',#41468,#9794);
#7489=LINE('',#41472,#9795);
#7490=LINE('',#41473,#9796);
#7491=LINE('',#41474,#9797);
#7492=LINE('',#41478,#9798);
#7493=LINE('',#41480,#9799);
#7494=LINE('',#41481,#9800);
#7495=LINE('',#41484,#9801);
#7496=LINE('',#41486,#9802);
#7497=LINE('',#41487,#9803);
#7498=LINE('',#41489,#9804);
#7499=LINE('',#41490,#9805);
#7500=LINE('',#41492,#9806);
#7501=LINE('',#41494,#9807);
#7502=LINE('',#41496,#9808);
#7503=LINE('',#41497,#9809);
#7504=LINE('',#41499,#9810);
#7505=LINE('',#41500,#9811);
#7506=LINE('',#41502,#9812);
#7507=LINE('',#41504,#9813);
#7508=LINE('',#41505,#9814);
#7509=LINE('',#41556,#9815);
#7510=LINE('',#41558,#9816);
#7511=LINE('',#41559,#9817);
#7512=LINE('',#41562,#9818);
#7513=LINE('',#41563,#9819);
#7514=LINE('',#41566,#9820);
#7515=LINE('',#41567,#9821);
#7516=LINE('',#41570,#9822);
#7517=LINE('',#41571,#9823);
#7518=LINE('',#41574,#9824);
#7519=LINE('',#41575,#9825);
#7520=LINE('',#41578,#9826);
#7521=LINE('',#41579,#9827);
#7522=LINE('',#41582,#9828);
#7523=LINE('',#41583,#9829);
#7524=LINE('',#41586,#9830);
#7525=LINE('',#41587,#9831);
#7526=LINE('',#41590,#9832);
#7527=LINE('',#41591,#9833);
#7528=LINE('',#41594,#9834);
#7529=LINE('',#41595,#9835);
#7530=LINE('',#41598,#9836);
#7531=LINE('',#41599,#9837);
#7532=LINE('',#41601,#9838);
#7533=LINE('',#41605,#9839);
#7534=LINE('',#41607,#9840);
#7535=LINE('',#41608,#9841);
#7536=LINE('',#41616,#9842);
#7537=LINE('',#41627,#9843);
#7538=LINE('',#41638,#9844);
#7539=LINE('',#41649,#9845);
#7540=LINE('',#41655,#9846);
#7541=LINE('',#41656,#9847);
#7542=LINE('',#41659,#9848);
#7543=LINE('',#41660,#9849);
#7544=LINE('',#41663,#9850);
#7545=LINE('',#41664,#9851);
#7546=LINE('',#41672,#9852);
#7547=LINE('',#41683,#9853);
#7548=LINE('',#41694,#9854);
#7549=LINE('',#41705,#9855);
#7550=LINE('',#41716,#9856);
#7551=LINE('',#41727,#9857);
#7552=LINE('',#41738,#9858);
#7553=LINE('',#41744,#9859);
#7554=LINE('',#41745,#9860);
#7555=LINE('',#41748,#9861);
#7556=LINE('',#41749,#9862);
#7557=LINE('',#41752,#9863);
#7558=LINE('',#41753,#9864);
#7559=LINE('',#41755,#9865);
#7560=LINE('',#41759,#9866);
#7561=LINE('',#41761,#9867);
#7562=LINE('',#41762,#9868);
#7563=LINE('',#41765,#9869);
#7564=LINE('',#41766,#9870);
#7565=LINE('',#41769,#9871);
#7566=LINE('',#41770,#9872);
#7567=LINE('',#41773,#9873);
#7568=LINE('',#41774,#9874);
#7569=LINE('',#41777,#9875);
#7570=LINE('',#41778,#9876);
#7571=LINE('',#41781,#9877);
#7572=LINE('',#41782,#9878);
#7573=LINE('',#41785,#9879);
#7574=LINE('',#41786,#9880);
#7575=LINE('',#41789,#9881);
#7576=LINE('',#41790,#9882);
#7577=LINE('',#41793,#9883);
#7578=LINE('',#41794,#9884);
#7579=LINE('',#41797,#9885);
#7580=LINE('',#41798,#9886);
#7581=LINE('',#41801,#9887);
#7582=LINE('',#41802,#9888);
#7583=LINE('',#41804,#9889);
#7584=LINE('',#41813,#9890);
#7585=LINE('',#41818,#9891);
#7586=LINE('',#41826,#9892);
#7587=LINE('',#41832,#9893);
#7588=LINE('',#41833,#9894);
#7589=LINE('',#41841,#9895);
#7590=LINE('',#41852,#9896);
#7591=LINE('',#41863,#9897);
#7592=LINE('',#41869,#9898);
#7593=LINE('',#41870,#9899);
#7594=LINE('',#41873,#9900);
#7595=LINE('',#41874,#9901);
#7596=LINE('',#41877,#9902);
#7597=LINE('',#41878,#9903);
#7598=LINE('',#41881,#9904);
#7599=LINE('',#41882,#9905);
#7600=LINE('',#41900,#9906);
#7601=LINE('',#41905,#9907);
#7602=LINE('',#41913,#9908);
#7603=LINE('',#41924,#9909);
#7604=LINE('',#41935,#9910);
#7605=LINE('',#41946,#9911);
#7606=LINE('',#41957,#9912);
#7607=LINE('',#41968,#9913);
#7608=LINE('',#41979,#9914);
#7609=LINE('',#41990,#9915);
#7610=LINE('',#42001,#9916);
#7611=LINE('',#42012,#9917);
#7612=LINE('',#42023,#9918);
#7613=LINE('',#42034,#9919);
#7614=LINE('',#42040,#9920);
#7615=LINE('',#42041,#9921);
#7616=LINE('',#42049,#9922);
#7617=LINE('',#42060,#9923);
#7618=LINE('',#42071,#9924);
#7619=LINE('',#42082,#9925);
#7620=LINE('',#42093,#9926);
#7621=LINE('',#42104,#9927);
#7622=LINE('',#42115,#9928);
#7623=LINE('',#42126,#9929);
#7624=LINE('',#42137,#9930);
#7625=LINE('',#42148,#9931);
#7626=LINE('',#42159,#9932);
#7627=LINE('',#42170,#9933);
#7628=LINE('',#42181,#9934);
#7629=LINE('',#42192,#9935);
#7630=LINE('',#42203,#9936);
#7631=LINE('',#42214,#9937);
#7632=LINE('',#42225,#9938);
#7633=LINE('',#42236,#9939);
#7634=LINE('',#42242,#9940);
#7635=LINE('',#42243,#9941);
#7636=LINE('',#42251,#9942);
#7637=LINE('',#42272,#9943);
#7638=LINE('',#42277,#9944);
#7639=LINE('',#42285,#9945);
#7640=LINE('',#42296,#9946);
#7641=LINE('',#42307,#9947);
#7642=LINE('',#42318,#9948);
#7643=LINE('',#42329,#9949);
#7644=LINE('',#42340,#9950);
#7645=LINE('',#42351,#9951);
#7646=LINE('',#42362,#9952);
#7647=LINE('',#42373,#9953);
#7648=LINE('',#42384,#9954);
#7649=LINE('',#42390,#9955);
#7650=LINE('',#42391,#9956);
#7651=LINE('',#42399,#9957);
#7652=LINE('',#42410,#9958);
#7653=LINE('',#42421,#9959);
#7654=LINE('',#42432,#9960);
#7655=LINE('',#42443,#9961);
#7656=LINE('',#42454,#9962);
#7657=LINE('',#42465,#9963);
#7658=LINE('',#42471,#9964);
#7659=LINE('',#42472,#9965);
#7660=LINE('',#42480,#9966);
#7661=LINE('',#42491,#9967);
#7662=LINE('',#42502,#9968);
#7663=LINE('',#42513,#9969);
#7664=LINE('',#42524,#9970);
#7665=LINE('',#42535,#9971);
#7666=LINE('',#42546,#9972);
#7667=LINE('',#42552,#9973);
#7668=LINE('',#42553,#9974);
#7669=LINE('',#42561,#9975);
#7670=LINE('',#42577,#9976);
#7671=LINE('',#42579,#9977);
#7672=LINE('',#42580,#9978);
#7673=LINE('',#42583,#9979);
#7674=LINE('',#42584,#9980);
#7675=LINE('',#42587,#9981);
#7676=LINE('',#42588,#9982);
#7677=LINE('',#42590,#9983);
#7678=LINE('',#42599,#9984);
#7679=LINE('',#42604,#9985);
#7680=LINE('',#42612,#9986);
#7681=LINE('',#42623,#9987);
#7682=LINE('',#42634,#9988);
#7683=LINE('',#42645,#9989);
#7684=LINE('',#42656,#9990);
#7685=LINE('',#42667,#9991);
#7686=LINE('',#42678,#9992);
#7687=LINE('',#42689,#9993);
#7688=LINE('',#42700,#9994);
#7689=LINE('',#42711,#9995);
#7690=LINE('',#42722,#9996);
#7691=LINE('',#42733,#9997);
#7692=LINE('',#42739,#9998);
#7693=LINE('',#42740,#9999);
#7694=LINE('',#42748,#10000);
#7695=LINE('',#42759,#10001);
#7696=LINE('',#42770,#10002);
#7697=LINE('',#42781,#10003);
#7698=LINE('',#42792,#10004);
#7699=LINE('',#42803,#10005);
#7700=LINE('',#42814,#10006);
#7701=LINE('',#42825,#10007);
#7702=LINE('',#42836,#10008);
#7703=LINE('',#42847,#10009);
#7704=LINE('',#42858,#10010);
#7705=LINE('',#42869,#10011);
#7706=LINE('',#42880,#10012);
#7707=LINE('',#42891,#10013);
#7708=LINE('',#42902,#10014);
#7709=LINE('',#42913,#10015);
#7710=LINE('',#42924,#10016);
#7711=LINE('',#42935,#10017);
#7712=LINE('',#42941,#10018);
#7713=LINE('',#42942,#10019);
#7714=LINE('',#42950,#10020);
#7715=LINE('',#42966,#10021);
#7716=LINE('',#42971,#10022);
#7717=LINE('',#42974,#10023);
#7718=LINE('',#42978,#10024);
#7719=LINE('',#42982,#10025);
#7720=LINE('',#42986,#10026);
#7721=LINE('',#42990,#10027);
#7722=LINE('',#42994,#10028);
#7723=LINE('',#42998,#10029);
#7724=LINE('',#43002,#10030);
#7725=LINE('',#43006,#10031);
#7726=LINE('',#43010,#10032);
#7727=LINE('',#43014,#10033);
#7728=LINE('',#43018,#10034);
#7729=LINE('',#43022,#10035);
#7730=LINE('',#43026,#10036);
#7731=LINE('',#43030,#10037);
#7732=LINE('',#43034,#10038);
#7733=LINE('',#43038,#10039);
#7734=LINE('',#43042,#10040);
#7735=LINE('',#43046,#10041);
#7736=LINE('',#43050,#10042);
#7737=LINE('',#43054,#10043);
#7738=LINE('',#43058,#10044);
#7739=LINE('',#43062,#10045);
#7740=LINE('',#43066,#10046);
#7741=LINE('',#43070,#10047);
#7742=LINE('',#43073,#10048);
#7743=LINE('',#43076,#10049);
#7744=LINE('',#43079,#10050);
#7745=LINE('',#43082,#10051);
#7746=LINE('',#43085,#10052);
#7747=LINE('',#43088,#10053);
#7748=LINE('',#43091,#10054);
#7749=LINE('',#43093,#10055);
#7750=LINE('',#43095,#10056);
#7751=LINE('',#43097,#10057);
#7752=LINE('',#43099,#10058);
#7753=LINE('',#43116,#10059);
#7754=LINE('',#43125,#10060);
#7755=LINE('',#43130,#10061);
#7756=LINE('',#43132,#10062);
#7757=LINE('',#43136,#10063);
#7758=LINE('',#43140,#10064);
#7759=LINE('',#43144,#10065);
#7760=LINE('',#43148,#10066);
#7761=LINE('',#43152,#10067);
#7762=LINE('',#43156,#10068);
#7763=LINE('',#43160,#10069);
#7764=LINE('',#43164,#10070);
#7765=LINE('',#43168,#10071);
#7766=LINE('',#43172,#10072);
#7767=LINE('',#43176,#10073);
#7768=LINE('',#43198,#10074);
#7769=LINE('',#43202,#10075);
#7770=LINE('',#43206,#10076);
#7771=LINE('',#43210,#10077);
#7772=LINE('',#43212,#10078);
#7773=LINE('',#43213,#10079);
#7774=LINE('',#43217,#10080);
#7775=LINE('',#43220,#10081);
#7776=LINE('',#43221,#10082);
#7777=LINE('',#43225,#10083);
#7778=LINE('',#43232,#10084);
#7779=LINE('',#43233,#10085);
#7780=LINE('',#43251,#10086);
#7781=LINE('',#43253,#10087);
#7782=LINE('',#43254,#10088);
#7783=LINE('',#43260,#10089);
#7784=LINE('',#43264,#10090);
#7785=LINE('',#43266,#10091);
#7786=LINE('',#43268,#10092);
#7787=LINE('',#43269,#10093);
#7788=LINE('',#43273,#10094);
#7789=LINE('',#43279,#10095);
#7790=LINE('',#43280,#10096);
#7791=LINE('',#43281,#10097);
#7792=LINE('',#43285,#10098);
#7793=LINE('',#43289,#10099);
#7794=LINE('',#43290,#10100);
#7795=LINE('',#43304,#10101);
#7796=LINE('',#43305,#10102);
#7797=LINE('',#43307,#10103);
#7798=LINE('',#43310,#10104);
#7799=LINE('',#43313,#10105);
#7800=LINE('',#43315,#10106);
#7801=LINE('',#43316,#10107);
#7802=LINE('',#43319,#10108);
#7803=LINE('',#43321,#10109);
#7804=LINE('',#43322,#10110);
#7805=LINE('',#43327,#10111);
#7806=LINE('',#43331,#10112);
#7807=LINE('',#43335,#10113);
#7808=LINE('',#43339,#10114);
#7809=LINE('',#43343,#10115);
#7810=LINE('',#43347,#10116);
#7811=LINE('',#43351,#10117);
#7812=LINE('',#43355,#10118);
#7813=LINE('',#43366,#10119);
#7814=LINE('',#43369,#10120);
#7815=LINE('',#43374,#10121);
#7816=LINE('',#43377,#10122);
#7817=LINE('',#43382,#10123);
#7818=LINE('',#43385,#10124);
#7819=LINE('',#43389,#10125);
#7820=LINE('',#43390,#10126);
#7821=LINE('',#43393,#10127);
#7822=LINE('',#43397,#10128);
#7823=LINE('',#43398,#10129);
#7824=LINE('',#43401,#10130);
#7825=LINE('',#43405,#10131);
#7826=LINE('',#43406,#10132);
#7827=LINE('',#43409,#10133);
#7828=LINE('',#43413,#10134);
#7829=LINE('',#43414,#10135);
#7830=LINE('',#43417,#10136);
#7831=LINE('',#43421,#10137);
#7832=LINE('',#43422,#10138);
#7833=LINE('',#43431,#10139);
#7834=LINE('',#43432,#10140);
#7835=LINE('',#43436,#10141);
#7836=LINE('',#43438,#10142);
#7837=LINE('',#43440,#10143);
#7838=LINE('',#43441,#10144);
#7839=LINE('',#43445,#10145);
#7840=LINE('',#43451,#10146);
#7841=LINE('',#43452,#10147);
#7842=LINE('',#43453,#10148);
#7843=LINE('',#43457,#10149);
#7844=LINE('',#43463,#10150);
#7845=LINE('',#43464,#10151);
#7846=LINE('',#43465,#10152);
#7847=LINE('',#43469,#10153);
#7848=LINE('',#43475,#10154);
#7849=LINE('',#43476,#10155);
#7850=LINE('',#43477,#10156);
#7851=LINE('',#43483,#10157);
#7852=LINE('',#43486,#10158);
#7853=LINE('',#43489,#10159);
#7854=LINE('',#43490,#10160);
#7855=LINE('',#43493,#10161);
#7856=LINE('',#43506,#10162);
#7857=LINE('',#43509,#10163);
#7858=LINE('',#43510,#10164);
#7859=LINE('',#43511,#10165);
#7860=LINE('',#43521,#10166);
#7861=LINE('',#43524,#10167);
#7862=LINE('',#43525,#10168);
#7863=LINE('',#43529,#10169);
#7864=LINE('',#43532,#10170);
#7865=LINE('',#43533,#10171);
#7866=LINE('',#43537,#10172);
#7867=LINE('',#43540,#10173);
#7868=LINE('',#43541,#10174);
#7869=LINE('',#43545,#10175);
#7870=LINE('',#43548,#10176);
#7871=LINE('',#43549,#10177);
#7872=LINE('',#43553,#10178);
#7873=LINE('',#43556,#10179);
#7874=LINE('',#43557,#10180);
#7875=LINE('',#43561,#10181);
#7876=LINE('',#43564,#10182);
#7877=LINE('',#43565,#10183);
#7878=LINE('',#43569,#10184);
#7879=LINE('',#43571,#10185);
#7880=LINE('',#43572,#10186);
#7881=LINE('',#43574,#10187);
#7882=LINE('',#43576,#10188);
#7883=LINE('',#43578,#10189);
#7884=LINE('',#43581,#10190);
#7885=LINE('',#43583,#10191);
#7886=LINE('',#43585,#10192);
#7887=LINE('',#43586,#10193);
#7888=LINE('',#43588,#10194);
#7889=LINE('',#43590,#10195);
#7890=LINE('',#43592,#10196);
#7891=LINE('',#43594,#10197);
#7892=LINE('',#43596,#10198);
#7893=LINE('',#43598,#10199);
#7894=LINE('',#43600,#10200);
#7895=LINE('',#43602,#10201);
#7896=LINE('',#43604,#10202);
#7897=LINE('',#43606,#10203);
#7898=LINE('',#43608,#10204);
#7899=LINE('',#43611,#10205);
#7900=LINE('',#43613,#10206);
#7901=LINE('',#43615,#10207);
#7902=LINE('',#43618,#10208);
#7903=LINE('',#43621,#10209);
#7904=LINE('',#43624,#10210);
#7905=LINE('',#43705,#10211);
#7906=LINE('',#43709,#10212);
#7907=LINE('',#43711,#10213);
#7908=LINE('',#43716,#10214);
#7909=LINE('',#43723,#10215);
#7910=LINE('',#43728,#10216);
#7911=LINE('',#43733,#10217);
#7912=LINE('',#43737,#10218);
#7913=LINE('',#43745,#10219);
#7914=LINE('',#43749,#10220);
#7915=LINE('',#43758,#10221);
#7916=LINE('',#43762,#10222);
#7917=LINE('',#43771,#10223);
#7918=LINE('',#43775,#10224);
#7919=LINE('',#43784,#10225);
#7920=LINE('',#43788,#10226);
#7921=LINE('',#43797,#10227);
#7922=LINE('',#43801,#10228);
#7923=LINE('',#43810,#10229);
#7924=LINE('',#43814,#10230);
#7925=LINE('',#43823,#10231);
#7926=LINE('',#43827,#10232);
#7927=LINE('',#43836,#10233);
#7928=LINE('',#43840,#10234);
#7929=LINE('',#43849,#10235);
#7930=LINE('',#43854,#10236);
#7931=LINE('',#43861,#10237);
#7932=LINE('',#43863,#10238);
#7933=LINE('',#43865,#10239);
#7934=LINE('',#43867,#10240);
#7935=LINE('',#43869,#10241);
#7936=LINE('',#43870,#10242);
#7937=LINE('',#43873,#10243);
#7938=LINE('',#43875,#10244);
#7939=LINE('',#43877,#10245);
#7940=LINE('',#43879,#10246);
#7941=LINE('',#43880,#10247);
#7942=LINE('',#43883,#10248);
#7943=LINE('',#43884,#10249);
#7944=LINE('',#43887,#10250);
#7945=LINE('',#43889,#10251);
#7946=LINE('',#43891,#10252);
#7947=LINE('',#43892,#10253);
#7948=LINE('',#43897,#10254);
#7949=LINE('',#43901,#10255);
#7950=LINE('',#43910,#10256);
#7951=LINE('',#43914,#10257);
#7952=LINE('',#43922,#10258);
#7953=LINE('',#43924,#10259);
#7954=LINE('',#43926,#10260);
#7955=LINE('',#43928,#10261);
#7956=LINE('',#43930,#10262);
#7957=LINE('',#43931,#10263);
#7958=LINE('',#43934,#10264);
#7959=LINE('',#43936,#10265);
#7960=LINE('',#43938,#10266);
#7961=LINE('',#43940,#10267);
#7962=LINE('',#43941,#10268);
#7963=LINE('',#43944,#10269);
#7964=LINE('',#43945,#10270);
#7965=LINE('',#43948,#10271);
#7966=LINE('',#43950,#10272);
#7967=LINE('',#43952,#10273);
#7968=LINE('',#43953,#10274);
#7969=LINE('',#43956,#10275);
#7970=LINE('',#43958,#10276);
#7971=LINE('',#43959,#10277);
#7972=LINE('',#43962,#10278);
#7973=LINE('',#43964,#10279);
#7974=LINE('',#43965,#10280);
#7975=LINE('',#43970,#10281);
#7976=LINE('',#43974,#10282);
#7977=LINE('',#43983,#10283);
#7978=LINE('',#43987,#10284);
#7979=LINE('',#43995,#10285);
#7980=LINE('',#43997,#10286);
#7981=LINE('',#43998,#10287);
#7982=LINE('',#44082,#10288);
#7983=LINE('',#44084,#10289);
#7984=LINE('',#44086,#10290);
#7985=LINE('',#44088,#10291);
#7986=LINE('',#44090,#10292);
#7987=LINE('',#44092,#10293);
#7988=LINE('',#44094,#10294);
#7989=LINE('',#44097,#10295);
#7990=LINE('',#44102,#10296);
#7991=LINE('',#44105,#10297);
#7992=LINE('',#44110,#10298);
#7993=LINE('',#44112,#10299);
#7994=LINE('',#44114,#10300);
#7995=LINE('',#44116,#10301);
#7996=LINE('',#44118,#10302);
#7997=LINE('',#44120,#10303);
#7998=LINE('',#44123,#10304);
#7999=LINE('',#44128,#10305);
#8000=LINE('',#44131,#10306);
#8001=LINE('',#44136,#10307);
#8002=LINE('',#44139,#10308);
#8003=LINE('',#44144,#10309);
#8004=LINE('',#44147,#10310);
#8005=LINE('',#44152,#10311);
#8006=LINE('',#44155,#10312);
#8007=LINE('',#44160,#10313);
#8008=LINE('',#44163,#10314);
#8009=LINE('',#44168,#10315);
#8010=LINE('',#44171,#10316);
#8011=LINE('',#44176,#10317);
#8012=LINE('',#44179,#10318);
#8013=LINE('',#44184,#10319);
#8014=LINE('',#44187,#10320);
#8015=LINE('',#44192,#10321);
#8016=LINE('',#44195,#10322);
#8017=LINE('',#44200,#10323);
#8018=LINE('',#44203,#10324);
#8019=LINE('',#44208,#10325);
#8020=LINE('',#44211,#10326);
#8021=LINE('',#44216,#10327);
#8022=LINE('',#44218,#10328);
#8023=LINE('',#44220,#10329);
#8024=LINE('',#44223,#10330);
#8025=LINE('',#44228,#10331);
#8026=LINE('',#44231,#10332);
#8027=LINE('',#44236,#10333);
#8028=LINE('',#44239,#10334);
#8029=LINE('',#44244,#10335);
#8030=LINE('',#44247,#10336);
#8031=LINE('',#44252,#10337);
#8032=LINE('',#44255,#10338);
#8033=LINE('',#44260,#10339);
#8034=LINE('',#44263,#10340);
#8035=LINE('',#44268,#10341);
#8036=LINE('',#44271,#10342);
#8037=LINE('',#44276,#10343);
#8038=LINE('',#44279,#10344);
#8039=LINE('',#44284,#10345);
#8040=LINE('',#44287,#10346);
#8041=LINE('',#44292,#10347);
#8042=LINE('',#44295,#10348);
#8043=LINE('',#44300,#10349);
#8044=LINE('',#44303,#10350);
#8045=LINE('',#44308,#10351);
#8046=LINE('',#44311,#10352);
#8047=LINE('',#44316,#10353);
#8048=LINE('',#44319,#10354);
#8049=LINE('',#44324,#10355);
#8050=LINE('',#44327,#10356);
#8051=LINE('',#44332,#10357);
#8052=LINE('',#44335,#10358);
#8053=LINE('',#44340,#10359);
#8054=LINE('',#44342,#10360);
#8055=LINE('',#44343,#10361);
#8056=LINE('',#44345,#10362);
#8057=LINE('',#44432,#10363);
#8058=LINE('',#44434,#10364);
#8059=LINE('',#44436,#10365);
#8060=LINE('',#44438,#10366);
#8061=LINE('',#44440,#10367);
#8062=LINE('',#44442,#10368);
#8063=LINE('',#44444,#10369);
#8064=LINE('',#44446,#10370);
#8065=LINE('',#44449,#10371);
#8066=LINE('',#44452,#10372);
#8067=LINE('',#44455,#10373);
#8068=LINE('',#44458,#10374);
#8069=LINE('',#44461,#10375);
#8070=LINE('',#44464,#10376);
#8071=LINE('',#44467,#10377);
#8072=LINE('',#44470,#10378);
#8073=LINE('',#44473,#10379);
#8074=LINE('',#44476,#10380);
#8075=LINE('',#44479,#10381);
#8076=LINE('',#44482,#10382);
#8077=LINE('',#44485,#10383);
#8078=LINE('',#44488,#10384);
#8079=LINE('',#44491,#10385);
#8080=LINE('',#44494,#10386);
#8081=LINE('',#44497,#10387);
#8082=LINE('',#44500,#10388);
#8083=LINE('',#44503,#10389);
#8084=LINE('',#44506,#10390);
#8085=LINE('',#44508,#10391);
#8086=LINE('',#44510,#10392);
#8087=LINE('',#44512,#10393);
#8088=LINE('',#44514,#10394);
#8089=LINE('',#44516,#10395);
#8090=LINE('',#44518,#10396);
#8091=LINE('',#44520,#10397);
#8092=LINE('',#44522,#10398);
#8093=LINE('',#44524,#10399);
#8094=LINE('',#44526,#10400);
#8095=LINE('',#44528,#10401);
#8096=LINE('',#44530,#10402);
#8097=LINE('',#44532,#10403);
#8098=LINE('',#44534,#10404);
#8099=LINE('',#44536,#10405);
#8100=LINE('',#44538,#10406);
#8101=LINE('',#44540,#10407);
#8102=LINE('',#44542,#10408);
#8103=LINE('',#44544,#10409);
#8104=LINE('',#44546,#10410);
#8105=LINE('',#44548,#10411);
#8106=LINE('',#44550,#10412);
#8107=LINE('',#44553,#10413);
#8108=LINE('',#44556,#10414);
#8109=LINE('',#44559,#10415);
#8110=LINE('',#44562,#10416);
#8111=LINE('',#44564,#10417);
#8112=LINE('',#44579,#10418);
#8113=LINE('',#44586,#10419);
#8114=LINE('',#44597,#10420);
#8115=LINE('',#44601,#10421);
#8116=LINE('',#44603,#10422);
#8117=LINE('',#44605,#10423);
#8118=LINE('',#44607,#10424);
#8119=LINE('',#44609,#10425);
#8120=LINE('',#44610,#10426);
#8121=LINE('',#44613,#10427);
#8122=LINE('',#44617,#10428);
#8123=LINE('',#44618,#10429);
#8124=LINE('',#44622,#10430);
#8125=LINE('',#44624,#10431);
#8126=LINE('',#44625,#10432);
#8127=LINE('',#44627,#10433);
#8128=LINE('',#44628,#10434);
#8129=LINE('',#44632,#10435);
#8130=LINE('',#44633,#10436);
#8131=LINE('',#44635,#10437);
#8132=LINE('',#44636,#10438);
#8133=LINE('',#44640,#10439);
#8134=LINE('',#44642,#10440);
#8135=LINE('',#44643,#10441);
#8136=LINE('',#44645,#10442);
#8137=LINE('',#44647,#10443);
#8138=LINE('',#44648,#10444);
#8139=LINE('',#44650,#10445);
#8140=LINE('',#44651,#10446);
#8141=LINE('',#44655,#10447);
#8142=LINE('',#44656,#10448);
#8143=LINE('',#44658,#10449);
#8144=LINE('',#44659,#10450);
#8145=LINE('',#44663,#10451);
#8146=LINE('',#44664,#10452);
#8147=LINE('',#44666,#10453);
#8148=LINE('',#44667,#10454);
#8149=LINE('',#44669,#10455);
#8150=LINE('',#44675,#10456);
#8151=LINE('',#44682,#10457);
#8152=LINE('',#44684,#10458);
#8153=LINE('',#44685,#10459);
#8154=LINE('',#44688,#10460);
#8155=LINE('',#44690,#10461);
#8156=LINE('',#44691,#10462);
#8157=LINE('',#44695,#10463);
#8158=LINE('',#44696,#10464);
#8159=LINE('',#44698,#10465);
#8160=LINE('',#44699,#10466);
#8161=LINE('',#44702,#10467);
#8162=LINE('',#44703,#10468);
#8163=LINE('',#44705,#10469);
#8164=LINE('',#44706,#10470);
#8165=LINE('',#44720,#10471);
#8166=LINE('',#44722,#10472);
#8167=LINE('',#44725,#10473);
#8168=LINE('',#44806,#10474);
#8169=LINE('',#44810,#10475);
#8170=LINE('',#44812,#10476);
#8171=LINE('',#44816,#10477);
#8172=LINE('',#44852,#10478);
#8173=LINE('',#44908,#10479);
#8174=LINE('',#44954,#10480);
#8175=LINE('',#45009,#10481);
#8176=LINE('',#46417,#10482);
#8177=LINE('',#46441,#10483);
#8178=LINE('',#46489,#10484);
#8179=LINE('',#46537,#10485);
#8180=LINE('',#46585,#10486);
#8181=LINE('',#46639,#10487);
#8182=LINE('',#46687,#10488);
#8183=LINE('',#46735,#10489);
#8184=LINE('',#46789,#10490);
#8185=LINE('',#46837,#10491);
#8186=LINE('',#46885,#10492);
#8187=LINE('',#46901,#10493);
#8188=LINE('',#46925,#10494);
#8189=LINE('',#46949,#10495);
#8190=LINE('',#46974,#10496);
#8191=LINE('',#46999,#10497);
#8192=LINE('',#47023,#10498);
#8193=LINE('',#47048,#10499);
#8194=LINE('',#47073,#10500);
#8195=LINE('',#47097,#10501);
#8196=LINE('',#48105,#10502);
#8197=LINE('',#48107,#10503);
#8198=LINE('',#48109,#10504);
#8199=LINE('',#48110,#10505);
#8200=LINE('',#48114,#10506);
#8201=LINE('',#48117,#10507);
#8202=LINE('',#48118,#10508);
#8203=LINE('',#48124,#10509);
#8204=LINE('',#48126,#10510);
#8205=LINE('',#48128,#10511);
#8206=LINE('',#48129,#10512);
#8207=LINE('',#48133,#10513);
#8208=LINE('',#48136,#10514);
#8209=LINE('',#48137,#10515);
#8210=LINE('',#48143,#10516);
#8211=LINE('',#48145,#10517);
#8212=LINE('',#48147,#10518);
#8213=LINE('',#48148,#10519);
#8214=LINE('',#48152,#10520);
#8215=LINE('',#48155,#10521);
#8216=LINE('',#48156,#10522);
#8217=LINE('',#48162,#10523);
#8218=LINE('',#48164,#10524);
#8219=LINE('',#48166,#10525);
#8220=LINE('',#48167,#10526);
#8221=LINE('',#48171,#10527);
#8222=LINE('',#48174,#10528);
#8223=LINE('',#48175,#10529);
#8224=LINE('',#48181,#10530);
#8225=LINE('',#48183,#10531);
#8226=LINE('',#48185,#10532);
#8227=LINE('',#48186,#10533);
#8228=LINE('',#48190,#10534);
#8229=LINE('',#48193,#10535);
#8230=LINE('',#48194,#10536);
#8231=LINE('',#48200,#10537);
#8232=LINE('',#48202,#10538);
#8233=LINE('',#48204,#10539);
#8234=LINE('',#48205,#10540);
#8235=LINE('',#48209,#10541);
#8236=LINE('',#48212,#10542);
#8237=LINE('',#48213,#10543);
#8238=LINE('',#48219,#10544);
#8239=LINE('',#48221,#10545);
#8240=LINE('',#48223,#10546);
#8241=LINE('',#48224,#10547);
#8242=LINE('',#48228,#10548);
#8243=LINE('',#48231,#10549);
#8244=LINE('',#48232,#10550);
#8245=LINE('',#48238,#10551);
#8246=LINE('',#48240,#10552);
#8247=LINE('',#48242,#10553);
#8248=LINE('',#48243,#10554);
#8249=LINE('',#48247,#10555);
#8250=LINE('',#48250,#10556);
#8251=LINE('',#48251,#10557);
#8252=LINE('',#48257,#10558);
#8253=LINE('',#48259,#10559);
#8254=LINE('',#48261,#10560);
#8255=LINE('',#48262,#10561);
#8256=LINE('',#48266,#10562);
#8257=LINE('',#48269,#10563);
#8258=LINE('',#48270,#10564);
#8259=LINE('',#48276,#10565);
#8260=LINE('',#48278,#10566);
#8261=LINE('',#48280,#10567);
#8262=LINE('',#48281,#10568);
#8263=LINE('',#48285,#10569);
#8264=LINE('',#48288,#10570);
#8265=LINE('',#48289,#10571);
#8266=LINE('',#48295,#10572);
#8267=LINE('',#48297,#10573);
#8268=LINE('',#48299,#10574);
#8269=LINE('',#48300,#10575);
#8270=LINE('',#48304,#10576);
#8271=LINE('',#48307,#10577);
#8272=LINE('',#48308,#10578);
#8273=LINE('',#48314,#10579);
#8274=LINE('',#48316,#10580);
#8275=LINE('',#48318,#10581);
#8276=LINE('',#48319,#10582);
#8277=LINE('',#48323,#10583);
#8278=LINE('',#48326,#10584);
#8279=LINE('',#48327,#10585);
#8280=LINE('',#48333,#10586);
#8281=LINE('',#48335,#10587);
#8282=LINE('',#48337,#10588);
#8283=LINE('',#48338,#10589);
#8284=LINE('',#48342,#10590);
#8285=LINE('',#48345,#10591);
#8286=LINE('',#48346,#10592);
#8287=LINE('',#48352,#10593);
#8288=LINE('',#48354,#10594);
#8289=LINE('',#48356,#10595);
#8290=LINE('',#48357,#10596);
#8291=LINE('',#48361,#10597);
#8292=LINE('',#48364,#10598);
#8293=LINE('',#48365,#10599);
#8294=LINE('',#48371,#10600);
#8295=LINE('',#48373,#10601);
#8296=LINE('',#48375,#10602);
#8297=LINE('',#48376,#10603);
#8298=LINE('',#48380,#10604);
#8299=LINE('',#48383,#10605);
#8300=LINE('',#48384,#10606);
#8301=LINE('',#48390,#10607);
#8302=LINE('',#48392,#10608);
#8303=LINE('',#48394,#10609);
#8304=LINE('',#48395,#10610);
#8305=LINE('',#48399,#10611);
#8306=LINE('',#48402,#10612);
#8307=LINE('',#48403,#10613);
#8308=LINE('',#48409,#10614);
#8309=LINE('',#48411,#10615);
#8310=LINE('',#48413,#10616);
#8311=LINE('',#48414,#10617);
#8312=LINE('',#48418,#10618);
#8313=LINE('',#48421,#10619);
#8314=LINE('',#48422,#10620);
#8315=LINE('',#48428,#10621);
#8316=LINE('',#48430,#10622);
#8317=LINE('',#48432,#10623);
#8318=LINE('',#48433,#10624);
#8319=LINE('',#48438,#10625);
#8320=LINE('',#48442,#10626);
#8321=LINE('',#48443,#10627);
#8322=LINE('',#48451,#10628);
#8323=LINE('',#48453,#10629);
#8324=LINE('',#48455,#10630);
#8325=LINE('',#48456,#10631);
#8326=LINE('',#48460,#10632);
#8327=LINE('',#48463,#10633);
#8328=LINE('',#48464,#10634);
#8329=LINE('',#48470,#10635);
#8330=LINE('',#48472,#10636);
#8331=LINE('',#48474,#10637);
#8332=LINE('',#48475,#10638);
#8333=LINE('',#48479,#10639);
#8334=LINE('',#48482,#10640);
#8335=LINE('',#48483,#10641);
#8336=LINE('',#48489,#10642);
#8337=LINE('',#48491,#10643);
#8338=LINE('',#48493,#10644);
#8339=LINE('',#48494,#10645);
#8340=LINE('',#48498,#10646);
#8341=LINE('',#48501,#10647);
#8342=LINE('',#48502,#10648);
#8343=LINE('',#48508,#10649);
#8344=LINE('',#48510,#10650);
#8345=LINE('',#48512,#10651);
#8346=LINE('',#48513,#10652);
#8347=LINE('',#48517,#10653);
#8348=LINE('',#48520,#10654);
#8349=LINE('',#48521,#10655);
#8350=LINE('',#48527,#10656);
#8351=LINE('',#48529,#10657);
#8352=LINE('',#48531,#10658);
#8353=LINE('',#48532,#10659);
#8354=LINE('',#48536,#10660);
#8355=LINE('',#48539,#10661);
#8356=LINE('',#48540,#10662);
#8357=LINE('',#48546,#10663);
#8358=LINE('',#48548,#10664);
#8359=LINE('',#48550,#10665);
#8360=LINE('',#48551,#10666);
#8361=LINE('',#48555,#10667);
#8362=LINE('',#48558,#10668);
#8363=LINE('',#48559,#10669);
#8364=LINE('',#48565,#10670);
#8365=LINE('',#48567,#10671);
#8366=LINE('',#48569,#10672);
#8367=LINE('',#48570,#10673);
#8368=LINE('',#48574,#10674);
#8369=LINE('',#48577,#10675);
#8370=LINE('',#48578,#10676);
#8371=LINE('',#48584,#10677);
#8372=LINE('',#48586,#10678);
#8373=LINE('',#48588,#10679);
#8374=LINE('',#48589,#10680);
#8375=LINE('',#48593,#10681);
#8376=LINE('',#48596,#10682);
#8377=LINE('',#48597,#10683);
#8378=LINE('',#48603,#10684);
#8379=LINE('',#48605,#10685);
#8380=LINE('',#48607,#10686);
#8381=LINE('',#48608,#10687);
#8382=LINE('',#48612,#10688);
#8383=LINE('',#48615,#10689);
#8384=LINE('',#48616,#10690);
#8385=LINE('',#48622,#10691);
#8386=LINE('',#48624,#10692);
#8387=LINE('',#48626,#10693);
#8388=LINE('',#48627,#10694);
#8389=LINE('',#48631,#10695);
#8390=LINE('',#48634,#10696);
#8391=LINE('',#48635,#10697);
#8392=LINE('',#48641,#10698);
#8393=LINE('',#48643,#10699);
#8394=LINE('',#48645,#10700);
#8395=LINE('',#48646,#10701);
#8396=LINE('',#48650,#10702);
#8397=LINE('',#48653,#10703);
#8398=LINE('',#48654,#10704);
#8399=LINE('',#48660,#10705);
#8400=LINE('',#48662,#10706);
#8401=LINE('',#48664,#10707);
#8402=LINE('',#48665,#10708);
#8403=LINE('',#48669,#10709);
#8404=LINE('',#48672,#10710);
#8405=LINE('',#48673,#10711);
#8406=LINE('',#48679,#10712);
#8407=LINE('',#48681,#10713);
#8408=LINE('',#48683,#10714);
#8409=LINE('',#48684,#10715);
#8410=LINE('',#48688,#10716);
#8411=LINE('',#48691,#10717);
#8412=LINE('',#48692,#10718);
#8413=LINE('',#48698,#10719);
#8414=LINE('',#48700,#10720);
#8415=LINE('',#48702,#10721);
#8416=LINE('',#48703,#10722);
#8417=LINE('',#48707,#10723);
#8418=LINE('',#48710,#10724);
#8419=LINE('',#48711,#10725);
#8420=LINE('',#48717,#10726);
#8421=LINE('',#48719,#10727);
#8422=LINE('',#48721,#10728);
#8423=LINE('',#48722,#10729);
#8424=LINE('',#48726,#10730);
#8425=LINE('',#48729,#10731);
#8426=LINE('',#48730,#10732);
#8427=LINE('',#48736,#10733);
#8428=LINE('',#48738,#10734);
#8429=LINE('',#48740,#10735);
#8430=LINE('',#48741,#10736);
#8431=LINE('',#48745,#10737);
#8432=LINE('',#48748,#10738);
#8433=LINE('',#48749,#10739);
#8434=LINE('',#48755,#10740);
#8435=LINE('',#48757,#10741);
#8436=LINE('',#48759,#10742);
#8437=LINE('',#48760,#10743);
#8438=LINE('',#48764,#10744);
#8439=LINE('',#48767,#10745);
#8440=LINE('',#48768,#10746);
#8441=LINE('',#48774,#10747);
#8442=LINE('',#48776,#10748);
#8443=LINE('',#48778,#10749);
#8444=LINE('',#48779,#10750);
#8445=LINE('',#48783,#10751);
#8446=LINE('',#48786,#10752);
#8447=LINE('',#48787,#10753);
#8448=LINE('',#48793,#10754);
#8449=LINE('',#48798,#10755);
#8450=LINE('',#48800,#10756);
#8451=LINE('',#48802,#10757);
#8452=LINE('',#48803,#10758);
#8453=LINE('',#48806,#10759);
#8454=LINE('',#48808,#10760);
#8455=LINE('',#48809,#10761);
#8456=LINE('',#48812,#10762);
#8457=LINE('',#48814,#10763);
#8458=LINE('',#48815,#10764);
#8459=LINE('',#48818,#10765);
#8460=LINE('',#48820,#10766);
#8461=LINE('',#48821,#10767);
#8462=LINE('',#48824,#10768);
#8463=LINE('',#48826,#10769);
#8464=LINE('',#48827,#10770);
#8465=LINE('',#48829,#10771);
#8466=LINE('',#48830,#10772);
#8467=LINE('',#48842,#10773);
#8468=LINE('',#48851,#10774);
#8469=LINE('',#48857,#10775);
#8470=LINE('',#48861,#10776);
#8471=LINE('',#48866,#10777);
#8472=LINE('',#48867,#10778);
#8473=LINE('',#48871,#10779);
#8474=LINE('',#48878,#10780);
#8475=LINE('',#48886,#10781);
#8476=LINE('',#48900,#10782);
#8477=LINE('',#48904,#10783);
#8478=LINE('',#48908,#10784);
#8479=LINE('',#49549,#10785);
#8480=LINE('',#49555,#10786);
#8481=LINE('',#49562,#10787);
#8482=LINE('',#49568,#10788);
#8483=LINE('',#49573,#10789);
#8484=LINE('',#49597,#10790);
#8485=LINE('',#49645,#10791);
#8486=LINE('',#49693,#10792);
#8487=LINE('',#49744,#10793);
#8488=LINE('',#49795,#10794);
#8489=LINE('',#49843,#10795);
#8490=LINE('',#49891,#10796);
#8491=LINE('',#49945,#10797);
#8492=LINE('',#49993,#10798);
#8493=LINE('',#50041,#10799);
#8494=LINE('',#50095,#10800);
#8495=LINE('',#50143,#10801);
#8496=LINE('',#50191,#10802);
#8497=LINE('',#50239,#10803);
#8498=LINE('',#50293,#10804);
#8499=LINE('',#50341,#10805);
#8500=LINE('',#50389,#10806);
#8501=LINE('',#50443,#10807);
#8502=LINE('',#50491,#10808);
#8503=LINE('',#50539,#10809);
#8504=LINE('',#50593,#10810);
#8505=LINE('',#50641,#10811);
#8506=LINE('',#50689,#10812);
#8507=LINE('',#50737,#10813);
#8508=LINE('',#50791,#10814);
#8509=LINE('',#50839,#10815);
#8510=LINE('',#50887,#10816);
#8511=LINE('',#50941,#10817);
#8512=LINE('',#50989,#10818);
#8513=LINE('',#51037,#10819);
#8514=LINE('',#51091,#10820);
#8515=LINE('',#51139,#10821);
#8516=LINE('',#51187,#10822);
#8517=LINE('',#51235,#10823);
#8518=LINE('',#51289,#10824);
#8519=LINE('',#51337,#10825);
#8520=LINE('',#51385,#10826);
#8521=LINE('',#51439,#10827);
#8522=LINE('',#51487,#10828);
#8523=LINE('',#51535,#10829);
#8524=LINE('',#51589,#10830);
#8525=LINE('',#51637,#10831);
#8526=LINE('',#51655,#10832);
#8527=LINE('',#51679,#10833);
#8528=LINE('',#51704,#10834);
#8529=LINE('',#51729,#10835);
#8530=LINE('',#51753,#10836);
#8531=LINE('',#51778,#10837);
#8532=LINE('',#51803,#10838);
#8533=LINE('',#51827,#10839);
#8534=LINE('',#51852,#10840);
#8535=LINE('',#51877,#10841);
#8536=LINE('',#51901,#10842);
#8537=LINE('',#51925,#10843);
#8538=LINE('',#51950,#10844);
#8539=LINE('',#51975,#10845);
#8540=LINE('',#51999,#10846);
#8541=LINE('',#52024,#10847);
#8542=LINE('',#52049,#10848);
#8543=LINE('',#52073,#10849);
#8544=LINE('',#52098,#10850);
#8545=LINE('',#52123,#10851);
#8546=LINE('',#52147,#10852);
#8547=LINE('',#52171,#10853);
#8548=LINE('',#52196,#10854);
#8549=LINE('',#52221,#10855);
#8550=LINE('',#52245,#10856);
#8551=LINE('',#52270,#10857);
#8552=LINE('',#52295,#10858);
#8553=LINE('',#52319,#10859);
#8554=LINE('',#52344,#10860);
#8555=LINE('',#52369,#10861);
#8556=LINE('',#52393,#10862);
#8557=LINE('',#52417,#10863);
#8558=LINE('',#52442,#10864);
#8559=LINE('',#52467,#10865);
#8560=LINE('',#52491,#10866);
#8561=LINE('',#52516,#10867);
#8562=LINE('',#52541,#10868);
#8563=LINE('',#52565,#10869);
#8564=LINE('',#52590,#10870);
#8565=LINE('',#52614,#10871);
#8566=LINE('',#52639,#10872);
#8567=LINE('',#55238,#10873);
#8568=LINE('',#55240,#10874);
#8569=LINE('',#55242,#10875);
#8570=LINE('',#55243,#10876);
#8571=LINE('',#55247,#10877);
#8572=LINE('',#55250,#10878);
#8573=LINE('',#55251,#10879);
#8574=LINE('',#55257,#10880);
#8575=LINE('',#55259,#10881);
#8576=LINE('',#55261,#10882);
#8577=LINE('',#55262,#10883);
#8578=LINE('',#55266,#10884);
#8579=LINE('',#55269,#10885);
#8580=LINE('',#55270,#10886);
#8581=LINE('',#55276,#10887);
#8582=LINE('',#55278,#10888);
#8583=LINE('',#55280,#10889);
#8584=LINE('',#55281,#10890);
#8585=LINE('',#55285,#10891);
#8586=LINE('',#55288,#10892);
#8587=LINE('',#55289,#10893);
#8588=LINE('',#55295,#10894);
#8589=LINE('',#55297,#10895);
#8590=LINE('',#55299,#10896);
#8591=LINE('',#55300,#10897);
#8592=LINE('',#55304,#10898);
#8593=LINE('',#55307,#10899);
#8594=LINE('',#55308,#10900);
#8595=LINE('',#55314,#10901);
#8596=LINE('',#55316,#10902);
#8597=LINE('',#55318,#10903);
#8598=LINE('',#55319,#10904);
#8599=LINE('',#55323,#10905);
#8600=LINE('',#55326,#10906);
#8601=LINE('',#55327,#10907);
#8602=LINE('',#55333,#10908);
#8603=LINE('',#55335,#10909);
#8604=LINE('',#55337,#10910);
#8605=LINE('',#55338,#10911);
#8606=LINE('',#55342,#10912);
#8607=LINE('',#55345,#10913);
#8608=LINE('',#55346,#10914);
#8609=LINE('',#55352,#10915);
#8610=LINE('',#55354,#10916);
#8611=LINE('',#55356,#10917);
#8612=LINE('',#55357,#10918);
#8613=LINE('',#55361,#10919);
#8614=LINE('',#55364,#10920);
#8615=LINE('',#55365,#10921);
#8616=LINE('',#55371,#10922);
#8617=LINE('',#55373,#10923);
#8618=LINE('',#55375,#10924);
#8619=LINE('',#55376,#10925);
#8620=LINE('',#55380,#10926);
#8621=LINE('',#55383,#10927);
#8622=LINE('',#55384,#10928);
#8623=LINE('',#55390,#10929);
#8624=LINE('',#55392,#10930);
#8625=LINE('',#55394,#10931);
#8626=LINE('',#55395,#10932);
#8627=LINE('',#55399,#10933);
#8628=LINE('',#55402,#10934);
#8629=LINE('',#55403,#10935);
#8630=LINE('',#55409,#10936);
#8631=LINE('',#55411,#10937);
#8632=LINE('',#55413,#10938);
#8633=LINE('',#55414,#10939);
#8634=LINE('',#55418,#10940);
#8635=LINE('',#55421,#10941);
#8636=LINE('',#55422,#10942);
#8637=LINE('',#55428,#10943);
#8638=LINE('',#55430,#10944);
#8639=LINE('',#55432,#10945);
#8640=LINE('',#55433,#10946);
#8641=LINE('',#55437,#10947);
#8642=LINE('',#55440,#10948);
#8643=LINE('',#55441,#10949);
#8644=LINE('',#55447,#10950);
#8645=LINE('',#55449,#10951);
#8646=LINE('',#55451,#10952);
#8647=LINE('',#55452,#10953);
#8648=LINE('',#55456,#10954);
#8649=LINE('',#55459,#10955);
#8650=LINE('',#55460,#10956);
#8651=LINE('',#55466,#10957);
#8652=LINE('',#55468,#10958);
#8653=LINE('',#55470,#10959);
#8654=LINE('',#55471,#10960);
#8655=LINE('',#55475,#10961);
#8656=LINE('',#55478,#10962);
#8657=LINE('',#55479,#10963);
#8658=LINE('',#55485,#10964);
#8659=LINE('',#55487,#10965);
#8660=LINE('',#55489,#10966);
#8661=LINE('',#55490,#10967);
#8662=LINE('',#55494,#10968);
#8663=LINE('',#55497,#10969);
#8664=LINE('',#55498,#10970);
#8665=LINE('',#55504,#10971);
#8666=LINE('',#55506,#10972);
#8667=LINE('',#55508,#10973);
#8668=LINE('',#55509,#10974);
#8669=LINE('',#55513,#10975);
#8670=LINE('',#55516,#10976);
#8671=LINE('',#55517,#10977);
#8672=LINE('',#55523,#10978);
#8673=LINE('',#55525,#10979);
#8674=LINE('',#55527,#10980);
#8675=LINE('',#55528,#10981);
#8676=LINE('',#55532,#10982);
#8677=LINE('',#55535,#10983);
#8678=LINE('',#55536,#10984);
#8679=LINE('',#55542,#10985);
#8680=LINE('',#55544,#10986);
#8681=LINE('',#55546,#10987);
#8682=LINE('',#55547,#10988);
#8683=LINE('',#55551,#10989);
#8684=LINE('',#55554,#10990);
#8685=LINE('',#55555,#10991);
#8686=LINE('',#55561,#10992);
#8687=LINE('',#55563,#10993);
#8688=LINE('',#55565,#10994);
#8689=LINE('',#55566,#10995);
#8690=LINE('',#55571,#10996);
#8691=LINE('',#55575,#10997);
#8692=LINE('',#55576,#10998);
#8693=LINE('',#55584,#10999);
#8694=LINE('',#55586,#11000);
#8695=LINE('',#55588,#11001);
#8696=LINE('',#55589,#11002);
#8697=LINE('',#55593,#11003);
#8698=LINE('',#55596,#11004);
#8699=LINE('',#55597,#11005);
#8700=LINE('',#55603,#11006);
#8701=LINE('',#55605,#11007);
#8702=LINE('',#55607,#11008);
#8703=LINE('',#55608,#11009);
#8704=LINE('',#55612,#11010);
#8705=LINE('',#55615,#11011);
#8706=LINE('',#55616,#11012);
#8707=LINE('',#55622,#11013);
#8708=LINE('',#55624,#11014);
#8709=LINE('',#55626,#11015);
#8710=LINE('',#55627,#11016);
#8711=LINE('',#55631,#11017);
#8712=LINE('',#55634,#11018);
#8713=LINE('',#55635,#11019);
#8714=LINE('',#55641,#11020);
#8715=LINE('',#55643,#11021);
#8716=LINE('',#55645,#11022);
#8717=LINE('',#55646,#11023);
#8718=LINE('',#55650,#11024);
#8719=LINE('',#55653,#11025);
#8720=LINE('',#55654,#11026);
#8721=LINE('',#55660,#11027);
#8722=LINE('',#55662,#11028);
#8723=LINE('',#55664,#11029);
#8724=LINE('',#55665,#11030);
#8725=LINE('',#55669,#11031);
#8726=LINE('',#55672,#11032);
#8727=LINE('',#55673,#11033);
#8728=LINE('',#55679,#11034);
#8729=LINE('',#55681,#11035);
#8730=LINE('',#55683,#11036);
#8731=LINE('',#55684,#11037);
#8732=LINE('',#55688,#11038);
#8733=LINE('',#55691,#11039);
#8734=LINE('',#55692,#11040);
#8735=LINE('',#55698,#11041);
#8736=LINE('',#55700,#11042);
#8737=LINE('',#55702,#11043);
#8738=LINE('',#55703,#11044);
#8739=LINE('',#55707,#11045);
#8740=LINE('',#55710,#11046);
#8741=LINE('',#55711,#11047);
#8742=LINE('',#55717,#11048);
#8743=LINE('',#55719,#11049);
#8744=LINE('',#55721,#11050);
#8745=LINE('',#55722,#11051);
#8746=LINE('',#55726,#11052);
#8747=LINE('',#55729,#11053);
#8748=LINE('',#55730,#11054);
#8749=LINE('',#55736,#11055);
#8750=LINE('',#55738,#11056);
#8751=LINE('',#55740,#11057);
#8752=LINE('',#55741,#11058);
#8753=LINE('',#55745,#11059);
#8754=LINE('',#55748,#11060);
#8755=LINE('',#55749,#11061);
#8756=LINE('',#55755,#11062);
#8757=LINE('',#55757,#11063);
#8758=LINE('',#55759,#11064);
#8759=LINE('',#55760,#11065);
#8760=LINE('',#55764,#11066);
#8761=LINE('',#55767,#11067);
#8762=LINE('',#55768,#11068);
#8763=LINE('',#55774,#11069);
#8764=LINE('',#55776,#11070);
#8765=LINE('',#55778,#11071);
#8766=LINE('',#55779,#11072);
#8767=LINE('',#55783,#11073);
#8768=LINE('',#55786,#11074);
#8769=LINE('',#55787,#11075);
#8770=LINE('',#55793,#11076);
#8771=LINE('',#55795,#11077);
#8772=LINE('',#55797,#11078);
#8773=LINE('',#55798,#11079);
#8774=LINE('',#55802,#11080);
#8775=LINE('',#55805,#11081);
#8776=LINE('',#55806,#11082);
#8777=LINE('',#55812,#11083);
#8778=LINE('',#55814,#11084);
#8779=LINE('',#55816,#11085);
#8780=LINE('',#55817,#11086);
#8781=LINE('',#55821,#11087);
#8782=LINE('',#55824,#11088);
#8783=LINE('',#55825,#11089);
#8784=LINE('',#55831,#11090);
#8785=LINE('',#55833,#11091);
#8786=LINE('',#55835,#11092);
#8787=LINE('',#55836,#11093);
#8788=LINE('',#55840,#11094);
#8789=LINE('',#55843,#11095);
#8790=LINE('',#55844,#11096);
#8791=LINE('',#55850,#11097);
#8792=LINE('',#55852,#11098);
#8793=LINE('',#55854,#11099);
#8794=LINE('',#55855,#11100);
#8795=LINE('',#55859,#11101);
#8796=LINE('',#55862,#11102);
#8797=LINE('',#55863,#11103);
#8798=LINE('',#55869,#11104);
#8799=LINE('',#55871,#11105);
#8800=LINE('',#55873,#11106);
#8801=LINE('',#55874,#11107);
#8802=LINE('',#55878,#11108);
#8803=LINE('',#55881,#11109);
#8804=LINE('',#55882,#11110);
#8805=LINE('',#55888,#11111);
#8806=LINE('',#55890,#11112);
#8807=LINE('',#55892,#11113);
#8808=LINE('',#55893,#11114);
#8809=LINE('',#55897,#11115);
#8810=LINE('',#55900,#11116);
#8811=LINE('',#55901,#11117);
#8812=LINE('',#55907,#11118);
#8813=LINE('',#55909,#11119);
#8814=LINE('',#55911,#11120);
#8815=LINE('',#55912,#11121);
#8816=LINE('',#55916,#11122);
#8817=LINE('',#55919,#11123);
#8818=LINE('',#55920,#11124);
#8819=LINE('',#55926,#11125);
#8820=LINE('',#55931,#11126);
#8821=LINE('',#55933,#11127);
#8822=LINE('',#55935,#11128);
#8823=LINE('',#55936,#11129);
#8824=LINE('',#55939,#11130);
#8825=LINE('',#55941,#11131);
#8826=LINE('',#55942,#11132);
#8827=LINE('',#55945,#11133);
#8828=LINE('',#55947,#11134);
#8829=LINE('',#55948,#11135);
#8830=LINE('',#55951,#11136);
#8831=LINE('',#55953,#11137);
#8832=LINE('',#55954,#11138);
#8833=LINE('',#55957,#11139);
#8834=LINE('',#55959,#11140);
#8835=LINE('',#55960,#11141);
#8836=LINE('',#55962,#11142);
#8837=LINE('',#55963,#11143);
#8838=LINE('',#55969,#11144);
#8839=LINE('',#55973,#11145);
#8840=LINE('',#55974,#11146);
#8841=LINE('',#55978,#11147);
#8842=LINE('',#55987,#11148);
#8843=LINE('',#55991,#11149);
#8844=LINE('',#55995,#11150);
#8845=LINE('',#56001,#11151);
#8846=LINE('',#56025,#11152);
#8847=LINE('',#56073,#11153);
#8848=LINE('',#56121,#11154);
#8849=LINE('',#56169,#11155);
#8850=LINE('',#56223,#11156);
#8851=LINE('',#56271,#11157);
#8852=LINE('',#56319,#11158);
#8853=LINE('',#56373,#11159);
#8854=LINE('',#56421,#11160);
#8855=LINE('',#56469,#11161);
#8856=LINE('',#56517,#11162);
#8857=LINE('',#56571,#11163);
#8858=LINE('',#56619,#11164);
#8859=LINE('',#56667,#11165);
#8860=LINE('',#56721,#11166);
#8861=LINE('',#56769,#11167);
#8862=LINE('',#56817,#11168);
#8863=LINE('',#56865,#11169);
#8864=LINE('',#56919,#11170);
#8865=LINE('',#56967,#11171);
#8866=LINE('',#57015,#11172);
#8867=LINE('',#57069,#11173);
#8868=LINE('',#57117,#11174);
#8869=LINE('',#57165,#11175);
#8870=LINE('',#57213,#11176);
#8871=LINE('',#57267,#11177);
#8872=LINE('',#57315,#11178);
#8873=LINE('',#57363,#11179);
#8874=LINE('',#57417,#11180);
#8875=LINE('',#57465,#11181);
#8876=LINE('',#57513,#11182);
#8877=LINE('',#57561,#11183);
#8878=LINE('',#57615,#11184);
#8879=LINE('',#57663,#11185);
#8880=LINE('',#57711,#11186);
#8881=LINE('',#57765,#11187);
#8882=LINE('',#57813,#11188);
#8883=LINE('',#57861,#11189);
#8884=LINE('',#57909,#11190);
#8885=LINE('',#57963,#11191);
#8886=LINE('',#58011,#11192);
#8887=LINE('',#58059,#11193);
#8888=LINE('',#58113,#11194);
#8889=LINE('',#58161,#11195);
#8890=LINE('',#58209,#11196);
#8891=LINE('',#58257,#11197);
#8892=LINE('',#58311,#11198);
#8893=LINE('',#58359,#11199);
#8894=LINE('',#58407,#11200);
#8895=LINE('',#58461,#11201);
#8896=LINE('',#58509,#11202);
#8897=LINE('',#58557,#11203);
#8898=LINE('',#58605,#11204);
#8899=LINE('',#58659,#11205);
#8900=LINE('',#58707,#11206);
#8901=LINE('',#58755,#11207);
#8902=LINE('',#58809,#11208);
#8903=LINE('',#58857,#11209);
#8904=LINE('',#58905,#11210);
#8905=LINE('',#58953,#11211);
#8906=LINE('',#59007,#11212);
#8907=LINE('',#59055,#11213);
#8908=LINE('',#59103,#11214);
#8909=LINE('',#59157,#11215);
#8910=LINE('',#59205,#11216);
#8911=LINE('',#59253,#11217);
#8912=LINE('',#59301,#11218);
#8913=LINE('',#59355,#11219);
#8914=LINE('',#59403,#11220);
#8915=LINE('',#59419,#11221);
#8916=LINE('',#59443,#11222);
#8917=LINE('',#59468,#11223);
#8918=LINE('',#59493,#11224);
#8919=LINE('',#59517,#11225);
#8920=LINE('',#59541,#11226);
#8921=LINE('',#59566,#11227);
#8922=LINE('',#59591,#11228);
#8923=LINE('',#59615,#11229);
#8924=LINE('',#59640,#11230);
#8925=LINE('',#59665,#11231);
#8926=LINE('',#59689,#11232);
#8927=LINE('',#59713,#11233);
#8928=LINE('',#59738,#11234);
#8929=LINE('',#59763,#11235);
#8930=LINE('',#59787,#11236);
#8931=LINE('',#59812,#11237);
#8932=LINE('',#59837,#11238);
#8933=LINE('',#59861,#11239);
#8934=LINE('',#59885,#11240);
#8935=LINE('',#59910,#11241);
#8936=LINE('',#59935,#11242);
#8937=LINE('',#59959,#11243);
#8938=LINE('',#59984,#11244);
#8939=LINE('',#60009,#11245);
#8940=LINE('',#60033,#11246);
#8941=LINE('',#60057,#11247);
#8942=LINE('',#60082,#11248);
#8943=LINE('',#60107,#11249);
#8944=LINE('',#60131,#11250);
#8945=LINE('',#60156,#11251);
#8946=LINE('',#60181,#11252);
#8947=LINE('',#60205,#11253);
#8948=LINE('',#60229,#11254);
#8949=LINE('',#60254,#11255);
#8950=LINE('',#60279,#11256);
#8951=LINE('',#60303,#11257);
#8952=LINE('',#60328,#11258);
#8953=LINE('',#60353,#11259);
#8954=LINE('',#60377,#11260);
#8955=LINE('',#60401,#11261);
#8956=LINE('',#60426,#11262);
#8957=LINE('',#60451,#11263);
#8958=LINE('',#60475,#11264);
#8959=LINE('',#60500,#11265);
#8960=LINE('',#60525,#11266);
#8961=LINE('',#60549,#11267);
#8962=LINE('',#60573,#11268);
#8963=LINE('',#60598,#11269);
#8964=LINE('',#60623,#11270);
#8965=LINE('',#60647,#11271);
#8966=LINE('',#60672,#11272);
#8967=LINE('',#60697,#11273);
#8968=LINE('',#60721,#11274);
#8969=LINE('',#60745,#11275);
#8970=LINE('',#60770,#11276);
#8971=LINE('',#60795,#11277);
#8972=LINE('',#60819,#11278);
#8973=LINE('',#60844,#11279);
#8974=LINE('',#60869,#11280);
#8975=LINE('',#60893,#11281);
#8976=LINE('',#60917,#11282);
#8977=LINE('',#60942,#11283);
#8978=LINE('',#60967,#11284);
#8979=LINE('',#60991,#11285);
#8980=LINE('',#61016,#11286);
#8981=LINE('',#61041,#11287);
#8982=LINE('',#61065,#11288);
#8983=LINE('',#64996,#11289);
#8984=LINE('',#64998,#11290);
#8985=LINE('',#65000,#11291);
#8986=LINE('',#65001,#11292);
#8987=LINE('',#65005,#11293);
#8988=LINE('',#65008,#11294);
#8989=LINE('',#65009,#11295);
#8990=LINE('',#65015,#11296);
#8991=LINE('',#65017,#11297);
#8992=LINE('',#65019,#11298);
#8993=LINE('',#65020,#11299);
#8994=LINE('',#65024,#11300);
#8995=LINE('',#65027,#11301);
#8996=LINE('',#65028,#11302);
#8997=LINE('',#65034,#11303);
#8998=LINE('',#65036,#11304);
#8999=LINE('',#65038,#11305);
#9000=LINE('',#65039,#11306);
#9001=LINE('',#65043,#11307);
#9002=LINE('',#65046,#11308);
#9003=LINE('',#65047,#11309);
#9004=LINE('',#65053,#11310);
#9005=LINE('',#65055,#11311);
#9006=LINE('',#65057,#11312);
#9007=LINE('',#65058,#11313);
#9008=LINE('',#65062,#11314);
#9009=LINE('',#65065,#11315);
#9010=LINE('',#65066,#11316);
#9011=LINE('',#65072,#11317);
#9012=LINE('',#65074,#11318);
#9013=LINE('',#65076,#11319);
#9014=LINE('',#65077,#11320);
#9015=LINE('',#65081,#11321);
#9016=LINE('',#65084,#11322);
#9017=LINE('',#65085,#11323);
#9018=LINE('',#65091,#11324);
#9019=LINE('',#65093,#11325);
#9020=LINE('',#65095,#11326);
#9021=LINE('',#65096,#11327);
#9022=LINE('',#65100,#11328);
#9023=LINE('',#65103,#11329);
#9024=LINE('',#65104,#11330);
#9025=LINE('',#65110,#11331);
#9026=LINE('',#65112,#11332);
#9027=LINE('',#65114,#11333);
#9028=LINE('',#65115,#11334);
#9029=LINE('',#65119,#11335);
#9030=LINE('',#65122,#11336);
#9031=LINE('',#65123,#11337);
#9032=LINE('',#65129,#11338);
#9033=LINE('',#65131,#11339);
#9034=LINE('',#65133,#11340);
#9035=LINE('',#65134,#11341);
#9036=LINE('',#65138,#11342);
#9037=LINE('',#65141,#11343);
#9038=LINE('',#65142,#11344);
#9039=LINE('',#65148,#11345);
#9040=LINE('',#65150,#11346);
#9041=LINE('',#65152,#11347);
#9042=LINE('',#65153,#11348);
#9043=LINE('',#65157,#11349);
#9044=LINE('',#65160,#11350);
#9045=LINE('',#65161,#11351);
#9046=LINE('',#65167,#11352);
#9047=LINE('',#65169,#11353);
#9048=LINE('',#65171,#11354);
#9049=LINE('',#65172,#11355);
#9050=LINE('',#65176,#11356);
#9051=LINE('',#65179,#11357);
#9052=LINE('',#65180,#11358);
#9053=LINE('',#65186,#11359);
#9054=LINE('',#65188,#11360);
#9055=LINE('',#65190,#11361);
#9056=LINE('',#65191,#11362);
#9057=LINE('',#65195,#11363);
#9058=LINE('',#65198,#11364);
#9059=LINE('',#65199,#11365);
#9060=LINE('',#65205,#11366);
#9061=LINE('',#65207,#11367);
#9062=LINE('',#65209,#11368);
#9063=LINE('',#65210,#11369);
#9064=LINE('',#65214,#11370);
#9065=LINE('',#65217,#11371);
#9066=LINE('',#65218,#11372);
#9067=LINE('',#65224,#11373);
#9068=LINE('',#65226,#11374);
#9069=LINE('',#65228,#11375);
#9070=LINE('',#65229,#11376);
#9071=LINE('',#65233,#11377);
#9072=LINE('',#65236,#11378);
#9073=LINE('',#65237,#11379);
#9074=LINE('',#65243,#11380);
#9075=LINE('',#65245,#11381);
#9076=LINE('',#65247,#11382);
#9077=LINE('',#65248,#11383);
#9078=LINE('',#65252,#11384);
#9079=LINE('',#65255,#11385);
#9080=LINE('',#65256,#11386);
#9081=LINE('',#65262,#11387);
#9082=LINE('',#65264,#11388);
#9083=LINE('',#65266,#11389);
#9084=LINE('',#65267,#11390);
#9085=LINE('',#65271,#11391);
#9086=LINE('',#65274,#11392);
#9087=LINE('',#65275,#11393);
#9088=LINE('',#65281,#11394);
#9089=LINE('',#65283,#11395);
#9090=LINE('',#65285,#11396);
#9091=LINE('',#65286,#11397);
#9092=LINE('',#65290,#11398);
#9093=LINE('',#65293,#11399);
#9094=LINE('',#65294,#11400);
#9095=LINE('',#65300,#11401);
#9096=LINE('',#65302,#11402);
#9097=LINE('',#65304,#11403);
#9098=LINE('',#65305,#11404);
#9099=LINE('',#65309,#11405);
#9100=LINE('',#65312,#11406);
#9101=LINE('',#65313,#11407);
#9102=LINE('',#65319,#11408);
#9103=LINE('',#65321,#11409);
#9104=LINE('',#65323,#11410);
#9105=LINE('',#65324,#11411);
#9106=LINE('',#65329,#11412);
#9107=LINE('',#65333,#11413);
#9108=LINE('',#65334,#11414);
#9109=LINE('',#65342,#11415);
#9110=LINE('',#65344,#11416);
#9111=LINE('',#65346,#11417);
#9112=LINE('',#65347,#11418);
#9113=LINE('',#65351,#11419);
#9114=LINE('',#65354,#11420);
#9115=LINE('',#65355,#11421);
#9116=LINE('',#65361,#11422);
#9117=LINE('',#65363,#11423);
#9118=LINE('',#65365,#11424);
#9119=LINE('',#65366,#11425);
#9120=LINE('',#65370,#11426);
#9121=LINE('',#65373,#11427);
#9122=LINE('',#65374,#11428);
#9123=LINE('',#65380,#11429);
#9124=LINE('',#65382,#11430);
#9125=LINE('',#65384,#11431);
#9126=LINE('',#65385,#11432);
#9127=LINE('',#65389,#11433);
#9128=LINE('',#65392,#11434);
#9129=LINE('',#65393,#11435);
#9130=LINE('',#65399,#11436);
#9131=LINE('',#65401,#11437);
#9132=LINE('',#65403,#11438);
#9133=LINE('',#65404,#11439);
#9134=LINE('',#65408,#11440);
#9135=LINE('',#65411,#11441);
#9136=LINE('',#65412,#11442);
#9137=LINE('',#65418,#11443);
#9138=LINE('',#65420,#11444);
#9139=LINE('',#65422,#11445);
#9140=LINE('',#65423,#11446);
#9141=LINE('',#65427,#11447);
#9142=LINE('',#65430,#11448);
#9143=LINE('',#65431,#11449);
#9144=LINE('',#65437,#11450);
#9145=LINE('',#65439,#11451);
#9146=LINE('',#65441,#11452);
#9147=LINE('',#65442,#11453);
#9148=LINE('',#65446,#11454);
#9149=LINE('',#65449,#11455);
#9150=LINE('',#65450,#11456);
#9151=LINE('',#65456,#11457);
#9152=LINE('',#65458,#11458);
#9153=LINE('',#65460,#11459);
#9154=LINE('',#65461,#11460);
#9155=LINE('',#65465,#11461);
#9156=LINE('',#65468,#11462);
#9157=LINE('',#65469,#11463);
#9158=LINE('',#65475,#11464);
#9159=LINE('',#65477,#11465);
#9160=LINE('',#65479,#11466);
#9161=LINE('',#65480,#11467);
#9162=LINE('',#65484,#11468);
#9163=LINE('',#65487,#11469);
#9164=LINE('',#65488,#11470);
#9165=LINE('',#65494,#11471);
#9166=LINE('',#65496,#11472);
#9167=LINE('',#65498,#11473);
#9168=LINE('',#65499,#11474);
#9169=LINE('',#65503,#11475);
#9170=LINE('',#65506,#11476);
#9171=LINE('',#65507,#11477);
#9172=LINE('',#65513,#11478);
#9173=LINE('',#65515,#11479);
#9174=LINE('',#65517,#11480);
#9175=LINE('',#65518,#11481);
#9176=LINE('',#65522,#11482);
#9177=LINE('',#65525,#11483);
#9178=LINE('',#65526,#11484);
#9179=LINE('',#65532,#11485);
#9180=LINE('',#65534,#11486);
#9181=LINE('',#65536,#11487);
#9182=LINE('',#65537,#11488);
#9183=LINE('',#65541,#11489);
#9184=LINE('',#65544,#11490);
#9185=LINE('',#65545,#11491);
#9186=LINE('',#65551,#11492);
#9187=LINE('',#65553,#11493);
#9188=LINE('',#65555,#11494);
#9189=LINE('',#65556,#11495);
#9190=LINE('',#65560,#11496);
#9191=LINE('',#65563,#11497);
#9192=LINE('',#65564,#11498);
#9193=LINE('',#65570,#11499);
#9194=LINE('',#65572,#11500);
#9195=LINE('',#65574,#11501);
#9196=LINE('',#65575,#11502);
#9197=LINE('',#65579,#11503);
#9198=LINE('',#65582,#11504);
#9199=LINE('',#65583,#11505);
#9200=LINE('',#65589,#11506);
#9201=LINE('',#65591,#11507);
#9202=LINE('',#65593,#11508);
#9203=LINE('',#65594,#11509);
#9204=LINE('',#65598,#11510);
#9205=LINE('',#65601,#11511);
#9206=LINE('',#65602,#11512);
#9207=LINE('',#65608,#11513);
#9208=LINE('',#65610,#11514);
#9209=LINE('',#65612,#11515);
#9210=LINE('',#65613,#11516);
#9211=LINE('',#65617,#11517);
#9212=LINE('',#65620,#11518);
#9213=LINE('',#65621,#11519);
#9214=LINE('',#65627,#11520);
#9215=LINE('',#65629,#11521);
#9216=LINE('',#65631,#11522);
#9217=LINE('',#65632,#11523);
#9218=LINE('',#65636,#11524);
#9219=LINE('',#65639,#11525);
#9220=LINE('',#65640,#11526);
#9221=LINE('',#65646,#11527);
#9222=LINE('',#65648,#11528);
#9223=LINE('',#65650,#11529);
#9224=LINE('',#65651,#11530);
#9225=LINE('',#65655,#11531);
#9226=LINE('',#65658,#11532);
#9227=LINE('',#65659,#11533);
#9228=LINE('',#65665,#11534);
#9229=LINE('',#65667,#11535);
#9230=LINE('',#65669,#11536);
#9231=LINE('',#65670,#11537);
#9232=LINE('',#65674,#11538);
#9233=LINE('',#65677,#11539);
#9234=LINE('',#65678,#11540);
#9235=LINE('',#65684,#11541);
#9236=LINE('',#65689,#11542);
#9237=LINE('',#65691,#11543);
#9238=LINE('',#65693,#11544);
#9239=LINE('',#65694,#11545);
#9240=LINE('',#65697,#11546);
#9241=LINE('',#65699,#11547);
#9242=LINE('',#65700,#11548);
#9243=LINE('',#65703,#11549);
#9244=LINE('',#65705,#11550);
#9245=LINE('',#65706,#11551);
#9246=LINE('',#65709,#11552);
#9247=LINE('',#65711,#11553);
#9248=LINE('',#65712,#11554);
#9249=LINE('',#65715,#11555);
#9250=LINE('',#65717,#11556);
#9251=LINE('',#65718,#11557);
#9252=LINE('',#65720,#11558);
#9253=LINE('',#65721,#11559);
#9254=LINE('',#65727,#11560);
#9255=LINE('',#65731,#11561);
#9256=LINE('',#65732,#11562);
#9257=LINE('',#65736,#11563);
#9258=LINE('',#65742,#11564);
#9259=LINE('',#65744,#11565);
#9260=LINE('',#65746,#11566);
#9261=LINE('',#65747,#11567);
#9262=LINE('',#65750,#11568);
#9263=LINE('',#65752,#11569);
#9264=LINE('',#65753,#11570);
#9265=LINE('',#65761,#11571);
#9266=LINE('',#65766,#11572);
#9267=LINE('',#65771,#11573);
#9268=LINE('',#65794,#11574);
#9269=LINE('',#65799,#11575);
#9270=LINE('',#65805,#11576);
#9271=LINE('',#65807,#11577);
#9272=LINE('',#65809,#11578);
#9273=LINE('',#65828,#11579);
#9274=LINE('',#65830,#11580);
#9275=LINE('',#65832,#11581);
#9276=LINE('',#65833,#11582);
#9277=LINE('',#65836,#11583);
#9278=LINE('',#65838,#11584);
#9279=LINE('',#65839,#11585);
#9280=LINE('',#65842,#11586);
#9281=LINE('',#65847,#11587);
#9282=LINE('',#65854,#11588);
#9283=LINE('',#65855,#11589);
#9284=LINE('',#65856,#11590);
#9285=LINE('',#65864,#11591);
#9286=LINE('',#65869,#11592);
#9287=LINE('',#65874,#11593);
#9288=LINE('',#65893,#11594);
#9289=LINE('',#65895,#11595);
#9290=LINE('',#65897,#11596);
#9291=LINE('',#65898,#11597);
#9292=LINE('',#65901,#11598);
#9293=LINE('',#65903,#11599);
#9294=LINE('',#65904,#11600);
#9295=LINE('',#65910,#11601);
#9296=LINE('',#65923,#11602);
#9297=LINE('',#65924,#11603);
#9298=LINE('',#65925,#11604);
#9299=LINE('',#65933,#11605);
#9300=LINE('',#65938,#11606);
#9301=LINE('',#65943,#11607);
#9302=LINE('',#65961,#11608);
#9303=LINE('',#65962,#11609);
#9304=LINE('',#65965,#11610);
#9305=LINE('',#65966,#11611);
#9306=LINE('',#65969,#11612);
#9307=LINE('',#65970,#11613);
#9308=LINE('',#65974,#11614);
#9309=LINE('',#65976,#11615);
#9310=LINE('',#65978,#11616);
#9311=LINE('',#65979,#11617);
#9312=LINE('',#65982,#11618);
#9313=LINE('',#65984,#11619);
#9314=LINE('',#65985,#11620);
#9315=LINE('',#65988,#11621);
#9316=LINE('',#65990,#11622);
#9317=LINE('',#65991,#11623);
#9318=LINE('',#65997,#11624);
#9319=LINE('',#66009,#11625);
#9320=LINE('',#66010,#11626);
#9321=LINE('',#66016,#11627);
#9322=LINE('',#66028,#11628);
#9323=LINE('',#66029,#11629);
#9324=LINE('',#66031,#11630);
#9325=LINE('',#66032,#11631);
#9326=LINE('',#66033,#11632);
#9327=LINE('',#66038,#11633);
#9328=LINE('',#66040,#11634);
#9329=LINE('',#66045,#11635);
#9330=LINE('',#66049,#11636);
#9331=LINE('',#66055,#11637);
#9332=LINE('',#66088,#11638);
#9333=LINE('',#66172,#11639);
#9334=LINE('',#66262,#11640);
#9335=LINE('',#66352,#11641);
#9336=LINE('',#66436,#11642);
#9337=LINE('',#66526,#11643);
#9338=LINE('',#66610,#11644);
#9339=LINE('',#66700,#11645);
#9340=LINE('',#66790,#11646);
#9341=LINE('',#66874,#11647);
#9342=LINE('',#66964,#11648);
#9343=LINE('',#67048,#11649);
#9344=LINE('',#67138,#11650);
#9345=LINE('',#67228,#11651);
#9346=LINE('',#67312,#11652);
#9347=LINE('',#67402,#11653);
#9348=LINE('',#67412,#11654);
#9349=LINE('',#67449,#11655);
#9350=LINE('',#67486,#11656);
#9351=LINE('',#67523,#11657);
#9352=LINE('',#67561,#11658);
#9353=LINE('',#67598,#11659);
#9354=LINE('',#67635,#11660);
#9355=LINE('',#67672,#11661);
#9356=LINE('',#67709,#11662);
#9357=LINE('',#67747,#11663);
#9358=LINE('',#67784,#11664);
#9359=LINE('',#67821,#11665);
#9360=LINE('',#67858,#11666);
#9361=LINE('',#67895,#11667);
#9362=LINE('',#67933,#11668);
#9363=LINE('',#67971,#11669);
#9364=LINE('',#67980,#11670);
#9365=LINE('',#67997,#11671);
#9366=LINE('',#68009,#11672);
#9367=LINE('',#68015,#11673);
#9368=LINE('',#68130,#11674);
#9369=LINE('',#68190,#11675);
#9370=LINE('',#68197,#11676);
#9371=LINE('',#70370,#11677);
#9372=LINE('',#70377,#11678);
#9373=LINE('',#70381,#11679);
#9374=LINE('',#70388,#11680);
#9375=LINE('',#70390,#11681);
#9376=LINE('',#70395,#11682);
#9377=LINE('',#70422,#11683);
#9378=LINE('',#70470,#11684);
#9379=LINE('',#70518,#11685);
#9380=LINE('',#70566,#11686);
#9381=LINE('',#70620,#11687);
#9382=LINE('',#70668,#11688);
#9383=LINE('',#70716,#11689);
#9384=LINE('',#70770,#11690);
#9385=LINE('',#70818,#11691);
#9386=LINE('',#70866,#11692);
#9387=LINE('',#70917,#11693);
#9388=LINE('',#70968,#11694);
#9389=LINE('',#71016,#11695);
#9390=LINE('',#71064,#11696);
#9391=LINE('',#71118,#11697);
#9392=LINE('',#71166,#11698);
#9393=LINE('',#71214,#11699);
#9394=LINE('',#71265,#11700);
#9395=LINE('',#71313,#11701);
#9396=LINE('',#71361,#11702);
#9397=LINE('',#71409,#11703);
#9398=LINE('',#71463,#11704);
#9399=LINE('',#71511,#11705);
#9400=LINE('',#71559,#11706);
#9401=LINE('',#71613,#11707);
#9402=LINE('',#71661,#11708);
#9403=LINE('',#71709,#11709);
#9404=LINE('',#71757,#11710);
#9405=LINE('',#71811,#11711);
#9406=LINE('',#71859,#11712);
#9407=LINE('',#71907,#11713);
#9408=LINE('',#71961,#11714);
#9409=LINE('',#72009,#11715);
#9410=LINE('',#72057,#11716);
#9411=LINE('',#72105,#11717);
#9412=LINE('',#72159,#11718);
#9413=LINE('',#72207,#11719);
#9414=LINE('',#72255,#11720);
#9415=LINE('',#72309,#11721);
#9416=LINE('',#72357,#11722);
#9417=LINE('',#72405,#11723);
#9418=LINE('',#72453,#11724);
#9419=LINE('',#72507,#11725);
#9420=LINE('',#72555,#11726);
#9421=LINE('',#72603,#11727);
#9422=LINE('',#72657,#11728);
#9423=LINE('',#72705,#11729);
#9424=LINE('',#72753,#11730);
#9425=LINE('',#72801,#11731);
#9426=LINE('',#72855,#11732);
#9427=LINE('',#72903,#11733);
#9428=LINE('',#72951,#11734);
#9429=LINE('',#73005,#11735);
#9430=LINE('',#73053,#11736);
#9431=LINE('',#73101,#11737);
#9432=LINE('',#73149,#11738);
#9433=LINE('',#73203,#11739);
#9434=LINE('',#73251,#11740);
#9435=LINE('',#73299,#11741);
#9436=LINE('',#73353,#11742);
#9437=LINE('',#73401,#11743);
#9438=LINE('',#73449,#11744);
#9439=LINE('',#73500,#11745);
#9440=LINE('',#73551,#11746);
#9441=LINE('',#73599,#11747);
#9442=LINE('',#73647,#11748);
#9443=LINE('',#73701,#11749);
#9444=LINE('',#73749,#11750);
#9445=LINE('',#73797,#11751);
#9446=LINE('',#73848,#11752);
#9447=LINE('',#73896,#11753);
#9448=LINE('',#73944,#11754);
#9449=LINE('',#73992,#11755);
#9450=LINE('',#74046,#11756);
#9451=LINE('',#74094,#11757);
#9452=LINE('',#74110,#11758);
#9453=LINE('',#74135,#11759);
#9454=LINE('',#74160,#11760);
#9455=LINE('',#74185,#11761);
#9456=LINE('',#74209,#11762);
#9457=LINE('',#74233,#11763);
#9458=LINE('',#74258,#11764);
#9459=LINE('',#74283,#11765);
#9460=LINE('',#74307,#11766);
#9461=LINE('',#74332,#11767);
#9462=LINE('',#74357,#11768);
#9463=LINE('',#74381,#11769);
#9464=LINE('',#74406,#11770);
#9465=LINE('',#74430,#11771);
#9466=LINE('',#74455,#11772);
#9467=LINE('',#74479,#11773);
#9468=LINE('',#74504,#11774);
#9469=LINE('',#74529,#11775);
#9470=LINE('',#74553,#11776);
#9471=LINE('',#74578,#11777);
#9472=LINE('',#74603,#11778);
#9473=LINE('',#74627,#11779);
#9474=LINE('',#74651,#11780);
#9475=LINE('',#74676,#11781);
#9476=LINE('',#74701,#11782);
#9477=LINE('',#74725,#11783);
#9478=LINE('',#74750,#11784);
#9479=LINE('',#74775,#11785);
#9480=LINE('',#74799,#11786);
#9481=LINE('',#74823,#11787);
#9482=LINE('',#74848,#11788);
#9483=LINE('',#74873,#11789);
#9484=LINE('',#74897,#11790);
#9485=LINE('',#74922,#11791);
#9486=LINE('',#74947,#11792);
#9487=LINE('',#74971,#11793);
#9488=LINE('',#74995,#11794);
#9489=LINE('',#75020,#11795);
#9490=LINE('',#75045,#11796);
#9491=LINE('',#75069,#11797);
#9492=LINE('',#75094,#11798);
#9493=LINE('',#75119,#11799);
#9494=LINE('',#75143,#11800);
#9495=LINE('',#75167,#11801);
#9496=LINE('',#75192,#11802);
#9497=LINE('',#75217,#11803);
#9498=LINE('',#75241,#11804);
#9499=LINE('',#75266,#11805);
#9500=LINE('',#75291,#11806);
#9501=LINE('',#75315,#11807);
#9502=LINE('',#75339,#11808);
#9503=LINE('',#75364,#11809);
#9504=LINE('',#75389,#11810);
#9505=LINE('',#75413,#11811);
#9506=LINE('',#75438,#11812);
#9507=LINE('',#75463,#11813);
#9508=LINE('',#75487,#11814);
#9509=LINE('',#75511,#11815);
#9510=LINE('',#75536,#11816);
#9511=LINE('',#75561,#11817);
#9512=LINE('',#75585,#11818);
#9513=LINE('',#75610,#11819);
#9514=LINE('',#75635,#11820);
#9515=LINE('',#75659,#11821);
#9516=LINE('',#75684,#11822);
#9517=LINE('',#75708,#11823);
#9518=LINE('',#75733,#11824);
#9519=LINE('',#75757,#11825);
#9520=LINE('',#75782,#11826);
#9521=LINE('',#75807,#11827);
#9522=LINE('',#75831,#11828);
#9523=LINE('',#75856,#11829);
#9524=LINE('',#75881,#11830);
#9525=LINE('',#75905,#11831);
#9526=LINE('',#80248,#11832);
#9527=LINE('',#80251,#11833);
#9528=LINE('',#80257,#11834);
#9529=LINE('',#80268,#11835);
#9530=LINE('',#80275,#11836);
#9531=LINE('',#80286,#11837);
#9532=LINE('',#80288,#11838);
#9533=LINE('',#80289,#11839);
#9534=LINE('',#80294,#11840);
#9535=LINE('',#80316,#11841);
#9536=LINE('',#80317,#11842);
#9537=LINE('',#80337,#11843);
#9538=LINE('',#80341,#11844);
#9539=LINE('',#80345,#11845);
#9540=LINE('',#80349,#11846);
#9541=LINE('',#80353,#11847);
#9542=LINE('',#80357,#11848);
#9543=LINE('',#80361,#11849);
#9544=LINE('',#80365,#11850);
#9545=LINE('',#80369,#11851);
#9546=LINE('',#80373,#11852);
#9547=LINE('',#80377,#11853);
#9548=LINE('',#80381,#11854);
#9549=LINE('',#80385,#11855);
#9550=LINE('',#80389,#11856);
#9551=LINE('',#80393,#11857);
#9552=LINE('',#80398,#11858);
#9553=LINE('',#80402,#11859);
#9554=LINE('',#80406,#11860);
#9555=LINE('',#80410,#11861);
#9556=LINE('',#80414,#11862);
#9557=LINE('',#80418,#11863);
#9558=LINE('',#80422,#11864);
#9559=LINE('',#80426,#11865);
#9560=LINE('',#80430,#11866);
#9561=LINE('',#80434,#11867);
#9562=LINE('',#80438,#11868);
#9563=LINE('',#80442,#11869);
#9564=LINE('',#80446,#11870);
#9565=LINE('',#80449,#11871);
#9566=LINE('',#80453,#11872);
#9567=LINE('',#80454,#11873);
#9568=LINE('',#80459,#11874);
#9569=LINE('',#80472,#11875);
#9570=LINE('',#80488,#11876);
#9571=LINE('',#80489,#11877);
#9572=LINE('',#80494,#11878);
#9573=LINE('',#80507,#11879);
#9574=LINE('',#80523,#11880);
#9575=LINE('',#80524,#11881);
#9576=LINE('',#80529,#11882);
#9577=LINE('',#80542,#11883);
#9578=LINE('',#80558,#11884);
#9579=LINE('',#80559,#11885);
#9580=LINE('',#80564,#11886);
#9581=LINE('',#80577,#11887);
#9582=LINE('',#80593,#11888);
#9583=LINE('',#80594,#11889);
#9584=LINE('',#80599,#11890);
#9585=LINE('',#80612,#11891);
#9586=LINE('',#80628,#11892);
#9587=LINE('',#80629,#11893);
#9588=LINE('',#80634,#11894);
#9589=LINE('',#80647,#11895);
#9590=LINE('',#80663,#11896);
#9591=LINE('',#80664,#11897);
#9592=LINE('',#80669,#11898);
#9593=LINE('',#80682,#11899);
#9594=LINE('',#80698,#11900);
#9595=LINE('',#80699,#11901);
#9596=LINE('',#80704,#11902);
#9597=LINE('',#80717,#11903);
#9598=LINE('',#80733,#11904);
#9599=LINE('',#80734,#11905);
#9600=LINE('',#80739,#11906);
#9601=LINE('',#80752,#11907);
#9602=LINE('',#80768,#11908);
#9603=LINE('',#80769,#11909);
#9604=LINE('',#80774,#11910);
#9605=LINE('',#80787,#11911);
#9606=LINE('',#80803,#11912);
#9607=LINE('',#80804,#11913);
#9608=LINE('',#80809,#11914);
#9609=LINE('',#80822,#11915);
#9610=LINE('',#80838,#11916);
#9611=LINE('',#80839,#11917);
#9612=LINE('',#80844,#11918);
#9613=LINE('',#80857,#11919);
#9614=LINE('',#80873,#11920);
#9615=LINE('',#80874,#11921);
#9616=LINE('',#80879,#11922);
#9617=LINE('',#80892,#11923);
#9618=LINE('',#80908,#11924);
#9619=LINE('',#80909,#11925);
#9620=LINE('',#80914,#11926);
#9621=LINE('',#80927,#11927);
#9622=LINE('',#80931,#11928);
#9623=LINE('',#80933,#11929);
#9624=LINE('',#80935,#11930);
#9625=LINE('',#80936,#11931);
#9626=LINE('',#80939,#11932);
#9627=LINE('',#80941,#11933);
#9628=LINE('',#80942,#11934);
#9629=LINE('',#80946,#11935);
#9630=LINE('',#80948,#11936);
#9631=LINE('',#80950,#11937);
#9632=LINE('',#80951,#11938);
#9633=LINE('',#80954,#11939);
#9634=LINE('',#80956,#11940);
#9635=LINE('',#80957,#11941);
#9636=LINE('',#80959,#11942);
#9637=LINE('',#80960,#11943);
#9638=LINE('',#80962,#11944);
#9639=LINE('',#80963,#11945);
#9640=LINE('',#80966,#11946);
#9641=LINE('',#80968,#11947);
#9642=LINE('',#80969,#11948);
#9643=LINE('',#80972,#11949);
#9644=LINE('',#80973,#11950);
#9645=LINE('',#80976,#11951);
#9646=LINE('',#80977,#11952);
#9647=LINE('',#80982,#11953);
#9648=LINE('',#80983,#11954);
#9649=LINE('',#80986,#11955);
#9650=LINE('',#80987,#11956);
#9651=LINE('',#80989,#11957);
#9652=LINE('',#81010,#11958);
#9653=LINE('',#81014,#11959);
#9654=LINE('',#81019,#11960);
#9655=LINE('',#81025,#11961);
#9656=LINE('',#81049,#11962);
#9657=LINE('',#81097,#11963);
#9658=LINE('',#81145,#11964);
#9659=LINE('',#81199,#11965);
#9660=LINE('',#81247,#11966);
#9661=LINE('',#81295,#11967);
#9662=LINE('',#81343,#11968);
#9663=LINE('',#81369,#11969);
#9664=LINE('',#81393,#11970);
#9665=LINE('',#81417,#11971);
#9666=LINE('',#81442,#11972);
#9667=LINE('',#81467,#11973);
#9668=LINE('',#82261,#11974);
#9669=LINE('',#82263,#11975);
#9670=LINE('',#82265,#11976);
#9671=LINE('',#82266,#11977);
#9672=LINE('',#82269,#11978);
#9673=LINE('',#82271,#11979);
#9674=LINE('',#82272,#11980);
#9675=LINE('',#82275,#11981);
#9676=LINE('',#82277,#11982);
#9677=LINE('',#82278,#11983);
#9678=LINE('',#82281,#11984);
#9679=LINE('',#82283,#11985);
#9680=LINE('',#82284,#11986);
#9681=LINE('',#82287,#11987);
#9682=LINE('',#82289,#11988);
#9683=LINE('',#82290,#11989);
#9684=LINE('',#82292,#11990);
#9685=LINE('',#82293,#11991);
#9686=LINE('',#82299,#11992);
#9687=LINE('',#82305,#11993);
#9688=VECTOR('',#33419,10.);
#9689=VECTOR('',#33420,10.);
#9690=VECTOR('',#33421,10.);
#9691=VECTOR('',#33422,10.);
#9692=VECTOR('',#33423,10.);
#9693=VECTOR('',#33424,10.);
#9694=VECTOR('',#33427,10.);
#9695=VECTOR('',#33428,10.);
#9696=VECTOR('',#33429,10.);
#9697=VECTOR('',#33432,10.);
#9698=VECTOR('',#33433,10.);
#9699=VECTOR('',#33434,10.);
#9700=VECTOR('',#33435,10.);
#9701=VECTOR('',#33438,10.);
#9702=VECTOR('',#33439,10.);
#9703=VECTOR('',#33440,10.);
#9704=VECTOR('',#33443,10.);
#9705=VECTOR('',#33444,10.);
#9706=VECTOR('',#33445,10.);
#9707=VECTOR('',#33446,10.);
#9708=VECTOR('',#33449,10.);
#9709=VECTOR('',#33450,10.);
#9710=VECTOR('',#33451,10.);
#9711=VECTOR('',#33454,10.);
#9712=VECTOR('',#33455,10.);
#9713=VECTOR('',#33456,10.);
#9714=VECTOR('',#33457,10.);
#9715=VECTOR('',#33460,10.);
#9716=VECTOR('',#33461,10.);
#9717=VECTOR('',#33462,10.);
#9718=VECTOR('',#33463,10.);
#9719=VECTOR('',#33464,10.);
#9720=VECTOR('',#33465,10.);
#9721=VECTOR('',#33466,10.);
#9722=VECTOR('',#33467,10.);
#9723=VECTOR('',#33468,10.);
#9724=VECTOR('',#33469,10.);
#9725=VECTOR('',#33470,10.);
#9726=VECTOR('',#33471,10.);
#9727=VECTOR('',#33472,10.);
#9728=VECTOR('',#33473,10.);
#9729=VECTOR('',#33474,10.);
#9730=VECTOR('',#33475,10.);
#9731=VECTOR('',#33476,10.);
#9732=VECTOR('',#33477,10.);
#9733=VECTOR('',#33478,10.);
#9734=VECTOR('',#33479,10.);
#9735=VECTOR('',#33480,10.);
#9736=VECTOR('',#33481,10.);
#9737=VECTOR('',#33482,10.);
#9738=VECTOR('',#33483,10.);
#9739=VECTOR('',#33484,10.);
#9740=VECTOR('',#33485,10.);
#9741=VECTOR('',#33486,10.);
#9742=VECTOR('',#33487,10.);
#9743=VECTOR('',#33488,10.);
#9744=VECTOR('',#33489,10.);
#9745=VECTOR('',#33490,10.);
#9746=VECTOR('',#33491,10.);
#9747=VECTOR('',#33492,10.);
#9748=VECTOR('',#33493,10.);
#9749=VECTOR('',#33494,10.);
#9750=VECTOR('',#33495,10.);
#9751=VECTOR('',#33496,10.);
#9752=VECTOR('',#33497,10.);
#9753=VECTOR('',#33498,10.);
#9754=VECTOR('',#33499,10.);
#9755=VECTOR('',#33500,10.);
#9756=VECTOR('',#33501,10.);
#9757=VECTOR('',#33502,10.);
#9758=VECTOR('',#33503,10.);
#9759=VECTOR('',#33504,10.);
#9760=VECTOR('',#33505,10.);
#9761=VECTOR('',#33506,10.);
#9762=VECTOR('',#33507,10.);
#9763=VECTOR('',#33508,10.);
#9764=VECTOR('',#33509,10.);
#9765=VECTOR('',#33512,10.);
#9766=VECTOR('',#33513,10.);
#9767=VECTOR('',#33514,10.);
#9768=VECTOR('',#33515,10.);
#9769=VECTOR('',#33518,10.);
#9770=VECTOR('',#33519,10.);
#9771=VECTOR('',#33520,10.);
#9772=VECTOR('',#33525,1.8);
#9773=VECTOR('',#33530,10.);
#9774=VECTOR('',#33531,10.);
#9775=VECTOR('',#33532,10.);
#9776=VECTOR('',#33533,10.);
#9777=VECTOR('',#33538,1.55);
#9778=VECTOR('',#33543,1.8);
#9779=VECTOR('',#33548,1.55);
#9780=VECTOR('',#33555,4.75);
#9781=VECTOR('',#33560,4.5);
#9782=VECTOR('',#33571,4.75);
#9783=VECTOR('',#33576,4.5);
#9784=VECTOR('',#33587,4.75);
#9785=VECTOR('',#33592,4.5);
#9786=VECTOR('',#33603,4.75);
#9787=VECTOR('',#33608,4.5);
#9788=VECTOR('',#33617,10.);
#9789=VECTOR('',#33618,10.);
#9790=VECTOR('',#33621,10.);
#9791=VECTOR('',#33622,10.);
#9792=VECTOR('',#33623,10.);
#9793=VECTOR('',#33626,10.);
#9794=VECTOR('',#33627,10.);
#9795=VECTOR('',#33630,10.);
#9796=VECTOR('',#33631,10.);
#9797=VECTOR('',#33632,10.);
#9798=VECTOR('',#33635,10.);
#9799=VECTOR('',#33636,10.);
#9800=VECTOR('',#33637,10.);
#9801=VECTOR('',#33640,10.);
#9802=VECTOR('',#33641,10.);
#9803=VECTOR('',#33642,10.);
#9804=VECTOR('',#33645,10.);
#9805=VECTOR('',#33646,10.);
#9806=VECTOR('',#33649,10.);
#9807=VECTOR('',#33652,10.);
#9808=VECTOR('',#33655,10.);
#9809=VECTOR('',#33656,10.);
#9810=VECTOR('',#33659,10.);
#9811=VECTOR('',#33660,10.);
#9812=VECTOR('',#33663,10.);
#9813=VECTOR('',#33666,10.);
#9814=VECTOR('',#33667,10.);
#9815=VECTOR('',#33722,10.);
#9816=VECTOR('',#33723,10.);
#9817=VECTOR('',#33724,10.);
#9818=VECTOR('',#33727,10.);
#9819=VECTOR('',#33728,10.);
#9820=VECTOR('',#33731,10.);
#9821=VECTOR('',#33732,10.);
#9822=VECTOR('',#33735,10.);
#9823=VECTOR('',#33736,10.);
#9824=VECTOR('',#33739,10.);
#9825=VECTOR('',#33740,10.);
#9826=VECTOR('',#33743,10.);
#9827=VECTOR('',#33744,10.);
#9828=VECTOR('',#33747,10.);
#9829=VECTOR('',#33748,10.);
#9830=VECTOR('',#33751,10.);
#9831=VECTOR('',#33752,10.);
#9832=VECTOR('',#33755,10.);
#9833=VECTOR('',#33756,10.);
#9834=VECTOR('',#33759,10.);
#9835=VECTOR('',#33760,10.);
#9836=VECTOR('',#33763,10.);
#9837=VECTOR('',#33764,10.);
#9838=VECTOR('',#33767,10.);
#9839=VECTOR('',#33772,10.);
#9840=VECTOR('',#33773,10.);
#9841=VECTOR('',#33774,10.);
#9842=VECTOR('',#33775,10.);
#9843=VECTOR('',#33776,10.);
#9844=VECTOR('',#33777,10.);
#9845=VECTOR('',#33778,10.);
#9846=VECTOR('',#33781,10.);
#9847=VECTOR('',#33782,10.);
#9848=VECTOR('',#33785,10.);
#9849=VECTOR('',#33786,10.);
#9850=VECTOR('',#33789,10.);
#9851=VECTOR('',#33790,10.);
#9852=VECTOR('',#33791,10.);
#9853=VECTOR('',#33792,10.);
#9854=VECTOR('',#33793,10.);
#9855=VECTOR('',#33794,10.);
#9856=VECTOR('',#33795,10.);
#9857=VECTOR('',#33796,10.);
#9858=VECTOR('',#33797,10.);
#9859=VECTOR('',#33800,10.);
#9860=VECTOR('',#33801,10.);
#9861=VECTOR('',#33804,10.);
#9862=VECTOR('',#33805,10.);
#9863=VECTOR('',#33808,10.);
#9864=VECTOR('',#33809,10.);
#9865=VECTOR('',#33812,10.);
#9866=VECTOR('',#33817,10.);
#9867=VECTOR('',#33818,10.);
#9868=VECTOR('',#33819,10.);
#9869=VECTOR('',#33822,10.);
#9870=VECTOR('',#33823,10.);
#9871=VECTOR('',#33826,10.);
#9872=VECTOR('',#33827,10.);
#9873=VECTOR('',#33830,10.);
#9874=VECTOR('',#33831,10.);
#9875=VECTOR('',#33834,10.);
#9876=VECTOR('',#33835,10.);
#9877=VECTOR('',#33838,10.);
#9878=VECTOR('',#33839,10.);
#9879=VECTOR('',#33842,10.);
#9880=VECTOR('',#33843,10.);
#9881=VECTOR('',#33846,10.);
#9882=VECTOR('',#33847,10.);
#9883=VECTOR('',#33850,10.);
#9884=VECTOR('',#33851,10.);
#9885=VECTOR('',#33854,10.);
#9886=VECTOR('',#33855,10.);
#9887=VECTOR('',#33858,10.);
#9888=VECTOR('',#33859,10.);
#9889=VECTOR('',#33862,10.);
#9890=VECTOR('',#33865,10.);
#9891=VECTOR('',#33866,10.);
#9892=VECTOR('',#33867,10.);
#9893=VECTOR('',#33870,10.);
#9894=VECTOR('',#33871,10.);
#9895=VECTOR('',#33872,10.);
#9896=VECTOR('',#33873,10.);
#9897=VECTOR('',#33874,10.);
#9898=VECTOR('',#33877,10.);
#9899=VECTOR('',#33878,10.);
#9900=VECTOR('',#33881,10.);
#9901=VECTOR('',#33882,10.);
#9902=VECTOR('',#33885,10.);
#9903=VECTOR('',#33886,10.);
#9904=VECTOR('',#33889,10.);
#9905=VECTOR('',#33890,10.);
#9906=VECTOR('',#33893,10.);
#9907=VECTOR('',#33894,10.);
#9908=VECTOR('',#33895,10.);
#9909=VECTOR('',#33896,10.);
#9910=VECTOR('',#33897,10.);
#9911=VECTOR('',#33898,10.);
#9912=VECTOR('',#33899,10.);
#9913=VECTOR('',#33900,10.);
#9914=VECTOR('',#33901,10.);
#9915=VECTOR('',#33902,10.);
#9916=VECTOR('',#33903,10.);
#9917=VECTOR('',#33904,10.);
#9918=VECTOR('',#33905,10.);
#9919=VECTOR('',#33906,10.);
#9920=VECTOR('',#33909,10.);
#9921=VECTOR('',#33910,10.);
#9922=VECTOR('',#33911,10.);
#9923=VECTOR('',#33912,10.);
#9924=VECTOR('',#33913,10.);
#9925=VECTOR('',#33914,10.);
#9926=VECTOR('',#33915,10.);
#9927=VECTOR('',#33916,10.);
#9928=VECTOR('',#33917,10.);
#9929=VECTOR('',#33918,10.);
#9930=VECTOR('',#33919,10.);
#9931=VECTOR('',#33920,10.);
#9932=VECTOR('',#33921,10.);
#9933=VECTOR('',#33922,10.);
#9934=VECTOR('',#33923,10.);
#9935=VECTOR('',#33924,10.);
#9936=VECTOR('',#33925,10.);
#9937=VECTOR('',#33926,10.);
#9938=VECTOR('',#33927,10.);
#9939=VECTOR('',#33928,10.);
#9940=VECTOR('',#33931,10.);
#9941=VECTOR('',#33932,10.);
#9942=VECTOR('',#33933,10.);
#9943=VECTOR('',#33936,10.);
#9944=VECTOR('',#33937,10.);
#9945=VECTOR('',#33938,10.);
#9946=VECTOR('',#33939,10.);
#9947=VECTOR('',#33940,10.);
#9948=VECTOR('',#33941,10.);
#9949=VECTOR('',#33942,10.);
#9950=VECTOR('',#33943,10.);
#9951=VECTOR('',#33944,10.);
#9952=VECTOR('',#33945,10.);
#9953=VECTOR('',#33946,10.);
#9954=VECTOR('',#33947,10.);
#9955=VECTOR('',#33950,10.);
#9956=VECTOR('',#33951,10.);
#9957=VECTOR('',#33952,10.);
#9958=VECTOR('',#33953,10.);
#9959=VECTOR('',#33954,10.);
#9960=VECTOR('',#33955,10.);
#9961=VECTOR('',#33956,10.);
#9962=VECTOR('',#33957,10.);
#9963=VECTOR('',#33958,10.);
#9964=VECTOR('',#33961,10.);
#9965=VECTOR('',#33962,10.);
#9966=VECTOR('',#33963,10.);
#9967=VECTOR('',#33964,10.);
#9968=VECTOR('',#33965,10.);
#9969=VECTOR('',#33966,10.);
#9970=VECTOR('',#33967,10.);
#9971=VECTOR('',#33968,10.);
#9972=VECTOR('',#33969,10.);
#9973=VECTOR('',#33972,10.);
#9974=VECTOR('',#33973,10.);
#9975=VECTOR('',#33974,10.);
#9976=VECTOR('',#33979,10.);
#9977=VECTOR('',#33980,10.);
#9978=VECTOR('',#33981,10.);
#9979=VECTOR('',#33984,10.);
#9980=VECTOR('',#33985,10.);
#9981=VECTOR('',#33988,10.);
#9982=VECTOR('',#33989,10.);
#9983=VECTOR('',#33992,10.);
#9984=VECTOR('',#33995,10.);
#9985=VECTOR('',#33996,10.);
#9986=VECTOR('',#33997,10.);
#9987=VECTOR('',#33998,10.);
#9988=VECTOR('',#33999,10.);
#9989=VECTOR('',#34000,10.);
#9990=VECTOR('',#34001,10.);
#9991=VECTOR('',#34002,10.);
#9992=VECTOR('',#34003,10.);
#9993=VECTOR('',#34004,10.);
#9994=VECTOR('',#34005,10.);
#9995=VECTOR('',#34006,10.);
#9996=VECTOR('',#34007,10.);
#9997=VECTOR('',#34008,10.);
#9998=VECTOR('',#34011,10.);
#9999=VECTOR('',#34012,10.);
#10000=VECTOR('',#34013,10.);
#10001=VECTOR('',#34014,10.);
#10002=VECTOR('',#34015,10.);
#10003=VECTOR('',#34016,10.);
#10004=VECTOR('',#34017,10.);
#10005=VECTOR('',#34018,10.);
#10006=VECTOR('',#34019,10.);
#10007=VECTOR('',#34020,10.);
#10008=VECTOR('',#34021,10.);
#10009=VECTOR('',#34022,10.);
#10010=VECTOR('',#34023,10.);
#10011=VECTOR('',#34024,10.);
#10012=VECTOR('',#34025,10.);
#10013=VECTOR('',#34026,10.);
#10014=VECTOR('',#34027,10.);
#10015=VECTOR('',#34028,10.);
#10016=VECTOR('',#34029,10.);
#10017=VECTOR('',#34030,10.);
#10018=VECTOR('',#34033,10.);
#10019=VECTOR('',#34034,10.);
#10020=VECTOR('',#34035,10.);
#10021=VECTOR('',#34040,4.25);
#10022=VECTOR('',#34047,4.05);
#10023=VECTOR('',#34050,3.25);
#10024=VECTOR('',#34055,3.05);
#10025=VECTOR('',#34060,3.25);
#10026=VECTOR('',#34065,3.05);
#10027=VECTOR('',#34070,3.25);
#10028=VECTOR('',#34075,3.05);
#10029=VECTOR('',#34080,3.25);
#10030=VECTOR('',#34085,3.05000000000001);
#10031=VECTOR('',#34090,3.25);
#10032=VECTOR('',#34095,3.05);
#10033=VECTOR('',#34100,3.25);
#10034=VECTOR('',#34105,3.05000000000001);
#10035=VECTOR('',#34110,3.25);
#10036=VECTOR('',#34115,3.05);
#10037=VECTOR('',#34120,3.25);
#10038=VECTOR('',#34125,3.05);
#10039=VECTOR('',#34130,3.25);
#10040=VECTOR('',#34135,3.05000000000001);
#10041=VECTOR('',#34140,3.25);
#10042=VECTOR('',#34145,3.05);
#10043=VECTOR('',#34150,3.25);
#10044=VECTOR('',#34155,3.05000000000001);
#10045=VECTOR('',#34160,3.25);
#10046=VECTOR('',#34165,3.05);
#10047=VECTOR('',#34170,7.2);
#10048=VECTOR('',#34175,7.);
#10049=VECTOR('',#34178,7.2);
#10050=VECTOR('',#34183,7.);
#10051=VECTOR('',#34186,7.2);
#10052=VECTOR('',#34191,7.);
#10053=VECTOR('',#34194,7.2);
#10054=VECTOR('',#34199,7.);
#10055=VECTOR('',#34202,4.7);
#10056=VECTOR('',#34205,4.7);
#10057=VECTOR('',#34208,4.7);
#10058=VECTOR('',#34211,4.7);
#10059=VECTOR('',#34242,5.5);
#10060=VECTOR('',#34255,2.3);
#10061=VECTOR('',#34260,10.);
#10062=VECTOR('',#34261,10.);
#10063=VECTOR('',#34264,10.);
#10064=VECTOR('',#34267,10.);
#10065=VECTOR('',#34270,10.);
#10066=VECTOR('',#34273,10.);
#10067=VECTOR('',#34276,10.);
#10068=VECTOR('',#34279,10.);
#10069=VECTOR('',#34282,10.);
#10070=VECTOR('',#34285,10.);
#10071=VECTOR('',#34288,10.);
#10072=VECTOR('',#34291,10.);
#10073=VECTOR('',#34294,10.);
#10074=VECTOR('',#34317,2.05);
#10075=VECTOR('',#34322,2.3);
#10076=VECTOR('',#34327,2.05);
#10077=VECTOR('',#34332,10.);
#10078=VECTOR('',#34333,10.);
#10079=VECTOR('',#34334,10.);
#10080=VECTOR('',#34339,10.);
#10081=VECTOR('',#34342,10.);
#10082=VECTOR('',#34343,10.);
#10083=VECTOR('',#34348,10.);
#10084=VECTOR('',#34351,10.);
#10085=VECTOR('',#34352,10.);
#10086=VECTOR('',#34359,10.);
#10087=VECTOR('',#34360,10.);
#10088=VECTOR('',#34361,10.);
#10089=VECTOR('',#34364,10.);
#10090=VECTOR('',#34367,10.);
#10091=VECTOR('',#34368,10.);
#10092=VECTOR('',#34369,10.);
#10093=VECTOR('',#34370,10.);
#10094=VECTOR('',#34373,10.);
#10095=VECTOR('',#34380,10.);
#10096=VECTOR('',#34381,10.);
#10097=VECTOR('',#34382,10.);
#10098=VECTOR('',#34385,10.);
#10099=VECTOR('',#34392,10.);
#10100=VECTOR('',#34393,10.);
#10101=VECTOR('',#34402,10.);
#10102=VECTOR('',#34403,10.);
#10103=VECTOR('',#34406,10.);
#10104=VECTOR('',#34411,10.);
#10105=VECTOR('',#34414,10.);
#10106=VECTOR('',#34415,10.);
#10107=VECTOR('',#34416,10.);
#10108=VECTOR('',#34419,10.);
#10109=VECTOR('',#34420,10.);
#10110=VECTOR('',#34421,10.);
#10111=VECTOR('',#34426,12.25);
#10112=VECTOR('',#34431,10.);
#10113=VECTOR('',#34434,10.);
#10114=VECTOR('',#34437,10.);
#10115=VECTOR('',#34440,10.);
#10116=VECTOR('',#34443,10.);
#10117=VECTOR('',#34446,10.);
#10118=VECTOR('',#34449,10.);
#10119=VECTOR('',#34462,12.);
#10120=VECTOR('',#34465,12.25);
#10121=VECTOR('',#34472,12.);
#10122=VECTOR('',#34475,12.25);
#10123=VECTOR('',#34482,12.);
#10124=VECTOR('',#34485,10.);
#10125=VECTOR('',#34490,10.);
#10126=VECTOR('',#34491,10.);
#10127=VECTOR('',#34494,10.);
#10128=VECTOR('',#34499,10.);
#10129=VECTOR('',#34500,10.);
#10130=VECTOR('',#34503,10.);
#10131=VECTOR('',#34508,10.);
#10132=VECTOR('',#34509,10.);
#10133=VECTOR('',#34512,10.);
#10134=VECTOR('',#34517,10.);
#10135=VECTOR('',#34518,10.);
#10136=VECTOR('',#34521,10.);
#10137=VECTOR('',#34526,10.);
#10138=VECTOR('',#34527,10.);
#10139=VECTOR('',#34534,10.);
#10140=VECTOR('',#34535,10.);
#10141=VECTOR('',#34538,10.);
#10142=VECTOR('',#34539,10.);
#10143=VECTOR('',#34540,10.);
#10144=VECTOR('',#34541,10.);
#10145=VECTOR('',#34544,10.);
#10146=VECTOR('',#34551,10.);
#10147=VECTOR('',#34552,10.);
#10148=VECTOR('',#34553,10.);
#10149=VECTOR('',#34556,10.);
#10150=VECTOR('',#34563,10.);
#10151=VECTOR('',#34564,10.);
#10152=VECTOR('',#34565,10.);
#10153=VECTOR('',#34568,10.);
#10154=VECTOR('',#34575,10.);
#10155=VECTOR('',#34576,10.);
#10156=VECTOR('',#34577,10.);
#10157=VECTOR('',#34586,10.);
#10158=VECTOR('',#34589,10.);
#10159=VECTOR('',#34592,10.);
#10160=VECTOR('',#34593,10.);
#10161=VECTOR('',#34596,10.);
#10162=VECTOR('',#34597,10.);
#10163=VECTOR('',#34602,10.);
#10164=VECTOR('',#34603,10.);
#10165=VECTOR('',#34604,10.);
#10166=VECTOR('',#34617,10.);
#10167=VECTOR('',#34620,10.);
#10168=VECTOR('',#34621,10.);
#10169=VECTOR('',#34626,10.);
#10170=VECTOR('',#34629,10.);
#10171=VECTOR('',#34630,10.);
#10172=VECTOR('',#34635,10.);
#10173=VECTOR('',#34638,10.);
#10174=VECTOR('',#34639,10.);
#10175=VECTOR('',#34644,10.);
#10176=VECTOR('',#34647,10.);
#10177=VECTOR('',#34648,10.);
#10178=VECTOR('',#34653,10.);
#10179=VECTOR('',#34656,10.);
#10180=VECTOR('',#34657,10.);
#10181=VECTOR('',#34662,10.);
#10182=VECTOR('',#34665,10.);
#10183=VECTOR('',#34666,10.);
#10184=VECTOR('',#34671,10.);
#10185=VECTOR('',#34674,10.);
#10186=VECTOR('',#34675,10.);
#10187=VECTOR('',#34678,10.);
#10188=VECTOR('',#34681,10.);
#10189=VECTOR('',#34684,10.);
#10190=VECTOR('',#34689,10.);
#10191=VECTOR('',#34692,10.);
#10192=VECTOR('',#34695,10.);
#10193=VECTOR('',#34696,10.);
#10194=VECTOR('',#34699,10.);
#10195=VECTOR('',#34702,10.);
#10196=VECTOR('',#34705,10.);
#10197=VECTOR('',#34708,10.);
#10198=VECTOR('',#34711,10.);
#10199=VECTOR('',#34714,10.);
#10200=VECTOR('',#34717,10.);
#10201=VECTOR('',#34720,10.);
#10202=VECTOR('',#34723,10.);
#10203=VECTOR('',#34726,10.);
#10204=VECTOR('',#34729,10.);
#10205=VECTOR('',#34734,12.25);
#10206=VECTOR('',#34737,12.25);
#10207=VECTOR('',#34740,12.25);
#10208=VECTOR('',#34743,5.325);
#10209=VECTOR('',#34748,5.025);
#10210=VECTOR('',#34751,1.5);
#10211=VECTOR('',#34754,1.5);
#10212=VECTOR('',#34761,4.5);
#10213=VECTOR('',#34762,4.5);
#10214=VECTOR('',#34769,5.);
#10215=VECTOR('',#34780,4.2379);
#10216=VECTOR('',#34787,5.);
#10217=VECTOR('',#34794,5.);
#10218=VECTOR('',#34801,10.);
#10219=VECTOR('',#34812,4.75);
#10220=VECTOR('',#34817,4.5);
#10221=VECTOR('',#34828,4.75);
#10222=VECTOR('',#34833,4.5);
#10223=VECTOR('',#34844,4.75);
#10224=VECTOR('',#34849,4.5);
#10225=VECTOR('',#34860,4.75);
#10226=VECTOR('',#34865,4.5);
#10227=VECTOR('',#34876,4.75);
#10228=VECTOR('',#34881,4.5);
#10229=VECTOR('',#34892,4.75);
#10230=VECTOR('',#34897,4.5);
#10231=VECTOR('',#34908,4.75);
#10232=VECTOR('',#34913,4.5);
#10233=VECTOR('',#34924,4.75);
#10234=VECTOR('',#34929,4.5);
#10235=VECTOR('',#34940,2.25);
#10236=VECTOR('',#34947,2.);
#10237=VECTOR('',#34954,10.);
#10238=VECTOR('',#34955,10.);
#10239=VECTOR('',#34956,10.);
#10240=VECTOR('',#34957,10.);
#10241=VECTOR('',#34958,10.);
#10242=VECTOR('',#34959,10.);
#10243=VECTOR('',#34962,10.);
#10244=VECTOR('',#34963,10.);
#10245=VECTOR('',#34964,10.);
#10246=VECTOR('',#34965,10.);
#10247=VECTOR('',#34966,10.);
#10248=VECTOR('',#34969,10.);
#10249=VECTOR('',#34970,10.);
#10250=VECTOR('',#34973,10.);
#10251=VECTOR('',#34974,10.);
#10252=VECTOR('',#34975,10.);
#10253=VECTOR('',#34976,10.);
#10254=VECTOR('',#34981,3.75);
#10255=VECTOR('',#34986,3.5);
#10256=VECTOR('',#34997,3.75);
#10257=VECTOR('',#35002,3.5);
#10258=VECTOR('',#35011,10.);
#10259=VECTOR('',#35012,10.);
#10260=VECTOR('',#35013,10.);
#10261=VECTOR('',#35014,10.);
#10262=VECTOR('',#35015,10.);
#10263=VECTOR('',#35016,10.);
#10264=VECTOR('',#35019,10.);
#10265=VECTOR('',#35020,10.);
#10266=VECTOR('',#35021,10.);
#10267=VECTOR('',#35022,10.);
#10268=VECTOR('',#35023,10.);
#10269=VECTOR('',#35026,10.);
#10270=VECTOR('',#35027,10.);
#10271=VECTOR('',#35030,10.);
#10272=VECTOR('',#35031,10.);
#10273=VECTOR('',#35032,10.);
#10274=VECTOR('',#35033,10.);
#10275=VECTOR('',#35036,10.);
#10276=VECTOR('',#35037,10.);
#10277=VECTOR('',#35038,10.);
#10278=VECTOR('',#35041,10.);
#10279=VECTOR('',#35042,10.);
#10280=VECTOR('',#35043,10.);
#10281=VECTOR('',#35048,4.75);
#10282=VECTOR('',#35053,4.5);
#10283=VECTOR('',#35064,4.75);
#10284=VECTOR('',#35069,4.5);
#10285=VECTOR('',#35080,4.75);
#10286=VECTOR('',#35083,10.);
#10287=VECTOR('',#35084,10.);
#10288=VECTOR('',#35169,4.75);
#10289=VECTOR('',#35172,4.75);
#10290=VECTOR('',#35175,4.75);
#10291=VECTOR('',#35178,4.75);
#10292=VECTOR('',#35181,4.75);
#10293=VECTOR('',#35184,4.75);
#10294=VECTOR('',#35187,4.75);
#10295=VECTOR('',#35190,7.3);
#10296=VECTOR('',#35197,7.05);
#10297=VECTOR('',#35200,7.3);
#10298=VECTOR('',#35207,7.05);
#10299=VECTOR('',#35210,4.75);
#10300=VECTOR('',#35213,4.75);
#10301=VECTOR('',#35216,10.);
#10302=VECTOR('',#35219,10.);
#10303=VECTOR('',#35222,10.);
#10304=VECTOR('',#35225,4.3);
#10305=VECTOR('',#35232,4.05);
#10306=VECTOR('',#35235,4.3);
#10307=VECTOR('',#35242,4.05);
#10308=VECTOR('',#35245,4.3);
#10309=VECTOR('',#35252,4.05);
#10310=VECTOR('',#35255,4.3);
#10311=VECTOR('',#35262,4.05);
#10312=VECTOR('',#35265,4.3);
#10313=VECTOR('',#35272,4.05);
#10314=VECTOR('',#35275,4.3);
#10315=VECTOR('',#35282,4.05);
#10316=VECTOR('',#35285,4.3);
#10317=VECTOR('',#35292,4.05);
#10318=VECTOR('',#35295,4.3);
#10319=VECTOR('',#35302,4.05);
#10320=VECTOR('',#35305,4.3);
#10321=VECTOR('',#35312,4.05);
#10322=VECTOR('',#35315,4.3);
#10323=VECTOR('',#35322,4.05);
#10324=VECTOR('',#35325,4.3);
#10325=VECTOR('',#35332,4.05);
#10326=VECTOR('',#35335,4.3);
#10327=VECTOR('',#35342,4.05);
#10328=VECTOR('',#35345,3.75);
#10329=VECTOR('',#35348,3.75);
#10330=VECTOR('',#35351,4.3);
#10331=VECTOR('',#35358,4.05);
#10332=VECTOR('',#35361,4.3);
#10333=VECTOR('',#35368,4.05);
#10334=VECTOR('',#35371,4.3);
#10335=VECTOR('',#35378,4.05);
#10336=VECTOR('',#35381,4.3);
#10337=VECTOR('',#35388,4.05);
#10338=VECTOR('',#35391,4.3);
#10339=VECTOR('',#35398,4.05);
#10340=VECTOR('',#35401,4.3);
#10341=VECTOR('',#35408,4.05);
#10342=VECTOR('',#35411,4.3);
#10343=VECTOR('',#35418,4.05);
#10344=VECTOR('',#35421,4.3);
#10345=VECTOR('',#35428,4.05);
#10346=VECTOR('',#35431,7.75);
#10347=VECTOR('',#35438,7.5);
#10348=VECTOR('',#35441,7.75);
#10349=VECTOR('',#35448,7.5);
#10350=VECTOR('',#35451,7.75);
#10351=VECTOR('',#35458,7.5);
#10352=VECTOR('',#35461,7.75);
#10353=VECTOR('',#35468,7.5);
#10354=VECTOR('',#35471,7.75);
#10355=VECTOR('',#35478,7.5);
#10356=VECTOR('',#35481,7.75);
#10357=VECTOR('',#35488,7.5);
#10358=VECTOR('',#35491,7.75);
#10359=VECTOR('',#35498,7.5);
#10360=VECTOR('',#35501,10.);
#10361=VECTOR('',#35502,10.);
#10362=VECTOR('',#35505,10.);
#10363=VECTOR('',#35594,2.25);
#10364=VECTOR('',#35597,7.75);
#10365=VECTOR('',#35600,7.75);
#10366=VECTOR('',#35603,7.75);
#10367=VECTOR('',#35606,7.75);
#10368=VECTOR('',#35609,7.75);
#10369=VECTOR('',#35612,7.75);
#10370=VECTOR('',#35615,7.75);
#10371=VECTOR('',#35618,7.25);
#10372=VECTOR('',#35623,7.);
#10373=VECTOR('',#35626,7.25);
#10374=VECTOR('',#35631,7.);
#10375=VECTOR('',#35634,7.25);
#10376=VECTOR('',#35639,7.);
#10377=VECTOR('',#35642,7.25);
#10378=VECTOR('',#35647,7.);
#10379=VECTOR('',#35650,7.25);
#10380=VECTOR('',#35655,7.);
#10381=VECTOR('',#35658,7.25);
#10382=VECTOR('',#35663,7.);
#10383=VECTOR('',#35666,7.25);
#10384=VECTOR('',#35671,7.);
#10385=VECTOR('',#35674,7.25);
#10386=VECTOR('',#35679,7.);
#10387=VECTOR('',#35682,7.25);
#10388=VECTOR('',#35687,7.);
#10389=VECTOR('',#35690,7.25);
#10390=VECTOR('',#35695,7.);
#10391=VECTOR('',#35698,4.3);
#10392=VECTOR('',#35701,4.3);
#10393=VECTOR('',#35704,4.3);
#10394=VECTOR('',#35707,4.3);
#10395=VECTOR('',#35710,4.3);
#10396=VECTOR('',#35713,4.3);
#10397=VECTOR('',#35716,4.3);
#10398=VECTOR('',#35719,4.3);
#10399=VECTOR('',#35722,4.3);
#10400=VECTOR('',#35725,4.3);
#10401=VECTOR('',#35728,4.3);
#10402=VECTOR('',#35731,4.3);
#10403=VECTOR('',#35734,4.3);
#10404=VECTOR('',#35737,4.3);
#10405=VECTOR('',#35740,4.3);
#10406=VECTOR('',#35743,4.3);
#10407=VECTOR('',#35746,4.3);
#10408=VECTOR('',#35749,4.3);
#10409=VECTOR('',#35752,4.3);
#10410=VECTOR('',#35755,4.3);
#10411=VECTOR('',#35758,7.3);
#10412=VECTOR('',#35761,7.3);
#10413=VECTOR('',#35764,6.75);
#10414=VECTOR('',#35769,6.5);
#10415=VECTOR('',#35772,6.75);
#10416=VECTOR('',#35777,6.5);
#10417=VECTOR('',#35780,4.2379);
#10418=VECTOR('',#35789,3.5);
#10419=VECTOR('',#35798,3.5);
#10420=VECTOR('',#35807,3.25);
#10421=VECTOR('',#35812,10.);
#10422=VECTOR('',#35813,10.);
#10423=VECTOR('',#35814,10.);
#10424=VECTOR('',#35815,10.);
#10425=VECTOR('',#35816,10.);
#10426=VECTOR('',#35817,10.);
#10427=VECTOR('',#35820,3.25);
#10428=VECTOR('',#35825,10.);
#10429=VECTOR('',#35826,10.);
#10430=VECTOR('',#35829,10.);
#10431=VECTOR('',#35830,10.);
#10432=VECTOR('',#35831,10.);
#10433=VECTOR('',#35834,10.);
#10434=VECTOR('',#35835,10.);
#10435=VECTOR('',#35838,10.);
#10436=VECTOR('',#35839,10.);
#10437=VECTOR('',#35840,10.);
#10438=VECTOR('',#35841,10.);
#10439=VECTOR('',#35844,10.);
#10440=VECTOR('',#35845,10.);
#10441=VECTOR('',#35846,10.);
#10442=VECTOR('',#35849,10.);
#10443=VECTOR('',#35850,10.);
#10444=VECTOR('',#35851,10.);
#10445=VECTOR('',#35854,10.);
#10446=VECTOR('',#35855,10.);
#10447=VECTOR('',#35858,10.);
#10448=VECTOR('',#35859,10.);
#10449=VECTOR('',#35860,10.);
#10450=VECTOR('',#35861,10.);
#10451=VECTOR('',#35864,10.);
#10452=VECTOR('',#35865,10.);
#10453=VECTOR('',#35866,10.);
#10454=VECTOR('',#35867,10.);
#10455=VECTOR('',#35870,10.);
#10456=VECTOR('',#35877,10.);
#10457=VECTOR('',#35884,10.);
#10458=VECTOR('',#35885,10.);
#10459=VECTOR('',#35886,10.);
#10460=VECTOR('',#35889,10.);
#10461=VECTOR('',#35890,10.);
#10462=VECTOR('',#35891,10.);
#10463=VECTOR('',#35896,10.);
#10464=VECTOR('',#35897,10.);
#10465=VECTOR('',#35900,10.);
#10466=VECTOR('',#35901,10.);
#10467=VECTOR('',#35904,10.);
#10468=VECTOR('',#35905,10.);
#10469=VECTOR('',#35908,10.);
#10470=VECTOR('',#35909,10.);
#10471=VECTOR('',#35928,1.7);
#10472=VECTOR('',#35931,1.7);
#10473=VECTOR('',#35934,1.5);
#10474=VECTOR('',#35937,1.5);
#10475=VECTOR('',#35944,4.5);
#10476=VECTOR('',#35945,4.5);
#10477=VECTOR('',#35952,7.05);
#10478=VECTOR('',#35961,0.4);
#10479=VECTOR('',#35966,10.);
#10480=VECTOR('',#35981,0.4);
#10481=VECTOR('',#35984,10.);
#10482=VECTOR('',#35999,4.);
#10483=VECTOR('',#36004,4.);
#10484=VECTOR('',#36007,4.);
#10485=VECTOR('',#36010,4.);
#10486=VECTOR('',#36013,4.);
#10487=VECTOR('',#36016,4.);
#10488=VECTOR('',#36019,4.);
#10489=VECTOR('',#36022,4.);
#10490=VECTOR('',#36025,4.);
#10491=VECTOR('',#36028,4.);
#10492=VECTOR('',#36031,3.22275);
#10493=VECTOR('',#36036,3.22275);
#10494=VECTOR('',#36039,3.22275);
#10495=VECTOR('',#36042,3.22275);
#10496=VECTOR('',#36045,3.22275);
#10497=VECTOR('',#36048,3.22275);
#10498=VECTOR('',#36051,3.22275);
#10499=VECTOR('',#36054,3.22275);
#10500=VECTOR('',#36057,3.22275);
#10501=VECTOR('',#36060,3.22275);
#10502=VECTOR('',#36079,10.);
#10503=VECTOR('',#36080,10.);
#10504=VECTOR('',#36081,10.);
#10505=VECTOR('',#36082,10.);
#10506=VECTOR('',#36087,10.);
#10507=VECTOR('',#36090,10.);
#10508=VECTOR('',#36091,10.);
#10509=VECTOR('',#36098,10.);
#10510=VECTOR('',#36099,10.);
#10511=VECTOR('',#36100,10.);
#10512=VECTOR('',#36101,10.);
#10513=VECTOR('',#36106,10.);
#10514=VECTOR('',#36109,10.);
#10515=VECTOR('',#36110,10.);
#10516=VECTOR('',#36117,10.);
#10517=VECTOR('',#36118,10.);
#10518=VECTOR('',#36119,10.);
#10519=VECTOR('',#36120,10.);
#10520=VECTOR('',#36125,10.);
#10521=VECTOR('',#36128,10.);
#10522=VECTOR('',#36129,10.);
#10523=VECTOR('',#36136,10.);
#10524=VECTOR('',#36137,10.);
#10525=VECTOR('',#36138,10.);
#10526=VECTOR('',#36139,10.);
#10527=VECTOR('',#36144,10.);
#10528=VECTOR('',#36147,10.);
#10529=VECTOR('',#36148,10.);
#10530=VECTOR('',#36155,10.);
#10531=VECTOR('',#36156,10.);
#10532=VECTOR('',#36157,10.);
#10533=VECTOR('',#36158,10.);
#10534=VECTOR('',#36163,10.);
#10535=VECTOR('',#36166,10.);
#10536=VECTOR('',#36167,10.);
#10537=VECTOR('',#36174,10.);
#10538=VECTOR('',#36175,10.);
#10539=VECTOR('',#36176,10.);
#10540=VECTOR('',#36177,10.);
#10541=VECTOR('',#36182,10.);
#10542=VECTOR('',#36185,10.);
#10543=VECTOR('',#36186,10.);
#10544=VECTOR('',#36193,10.);
#10545=VECTOR('',#36194,10.);
#10546=VECTOR('',#36195,10.);
#10547=VECTOR('',#36196,10.);
#10548=VECTOR('',#36201,10.);
#10549=VECTOR('',#36204,10.);
#10550=VECTOR('',#36205,10.);
#10551=VECTOR('',#36212,10.);
#10552=VECTOR('',#36213,10.);
#10553=VECTOR('',#36214,10.);
#10554=VECTOR('',#36215,10.);
#10555=VECTOR('',#36220,10.);
#10556=VECTOR('',#36223,10.);
#10557=VECTOR('',#36224,10.);
#10558=VECTOR('',#36231,10.);
#10559=VECTOR('',#36232,10.);
#10560=VECTOR('',#36233,10.);
#10561=VECTOR('',#36234,10.);
#10562=VECTOR('',#36239,10.);
#10563=VECTOR('',#36242,10.);
#10564=VECTOR('',#36243,10.);
#10565=VECTOR('',#36250,10.);
#10566=VECTOR('',#36251,10.);
#10567=VECTOR('',#36252,10.);
#10568=VECTOR('',#36253,10.);
#10569=VECTOR('',#36258,10.);
#10570=VECTOR('',#36261,10.);
#10571=VECTOR('',#36262,10.);
#10572=VECTOR('',#36269,10.);
#10573=VECTOR('',#36270,10.);
#10574=VECTOR('',#36271,10.);
#10575=VECTOR('',#36272,10.);
#10576=VECTOR('',#36277,10.);
#10577=VECTOR('',#36280,10.);
#10578=VECTOR('',#36281,10.);
#10579=VECTOR('',#36288,10.);
#10580=VECTOR('',#36289,10.);
#10581=VECTOR('',#36290,10.);
#10582=VECTOR('',#36291,10.);
#10583=VECTOR('',#36296,10.);
#10584=VECTOR('',#36299,10.);
#10585=VECTOR('',#36300,10.);
#10586=VECTOR('',#36307,10.);
#10587=VECTOR('',#36308,10.);
#10588=VECTOR('',#36309,10.);
#10589=VECTOR('',#36310,10.);
#10590=VECTOR('',#36315,10.);
#10591=VECTOR('',#36318,10.);
#10592=VECTOR('',#36319,10.);
#10593=VECTOR('',#36326,10.);
#10594=VECTOR('',#36327,10.);
#10595=VECTOR('',#36328,10.);
#10596=VECTOR('',#36329,10.);
#10597=VECTOR('',#36334,10.);
#10598=VECTOR('',#36337,10.);
#10599=VECTOR('',#36338,10.);
#10600=VECTOR('',#36345,10.);
#10601=VECTOR('',#36346,10.);
#10602=VECTOR('',#36347,10.);
#10603=VECTOR('',#36348,10.);
#10604=VECTOR('',#36353,10.);
#10605=VECTOR('',#36356,10.);
#10606=VECTOR('',#36357,10.);
#10607=VECTOR('',#36364,10.);
#10608=VECTOR('',#36365,10.);
#10609=VECTOR('',#36366,10.);
#10610=VECTOR('',#36367,10.);
#10611=VECTOR('',#36372,10.);
#10612=VECTOR('',#36375,10.);
#10613=VECTOR('',#36376,10.);
#10614=VECTOR('',#36383,10.);
#10615=VECTOR('',#36384,10.);
#10616=VECTOR('',#36385,10.);
#10617=VECTOR('',#36386,10.);
#10618=VECTOR('',#36391,10.);
#10619=VECTOR('',#36394,10.);
#10620=VECTOR('',#36395,10.);
#10621=VECTOR('',#36402,10.);
#10622=VECTOR('',#36403,10.);
#10623=VECTOR('',#36404,10.);
#10624=VECTOR('',#36405,10.);
#10625=VECTOR('',#36410,10.);
#10626=VECTOR('',#36415,10.);
#10627=VECTOR('',#36416,10.);
#10628=VECTOR('',#36425,10.);
#10629=VECTOR('',#36426,10.);
#10630=VECTOR('',#36427,10.);
#10631=VECTOR('',#36428,10.);
#10632=VECTOR('',#36433,10.);
#10633=VECTOR('',#36436,10.);
#10634=VECTOR('',#36437,10.);
#10635=VECTOR('',#36444,10.);
#10636=VECTOR('',#36445,10.);
#10637=VECTOR('',#36446,10.);
#10638=VECTOR('',#36447,10.);
#10639=VECTOR('',#36452,10.);
#10640=VECTOR('',#36455,10.);
#10641=VECTOR('',#36456,10.);
#10642=VECTOR('',#36463,10.);
#10643=VECTOR('',#36464,10.);
#10644=VECTOR('',#36465,10.);
#10645=VECTOR('',#36466,10.);
#10646=VECTOR('',#36471,10.);
#10647=VECTOR('',#36474,10.);
#10648=VECTOR('',#36475,10.);
#10649=VECTOR('',#36482,10.);
#10650=VECTOR('',#36483,10.);
#10651=VECTOR('',#36484,10.);
#10652=VECTOR('',#36485,10.);
#10653=VECTOR('',#36490,10.);
#10654=VECTOR('',#36493,10.);
#10655=VECTOR('',#36494,10.);
#10656=VECTOR('',#36501,10.);
#10657=VECTOR('',#36502,10.);
#10658=VECTOR('',#36503,10.);
#10659=VECTOR('',#36504,10.);
#10660=VECTOR('',#36509,10.);
#10661=VECTOR('',#36512,10.);
#10662=VECTOR('',#36513,10.);
#10663=VECTOR('',#36520,10.);
#10664=VECTOR('',#36521,10.);
#10665=VECTOR('',#36522,10.);
#10666=VECTOR('',#36523,10.);
#10667=VECTOR('',#36528,10.);
#10668=VECTOR('',#36531,10.);
#10669=VECTOR('',#36532,10.);
#10670=VECTOR('',#36539,10.);
#10671=VECTOR('',#36540,10.);
#10672=VECTOR('',#36541,10.);
#10673=VECTOR('',#36542,10.);
#10674=VECTOR('',#36547,10.);
#10675=VECTOR('',#36550,10.);
#10676=VECTOR('',#36551,10.);
#10677=VECTOR('',#36558,10.);
#10678=VECTOR('',#36559,10.);
#10679=VECTOR('',#36560,10.);
#10680=VECTOR('',#36561,10.);
#10681=VECTOR('',#36566,10.);
#10682=VECTOR('',#36569,10.);
#10683=VECTOR('',#36570,10.);
#10684=VECTOR('',#36577,10.);
#10685=VECTOR('',#36578,10.);
#10686=VECTOR('',#36579,10.);
#10687=VECTOR('',#36580,10.);
#10688=VECTOR('',#36585,10.);
#10689=VECTOR('',#36588,10.);
#10690=VECTOR('',#36589,10.);
#10691=VECTOR('',#36596,10.);
#10692=VECTOR('',#36597,10.);
#10693=VECTOR('',#36598,10.);
#10694=VECTOR('',#36599,10.);
#10695=VECTOR('',#36604,10.);
#10696=VECTOR('',#36607,10.);
#10697=VECTOR('',#36608,10.);
#10698=VECTOR('',#36615,10.);
#10699=VECTOR('',#36616,10.);
#10700=VECTOR('',#36617,10.);
#10701=VECTOR('',#36618,10.);
#10702=VECTOR('',#36623,10.);
#10703=VECTOR('',#36626,10.);
#10704=VECTOR('',#36627,10.);
#10705=VECTOR('',#36634,10.);
#10706=VECTOR('',#36635,10.);
#10707=VECTOR('',#36636,10.);
#10708=VECTOR('',#36637,10.);
#10709=VECTOR('',#36642,10.);
#10710=VECTOR('',#36645,10.);
#10711=VECTOR('',#36646,10.);
#10712=VECTOR('',#36653,10.);
#10713=VECTOR('',#36654,10.);
#10714=VECTOR('',#36655,10.);
#10715=VECTOR('',#36656,10.);
#10716=VECTOR('',#36661,10.);
#10717=VECTOR('',#36664,10.);
#10718=VECTOR('',#36665,10.);
#10719=VECTOR('',#36672,10.);
#10720=VECTOR('',#36673,10.);
#10721=VECTOR('',#36674,10.);
#10722=VECTOR('',#36675,10.);
#10723=VECTOR('',#36680,10.);
#10724=VECTOR('',#36683,10.);
#10725=VECTOR('',#36684,10.);
#10726=VECTOR('',#36691,10.);
#10727=VECTOR('',#36692,10.);
#10728=VECTOR('',#36693,10.);
#10729=VECTOR('',#36694,10.);
#10730=VECTOR('',#36699,10.);
#10731=VECTOR('',#36702,10.);
#10732=VECTOR('',#36703,10.);
#10733=VECTOR('',#36710,10.);
#10734=VECTOR('',#36711,10.);
#10735=VECTOR('',#36712,10.);
#10736=VECTOR('',#36713,10.);
#10737=VECTOR('',#36718,10.);
#10738=VECTOR('',#36721,10.);
#10739=VECTOR('',#36722,10.);
#10740=VECTOR('',#36729,10.);
#10741=VECTOR('',#36730,10.);
#10742=VECTOR('',#36731,10.);
#10743=VECTOR('',#36732,10.);
#10744=VECTOR('',#36737,10.);
#10745=VECTOR('',#36740,10.);
#10746=VECTOR('',#36741,10.);
#10747=VECTOR('',#36748,10.);
#10748=VECTOR('',#36749,10.);
#10749=VECTOR('',#36750,10.);
#10750=VECTOR('',#36751,10.);
#10751=VECTOR('',#36756,10.);
#10752=VECTOR('',#36759,10.);
#10753=VECTOR('',#36760,10.);
#10754=VECTOR('',#36767,1.25);
#10755=VECTOR('',#36772,10.);
#10756=VECTOR('',#36773,10.);
#10757=VECTOR('',#36774,10.);
#10758=VECTOR('',#36775,10.);
#10759=VECTOR('',#36778,10.);
#10760=VECTOR('',#36779,10.);
#10761=VECTOR('',#36780,10.);
#10762=VECTOR('',#36783,10.);
#10763=VECTOR('',#36784,10.);
#10764=VECTOR('',#36785,10.);
#10765=VECTOR('',#36788,10.);
#10766=VECTOR('',#36789,10.);
#10767=VECTOR('',#36790,10.);
#10768=VECTOR('',#36793,10.);
#10769=VECTOR('',#36794,10.);
#10770=VECTOR('',#36795,10.);
#10771=VECTOR('',#36798,10.);
#10772=VECTOR('',#36799,10.);
#10773=VECTOR('',#36814,5.);
#10774=VECTOR('',#36827,3.6);
#10775=VECTOR('',#36836,3.625);
#10776=VECTOR('',#36841,3.25);
#10777=VECTOR('',#36848,8.);
#10778=VECTOR('',#36849,8.);
#10779=VECTOR('',#36854,7.75);
#10780=VECTOR('',#36863,5.25);
#10781=VECTOR('',#36874,15.);
#10782=VECTOR('',#36893,4.85);
#10783=VECTOR('',#36898,5.);
#10784=VECTOR('',#36903,4.85);
#10785=VECTOR('',#36922,4.4);
#10786=VECTOR('',#36929,4.5);
#10787=VECTOR('',#36938,2.225);
#10788=VECTOR('',#36947,4.425);
#10789=VECTOR('',#36952,2.);
#10790=VECTOR('',#36957,2.);
#10791=VECTOR('',#36960,2.);
#10792=VECTOR('',#36963,2.);
#10793=VECTOR('',#36966,2.);
#10794=VECTOR('',#36969,2.);
#10795=VECTOR('',#36972,2.);
#10796=VECTOR('',#36975,2.);
#10797=VECTOR('',#36978,2.);
#10798=VECTOR('',#36981,2.);
#10799=VECTOR('',#36984,2.);
#10800=VECTOR('',#36987,2.);
#10801=VECTOR('',#36990,2.);
#10802=VECTOR('',#36993,2.);
#10803=VECTOR('',#36996,2.);
#10804=VECTOR('',#36999,2.);
#10805=VECTOR('',#37002,2.);
#10806=VECTOR('',#37005,2.);
#10807=VECTOR('',#37008,2.);
#10808=VECTOR('',#37011,2.);
#10809=VECTOR('',#37014,2.);
#10810=VECTOR('',#37017,2.);
#10811=VECTOR('',#37020,2.);
#10812=VECTOR('',#37023,2.);
#10813=VECTOR('',#37026,2.);
#10814=VECTOR('',#37029,2.);
#10815=VECTOR('',#37032,2.);
#10816=VECTOR('',#37035,2.);
#10817=VECTOR('',#37038,2.);
#10818=VECTOR('',#37041,2.);
#10819=VECTOR('',#37044,2.);
#10820=VECTOR('',#37047,2.);
#10821=VECTOR('',#37050,2.);
#10822=VECTOR('',#37053,2.);
#10823=VECTOR('',#37056,2.);
#10824=VECTOR('',#37059,2.);
#10825=VECTOR('',#37062,2.);
#10826=VECTOR('',#37065,2.);
#10827=VECTOR('',#37068,2.);
#10828=VECTOR('',#37071,2.);
#10829=VECTOR('',#37074,2.);
#10830=VECTOR('',#37077,2.);
#10831=VECTOR('',#37080,1.5555);
#10832=VECTOR('',#37085,1.5555);
#10833=VECTOR('',#37088,1.5555);
#10834=VECTOR('',#37091,1.5555);
#10835=VECTOR('',#37094,1.5555);
#10836=VECTOR('',#37097,1.5555);
#10837=VECTOR('',#37100,1.5555);
#10838=VECTOR('',#37103,1.5555);
#10839=VECTOR('',#37106,1.5555);
#10840=VECTOR('',#37109,1.5555);
#10841=VECTOR('',#37112,1.5555);
#10842=VECTOR('',#37115,1.5555);
#10843=VECTOR('',#37118,1.5555);
#10844=VECTOR('',#37121,1.5555);
#10845=VECTOR('',#37124,1.5555);
#10846=VECTOR('',#37127,1.5555);
#10847=VECTOR('',#37130,1.5555);
#10848=VECTOR('',#37133,1.5555);
#10849=VECTOR('',#37136,1.5555);
#10850=VECTOR('',#37139,1.5555);
#10851=VECTOR('',#37142,1.5555);
#10852=VECTOR('',#37145,1.5555);
#10853=VECTOR('',#37148,1.5555);
#10854=VECTOR('',#37151,1.5555);
#10855=VECTOR('',#37154,1.5555);
#10856=VECTOR('',#37157,1.5555);
#10857=VECTOR('',#37160,1.5555);
#10858=VECTOR('',#37163,1.5555);
#10859=VECTOR('',#37166,1.5555);
#10860=VECTOR('',#37169,1.5555);
#10861=VECTOR('',#37172,1.5555);
#10862=VECTOR('',#37175,1.5555);
#10863=VECTOR('',#37178,1.5555);
#10864=VECTOR('',#37181,1.5555);
#10865=VECTOR('',#37184,1.5555);
#10866=VECTOR('',#37187,1.5555);
#10867=VECTOR('',#37190,1.5555);
#10868=VECTOR('',#37193,1.5555);
#10869=VECTOR('',#37196,1.5555);
#10870=VECTOR('',#37199,1.5555);
#10871=VECTOR('',#37202,1.5555);
#10872=VECTOR('',#37205,1.5555);
#10873=VECTOR('',#37238,10.);
#10874=VECTOR('',#37239,10.);
#10875=VECTOR('',#37240,10.);
#10876=VECTOR('',#37241,10.);
#10877=VECTOR('',#37246,10.);
#10878=VECTOR('',#37249,10.);
#10879=VECTOR('',#37250,10.);
#10880=VECTOR('',#37257,10.);
#10881=VECTOR('',#37258,10.);
#10882=VECTOR('',#37259,10.);
#10883=VECTOR('',#37260,10.);
#10884=VECTOR('',#37265,10.);
#10885=VECTOR('',#37268,10.);
#10886=VECTOR('',#37269,10.);
#10887=VECTOR('',#37276,10.);
#10888=VECTOR('',#37277,10.);
#10889=VECTOR('',#37278,10.);
#10890=VECTOR('',#37279,10.);
#10891=VECTOR('',#37284,10.);
#10892=VECTOR('',#37287,10.);
#10893=VECTOR('',#37288,10.);
#10894=VECTOR('',#37295,10.);
#10895=VECTOR('',#37296,10.);
#10896=VECTOR('',#37297,10.);
#10897=VECTOR('',#37298,10.);
#10898=VECTOR('',#37303,10.);
#10899=VECTOR('',#37306,10.);
#10900=VECTOR('',#37307,10.);
#10901=VECTOR('',#37314,10.);
#10902=VECTOR('',#37315,10.);
#10903=VECTOR('',#37316,10.);
#10904=VECTOR('',#37317,10.);
#10905=VECTOR('',#37322,10.);
#10906=VECTOR('',#37325,10.);
#10907=VECTOR('',#37326,10.);
#10908=VECTOR('',#37333,10.);
#10909=VECTOR('',#37334,10.);
#10910=VECTOR('',#37335,10.);
#10911=VECTOR('',#37336,10.);
#10912=VECTOR('',#37341,10.);
#10913=VECTOR('',#37344,10.);
#10914=VECTOR('',#37345,10.);
#10915=VECTOR('',#37352,10.);
#10916=VECTOR('',#37353,10.);
#10917=VECTOR('',#37354,10.);
#10918=VECTOR('',#37355,10.);
#10919=VECTOR('',#37360,10.);
#10920=VECTOR('',#37363,10.);
#10921=VECTOR('',#37364,10.);
#10922=VECTOR('',#37371,10.);
#10923=VECTOR('',#37372,10.);
#10924=VECTOR('',#37373,10.);
#10925=VECTOR('',#37374,10.);
#10926=VECTOR('',#37379,10.);
#10927=VECTOR('',#37382,10.);
#10928=VECTOR('',#37383,10.);
#10929=VECTOR('',#37390,10.);
#10930=VECTOR('',#37391,10.);
#10931=VECTOR('',#37392,10.);
#10932=VECTOR('',#37393,10.);
#10933=VECTOR('',#37398,10.);
#10934=VECTOR('',#37401,10.);
#10935=VECTOR('',#37402,10.);
#10936=VECTOR('',#37409,10.);
#10937=VECTOR('',#37410,10.);
#10938=VECTOR('',#37411,10.);
#10939=VECTOR('',#37412,10.);
#10940=VECTOR('',#37417,10.);
#10941=VECTOR('',#37420,10.);
#10942=VECTOR('',#37421,10.);
#10943=VECTOR('',#37428,10.);
#10944=VECTOR('',#37429,10.);
#10945=VECTOR('',#37430,10.);
#10946=VECTOR('',#37431,10.);
#10947=VECTOR('',#37436,10.);
#10948=VECTOR('',#37439,10.);
#10949=VECTOR('',#37440,10.);
#10950=VECTOR('',#37447,10.);
#10951=VECTOR('',#37448,10.);
#10952=VECTOR('',#37449,10.);
#10953=VECTOR('',#37450,10.);
#10954=VECTOR('',#37455,10.);
#10955=VECTOR('',#37458,10.);
#10956=VECTOR('',#37459,10.);
#10957=VECTOR('',#37466,10.);
#10958=VECTOR('',#37467,10.);
#10959=VECTOR('',#37468,10.);
#10960=VECTOR('',#37469,10.);
#10961=VECTOR('',#37474,10.);
#10962=VECTOR('',#37477,10.);
#10963=VECTOR('',#37478,10.);
#10964=VECTOR('',#37485,10.);
#10965=VECTOR('',#37486,10.);
#10966=VECTOR('',#37487,10.);
#10967=VECTOR('',#37488,10.);
#10968=VECTOR('',#37493,10.);
#10969=VECTOR('',#37496,10.);
#10970=VECTOR('',#37497,10.);
#10971=VECTOR('',#37504,10.);
#10972=VECTOR('',#37505,10.);
#10973=VECTOR('',#37506,10.);
#10974=VECTOR('',#37507,10.);
#10975=VECTOR('',#37512,10.);
#10976=VECTOR('',#37515,10.);
#10977=VECTOR('',#37516,10.);
#10978=VECTOR('',#37523,10.);
#10979=VECTOR('',#37524,10.);
#10980=VECTOR('',#37525,10.);
#10981=VECTOR('',#37526,10.);
#10982=VECTOR('',#37531,10.);
#10983=VECTOR('',#37534,10.);
#10984=VECTOR('',#37535,10.);
#10985=VECTOR('',#37542,10.);
#10986=VECTOR('',#37543,10.);
#10987=VECTOR('',#37544,10.);
#10988=VECTOR('',#37545,10.);
#10989=VECTOR('',#37550,10.);
#10990=VECTOR('',#37553,10.);
#10991=VECTOR('',#37554,10.);
#10992=VECTOR('',#37561,10.);
#10993=VECTOR('',#37562,10.);
#10994=VECTOR('',#37563,10.);
#10995=VECTOR('',#37564,10.);
#10996=VECTOR('',#37569,10.);
#10997=VECTOR('',#37574,10.);
#10998=VECTOR('',#37575,10.);
#10999=VECTOR('',#37584,10.);
#11000=VECTOR('',#37585,10.);
#11001=VECTOR('',#37586,10.);
#11002=VECTOR('',#37587,10.);
#11003=VECTOR('',#37592,10.);
#11004=VECTOR('',#37595,10.);
#11005=VECTOR('',#37596,10.);
#11006=VECTOR('',#37603,10.);
#11007=VECTOR('',#37604,10.);
#11008=VECTOR('',#37605,10.);
#11009=VECTOR('',#37606,10.);
#11010=VECTOR('',#37611,10.);
#11011=VECTOR('',#37614,10.);
#11012=VECTOR('',#37615,10.);
#11013=VECTOR('',#37622,10.);
#11014=VECTOR('',#37623,10.);
#11015=VECTOR('',#37624,10.);
#11016=VECTOR('',#37625,10.);
#11017=VECTOR('',#37630,10.);
#11018=VECTOR('',#37633,10.);
#11019=VECTOR('',#37634,10.);
#11020=VECTOR('',#37641,10.);
#11021=VECTOR('',#37642,10.);
#11022=VECTOR('',#37643,10.);
#11023=VECTOR('',#37644,10.);
#11024=VECTOR('',#37649,10.);
#11025=VECTOR('',#37652,10.);
#11026=VECTOR('',#37653,10.);
#11027=VECTOR('',#37660,10.);
#11028=VECTOR('',#37661,10.);
#11029=VECTOR('',#37662,10.);
#11030=VECTOR('',#37663,10.);
#11031=VECTOR('',#37668,10.);
#11032=VECTOR('',#37671,10.);
#11033=VECTOR('',#37672,10.);
#11034=VECTOR('',#37679,10.);
#11035=VECTOR('',#37680,10.);
#11036=VECTOR('',#37681,10.);
#11037=VECTOR('',#37682,10.);
#11038=VECTOR('',#37687,10.);
#11039=VECTOR('',#37690,10.);
#11040=VECTOR('',#37691,10.);
#11041=VECTOR('',#37698,10.);
#11042=VECTOR('',#37699,10.);
#11043=VECTOR('',#37700,10.);
#11044=VECTOR('',#37701,10.);
#11045=VECTOR('',#37706,10.);
#11046=VECTOR('',#37709,10.);
#11047=VECTOR('',#37710,10.);
#11048=VECTOR('',#37717,10.);
#11049=VECTOR('',#37718,10.);
#11050=VECTOR('',#37719,10.);
#11051=VECTOR('',#37720,10.);
#11052=VECTOR('',#37725,10.);
#11053=VECTOR('',#37728,10.);
#11054=VECTOR('',#37729,10.);
#11055=VECTOR('',#37736,10.);
#11056=VECTOR('',#37737,10.);
#11057=VECTOR('',#37738,10.);
#11058=VECTOR('',#37739,10.);
#11059=VECTOR('',#37744,10.);
#11060=VECTOR('',#37747,10.);
#11061=VECTOR('',#37748,10.);
#11062=VECTOR('',#37755,10.);
#11063=VECTOR('',#37756,10.);
#11064=VECTOR('',#37757,10.);
#11065=VECTOR('',#37758,10.);
#11066=VECTOR('',#37763,10.);
#11067=VECTOR('',#37766,10.);
#11068=VECTOR('',#37767,10.);
#11069=VECTOR('',#37774,10.);
#11070=VECTOR('',#37775,10.);
#11071=VECTOR('',#37776,10.);
#11072=VECTOR('',#37777,10.);
#11073=VECTOR('',#37782,10.);
#11074=VECTOR('',#37785,10.);
#11075=VECTOR('',#37786,10.);
#11076=VECTOR('',#37793,10.);
#11077=VECTOR('',#37794,10.);
#11078=VECTOR('',#37795,10.);
#11079=VECTOR('',#37796,10.);
#11080=VECTOR('',#37801,10.);
#11081=VECTOR('',#37804,10.);
#11082=VECTOR('',#37805,10.);
#11083=VECTOR('',#37812,10.);
#11084=VECTOR('',#37813,10.);
#11085=VECTOR('',#37814,10.);
#11086=VECTOR('',#37815,10.);
#11087=VECTOR('',#37820,10.);
#11088=VECTOR('',#37823,10.);
#11089=VECTOR('',#37824,10.);
#11090=VECTOR('',#37831,10.);
#11091=VECTOR('',#37832,10.);
#11092=VECTOR('',#37833,10.);
#11093=VECTOR('',#37834,10.);
#11094=VECTOR('',#37839,10.);
#11095=VECTOR('',#37842,10.);
#11096=VECTOR('',#37843,10.);
#11097=VECTOR('',#37850,10.);
#11098=VECTOR('',#37851,10.);
#11099=VECTOR('',#37852,10.);
#11100=VECTOR('',#37853,10.);
#11101=VECTOR('',#37858,10.);
#11102=VECTOR('',#37861,10.);
#11103=VECTOR('',#37862,10.);
#11104=VECTOR('',#37869,10.);
#11105=VECTOR('',#37870,10.);
#11106=VECTOR('',#37871,10.);
#11107=VECTOR('',#37872,10.);
#11108=VECTOR('',#37877,10.);
#11109=VECTOR('',#37880,10.);
#11110=VECTOR('',#37881,10.);
#11111=VECTOR('',#37888,10.);
#11112=VECTOR('',#37889,10.);
#11113=VECTOR('',#37890,10.);
#11114=VECTOR('',#37891,10.);
#11115=VECTOR('',#37896,10.);
#11116=VECTOR('',#37899,10.);
#11117=VECTOR('',#37900,10.);
#11118=VECTOR('',#37907,10.);
#11119=VECTOR('',#37908,10.);
#11120=VECTOR('',#37909,10.);
#11121=VECTOR('',#37910,10.);
#11122=VECTOR('',#37915,10.);
#11123=VECTOR('',#37918,10.);
#11124=VECTOR('',#37919,10.);
#11125=VECTOR('',#37926,0.75);
#11126=VECTOR('',#37931,10.);
#11127=VECTOR('',#37932,10.);
#11128=VECTOR('',#37933,10.);
#11129=VECTOR('',#37934,10.);
#11130=VECTOR('',#37937,10.);
#11131=VECTOR('',#37938,10.);
#11132=VECTOR('',#37939,10.);
#11133=VECTOR('',#37942,10.);
#11134=VECTOR('',#37943,10.);
#11135=VECTOR('',#37944,10.);
#11136=VECTOR('',#37947,10.);
#11137=VECTOR('',#37948,10.);
#11138=VECTOR('',#37949,10.);
#11139=VECTOR('',#37952,10.);
#11140=VECTOR('',#37953,10.);
#11141=VECTOR('',#37954,10.);
#11142=VECTOR('',#37957,10.);
#11143=VECTOR('',#37958,10.);
#11144=VECTOR('',#37967,1.8);
#11145=VECTOR('',#37972,3.5);
#11146=VECTOR('',#37973,3.5);
#11147=VECTOR('',#37978,3.3);
#11148=VECTOR('',#37991,1.35);
#11149=VECTOR('',#37996,1.5);
#11150=VECTOR('',#38001,1.35);
#11151=VECTOR('',#38008,1.5);
#11152=VECTOR('',#38013,1.5);
#11153=VECTOR('',#38016,1.5);
#11154=VECTOR('',#38019,1.5);
#11155=VECTOR('',#38022,1.5);
#11156=VECTOR('',#38025,1.5);
#11157=VECTOR('',#38028,1.5);
#11158=VECTOR('',#38031,1.5);
#11159=VECTOR('',#38034,1.5);
#11160=VECTOR('',#38037,1.5);
#11161=VECTOR('',#38040,1.5);
#11162=VECTOR('',#38043,1.5);
#11163=VECTOR('',#38046,1.5);
#11164=VECTOR('',#38049,1.5);
#11165=VECTOR('',#38052,1.5);
#11166=VECTOR('',#38055,1.5);
#11167=VECTOR('',#38058,1.5);
#11168=VECTOR('',#38061,1.5);
#11169=VECTOR('',#38064,1.5);
#11170=VECTOR('',#38067,1.5);
#11171=VECTOR('',#38070,1.5);
#11172=VECTOR('',#38073,1.5);
#11173=VECTOR('',#38076,1.5);
#11174=VECTOR('',#38079,1.5);
#11175=VECTOR('',#38082,1.5);
#11176=VECTOR('',#38085,1.5);
#11177=VECTOR('',#38088,1.5);
#11178=VECTOR('',#38091,1.5);
#11179=VECTOR('',#38094,1.5);
#11180=VECTOR('',#38097,1.5);
#11181=VECTOR('',#38100,1.5);
#11182=VECTOR('',#38103,1.5);
#11183=VECTOR('',#38106,1.5);
#11184=VECTOR('',#38109,1.5);
#11185=VECTOR('',#38112,1.5);
#11186=VECTOR('',#38115,1.5);
#11187=VECTOR('',#38118,1.5);
#11188=VECTOR('',#38121,1.5);
#11189=VECTOR('',#38124,1.5);
#11190=VECTOR('',#38127,1.5);
#11191=VECTOR('',#38130,1.5);
#11192=VECTOR('',#38133,1.5);
#11193=VECTOR('',#38136,1.5);
#11194=VECTOR('',#38139,1.5);
#11195=VECTOR('',#38142,1.5);
#11196=VECTOR('',#38145,1.5);
#11197=VECTOR('',#38148,1.5);
#11198=VECTOR('',#38151,1.5);
#11199=VECTOR('',#38154,1.5);
#11200=VECTOR('',#38157,1.5);
#11201=VECTOR('',#38160,1.5);
#11202=VECTOR('',#38163,1.5);
#11203=VECTOR('',#38166,1.5);
#11204=VECTOR('',#38169,1.5);
#11205=VECTOR('',#38172,1.5);
#11206=VECTOR('',#38175,1.5);
#11207=VECTOR('',#38178,1.5);
#11208=VECTOR('',#38181,1.5);
#11209=VECTOR('',#38184,1.5);
#11210=VECTOR('',#38187,1.5);
#11211=VECTOR('',#38190,1.5);
#11212=VECTOR('',#38193,1.5);
#11213=VECTOR('',#38196,1.5);
#11214=VECTOR('',#38199,1.5);
#11215=VECTOR('',#38202,1.5);
#11216=VECTOR('',#38205,1.5);
#11217=VECTOR('',#38208,1.5);
#11218=VECTOR('',#38211,1.5);
#11219=VECTOR('',#38214,1.5);
#11220=VECTOR('',#38217,1.17775);
#11221=VECTOR('',#38222,1.17775);
#11222=VECTOR('',#38225,1.17775);
#11223=VECTOR('',#38228,1.17775);
#11224=VECTOR('',#38231,1.17775);
#11225=VECTOR('',#38234,1.17775);
#11226=VECTOR('',#38237,1.17775);
#11227=VECTOR('',#38240,1.17775);
#11228=VECTOR('',#38243,1.17775);
#11229=VECTOR('',#38246,1.17775);
#11230=VECTOR('',#38249,1.17775);
#11231=VECTOR('',#38252,1.17775);
#11232=VECTOR('',#38255,1.17775);
#11233=VECTOR('',#38258,1.17775);
#11234=VECTOR('',#38261,1.17775);
#11235=VECTOR('',#38264,1.17775);
#11236=VECTOR('',#38267,1.17775);
#11237=VECTOR('',#38270,1.17775);
#11238=VECTOR('',#38273,1.17775);
#11239=VECTOR('',#38276,1.17775);
#11240=VECTOR('',#38279,1.17775);
#11241=VECTOR('',#38282,1.17775);
#11242=VECTOR('',#38285,1.17775);
#11243=VECTOR('',#38288,1.17775);
#11244=VECTOR('',#38291,1.17775);
#11245=VECTOR('',#38294,1.17775);
#11246=VECTOR('',#38297,1.17775);
#11247=VECTOR('',#38300,1.17775);
#11248=VECTOR('',#38303,1.17775);
#11249=VECTOR('',#38306,1.17775);
#11250=VECTOR('',#38309,1.17775);
#11251=VECTOR('',#38312,1.17775);
#11252=VECTOR('',#38315,1.17775);
#11253=VECTOR('',#38318,1.17775);
#11254=VECTOR('',#38321,1.17775);
#11255=VECTOR('',#38324,1.17775);
#11256=VECTOR('',#38327,1.17775);
#11257=VECTOR('',#38330,1.17775);
#11258=VECTOR('',#38333,1.17775);
#11259=VECTOR('',#38336,1.17775);
#11260=VECTOR('',#38339,1.17775);
#11261=VECTOR('',#38342,1.17775);
#11262=VECTOR('',#38345,1.17775);
#11263=VECTOR('',#38348,1.17775);
#11264=VECTOR('',#38351,1.17775);
#11265=VECTOR('',#38354,1.17775);
#11266=VECTOR('',#38357,1.17775);
#11267=VECTOR('',#38360,1.17775);
#11268=VECTOR('',#38363,1.17775);
#11269=VECTOR('',#38366,1.17775);
#11270=VECTOR('',#38369,1.17775);
#11271=VECTOR('',#38372,1.17775);
#11272=VECTOR('',#38375,1.17775);
#11273=VECTOR('',#38378,1.17775);
#11274=VECTOR('',#38381,1.17775);
#11275=VECTOR('',#38384,1.17775);
#11276=VECTOR('',#38387,1.17775);
#11277=VECTOR('',#38390,1.17775);
#11278=VECTOR('',#38393,1.17775);
#11279=VECTOR('',#38396,1.17775);
#11280=VECTOR('',#38399,1.17775);
#11281=VECTOR('',#38402,1.17775);
#11282=VECTOR('',#38405,1.17775);
#11283=VECTOR('',#38408,1.17775);
#11284=VECTOR('',#38411,1.17775);
#11285=VECTOR('',#38414,1.17775);
#11286=VECTOR('',#38417,1.17775);
#11287=VECTOR('',#38420,1.17775);
#11288=VECTOR('',#38423,1.17775);
#11289=VECTOR('',#38456,10.);
#11290=VECTOR('',#38457,10.);
#11291=VECTOR('',#38458,10.);
#11292=VECTOR('',#38459,10.);
#11293=VECTOR('',#38464,10.);
#11294=VECTOR('',#38467,10.);
#11295=VECTOR('',#38468,10.);
#11296=VECTOR('',#38475,10.);
#11297=VECTOR('',#38476,10.);
#11298=VECTOR('',#38477,10.);
#11299=VECTOR('',#38478,10.);
#11300=VECTOR('',#38483,10.);
#11301=VECTOR('',#38486,10.);
#11302=VECTOR('',#38487,10.);
#11303=VECTOR('',#38494,10.);
#11304=VECTOR('',#38495,10.);
#11305=VECTOR('',#38496,10.);
#11306=VECTOR('',#38497,10.);
#11307=VECTOR('',#38502,10.);
#11308=VECTOR('',#38505,10.);
#11309=VECTOR('',#38506,10.);
#11310=VECTOR('',#38513,10.);
#11311=VECTOR('',#38514,10.);
#11312=VECTOR('',#38515,10.);
#11313=VECTOR('',#38516,10.);
#11314=VECTOR('',#38521,10.);
#11315=VECTOR('',#38524,10.);
#11316=VECTOR('',#38525,10.);
#11317=VECTOR('',#38532,10.);
#11318=VECTOR('',#38533,10.);
#11319=VECTOR('',#38534,10.);
#11320=VECTOR('',#38535,10.);
#11321=VECTOR('',#38540,10.);
#11322=VECTOR('',#38543,10.);
#11323=VECTOR('',#38544,10.);
#11324=VECTOR('',#38551,10.);
#11325=VECTOR('',#38552,10.);
#11326=VECTOR('',#38553,10.);
#11327=VECTOR('',#38554,10.);
#11328=VECTOR('',#38559,10.);
#11329=VECTOR('',#38562,10.);
#11330=VECTOR('',#38563,10.);
#11331=VECTOR('',#38570,10.);
#11332=VECTOR('',#38571,10.);
#11333=VECTOR('',#38572,10.);
#11334=VECTOR('',#38573,10.);
#11335=VECTOR('',#38578,10.);
#11336=VECTOR('',#38581,10.);
#11337=VECTOR('',#38582,10.);
#11338=VECTOR('',#38589,10.);
#11339=VECTOR('',#38590,10.);
#11340=VECTOR('',#38591,10.);
#11341=VECTOR('',#38592,10.);
#11342=VECTOR('',#38597,10.);
#11343=VECTOR('',#38600,10.);
#11344=VECTOR('',#38601,10.);
#11345=VECTOR('',#38608,10.);
#11346=VECTOR('',#38609,10.);
#11347=VECTOR('',#38610,10.);
#11348=VECTOR('',#38611,10.);
#11349=VECTOR('',#38616,10.);
#11350=VECTOR('',#38619,10.);
#11351=VECTOR('',#38620,10.);
#11352=VECTOR('',#38627,10.);
#11353=VECTOR('',#38628,10.);
#11354=VECTOR('',#38629,10.);
#11355=VECTOR('',#38630,10.);
#11356=VECTOR('',#38635,10.);
#11357=VECTOR('',#38638,10.);
#11358=VECTOR('',#38639,10.);
#11359=VECTOR('',#38646,10.);
#11360=VECTOR('',#38647,10.);
#11361=VECTOR('',#38648,10.);
#11362=VECTOR('',#38649,10.);
#11363=VECTOR('',#38654,10.);
#11364=VECTOR('',#38657,10.);
#11365=VECTOR('',#38658,10.);
#11366=VECTOR('',#38665,10.);
#11367=VECTOR('',#38666,10.);
#11368=VECTOR('',#38667,10.);
#11369=VECTOR('',#38668,10.);
#11370=VECTOR('',#38673,10.);
#11371=VECTOR('',#38676,10.);
#11372=VECTOR('',#38677,10.);
#11373=VECTOR('',#38684,10.);
#11374=VECTOR('',#38685,10.);
#11375=VECTOR('',#38686,10.);
#11376=VECTOR('',#38687,10.);
#11377=VECTOR('',#38692,10.);
#11378=VECTOR('',#38695,10.);
#11379=VECTOR('',#38696,10.);
#11380=VECTOR('',#38703,10.);
#11381=VECTOR('',#38704,10.);
#11382=VECTOR('',#38705,10.);
#11383=VECTOR('',#38706,10.);
#11384=VECTOR('',#38711,10.);
#11385=VECTOR('',#38714,10.);
#11386=VECTOR('',#38715,10.);
#11387=VECTOR('',#38722,10.);
#11388=VECTOR('',#38723,10.);
#11389=VECTOR('',#38724,10.);
#11390=VECTOR('',#38725,10.);
#11391=VECTOR('',#38730,10.);
#11392=VECTOR('',#38733,10.);
#11393=VECTOR('',#38734,10.);
#11394=VECTOR('',#38741,10.);
#11395=VECTOR('',#38742,10.);
#11396=VECTOR('',#38743,10.);
#11397=VECTOR('',#38744,10.);
#11398=VECTOR('',#38749,10.);
#11399=VECTOR('',#38752,10.);
#11400=VECTOR('',#38753,10.);
#11401=VECTOR('',#38760,10.);
#11402=VECTOR('',#38761,10.);
#11403=VECTOR('',#38762,10.);
#11404=VECTOR('',#38763,10.);
#11405=VECTOR('',#38768,10.);
#11406=VECTOR('',#38771,10.);
#11407=VECTOR('',#38772,10.);
#11408=VECTOR('',#38779,10.);
#11409=VECTOR('',#38780,10.);
#11410=VECTOR('',#38781,10.);
#11411=VECTOR('',#38782,10.);
#11412=VECTOR('',#38787,10.);
#11413=VECTOR('',#38792,10.);
#11414=VECTOR('',#38793,10.);
#11415=VECTOR('',#38802,10.);
#11416=VECTOR('',#38803,10.);
#11417=VECTOR('',#38804,10.);
#11418=VECTOR('',#38805,10.);
#11419=VECTOR('',#38810,10.);
#11420=VECTOR('',#38813,10.);
#11421=VECTOR('',#38814,10.);
#11422=VECTOR('',#38821,10.);
#11423=VECTOR('',#38822,10.);
#11424=VECTOR('',#38823,10.);
#11425=VECTOR('',#38824,10.);
#11426=VECTOR('',#38829,10.);
#11427=VECTOR('',#38832,10.);
#11428=VECTOR('',#38833,10.);
#11429=VECTOR('',#38840,10.);
#11430=VECTOR('',#38841,10.);
#11431=VECTOR('',#38842,10.);
#11432=VECTOR('',#38843,10.);
#11433=VECTOR('',#38848,10.);
#11434=VECTOR('',#38851,10.);
#11435=VECTOR('',#38852,10.);
#11436=VECTOR('',#38859,10.);
#11437=VECTOR('',#38860,10.);
#11438=VECTOR('',#38861,10.);
#11439=VECTOR('',#38862,10.);
#11440=VECTOR('',#38867,10.);
#11441=VECTOR('',#38870,10.);
#11442=VECTOR('',#38871,10.);
#11443=VECTOR('',#38878,10.);
#11444=VECTOR('',#38879,10.);
#11445=VECTOR('',#38880,10.);
#11446=VECTOR('',#38881,10.);
#11447=VECTOR('',#38886,10.);
#11448=VECTOR('',#38889,10.);
#11449=VECTOR('',#38890,10.);
#11450=VECTOR('',#38897,10.);
#11451=VECTOR('',#38898,10.);
#11452=VECTOR('',#38899,10.);
#11453=VECTOR('',#38900,10.);
#11454=VECTOR('',#38905,10.);
#11455=VECTOR('',#38908,10.);
#11456=VECTOR('',#38909,10.);
#11457=VECTOR('',#38916,10.);
#11458=VECTOR('',#38917,10.);
#11459=VECTOR('',#38918,10.);
#11460=VECTOR('',#38919,10.);
#11461=VECTOR('',#38924,10.);
#11462=VECTOR('',#38927,10.);
#11463=VECTOR('',#38928,10.);
#11464=VECTOR('',#38935,10.);
#11465=VECTOR('',#38936,10.);
#11466=VECTOR('',#38937,10.);
#11467=VECTOR('',#38938,10.);
#11468=VECTOR('',#38943,10.);
#11469=VECTOR('',#38946,10.);
#11470=VECTOR('',#38947,10.);
#11471=VECTOR('',#38954,10.);
#11472=VECTOR('',#38955,10.);
#11473=VECTOR('',#38956,10.);
#11474=VECTOR('',#38957,10.);
#11475=VECTOR('',#38962,10.);
#11476=VECTOR('',#38965,10.);
#11477=VECTOR('',#38966,10.);
#11478=VECTOR('',#38973,10.);
#11479=VECTOR('',#38974,10.);
#11480=VECTOR('',#38975,10.);
#11481=VECTOR('',#38976,10.);
#11482=VECTOR('',#38981,10.);
#11483=VECTOR('',#38984,10.);
#11484=VECTOR('',#38985,10.);
#11485=VECTOR('',#38992,10.);
#11486=VECTOR('',#38993,10.);
#11487=VECTOR('',#38994,10.);
#11488=VECTOR('',#38995,10.);
#11489=VECTOR('',#39000,10.);
#11490=VECTOR('',#39003,10.);
#11491=VECTOR('',#39004,10.);
#11492=VECTOR('',#39011,10.);
#11493=VECTOR('',#39012,10.);
#11494=VECTOR('',#39013,10.);
#11495=VECTOR('',#39014,10.);
#11496=VECTOR('',#39019,10.);
#11497=VECTOR('',#39022,10.);
#11498=VECTOR('',#39023,10.);
#11499=VECTOR('',#39030,10.);
#11500=VECTOR('',#39031,10.);
#11501=VECTOR('',#39032,10.);
#11502=VECTOR('',#39033,10.);
#11503=VECTOR('',#39038,10.);
#11504=VECTOR('',#39041,10.);
#11505=VECTOR('',#39042,10.);
#11506=VECTOR('',#39049,10.);
#11507=VECTOR('',#39050,10.);
#11508=VECTOR('',#39051,10.);
#11509=VECTOR('',#39052,10.);
#11510=VECTOR('',#39057,10.);
#11511=VECTOR('',#39060,10.);
#11512=VECTOR('',#39061,10.);
#11513=VECTOR('',#39068,10.);
#11514=VECTOR('',#39069,10.);
#11515=VECTOR('',#39070,10.);
#11516=VECTOR('',#39071,10.);
#11517=VECTOR('',#39076,10.);
#11518=VECTOR('',#39079,10.);
#11519=VECTOR('',#39080,10.);
#11520=VECTOR('',#39087,10.);
#11521=VECTOR('',#39088,10.);
#11522=VECTOR('',#39089,10.);
#11523=VECTOR('',#39090,10.);
#11524=VECTOR('',#39095,10.);
#11525=VECTOR('',#39098,10.);
#11526=VECTOR('',#39099,10.);
#11527=VECTOR('',#39106,10.);
#11528=VECTOR('',#39107,10.);
#11529=VECTOR('',#39108,10.);
#11530=VECTOR('',#39109,10.);
#11531=VECTOR('',#39114,10.);
#11532=VECTOR('',#39117,10.);
#11533=VECTOR('',#39118,10.);
#11534=VECTOR('',#39125,10.);
#11535=VECTOR('',#39126,10.);
#11536=VECTOR('',#39127,10.);
#11537=VECTOR('',#39128,10.);
#11538=VECTOR('',#39133,10.);
#11539=VECTOR('',#39136,10.);
#11540=VECTOR('',#39137,10.);
#11541=VECTOR('',#39144,0.625);
#11542=VECTOR('',#39149,10.);
#11543=VECTOR('',#39150,10.);
#11544=VECTOR('',#39151,10.);
#11545=VECTOR('',#39152,10.);
#11546=VECTOR('',#39155,10.);
#11547=VECTOR('',#39156,10.);
#11548=VECTOR('',#39157,10.);
#11549=VECTOR('',#39160,10.);
#11550=VECTOR('',#39161,10.);
#11551=VECTOR('',#39162,10.);
#11552=VECTOR('',#39165,10.);
#11553=VECTOR('',#39166,10.);
#11554=VECTOR('',#39167,10.);
#11555=VECTOR('',#39170,10.);
#11556=VECTOR('',#39171,10.);
#11557=VECTOR('',#39172,10.);
#11558=VECTOR('',#39175,10.);
#11559=VECTOR('',#39176,10.);
#11560=VECTOR('',#39185,1.3);
#11561=VECTOR('',#39190,2.75);
#11562=VECTOR('',#39191,2.75);
#11563=VECTOR('',#39196,2.6);
#11564=VECTOR('',#39203,10.);
#11565=VECTOR('',#39204,10.);
#11566=VECTOR('',#39205,10.);
#11567=VECTOR('',#39206,10.);
#11568=VECTOR('',#39209,10.);
#11569=VECTOR('',#39210,10.);
#11570=VECTOR('',#39211,10.);
#11571=VECTOR('',#39214,10.);
#11572=VECTOR('',#39215,10.);
#11573=VECTOR('',#39220,10.);
#11574=VECTOR('',#39229,10.);
#11575=VECTOR('',#39230,10.);
#11576=VECTOR('',#39233,10.);
#11577=VECTOR('',#39234,10.);
#11578=VECTOR('',#39235,10.);
#11579=VECTOR('',#39244,10.);
#11580=VECTOR('',#39245,10.);
#11581=VECTOR('',#39246,10.);
#11582=VECTOR('',#39247,10.);
#11583=VECTOR('',#39250,10.);
#11584=VECTOR('',#39251,10.);
#11585=VECTOR('',#39252,10.);
#11586=VECTOR('',#39255,10.);
#11587=VECTOR('',#39256,10.);
#11588=VECTOR('',#39259,10.);
#11589=VECTOR('',#39260,10.);
#11590=VECTOR('',#39261,10.);
#11591=VECTOR('',#39264,10.);
#11592=VECTOR('',#39265,10.);
#11593=VECTOR('',#39270,10.);
#11594=VECTOR('',#39279,10.);
#11595=VECTOR('',#39280,10.);
#11596=VECTOR('',#39281,10.);
#11597=VECTOR('',#39282,10.);
#11598=VECTOR('',#39285,10.);
#11599=VECTOR('',#39286,10.);
#11600=VECTOR('',#39287,10.);
#11601=VECTOR('',#39290,10.);
#11602=VECTOR('',#39297,10.);
#11603=VECTOR('',#39298,10.);
#11604=VECTOR('',#39299,10.);
#11605=VECTOR('',#39302,10.);
#11606=VECTOR('',#39303,10.);
#11607=VECTOR('',#39308,10.);
#11608=VECTOR('',#39317,10.);
#11609=VECTOR('',#39318,10.);
#11610=VECTOR('',#39321,10.);
#11611=VECTOR('',#39322,10.);
#11612=VECTOR('',#39325,10.);
#11613=VECTOR('',#39326,10.);
#11614=VECTOR('',#39329,10.);
#11615=VECTOR('',#39330,10.);
#11616=VECTOR('',#39331,10.);
#11617=VECTOR('',#39332,10.);
#11618=VECTOR('',#39335,10.);
#11619=VECTOR('',#39336,10.);
#11620=VECTOR('',#39337,10.);
#11621=VECTOR('',#39340,10.);
#11622=VECTOR('',#39341,10.);
#11623=VECTOR('',#39342,10.);
#11624=VECTOR('',#39345,10.);
#11625=VECTOR('',#39352,10.);
#11626=VECTOR('',#39353,10.);
#11627=VECTOR('',#39356,10.);
#11628=VECTOR('',#39363,10.);
#11629=VECTOR('',#39364,10.);
#11630=VECTOR('',#39367,10.);
#11631=VECTOR('',#39368,10.);
#11632=VECTOR('',#39369,10.);
#11633=VECTOR('',#39376,10.);
#11634=VECTOR('',#39379,10.);
#11635=VECTOR('',#39388,10.);
#11636=VECTOR('',#39393,7.05);
#11637=VECTOR('',#39400,7.);
#11638=VECTOR('',#39405,7.);
#11639=VECTOR('',#39408,7.);
#11640=VECTOR('',#39411,7.);
#11641=VECTOR('',#39414,7.);
#11642=VECTOR('',#39417,7.);
#11643=VECTOR('',#39420,7.);
#11644=VECTOR('',#39423,7.);
#11645=VECTOR('',#39426,7.);
#11646=VECTOR('',#39429,7.);
#11647=VECTOR('',#39432,7.);
#11648=VECTOR('',#39435,7.);
#11649=VECTOR('',#39438,7.);
#11650=VECTOR('',#39441,7.);
#11651=VECTOR('',#39444,7.);
#11652=VECTOR('',#39447,7.);
#11653=VECTOR('',#39450,6.21925);
#11654=VECTOR('',#39455,6.21925);
#11655=VECTOR('',#39460,6.21925);
#11656=VECTOR('',#39463,6.21925);
#11657=VECTOR('',#39466,6.21925);
#11658=VECTOR('',#39469,6.21925);
#11659=VECTOR('',#39472,6.21925);
#11660=VECTOR('',#39475,6.21925);
#11661=VECTOR('',#39478,6.21925);
#11662=VECTOR('',#39481,6.21925);
#11663=VECTOR('',#39484,6.21925);
#11664=VECTOR('',#39487,6.21925);
#11665=VECTOR('',#39490,6.21925);
#11666=VECTOR('',#39493,6.21925);
#11667=VECTOR('',#39496,6.21925);
#11668=VECTOR('',#39499,6.21925);
#11669=VECTOR('',#39504,5.3);
#11670=VECTOR('',#39515,5.05);
#11671=VECTOR('',#39516,10.);
#11672=VECTOR('',#39517,10.);
#11673=VECTOR('',#39524,5.3);
#11674=VECTOR('',#39531,10.);
#11675=VECTOR('',#39534,1.55);
#11676=VECTOR('',#39543,12.);
#11677=VECTOR('',#39562,6.65);
#11678=VECTOR('',#39573,11.75);
#11679=VECTOR('',#39578,11.75);
#11680=VECTOR('',#39587,8.);
#11681=VECTOR('',#39590,7.8);
#11682=VECTOR('',#39595,5.);
#11683=VECTOR('',#39600,5.);
#11684=VECTOR('',#39603,5.);
#11685=VECTOR('',#39606,5.);
#11686=VECTOR('',#39609,5.);
#11687=VECTOR('',#39612,5.);
#11688=VECTOR('',#39615,5.);
#11689=VECTOR('',#39618,5.);
#11690=VECTOR('',#39621,5.);
#11691=VECTOR('',#39624,5.);
#11692=VECTOR('',#39627,5.);
#11693=VECTOR('',#39630,5.);
#11694=VECTOR('',#39633,5.);
#11695=VECTOR('',#39636,5.);
#11696=VECTOR('',#39639,5.);
#11697=VECTOR('',#39642,5.);
#11698=VECTOR('',#39645,5.);
#11699=VECTOR('',#39648,5.);
#11700=VECTOR('',#39651,5.);
#11701=VECTOR('',#39654,5.);
#11702=VECTOR('',#39657,5.);
#11703=VECTOR('',#39660,5.);
#11704=VECTOR('',#39663,5.);
#11705=VECTOR('',#39666,5.);
#11706=VECTOR('',#39669,5.);
#11707=VECTOR('',#39672,5.);
#11708=VECTOR('',#39675,5.);
#11709=VECTOR('',#39678,5.);
#11710=VECTOR('',#39681,5.);
#11711=VECTOR('',#39684,5.);
#11712=VECTOR('',#39687,5.);
#11713=VECTOR('',#39690,5.);
#11714=VECTOR('',#39693,5.);
#11715=VECTOR('',#39696,5.);
#11716=VECTOR('',#39699,5.);
#11717=VECTOR('',#39702,5.);
#11718=VECTOR('',#39705,5.);
#11719=VECTOR('',#39708,5.);
#11720=VECTOR('',#39711,5.);
#11721=VECTOR('',#39714,5.);
#11722=VECTOR('',#39717,5.);
#11723=VECTOR('',#39720,5.);
#11724=VECTOR('',#39723,5.);
#11725=VECTOR('',#39726,5.);
#11726=VECTOR('',#39729,5.);
#11727=VECTOR('',#39732,5.);
#11728=VECTOR('',#39735,5.);
#11729=VECTOR('',#39738,5.);
#11730=VECTOR('',#39741,5.);
#11731=VECTOR('',#39744,5.);
#11732=VECTOR('',#39747,5.);
#11733=VECTOR('',#39750,5.);
#11734=VECTOR('',#39753,5.);
#11735=VECTOR('',#39756,5.);
#11736=VECTOR('',#39759,5.);
#11737=VECTOR('',#39762,5.);
#11738=VECTOR('',#39765,5.);
#11739=VECTOR('',#39768,5.);
#11740=VECTOR('',#39771,5.);
#11741=VECTOR('',#39774,5.);
#11742=VECTOR('',#39777,5.);
#11743=VECTOR('',#39780,5.);
#11744=VECTOR('',#39783,5.);
#11745=VECTOR('',#39786,5.);
#11746=VECTOR('',#39789,5.);
#11747=VECTOR('',#39792,5.);
#11748=VECTOR('',#39795,5.);
#11749=VECTOR('',#39798,5.);
#11750=VECTOR('',#39801,5.);
#11751=VECTOR('',#39804,5.);
#11752=VECTOR('',#39807,5.);
#11753=VECTOR('',#39810,5.);
#11754=VECTOR('',#39813,5.);
#11755=VECTOR('',#39816,5.);
#11756=VECTOR('',#39819,5.);
#11757=VECTOR('',#39822,4.52375);
#11758=VECTOR('',#39827,4.52375);
#11759=VECTOR('',#39830,4.52375);
#11760=VECTOR('',#39833,4.52375);
#11761=VECTOR('',#39836,4.52375);
#11762=VECTOR('',#39839,4.52375);
#11763=VECTOR('',#39842,4.52375);
#11764=VECTOR('',#39845,4.52375);
#11765=VECTOR('',#39848,4.52375);
#11766=VECTOR('',#39851,4.52375);
#11767=VECTOR('',#39854,4.52375);
#11768=VECTOR('',#39857,4.52375);
#11769=VECTOR('',#39860,4.52375);
#11770=VECTOR('',#39863,4.52375);
#11771=VECTOR('',#39866,4.52375);
#11772=VECTOR('',#39869,4.52375);
#11773=VECTOR('',#39872,4.52375);
#11774=VECTOR('',#39875,4.52375);
#11775=VECTOR('',#39878,4.52375);
#11776=VECTOR('',#39881,4.52375);
#11777=VECTOR('',#39884,4.52375);
#11778=VECTOR('',#39887,4.52375);
#11779=VECTOR('',#39890,4.52375);
#11780=VECTOR('',#39893,4.52375);
#11781=VECTOR('',#39896,4.52375);
#11782=VECTOR('',#39899,4.52375);
#11783=VECTOR('',#39902,4.52375);
#11784=VECTOR('',#39905,4.52375);
#11785=VECTOR('',#39908,4.52375);
#11786=VECTOR('',#39911,4.52375);
#11787=VECTOR('',#39914,4.52375);
#11788=VECTOR('',#39917,4.52375);
#11789=VECTOR('',#39920,4.52375);
#11790=VECTOR('',#39923,4.52375);
#11791=VECTOR('',#39926,4.52375);
#11792=VECTOR('',#39929,4.52375);
#11793=VECTOR('',#39932,4.52375);
#11794=VECTOR('',#39935,4.52375);
#11795=VECTOR('',#39938,4.52375);
#11796=VECTOR('',#39941,4.52375);
#11797=VECTOR('',#39944,4.52375);
#11798=VECTOR('',#39947,4.52375);
#11799=VECTOR('',#39950,4.52375);
#11800=VECTOR('',#39953,4.52375);
#11801=VECTOR('',#39956,4.52375);
#11802=VECTOR('',#39959,4.52375);
#11803=VECTOR('',#39962,4.52375);
#11804=VECTOR('',#39965,4.52375);
#11805=VECTOR('',#39968,4.52375);
#11806=VECTOR('',#39971,4.52375);
#11807=VECTOR('',#39974,4.52375);
#11808=VECTOR('',#39977,4.52375);
#11809=VECTOR('',#39980,4.52375);
#11810=VECTOR('',#39983,4.52375);
#11811=VECTOR('',#39986,4.52375);
#11812=VECTOR('',#39989,4.52375);
#11813=VECTOR('',#39992,4.52375);
#11814=VECTOR('',#39995,4.52375);
#11815=VECTOR('',#39998,4.52375);
#11816=VECTOR('',#40001,4.52375);
#11817=VECTOR('',#40004,4.52375);
#11818=VECTOR('',#40007,4.52375);
#11819=VECTOR('',#40010,4.52375);
#11820=VECTOR('',#40013,4.52375);
#11821=VECTOR('',#40016,4.52375);
#11822=VECTOR('',#40019,4.52375);
#11823=VECTOR('',#40022,4.52375);
#11824=VECTOR('',#40025,4.52375);
#11825=VECTOR('',#40028,4.52375);
#11826=VECTOR('',#40031,4.52375);
#11827=VECTOR('',#40034,4.52375);
#11828=VECTOR('',#40037,4.52375);
#11829=VECTOR('',#40040,4.52375);
#11830=VECTOR('',#40043,4.52375);
#11831=VECTOR('',#40046,4.52375);
#11832=VECTOR('',#40067,2.5);
#11833=VECTOR('',#40072,3.75);
#11834=VECTOR('',#40081,4.75);
#11835=VECTOR('',#40094,5.3);
#11836=VECTOR('',#40103,5.05);
#11837=VECTOR('',#40110,10.);
#11838=VECTOR('',#40111,10.);
#11839=VECTOR('',#40112,10.);
#11840=VECTOR('',#40117,10.);
#11841=VECTOR('',#40122,10.);
#11842=VECTOR('',#40123,10.);
#11843=VECTOR('',#40134,10.);
#11844=VECTOR('',#40137,10.);
#11845=VECTOR('',#40140,10.);
#11846=VECTOR('',#40143,10.);
#11847=VECTOR('',#40146,10.);
#11848=VECTOR('',#40149,10.);
#11849=VECTOR('',#40152,10.);
#11850=VECTOR('',#40155,10.);
#11851=VECTOR('',#40158,10.);
#11852=VECTOR('',#40161,10.);
#11853=VECTOR('',#40164,10.);
#11854=VECTOR('',#40167,10.);
#11855=VECTOR('',#40170,10.);
#11856=VECTOR('',#40173,10.);
#11857=VECTOR('',#40176,9.5);
#11858=VECTOR('',#40181,10.);
#11859=VECTOR('',#40184,10.);
#11860=VECTOR('',#40187,10.);
#11861=VECTOR('',#40190,10.);
#11862=VECTOR('',#40193,10.);
#11863=VECTOR('',#40196,10.);
#11864=VECTOR('',#40199,10.);
#11865=VECTOR('',#40202,10.);
#11866=VECTOR('',#40205,10.);
#11867=VECTOR('',#40208,10.);
#11868=VECTOR('',#40211,10.);
#11869=VECTOR('',#40214,10.);
#11870=VECTOR('',#40217,10.);
#11871=VECTOR('',#40220,10.);
#11872=VECTOR('',#40225,10.);
#11873=VECTOR('',#40226,10.);
#11874=VECTOR('',#40231,10.);
#11875=VECTOR('',#40236,10.);
#11876=VECTOR('',#40243,10.);
#11877=VECTOR('',#40244,10.);
#11878=VECTOR('',#40249,10.);
#11879=VECTOR('',#40254,10.);
#11880=VECTOR('',#40261,10.);
#11881=VECTOR('',#40262,10.);
#11882=VECTOR('',#40267,10.);
#11883=VECTOR('',#40272,10.);
#11884=VECTOR('',#40279,10.);
#11885=VECTOR('',#40280,10.);
#11886=VECTOR('',#40285,10.);
#11887=VECTOR('',#40290,10.);
#11888=VECTOR('',#40297,10.);
#11889=VECTOR('',#40298,10.);
#11890=VECTOR('',#40303,10.);
#11891=VECTOR('',#40308,10.);
#11892=VECTOR('',#40315,10.);
#11893=VECTOR('',#40316,10.);
#11894=VECTOR('',#40321,10.);
#11895=VECTOR('',#40326,10.);
#11896=VECTOR('',#40333,10.);
#11897=VECTOR('',#40334,10.);
#11898=VECTOR('',#40339,10.);
#11899=VECTOR('',#40344,10.);
#11900=VECTOR('',#40351,10.);
#11901=VECTOR('',#40352,10.);
#11902=VECTOR('',#40357,10.);
#11903=VECTOR('',#40362,10.);
#11904=VECTOR('',#40369,10.);
#11905=VECTOR('',#40370,10.);
#11906=VECTOR('',#40375,10.);
#11907=VECTOR('',#40380,10.);
#11908=VECTOR('',#40387,10.);
#11909=VECTOR('',#40388,10.);
#11910=VECTOR('',#40393,10.);
#11911=VECTOR('',#40398,10.);
#11912=VECTOR('',#40405,10.);
#11913=VECTOR('',#40406,10.);
#11914=VECTOR('',#40411,10.);
#11915=VECTOR('',#40416,10.);
#11916=VECTOR('',#40423,10.);
#11917=VECTOR('',#40424,10.);
#11918=VECTOR('',#40429,10.);
#11919=VECTOR('',#40434,10.);
#11920=VECTOR('',#40441,10.);
#11921=VECTOR('',#40442,10.);
#11922=VECTOR('',#40447,10.);
#11923=VECTOR('',#40452,10.);
#11924=VECTOR('',#40459,10.);
#11925=VECTOR('',#40460,10.);
#11926=VECTOR('',#40465,10.);
#11927=VECTOR('',#40470,10.);
#11928=VECTOR('',#40473,10.);
#11929=VECTOR('',#40474,10.);
#11930=VECTOR('',#40475,10.);
#11931=VECTOR('',#40476,10.);
#11932=VECTOR('',#40479,10.);
#11933=VECTOR('',#40480,10.);
#11934=VECTOR('',#40481,10.);
#11935=VECTOR('',#40484,10.);
#11936=VECTOR('',#40485,10.);
#11937=VECTOR('',#40486,10.);
#11938=VECTOR('',#40487,10.);
#11939=VECTOR('',#40490,10.);
#11940=VECTOR('',#40491,10.);
#11941=VECTOR('',#40492,10.);
#11942=VECTOR('',#40495,10.);
#11943=VECTOR('',#40496,10.);
#11944=VECTOR('',#40499,10.);
#11945=VECTOR('',#40500,10.);
#11946=VECTOR('',#40503,10.);
#11947=VECTOR('',#40504,10.);
#11948=VECTOR('',#40505,10.);
#11949=VECTOR('',#40508,10.);
#11950=VECTOR('',#40509,10.);
#11951=VECTOR('',#40512,10.);
#11952=VECTOR('',#40513,10.);
#11953=VECTOR('',#40520,10.);
#11954=VECTOR('',#40521,10.);
#11955=VECTOR('',#40524,10.);
#11956=VECTOR('',#40525,10.);
#11957=VECTOR('',#40528,10.);
#11958=VECTOR('',#40567,7.8);
#11959=VECTOR('',#40572,8.);
#11960=VECTOR('',#40579,9.25);
#11961=VECTOR('',#40586,1.5);
#11962=VECTOR('',#40591,1.5);
#11963=VECTOR('',#40594,1.5);
#11964=VECTOR('',#40597,1.5);
#11965=VECTOR('',#40600,1.5);
#11966=VECTOR('',#40603,1.5);
#11967=VECTOR('',#40606,1.5);
#11968=VECTOR('',#40609,1.17775);
#11969=VECTOR('',#40614,1.17775);
#11970=VECTOR('',#40617,1.17775);
#11971=VECTOR('',#40620,1.17775);
#11972=VECTOR('',#40623,1.17775);
#11973=VECTOR('',#40626,1.17775);
#11974=VECTOR('',#40645,10.);
#11975=VECTOR('',#40646,10.);
#11976=VECTOR('',#40647,10.);
#11977=VECTOR('',#40648,10.);
#11978=VECTOR('',#40651,10.);
#11979=VECTOR('',#40652,10.);
#11980=VECTOR('',#40653,10.);
#11981=VECTOR('',#40656,10.);
#11982=VECTOR('',#40657,10.);
#11983=VECTOR('',#40658,10.);
#11984=VECTOR('',#40661,10.);
#11985=VECTOR('',#40662,10.);
#11986=VECTOR('',#40663,10.);
#11987=VECTOR('',#40666,10.);
#11988=VECTOR('',#40667,10.);
#11989=VECTOR('',#40668,10.);
#11990=VECTOR('',#40671,10.);
#11991=VECTOR('',#40672,10.);
#11992=VECTOR('',#40681,1.275);
#11993=VECTOR('',#40690,1.35);
#11994=VERTEX_POINT('',#40768);
#11995=VERTEX_POINT('',#40769);
#11996=VERTEX_POINT('',#40771);
#11997=VERTEX_POINT('',#40773);
#11998=VERTEX_POINT('',#40775);
#11999=VERTEX_POINT('',#40777);
#12000=VERTEX_POINT('',#40781);
#12001=VERTEX_POINT('',#40783);
#12002=VERTEX_POINT('',#40787);
#12003=VERTEX_POINT('',#40789);
#12004=VERTEX_POINT('',#40791);
#12005=VERTEX_POINT('',#40795);
#12006=VERTEX_POINT('',#40797);
#12007=VERTEX_POINT('',#40801);
#12008=VERTEX_POINT('',#40803);
#12009=VERTEX_POINT('',#40805);
#12010=VERTEX_POINT('',#40809);
#12011=VERTEX_POINT('',#40811);
#12012=VERTEX_POINT('',#40815);
#12013=VERTEX_POINT('',#40817);
#12014=VERTEX_POINT('',#40819);
#12015=VERTEX_POINT('',#40823);
#12016=VERTEX_POINT('',#40826);
#12017=VERTEX_POINT('',#40827);
#12018=VERTEX_POINT('',#40829);
#12019=VERTEX_POINT('',#40831);
#12020=VERTEX_POINT('',#40833);
#12021=VERTEX_POINT('',#40835);
#12022=VERTEX_POINT('',#40837);
#12023=VERTEX_POINT('',#40839);
#12024=VERTEX_POINT('',#40841);
#12025=VERTEX_POINT('',#40843);
#12026=VERTEX_POINT('',#40845);
#12027=VERTEX_POINT('',#40847);
#12028=VERTEX_POINT('',#40850);
#12029=VERTEX_POINT('',#40851);
#12030=VERTEX_POINT('',#40853);
#12031=VERTEX_POINT('',#40855);
#12032=VERTEX_POINT('',#40857);
#12033=VERTEX_POINT('',#40859);
#12034=VERTEX_POINT('',#40861);
#12035=VERTEX_POINT('',#40865);
#12036=VERTEX_POINT('',#40869);
#12037=VERTEX_POINT('',#40873);
#12038=VERTEX_POINT('',#40877);
#12039=VERTEX_POINT('',#40881);
#12040=VERTEX_POINT('',#40885);
#12041=VERTEX_POINT('',#40889);
#12042=VERTEX_POINT('',#40891);
#12043=VERTEX_POINT('',#40893);
#12044=VERTEX_POINT('',#40895);
#12045=VERTEX_POINT('',#40899);
#12046=VERTEX_POINT('',#40903);
#12047=VERTEX_POINT('',#40910);
#12048=VERTEX_POINT('',#40911);
#12049=VERTEX_POINT('',#40913);
#12050=VERTEX_POINT('',#40915);
#12051=VERTEX_POINT('',#40917);
#12052=VERTEX_POINT('',#40919);
#12053=VERTEX_POINT('',#40921);
#12054=VERTEX_POINT('',#40923);
#12055=VERTEX_POINT('',#40925);
#12056=VERTEX_POINT('',#40927);
#12057=VERTEX_POINT('',#40929);
#12058=VERTEX_POINT('',#40931);
#12059=VERTEX_POINT('',#40934);
#12060=VERTEX_POINT('',#40935);
#12061=VERTEX_POINT('',#40939);
#12062=VERTEX_POINT('',#40943);
#12063=VERTEX_POINT('',#40945);
#12064=VERTEX_POINT('',#40947);
#12065=VERTEX_POINT('',#40949);
#12066=VERTEX_POINT('',#40951);
#12067=VERTEX_POINT('',#40955);
#12068=VERTEX_POINT('',#40959);
#12069=VERTEX_POINT('',#40963);
#12070=VERTEX_POINT('',#40968);
#12071=VERTEX_POINT('',#40969);
#12072=VERTEX_POINT('',#40973);
#12073=VERTEX_POINT('',#40977);
#12074=VERTEX_POINT('',#40981);
#12075=VERTEX_POINT('',#40983);
#12076=VERTEX_POINT('',#40987);
#12077=VERTEX_POINT('',#40991);
#12078=VERTEX_POINT('',#40995);
#12079=VERTEX_POINT('',#40999);
#12080=VERTEX_POINT('',#41003);
#12081=VERTEX_POINT('',#41007);
#12082=VERTEX_POINT('',#41011);
#12083=VERTEX_POINT('',#41015);
#12084=VERTEX_POINT('',#41019);
#12085=VERTEX_POINT('',#41023);
#12086=VERTEX_POINT('',#41027);
#12087=VERTEX_POINT('',#41031);
#12088=VERTEX_POINT('',#41035);
#12089=VERTEX_POINT('',#41039);
#12090=VERTEX_POINT('',#41043);
#12091=VERTEX_POINT('',#41047);
#12092=VERTEX_POINT('',#41051);
#12093=VERTEX_POINT('',#41055);
#12094=VERTEX_POINT('',#41057);
#12095=VERTEX_POINT('',#41061);
#12096=VERTEX_POINT('',#41065);
#12097=VERTEX_POINT('',#41069);
#12098=VERTEX_POINT('',#41073);
#12099=VERTEX_POINT('',#41077);
#12100=VERTEX_POINT('',#41081);
#12101=VERTEX_POINT('',#41085);
#12102=VERTEX_POINT('',#41089);
#12103=VERTEX_POINT('',#41093);
#12104=VERTEX_POINT('',#41097);
#12105=VERTEX_POINT('',#41104);
#12106=VERTEX_POINT('',#41105);
#12107=VERTEX_POINT('',#41109);
#12108=VERTEX_POINT('',#41113);
#12109=VERTEX_POINT('',#41117);
#12110=VERTEX_POINT('',#41119);
#12111=VERTEX_POINT('',#41123);
#12112=VERTEX_POINT('',#41127);
#12113=VERTEX_POINT('',#41131);
#12114=VERTEX_POINT('',#41135);
#12115=VERTEX_POINT('',#41139);
#12116=VERTEX_POINT('',#41143);
#12117=VERTEX_POINT('',#41147);
#12118=VERTEX_POINT('',#41149);
#12119=VERTEX_POINT('',#41153);
#12120=VERTEX_POINT('',#41157);
#12121=VERTEX_POINT('',#41161);
#12122=VERTEX_POINT('',#41165);
#12123=VERTEX_POINT('',#41169);
#12124=VERTEX_POINT('',#41173);
#12125=VERTEX_POINT('',#41177);
#12126=VERTEX_POINT('',#41179);
#12127=VERTEX_POINT('',#41183);
#12128=VERTEX_POINT('',#41187);
#12129=VERTEX_POINT('',#41191);
#12130=VERTEX_POINT('',#41195);
#12131=VERTEX_POINT('',#41199);
#12132=VERTEX_POINT('',#41203);
#12133=VERTEX_POINT('',#41207);
#12134=VERTEX_POINT('',#41211);
#12135=VERTEX_POINT('',#41218);
#12136=VERTEX_POINT('',#41219);
#12137=VERTEX_POINT('',#41221);
#12138=VERTEX_POINT('',#41223);
#12139=VERTEX_POINT('',#41226);
#12140=VERTEX_POINT('',#41227);
#12141=VERTEX_POINT('',#41231);
#12142=VERTEX_POINT('',#41235);
#12143=VERTEX_POINT('',#41239);
#12144=VERTEX_POINT('',#41241);
#12145=VERTEX_POINT('',#41245);
#12146=VERTEX_POINT('',#41249);
#12147=VERTEX_POINT('',#41253);
#12148=VERTEX_POINT('',#41257);
#12149=VERTEX_POINT('',#41261);
#12150=VERTEX_POINT('',#41265);
#12151=VERTEX_POINT('',#41269);
#12152=VERTEX_POINT('',#41273);
#12153=VERTEX_POINT('',#41277);
#12154=VERTEX_POINT('',#41281);
#12155=VERTEX_POINT('',#41285);
#12156=VERTEX_POINT('',#41289);
#12157=VERTEX_POINT('',#41293);
#12158=VERTEX_POINT('',#41297);
#12159=VERTEX_POINT('',#41301);
#12160=VERTEX_POINT('',#41305);
#12161=VERTEX_POINT('',#41309);
#12162=VERTEX_POINT('',#41313);
#12163=VERTEX_POINT('',#41315);
#12164=VERTEX_POINT('',#41319);
#12165=VERTEX_POINT('',#41323);
#12166=VERTEX_POINT('',#41327);
#12167=VERTEX_POINT('',#41331);
#12168=VERTEX_POINT('',#41335);
#12169=VERTEX_POINT('',#41339);
#12170=VERTEX_POINT('',#41343);
#12171=VERTEX_POINT('',#41347);
#12172=VERTEX_POINT('',#41351);
#12173=VERTEX_POINT('',#41355);
#12174=VERTEX_POINT('',#41363);
#12175=VERTEX_POINT('',#41364);
#12176=VERTEX_POINT('',#41366);
#12177=VERTEX_POINT('',#41371);
#12178=VERTEX_POINT('',#41373);
#12179=VERTEX_POINT('',#41377);
#12180=VERTEX_POINT('',#41379);
#12181=VERTEX_POINT('',#41383);
#12182=VERTEX_POINT('',#41384);
#12183=VERTEX_POINT('',#41386);
#12184=VERTEX_POINT('',#41390);
#12185=VERTEX_POINT('',#41393);
#12186=VERTEX_POINT('',#41397);
#12187=VERTEX_POINT('',#41401);
#12188=VERTEX_POINT('',#41405);
#12189=VERTEX_POINT('',#41407);
#12190=VERTEX_POINT('',#41411);
#12191=VERTEX_POINT('',#41415);
#12192=VERTEX_POINT('',#41418);
#12193=VERTEX_POINT('',#41420);
#12194=VERTEX_POINT('',#41424);
#12195=VERTEX_POINT('',#41428);
#12196=VERTEX_POINT('',#41431);
#12197=VERTEX_POINT('',#41433);
#12198=VERTEX_POINT('',#41437);
#12199=VERTEX_POINT('',#41441);
#12200=VERTEX_POINT('',#41444);
#12201=VERTEX_POINT('',#41446);
#12202=VERTEX_POINT('',#41450);
#12203=VERTEX_POINT('',#41454);
#12204=VERTEX_POINT('',#41457);
#12205=VERTEX_POINT('',#41461);
#12206=VERTEX_POINT('',#41466);
#12207=VERTEX_POINT('',#41470);
#12208=VERTEX_POINT('',#41471);
#12209=VERTEX_POINT('',#41476);
#12210=VERTEX_POINT('',#41477);
#12211=VERTEX_POINT('',#41479);
#12212=VERTEX_POINT('',#41483);
#12213=VERTEX_POINT('',#41485);
#12214=VERTEX_POINT('',#41508);
#12215=VERTEX_POINT('',#41510);
#12216=VERTEX_POINT('',#41512);
#12217=VERTEX_POINT('',#41514);
#12218=VERTEX_POINT('',#41516);
#12219=VERTEX_POINT('',#41518);
#12220=VERTEX_POINT('',#41520);
#12221=VERTEX_POINT('',#41522);
#12222=VERTEX_POINT('',#41524);
#12223=VERTEX_POINT('',#41526);
#12224=VERTEX_POINT('',#41528);
#12225=VERTEX_POINT('',#41530);
#12226=VERTEX_POINT('',#41532);
#12227=VERTEX_POINT('',#41534);
#12228=VERTEX_POINT('',#41536);
#12229=VERTEX_POINT('',#41538);
#12230=VERTEX_POINT('',#41540);
#12231=VERTEX_POINT('',#41544);
#12232=VERTEX_POINT('',#41546);
#12233=VERTEX_POINT('',#41548);
#12234=VERTEX_POINT('',#41550);
#12235=VERTEX_POINT('',#41552);
#12236=VERTEX_POINT('',#41555);
#12237=VERTEX_POINT('',#41557);
#12238=VERTEX_POINT('',#41561);
#12239=VERTEX_POINT('',#41565);
#12240=VERTEX_POINT('',#41569);
#12241=VERTEX_POINT('',#41573);
#12242=VERTEX_POINT('',#41577);
#12243=VERTEX_POINT('',#41581);
#12244=VERTEX_POINT('',#41585);
#12245=VERTEX_POINT('',#41589);
#12246=VERTEX_POINT('',#41593);
#12247=VERTEX_POINT('',#41597);
#12248=VERTEX_POINT('',#41604);
#12249=VERTEX_POINT('',#41606);
#12250=VERTEX_POINT('',#41615);
#12251=VERTEX_POINT('',#41626);
#12252=VERTEX_POINT('',#41637);
#12253=VERTEX_POINT('',#41648);
#12254=VERTEX_POINT('',#41654);
#12255=VERTEX_POINT('',#41658);
#12256=VERTEX_POINT('',#41662);
#12257=VERTEX_POINT('',#41671);
#12258=VERTEX_POINT('',#41682);
#12259=VERTEX_POINT('',#41693);
#12260=VERTEX_POINT('',#41704);
#12261=VERTEX_POINT('',#41715);
#12262=VERTEX_POINT('',#41726);
#12263=VERTEX_POINT('',#41737);
#12264=VERTEX_POINT('',#41743);
#12265=VERTEX_POINT('',#41747);
#12266=VERTEX_POINT('',#41751);
#12267=VERTEX_POINT('',#41758);
#12268=VERTEX_POINT('',#41760);
#12269=VERTEX_POINT('',#41764);
#12270=VERTEX_POINT('',#41768);
#12271=VERTEX_POINT('',#41772);
#12272=VERTEX_POINT('',#41776);
#12273=VERTEX_POINT('',#41780);
#12274=VERTEX_POINT('',#41784);
#12275=VERTEX_POINT('',#41788);
#12276=VERTEX_POINT('',#41792);
#12277=VERTEX_POINT('',#41796);
#12278=VERTEX_POINT('',#41800);
#12279=VERTEX_POINT('',#41812);
#12280=VERTEX_POINT('',#41814);
#12281=VERTEX_POINT('',#41825);
#12282=VERTEX_POINT('',#41831);
#12283=VERTEX_POINT('',#41840);
#12284=VERTEX_POINT('',#41851);
#12285=VERTEX_POINT('',#41862);
#12286=VERTEX_POINT('',#41868);
#12287=VERTEX_POINT('',#41872);
#12288=VERTEX_POINT('',#41876);
#12289=VERTEX_POINT('',#41880);
#12290=VERTEX_POINT('',#41899);
#12291=VERTEX_POINT('',#41901);
#12292=VERTEX_POINT('',#41912);
#12293=VERTEX_POINT('',#41923);
#12294=VERTEX_POINT('',#41934);
#12295=VERTEX_POINT('',#41945);
#12296=VERTEX_POINT('',#41956);
#12297=VERTEX_POINT('',#41967);
#12298=VERTEX_POINT('',#41978);
#12299=VERTEX_POINT('',#41989);
#12300=VERTEX_POINT('',#42000);
#12301=VERTEX_POINT('',#42011);
#12302=VERTEX_POINT('',#42022);
#12303=VERTEX_POINT('',#42033);
#12304=VERTEX_POINT('',#42039);
#12305=VERTEX_POINT('',#42048);
#12306=VERTEX_POINT('',#42059);
#12307=VERTEX_POINT('',#42070);
#12308=VERTEX_POINT('',#42081);
#12309=VERTEX_POINT('',#42092);
#12310=VERTEX_POINT('',#42103);
#12311=VERTEX_POINT('',#42114);
#12312=VERTEX_POINT('',#42125);
#12313=VERTEX_POINT('',#42136);
#12314=VERTEX_POINT('',#42147);
#12315=VERTEX_POINT('',#42158);
#12316=VERTEX_POINT('',#42169);
#12317=VERTEX_POINT('',#42180);
#12318=VERTEX_POINT('',#42191);
#12319=VERTEX_POINT('',#42202);
#12320=VERTEX_POINT('',#42213);
#12321=VERTEX_POINT('',#42224);
#12322=VERTEX_POINT('',#42235);
#12323=VERTEX_POINT('',#42241);
#12324=VERTEX_POINT('',#42250);
#12325=VERTEX_POINT('',#42271);
#12326=VERTEX_POINT('',#42273);
#12327=VERTEX_POINT('',#42284);
#12328=VERTEX_POINT('',#42295);
#12329=VERTEX_POINT('',#42306);
#12330=VERTEX_POINT('',#42317);
#12331=VERTEX_POINT('',#42328);
#12332=VERTEX_POINT('',#42339);
#12333=VERTEX_POINT('',#42350);
#12334=VERTEX_POINT('',#42361);
#12335=VERTEX_POINT('',#42372);
#12336=VERTEX_POINT('',#42383);
#12337=VERTEX_POINT('',#42389);
#12338=VERTEX_POINT('',#42398);
#12339=VERTEX_POINT('',#42409);
#12340=VERTEX_POINT('',#42420);
#12341=VERTEX_POINT('',#42431);
#12342=VERTEX_POINT('',#42442);
#12343=VERTEX_POINT('',#42453);
#12344=VERTEX_POINT('',#42464);
#12345=VERTEX_POINT('',#42470);
#12346=VERTEX_POINT('',#42479);
#12347=VERTEX_POINT('',#42490);
#12348=VERTEX_POINT('',#42501);
#12349=VERTEX_POINT('',#42512);
#12350=VERTEX_POINT('',#42523);
#12351=VERTEX_POINT('',#42534);
#12352=VERTEX_POINT('',#42545);
#12353=VERTEX_POINT('',#42551);
#12354=VERTEX_POINT('',#42560);
#12355=VERTEX_POINT('',#42576);
#12356=VERTEX_POINT('',#42578);
#12357=VERTEX_POINT('',#42582);
#12358=VERTEX_POINT('',#42586);
#12359=VERTEX_POINT('',#42598);
#12360=VERTEX_POINT('',#42600);
#12361=VERTEX_POINT('',#42611);
#12362=VERTEX_POINT('',#42622);
#12363=VERTEX_POINT('',#42633);
#12364=VERTEX_POINT('',#42644);
#12365=VERTEX_POINT('',#42655);
#12366=VERTEX_POINT('',#42666);
#12367=VERTEX_POINT('',#42677);
#12368=VERTEX_POINT('',#42688);
#12369=VERTEX_POINT('',#42699);
#12370=VERTEX_POINT('',#42710);
#12371=VERTEX_POINT('',#42721);
#12372=VERTEX_POINT('',#42732);
#12373=VERTEX_POINT('',#42738);
#12374=VERTEX_POINT('',#42747);
#12375=VERTEX_POINT('',#42758);
#12376=VERTEX_POINT('',#42769);
#12377=VERTEX_POINT('',#42780);
#12378=VERTEX_POINT('',#42791);
#12379=VERTEX_POINT('',#42802);
#12380=VERTEX_POINT('',#42813);
#12381=VERTEX_POINT('',#42824);
#12382=VERTEX_POINT('',#42835);
#12383=VERTEX_POINT('',#42846);
#12384=VERTEX_POINT('',#42857);
#12385=VERTEX_POINT('',#42868);
#12386=VERTEX_POINT('',#42879);
#12387=VERTEX_POINT('',#42890);
#12388=VERTEX_POINT('',#42901);
#12389=VERTEX_POINT('',#42912);
#12390=VERTEX_POINT('',#42923);
#12391=VERTEX_POINT('',#42934);
#12392=VERTEX_POINT('',#42940);
#12393=VERTEX_POINT('',#42949);
#12394=VERTEX_POINT('',#42965);
#12395=VERTEX_POINT('',#42969);
#12396=VERTEX_POINT('',#42973);
#12397=VERTEX_POINT('',#42977);
#12398=VERTEX_POINT('',#42981);
#12399=VERTEX_POINT('',#42985);
#12400=VERTEX_POINT('',#42989);
#12401=VERTEX_POINT('',#42993);
#12402=VERTEX_POINT('',#42997);
#12403=VERTEX_POINT('',#43001);
#12404=VERTEX_POINT('',#43005);
#12405=VERTEX_POINT('',#43009);
#12406=VERTEX_POINT('',#43013);
#12407=VERTEX_POINT('',#43017);
#12408=VERTEX_POINT('',#43021);
#12409=VERTEX_POINT('',#43025);
#12410=VERTEX_POINT('',#43029);
#12411=VERTEX_POINT('',#43033);
#12412=VERTEX_POINT('',#43037);
#12413=VERTEX_POINT('',#43041);
#12414=VERTEX_POINT('',#43045);
#12415=VERTEX_POINT('',#43049);
#12416=VERTEX_POINT('',#43053);
#12417=VERTEX_POINT('',#43057);
#12418=VERTEX_POINT('',#43061);
#12419=VERTEX_POINT('',#43065);
#12420=VERTEX_POINT('',#43069);
#12421=VERTEX_POINT('',#43075);
#12422=VERTEX_POINT('',#43081);
#12423=VERTEX_POINT('',#43087);
#12424=VERTEX_POINT('',#43115);
#12425=VERTEX_POINT('',#43122);
#12426=VERTEX_POINT('',#43124);
#12427=VERTEX_POINT('',#43128);
#12428=VERTEX_POINT('',#43129);
#12429=VERTEX_POINT('',#43131);
#12430=VERTEX_POINT('',#43133);
#12431=VERTEX_POINT('',#43135);
#12432=VERTEX_POINT('',#43137);
#12433=VERTEX_POINT('',#43139);
#12434=VERTEX_POINT('',#43141);
#12435=VERTEX_POINT('',#43143);
#12436=VERTEX_POINT('',#43145);
#12437=VERTEX_POINT('',#43147);
#12438=VERTEX_POINT('',#43149);
#12439=VERTEX_POINT('',#43151);
#12440=VERTEX_POINT('',#43153);
#12441=VERTEX_POINT('',#43155);
#12442=VERTEX_POINT('',#43157);
#12443=VERTEX_POINT('',#43159);
#12444=VERTEX_POINT('',#43161);
#12445=VERTEX_POINT('',#43163);
#12446=VERTEX_POINT('',#43165);
#12447=VERTEX_POINT('',#43167);
#12448=VERTEX_POINT('',#43169);
#12449=VERTEX_POINT('',#43171);
#12450=VERTEX_POINT('',#43173);
#12451=VERTEX_POINT('',#43175);
#12452=VERTEX_POINT('',#43178);
#12453=VERTEX_POINT('',#43180);
#12454=VERTEX_POINT('',#43182);
#12455=VERTEX_POINT('',#43184);
#12456=VERTEX_POINT('',#43186);
#12457=VERTEX_POINT('',#43188);
#12458=VERTEX_POINT('',#43190);
#12459=VERTEX_POINT('',#43192);
#12460=VERTEX_POINT('',#43194);
#12461=VERTEX_POINT('',#43197);
#12462=VERTEX_POINT('',#43201);
#12463=VERTEX_POINT('',#43205);
#12464=VERTEX_POINT('',#43209);
#12465=VERTEX_POINT('',#43211);
#12466=VERTEX_POINT('',#43215);
#12467=VERTEX_POINT('',#43219);
#12468=VERTEX_POINT('',#43223);
#12469=VERTEX_POINT('',#43227);
#12470=VERTEX_POINT('',#43231);
#12471=VERTEX_POINT('',#43235);
#12472=VERTEX_POINT('',#43239);
#12473=VERTEX_POINT('',#43241);
#12474=VERTEX_POINT('',#43250);
#12475=VERTEX_POINT('',#43252);
#12476=VERTEX_POINT('',#43256);
#12477=VERTEX_POINT('',#43262);
#12478=VERTEX_POINT('',#43263);
#12479=VERTEX_POINT('',#43265);
#12480=VERTEX_POINT('',#43267);
#12481=VERTEX_POINT('',#43271);
#12482=VERTEX_POINT('',#43272);
#12483=VERTEX_POINT('',#43277);
#12484=VERTEX_POINT('',#43278);
#12485=VERTEX_POINT('',#43283);
#12486=VERTEX_POINT('',#43284);
#12487=VERTEX_POINT('',#43292);
#12488=VERTEX_POINT('',#43293);
#12489=VERTEX_POINT('',#43298);
#12490=VERTEX_POINT('',#43312);
#12491=VERTEX_POINT('',#43314);
#12492=VERTEX_POINT('',#43318);
#12493=VERTEX_POINT('',#43320);
#12494=VERTEX_POINT('',#43324);
#12495=VERTEX_POINT('',#43326);
#12496=VERTEX_POINT('',#43330);
#12497=VERTEX_POINT('',#43332);
#12498=VERTEX_POINT('',#43334);
#12499=VERTEX_POINT('',#43336);
#12500=VERTEX_POINT('',#43338);
#12501=VERTEX_POINT('',#43340);
#12502=VERTEX_POINT('',#43342);
#12503=VERTEX_POINT('',#43344);
#12504=VERTEX_POINT('',#43346);
#12505=VERTEX_POINT('',#43348);
#12506=VERTEX_POINT('',#43350);
#12507=VERTEX_POINT('',#43352);
#12508=VERTEX_POINT('',#43354);
#12509=VERTEX_POINT('',#43357);
#12510=VERTEX_POINT('',#43359);
#12511=VERTEX_POINT('',#43361);
#12512=VERTEX_POINT('',#43364);
#12513=VERTEX_POINT('',#43368);
#12514=VERTEX_POINT('',#43372);
#12515=VERTEX_POINT('',#43376);
#12516=VERTEX_POINT('',#43380);
#12517=VERTEX_POINT('',#43384);
#12518=VERTEX_POINT('',#43388);
#12519=VERTEX_POINT('',#43392);
#12520=VERTEX_POINT('',#43396);
#12521=VERTEX_POINT('',#43400);
#12522=VERTEX_POINT('',#43404);
#12523=VERTEX_POINT('',#43408);
#12524=VERTEX_POINT('',#43412);
#12525=VERTEX_POINT('',#43416);
#12526=VERTEX_POINT('',#43420);
#12527=VERTEX_POINT('',#43424);
#12528=VERTEX_POINT('',#43430);
#12529=VERTEX_POINT('',#43434);
#12530=VERTEX_POINT('',#43435);
#12531=VERTEX_POINT('',#43437);
#12532=VERTEX_POINT('',#43439);
#12533=VERTEX_POINT('',#43443);
#12534=VERTEX_POINT('',#43444);
#12535=VERTEX_POINT('',#43449);
#12536=VERTEX_POINT('',#43450);
#12537=VERTEX_POINT('',#43455);
#12538=VERTEX_POINT('',#43456);
#12539=VERTEX_POINT('',#43461);
#12540=VERTEX_POINT('',#43462);
#12541=VERTEX_POINT('',#43467);
#12542=VERTEX_POINT('',#43468);
#12543=VERTEX_POINT('',#43473);
#12544=VERTEX_POINT('',#43474);
#12545=VERTEX_POINT('',#43482);
#12546=VERTEX_POINT('',#43484);
#12547=VERTEX_POINT('',#43488);
#12548=VERTEX_POINT('',#43492);
#12549=VERTEX_POINT('',#43494);
#12550=VERTEX_POINT('',#43505);
#12551=VERTEX_POINT('',#43512);
#12552=VERTEX_POINT('',#43515);
#12553=VERTEX_POINT('',#43519);
#12554=VERTEX_POINT('',#43523);
#12555=VERTEX_POINT('',#43527);
#12556=VERTEX_POINT('',#43531);
#12557=VERTEX_POINT('',#43535);
#12558=VERTEX_POINT('',#43539);
#12559=VERTEX_POINT('',#43543);
#12560=VERTEX_POINT('',#43547);
#12561=VERTEX_POINT('',#43551);
#12562=VERTEX_POINT('',#43555);
#12563=VERTEX_POINT('',#43559);
#12564=VERTEX_POINT('',#43563);
#12565=VERTEX_POINT('',#43567);
#12566=VERTEX_POINT('',#43617);
#12567=VERTEX_POINT('',#43623);
#12568=VERTEX_POINT('',#43625);
#12569=VERTEX_POINT('',#43644);
#12570=VERTEX_POINT('',#43666);
#12571=VERTEX_POINT('',#43667);
#12572=VERTEX_POINT('',#43704);
#12573=VERTEX_POINT('',#43710);
#12574=VERTEX_POINT('',#43715);
#12575=VERTEX_POINT('',#43722);
#12576=VERTEX_POINT('',#43727);
#12577=VERTEX_POINT('',#43732);
#12578=VERTEX_POINT('',#43742);
#12579=VERTEX_POINT('',#43744);
#12580=VERTEX_POINT('',#43748);
#12581=VERTEX_POINT('',#43752);
#12582=VERTEX_POINT('',#43755);
#12583=VERTEX_POINT('',#43757);
#12584=VERTEX_POINT('',#43761);
#12585=VERTEX_POINT('',#43765);
#12586=VERTEX_POINT('',#43768);
#12587=VERTEX_POINT('',#43770);
#12588=VERTEX_POINT('',#43774);
#12589=VERTEX_POINT('',#43778);
#12590=VERTEX_POINT('',#43781);
#12591=VERTEX_POINT('',#43783);
#12592=VERTEX_POINT('',#43787);
#12593=VERTEX_POINT('',#43791);
#12594=VERTEX_POINT('',#43794);
#12595=VERTEX_POINT('',#43796);
#12596=VERTEX_POINT('',#43800);
#12597=VERTEX_POINT('',#43804);
#12598=VERTEX_POINT('',#43807);
#12599=VERTEX_POINT('',#43809);
#12600=VERTEX_POINT('',#43813);
#12601=VERTEX_POINT('',#43817);
#12602=VERTEX_POINT('',#43820);
#12603=VERTEX_POINT('',#43822);
#12604=VERTEX_POINT('',#43826);
#12605=VERTEX_POINT('',#43830);
#12606=VERTEX_POINT('',#43833);
#12607=VERTEX_POINT('',#43835);
#12608=VERTEX_POINT('',#43839);
#12609=VERTEX_POINT('',#43843);
#12610=VERTEX_POINT('',#43846);
#12611=VERTEX_POINT('',#43848);
#12612=VERTEX_POINT('',#43852);
#12613=VERTEX_POINT('',#43856);
#12614=VERTEX_POINT('',#43859);
#12615=VERTEX_POINT('',#43860);
#12616=VERTEX_POINT('',#43862);
#12617=VERTEX_POINT('',#43864);
#12618=VERTEX_POINT('',#43866);
#12619=VERTEX_POINT('',#43868);
#12620=VERTEX_POINT('',#43872);
#12621=VERTEX_POINT('',#43874);
#12622=VERTEX_POINT('',#43876);
#12623=VERTEX_POINT('',#43878);
#12624=VERTEX_POINT('',#43882);
#12625=VERTEX_POINT('',#43886);
#12626=VERTEX_POINT('',#43888);
#12627=VERTEX_POINT('',#43890);
#12628=VERTEX_POINT('',#43894);
#12629=VERTEX_POINT('',#43896);
#12630=VERTEX_POINT('',#43900);
#12631=VERTEX_POINT('',#43904);
#12632=VERTEX_POINT('',#43907);
#12633=VERTEX_POINT('',#43909);
#12634=VERTEX_POINT('',#43913);
#12635=VERTEX_POINT('',#43917);
#12636=VERTEX_POINT('',#43920);
#12637=VERTEX_POINT('',#43921);
#12638=VERTEX_POINT('',#43923);
#12639=VERTEX_POINT('',#43925);
#12640=VERTEX_POINT('',#43927);
#12641=VERTEX_POINT('',#43929);
#12642=VERTEX_POINT('',#43933);
#12643=VERTEX_POINT('',#43935);
#12644=VERTEX_POINT('',#43937);
#12645=VERTEX_POINT('',#43939);
#12646=VERTEX_POINT('',#43943);
#12647=VERTEX_POINT('',#43947);
#12648=VERTEX_POINT('',#43949);
#12649=VERTEX_POINT('',#43951);
#12650=VERTEX_POINT('',#43955);
#12651=VERTEX_POINT('',#43957);
#12652=VERTEX_POINT('',#43961);
#12653=VERTEX_POINT('',#43963);
#12654=VERTEX_POINT('',#43967);
#12655=VERTEX_POINT('',#43969);
#12656=VERTEX_POINT('',#43973);
#12657=VERTEX_POINT('',#43977);
#12658=VERTEX_POINT('',#43980);
#12659=VERTEX_POINT('',#43982);
#12660=VERTEX_POINT('',#43986);
#12661=VERTEX_POINT('',#43990);
#12662=VERTEX_POINT('',#43993);
#12663=VERTEX_POINT('',#43999);
#12664=VERTEX_POINT('',#44001);
#12665=VERTEX_POINT('',#44003);
#12666=VERTEX_POINT('',#44005);
#12667=VERTEX_POINT('',#44007);
#12668=VERTEX_POINT('',#44009);
#12669=VERTEX_POINT('',#44011);
#12670=VERTEX_POINT('',#44013);
#12671=VERTEX_POINT('',#44015);
#12672=VERTEX_POINT('',#44017);
#12673=VERTEX_POINT('',#44019);
#12674=VERTEX_POINT('',#44021);
#12675=VERTEX_POINT('',#44023);
#12676=VERTEX_POINT('',#44025);
#12677=VERTEX_POINT('',#44027);
#12678=VERTEX_POINT('',#44029);
#12679=VERTEX_POINT('',#44031);
#12680=VERTEX_POINT('',#44033);
#12681=VERTEX_POINT('',#44035);
#12682=VERTEX_POINT('',#44037);
#12683=VERTEX_POINT('',#44039);
#12684=VERTEX_POINT('',#44041);
#12685=VERTEX_POINT('',#44043);
#12686=VERTEX_POINT('',#44045);
#12687=VERTEX_POINT('',#44047);
#12688=VERTEX_POINT('',#44049);
#12689=VERTEX_POINT('',#44051);
#12690=VERTEX_POINT('',#44053);
#12691=VERTEX_POINT('',#44055);
#12692=VERTEX_POINT('',#44057);
#12693=VERTEX_POINT('',#44059);
#12694=VERTEX_POINT('',#44061);
#12695=VERTEX_POINT('',#44063);
#12696=VERTEX_POINT('',#44065);
#12697=VERTEX_POINT('',#44067);
#12698=VERTEX_POINT('',#44069);
#12699=VERTEX_POINT('',#44071);
#12700=VERTEX_POINT('',#44073);
#12701=VERTEX_POINT('',#44075);
#12702=VERTEX_POINT('',#44077);
#12703=VERTEX_POINT('',#44079);
#12704=VERTEX_POINT('',#44096);
#12705=VERTEX_POINT('',#44100);
#12706=VERTEX_POINT('',#44104);
#12707=VERTEX_POINT('',#44108);
#12708=VERTEX_POINT('',#44122);
#12709=VERTEX_POINT('',#44126);
#12710=VERTEX_POINT('',#44130);
#12711=VERTEX_POINT('',#44134);
#12712=VERTEX_POINT('',#44138);
#12713=VERTEX_POINT('',#44142);
#12714=VERTEX_POINT('',#44146);
#12715=VERTEX_POINT('',#44150);
#12716=VERTEX_POINT('',#44154);
#12717=VERTEX_POINT('',#44158);
#12718=VERTEX_POINT('',#44162);
#12719=VERTEX_POINT('',#44166);
#12720=VERTEX_POINT('',#44170);
#12721=VERTEX_POINT('',#44174);
#12722=VERTEX_POINT('',#44178);
#12723=VERTEX_POINT('',#44182);
#12724=VERTEX_POINT('',#44186);
#12725=VERTEX_POINT('',#44190);
#12726=VERTEX_POINT('',#44194);
#12727=VERTEX_POINT('',#44198);
#12728=VERTEX_POINT('',#44202);
#12729=VERTEX_POINT('',#44206);
#12730=VERTEX_POINT('',#44210);
#12731=VERTEX_POINT('',#44214);
#12732=VERTEX_POINT('',#44222);
#12733=VERTEX_POINT('',#44226);
#12734=VERTEX_POINT('',#44230);
#12735=VERTEX_POINT('',#44234);
#12736=VERTEX_POINT('',#44238);
#12737=VERTEX_POINT('',#44242);
#12738=VERTEX_POINT('',#44246);
#12739=VERTEX_POINT('',#44250);
#12740=VERTEX_POINT('',#44254);
#12741=VERTEX_POINT('',#44258);
#12742=VERTEX_POINT('',#44262);
#12743=VERTEX_POINT('',#44266);
#12744=VERTEX_POINT('',#44270);
#12745=VERTEX_POINT('',#44274);
#12746=VERTEX_POINT('',#44278);
#12747=VERTEX_POINT('',#44282);
#12748=VERTEX_POINT('',#44286);
#12749=VERTEX_POINT('',#44290);
#12750=VERTEX_POINT('',#44294);
#12751=VERTEX_POINT('',#44298);
#12752=VERTEX_POINT('',#44302);
#12753=VERTEX_POINT('',#44306);
#12754=VERTEX_POINT('',#44310);
#12755=VERTEX_POINT('',#44314);
#12756=VERTEX_POINT('',#44318);
#12757=VERTEX_POINT('',#44322);
#12758=VERTEX_POINT('',#44326);
#12759=VERTEX_POINT('',#44330);
#12760=VERTEX_POINT('',#44334);
#12761=VERTEX_POINT('',#44338);
#12762=VERTEX_POINT('',#44347);
#12763=VERTEX_POINT('',#44349);
#12764=VERTEX_POINT('',#44351);
#12765=VERTEX_POINT('',#44353);
#12766=VERTEX_POINT('',#44355);
#12767=VERTEX_POINT('',#44357);
#12768=VERTEX_POINT('',#44359);
#12769=VERTEX_POINT('',#44361);
#12770=VERTEX_POINT('',#44363);
#12771=VERTEX_POINT('',#44365);
#12772=VERTEX_POINT('',#44367);
#12773=VERTEX_POINT('',#44369);
#12774=VERTEX_POINT('',#44371);
#12775=VERTEX_POINT('',#44373);
#12776=VERTEX_POINT('',#44375);
#12777=VERTEX_POINT('',#44377);
#12778=VERTEX_POINT('',#44379);
#12779=VERTEX_POINT('',#44381);
#12780=VERTEX_POINT('',#44383);
#12781=VERTEX_POINT('',#44385);
#12782=VERTEX_POINT('',#44387);
#12783=VERTEX_POINT('',#44389);
#12784=VERTEX_POINT('',#44391);
#12785=VERTEX_POINT('',#44393);
#12786=VERTEX_POINT('',#44395);
#12787=VERTEX_POINT('',#44397);
#12788=VERTEX_POINT('',#44399);
#12789=VERTEX_POINT('',#44401);
#12790=VERTEX_POINT('',#44403);
#12791=VERTEX_POINT('',#44405);
#12792=VERTEX_POINT('',#44407);
#12793=VERTEX_POINT('',#44409);
#12794=VERTEX_POINT('',#44411);
#12795=VERTEX_POINT('',#44413);
#12796=VERTEX_POINT('',#44415);
#12797=VERTEX_POINT('',#44417);
#12798=VERTEX_POINT('',#44419);
#12799=VERTEX_POINT('',#44421);
#12800=VERTEX_POINT('',#44423);
#12801=VERTEX_POINT('',#44425);
#12802=VERTEX_POINT('',#44427);
#12803=VERTEX_POINT('',#44429);
#12804=VERTEX_POINT('',#44448);
#12805=VERTEX_POINT('',#44454);
#12806=VERTEX_POINT('',#44460);
#12807=VERTEX_POINT('',#44466);
#12808=VERTEX_POINT('',#44472);
#12809=VERTEX_POINT('',#44478);
#12810=VERTEX_POINT('',#44484);
#12811=VERTEX_POINT('',#44490);
#12812=VERTEX_POINT('',#44496);
#12813=VERTEX_POINT('',#44502);
#12814=VERTEX_POINT('',#44552);
#12815=VERTEX_POINT('',#44558);
#12816=VERTEX_POINT('',#44568);
#12817=VERTEX_POINT('',#44569);
#12818=VERTEX_POINT('',#44576);
#12819=VERTEX_POINT('',#44578);
#12820=VERTEX_POINT('',#44583);
#12821=VERTEX_POINT('',#44585);
#12822=VERTEX_POINT('',#44588);
#12823=VERTEX_POINT('',#44590);
#12824=VERTEX_POINT('',#44596);
#12825=VERTEX_POINT('',#44600);
#12826=VERTEX_POINT('',#44602);
#12827=VERTEX_POINT('',#44604);
#12828=VERTEX_POINT('',#44606);
#12829=VERTEX_POINT('',#44608);
#12830=VERTEX_POINT('',#44612);
#12831=VERTEX_POINT('',#44616);
#12832=VERTEX_POINT('',#44620);
#12833=VERTEX_POINT('',#44621);
#12834=VERTEX_POINT('',#44623);
#12835=VERTEX_POINT('',#44630);
#12836=VERTEX_POINT('',#44631);
#12837=VERTEX_POINT('',#44634);
#12838=VERTEX_POINT('',#44638);
#12839=VERTEX_POINT('',#44639);
#12840=VERTEX_POINT('',#44641);
#12841=VERTEX_POINT('',#44646);
#12842=VERTEX_POINT('',#44653);
#12843=VERTEX_POINT('',#44654);
#12844=VERTEX_POINT('',#44657);
#12845=VERTEX_POINT('',#44661);
#12846=VERTEX_POINT('',#44662);
#12847=VERTEX_POINT('',#44665);
#12848=VERTEX_POINT('',#44670);
#12849=VERTEX_POINT('',#44672);
#12850=VERTEX_POINT('',#44676);
#12851=VERTEX_POINT('',#44678);
#12852=VERTEX_POINT('',#44681);
#12853=VERTEX_POINT('',#44683);
#12854=VERTEX_POINT('',#44687);
#12855=VERTEX_POINT('',#44689);
#12856=VERTEX_POINT('',#44694);
#12857=VERTEX_POINT('',#44701);
#12858=VERTEX_POINT('',#44708);
#12859=VERTEX_POINT('',#44711);
#12860=VERTEX_POINT('',#44714);
#12861=VERTEX_POINT('',#44717);
#12862=VERTEX_POINT('',#44724);
#12863=VERTEX_POINT('',#44726);
#12864=VERTEX_POINT('',#44737);
#12865=VERTEX_POINT('',#44767);
#12866=VERTEX_POINT('',#44768);
#12867=VERTEX_POINT('',#44805);
#12868=VERTEX_POINT('',#44811);
#12869=VERTEX_POINT('',#44820);
#12870=VERTEX_POINT('',#44821);
#12871=VERTEX_POINT('',#44826);
#12872=VERTEX_POINT('',#44849);
#12873=VERTEX_POINT('',#44851);
#12874=VERTEX_POINT('',#44853);
#12875=VERTEX_POINT('',#44910);
#12876=VERTEX_POINT('',#44916);
#12877=VERTEX_POINT('',#44917);
#12878=VERTEX_POINT('',#44926);
#12879=VERTEX_POINT('',#44937);
#12880=VERTEX_POINT('',#44953);
#12881=VERTEX_POINT('',#44955);
#12882=VERTEX_POINT('',#45011);
#12883=VERTEX_POINT('',#46415);
#12884=VERTEX_POINT('',#46416);
#12885=VERTEX_POINT('',#46418);
#12886=VERTEX_POINT('',#46429);
#12887=VERTEX_POINT('',#46439);
#12888=VERTEX_POINT('',#46440);
#12889=VERTEX_POINT('',#46487);
#12890=VERTEX_POINT('',#46488);
#12891=VERTEX_POINT('',#46535);
#12892=VERTEX_POINT('',#46536);
#12893=VERTEX_POINT('',#46583);
#12894=VERTEX_POINT('',#46584);
#12895=VERTEX_POINT('',#46637);
#12896=VERTEX_POINT('',#46638);
#12897=VERTEX_POINT('',#46685);
#12898=VERTEX_POINT('',#46686);
#12899=VERTEX_POINT('',#46733);
#12900=VERTEX_POINT('',#46734);
#12901=VERTEX_POINT('',#46787);
#12902=VERTEX_POINT('',#46788);
#12903=VERTEX_POINT('',#46835);
#12904=VERTEX_POINT('',#46836);
#12905=VERTEX_POINT('',#46883);
#12906=VERTEX_POINT('',#46884);
#12907=VERTEX_POINT('',#46886);
#12908=VERTEX_POINT('',#46892);
#12909=VERTEX_POINT('',#46899);
#12910=VERTEX_POINT('',#46900);
#12911=VERTEX_POINT('',#46923);
#12912=VERTEX_POINT('',#46924);
#12913=VERTEX_POINT('',#46947);
#12914=VERTEX_POINT('',#46948);
#12915=VERTEX_POINT('',#46972);
#12916=VERTEX_POINT('',#46973);
#12917=VERTEX_POINT('',#46997);
#12918=VERTEX_POINT('',#46998);
#12919=VERTEX_POINT('',#47021);
#12920=VERTEX_POINT('',#47022);
#12921=VERTEX_POINT('',#47046);
#12922=VERTEX_POINT('',#47047);
#12923=VERTEX_POINT('',#47071);
#12924=VERTEX_POINT('',#47072);
#12925=VERTEX_POINT('',#47095);
#12926=VERTEX_POINT('',#47096);
#12927=VERTEX_POINT('',#47119);
#12928=VERTEX_POINT('',#47217);
#12929=VERTEX_POINT('',#47219);
#12930=VERTEX_POINT('',#47602);
#12931=VERTEX_POINT('',#47710);
#12932=VERTEX_POINT('',#47713);
#12933=VERTEX_POINT('',#48103);
#12934=VERTEX_POINT('',#48104);
#12935=VERTEX_POINT('',#48106);
#12936=VERTEX_POINT('',#48108);
#12937=VERTEX_POINT('',#48112);
#12938=VERTEX_POINT('',#48116);
#12939=VERTEX_POINT('',#48122);
#12940=VERTEX_POINT('',#48123);
#12941=VERTEX_POINT('',#48125);
#12942=VERTEX_POINT('',#48127);
#12943=VERTEX_POINT('',#48131);
#12944=VERTEX_POINT('',#48135);
#12945=VERTEX_POINT('',#48141);
#12946=VERTEX_POINT('',#48142);
#12947=VERTEX_POINT('',#48144);
#12948=VERTEX_POINT('',#48146);
#12949=VERTEX_POINT('',#48150);
#12950=VERTEX_POINT('',#48154);
#12951=VERTEX_POINT('',#48160);
#12952=VERTEX_POINT('',#48161);
#12953=VERTEX_POINT('',#48163);
#12954=VERTEX_POINT('',#48165);
#12955=VERTEX_POINT('',#48169);
#12956=VERTEX_POINT('',#48173);
#12957=VERTEX_POINT('',#48179);
#12958=VERTEX_POINT('',#48180);
#12959=VERTEX_POINT('',#48182);
#12960=VERTEX_POINT('',#48184);
#12961=VERTEX_POINT('',#48188);
#12962=VERTEX_POINT('',#48192);
#12963=VERTEX_POINT('',#48198);
#12964=VERTEX_POINT('',#48199);
#12965=VERTEX_POINT('',#48201);
#12966=VERTEX_POINT('',#48203);
#12967=VERTEX_POINT('',#48207);
#12968=VERTEX_POINT('',#48211);
#12969=VERTEX_POINT('',#48217);
#12970=VERTEX_POINT('',#48218);
#12971=VERTEX_POINT('',#48220);
#12972=VERTEX_POINT('',#48222);
#12973=VERTEX_POINT('',#48226);
#12974=VERTEX_POINT('',#48230);
#12975=VERTEX_POINT('',#48236);
#12976=VERTEX_POINT('',#48237);
#12977=VERTEX_POINT('',#48239);
#12978=VERTEX_POINT('',#48241);
#12979=VERTEX_POINT('',#48245);
#12980=VERTEX_POINT('',#48249);
#12981=VERTEX_POINT('',#48255);
#12982=VERTEX_POINT('',#48256);
#12983=VERTEX_POINT('',#48258);
#12984=VERTEX_POINT('',#48260);
#12985=VERTEX_POINT('',#48264);
#12986=VERTEX_POINT('',#48268);
#12987=VERTEX_POINT('',#48274);
#12988=VERTEX_POINT('',#48275);
#12989=VERTEX_POINT('',#48277);
#12990=VERTEX_POINT('',#48279);
#12991=VERTEX_POINT('',#48283);
#12992=VERTEX_POINT('',#48287);
#12993=VERTEX_POINT('',#48293);
#12994=VERTEX_POINT('',#48294);
#12995=VERTEX_POINT('',#48296);
#12996=VERTEX_POINT('',#48298);
#12997=VERTEX_POINT('',#48302);
#12998=VERTEX_POINT('',#48306);
#12999=VERTEX_POINT('',#48312);
#13000=VERTEX_POINT('',#48313);
#13001=VERTEX_POINT('',#48315);
#13002=VERTEX_POINT('',#48317);
#13003=VERTEX_POINT('',#48321);
#13004=VERTEX_POINT('',#48325);
#13005=VERTEX_POINT('',#48331);
#13006=VERTEX_POINT('',#48332);
#13007=VERTEX_POINT('',#48334);
#13008=VERTEX_POINT('',#48336);
#13009=VERTEX_POINT('',#48340);
#13010=VERTEX_POINT('',#48344);
#13011=VERTEX_POINT('',#48350);
#13012=VERTEX_POINT('',#48351);
#13013=VERTEX_POINT('',#48353);
#13014=VERTEX_POINT('',#48355);
#13015=VERTEX_POINT('',#48359);
#13016=VERTEX_POINT('',#48363);
#13017=VERTEX_POINT('',#48369);
#13018=VERTEX_POINT('',#48370);
#13019=VERTEX_POINT('',#48372);
#13020=VERTEX_POINT('',#48374);
#13021=VERTEX_POINT('',#48378);
#13022=VERTEX_POINT('',#48382);
#13023=VERTEX_POINT('',#48388);
#13024=VERTEX_POINT('',#48389);
#13025=VERTEX_POINT('',#48391);
#13026=VERTEX_POINT('',#48393);
#13027=VERTEX_POINT('',#48397);
#13028=VERTEX_POINT('',#48401);
#13029=VERTEX_POINT('',#48407);
#13030=VERTEX_POINT('',#48408);
#13031=VERTEX_POINT('',#48410);
#13032=VERTEX_POINT('',#48412);
#13033=VERTEX_POINT('',#48416);
#13034=VERTEX_POINT('',#48420);
#13035=VERTEX_POINT('',#48426);
#13036=VERTEX_POINT('',#48427);
#13037=VERTEX_POINT('',#48429);
#13038=VERTEX_POINT('',#48431);
#13039=VERTEX_POINT('',#48435);
#13040=VERTEX_POINT('',#48437);
#13041=VERTEX_POINT('',#48441);
#13042=VERTEX_POINT('',#48445);
#13043=VERTEX_POINT('',#48449);
#13044=VERTEX_POINT('',#48450);
#13045=VERTEX_POINT('',#48452);
#13046=VERTEX_POINT('',#48454);
#13047=VERTEX_POINT('',#48458);
#13048=VERTEX_POINT('',#48462);
#13049=VERTEX_POINT('',#48468);
#13050=VERTEX_POINT('',#48469);
#13051=VERTEX_POINT('',#48471);
#13052=VERTEX_POINT('',#48473);
#13053=VERTEX_POINT('',#48477);
#13054=VERTEX_POINT('',#48481);
#13055=VERTEX_POINT('',#48487);
#13056=VERTEX_POINT('',#48488);
#13057=VERTEX_POINT('',#48490);
#13058=VERTEX_POINT('',#48492);
#13059=VERTEX_POINT('',#48496);
#13060=VERTEX_POINT('',#48500);
#13061=VERTEX_POINT('',#48506);
#13062=VERTEX_POINT('',#48507);
#13063=VERTEX_POINT('',#48509);
#13064=VERTEX_POINT('',#48511);
#13065=VERTEX_POINT('',#48515);
#13066=VERTEX_POINT('',#48519);
#13067=VERTEX_POINT('',#48525);
#13068=VERTEX_POINT('',#48526);
#13069=VERTEX_POINT('',#48528);
#13070=VERTEX_POINT('',#48530);
#13071=VERTEX_POINT('',#48534);
#13072=VERTEX_POINT('',#48538);
#13073=VERTEX_POINT('',#48544);
#13074=VERTEX_POINT('',#48545);
#13075=VERTEX_POINT('',#48547);
#13076=VERTEX_POINT('',#48549);
#13077=VERTEX_POINT('',#48553);
#13078=VERTEX_POINT('',#48557);
#13079=VERTEX_POINT('',#48563);
#13080=VERTEX_POINT('',#48564);
#13081=VERTEX_POINT('',#48566);
#13082=VERTEX_POINT('',#48568);
#13083=VERTEX_POINT('',#48572);
#13084=VERTEX_POINT('',#48576);
#13085=VERTEX_POINT('',#48582);
#13086=VERTEX_POINT('',#48583);
#13087=VERTEX_POINT('',#48585);
#13088=VERTEX_POINT('',#48587);
#13089=VERTEX_POINT('',#48591);
#13090=VERTEX_POINT('',#48595);
#13091=VERTEX_POINT('',#48601);
#13092=VERTEX_POINT('',#48602);
#13093=VERTEX_POINT('',#48604);
#13094=VERTEX_POINT('',#48606);
#13095=VERTEX_POINT('',#48610);
#13096=VERTEX_POINT('',#48614);
#13097=VERTEX_POINT('',#48620);
#13098=VERTEX_POINT('',#48621);
#13099=VERTEX_POINT('',#48623);
#13100=VERTEX_POINT('',#48625);
#13101=VERTEX_POINT('',#48629);
#13102=VERTEX_POINT('',#48633);
#13103=VERTEX_POINT('',#48639);
#13104=VERTEX_POINT('',#48640);
#13105=VERTEX_POINT('',#48642);
#13106=VERTEX_POINT('',#48644);
#13107=VERTEX_POINT('',#48648);
#13108=VERTEX_POINT('',#48652);
#13109=VERTEX_POINT('',#48658);
#13110=VERTEX_POINT('',#48659);
#13111=VERTEX_POINT('',#48661);
#13112=VERTEX_POINT('',#48663);
#13113=VERTEX_POINT('',#48667);
#13114=VERTEX_POINT('',#48671);
#13115=VERTEX_POINT('',#48677);
#13116=VERTEX_POINT('',#48678);
#13117=VERTEX_POINT('',#48680);
#13118=VERTEX_POINT('',#48682);
#13119=VERTEX_POINT('',#48686);
#13120=VERTEX_POINT('',#48690);
#13121=VERTEX_POINT('',#48696);
#13122=VERTEX_POINT('',#48697);
#13123=VERTEX_POINT('',#48699);
#13124=VERTEX_POINT('',#48701);
#13125=VERTEX_POINT('',#48705);
#13126=VERTEX_POINT('',#48709);
#13127=VERTEX_POINT('',#48715);
#13128=VERTEX_POINT('',#48716);
#13129=VERTEX_POINT('',#48718);
#13130=VERTEX_POINT('',#48720);
#13131=VERTEX_POINT('',#48724);
#13132=VERTEX_POINT('',#48728);
#13133=VERTEX_POINT('',#48734);
#13134=VERTEX_POINT('',#48735);
#13135=VERTEX_POINT('',#48737);
#13136=VERTEX_POINT('',#48739);
#13137=VERTEX_POINT('',#48743);
#13138=VERTEX_POINT('',#48747);
#13139=VERTEX_POINT('',#48753);
#13140=VERTEX_POINT('',#48754);
#13141=VERTEX_POINT('',#48756);
#13142=VERTEX_POINT('',#48758);
#13143=VERTEX_POINT('',#48762);
#13144=VERTEX_POINT('',#48766);
#13145=VERTEX_POINT('',#48772);
#13146=VERTEX_POINT('',#48773);
#13147=VERTEX_POINT('',#48775);
#13148=VERTEX_POINT('',#48777);
#13149=VERTEX_POINT('',#48781);
#13150=VERTEX_POINT('',#48785);
#13151=VERTEX_POINT('',#48791);
#13152=VERTEX_POINT('',#48792);
#13153=VERTEX_POINT('',#48796);
#13154=VERTEX_POINT('',#48797);
#13155=VERTEX_POINT('',#48799);
#13156=VERTEX_POINT('',#48801);
#13157=VERTEX_POINT('',#48805);
#13158=VERTEX_POINT('',#48807);
#13159=VERTEX_POINT('',#48811);
#13160=VERTEX_POINT('',#48813);
#13161=VERTEX_POINT('',#48817);
#13162=VERTEX_POINT('',#48819);
#13163=VERTEX_POINT('',#48823);
#13164=VERTEX_POINT('',#48825);
#13165=VERTEX_POINT('',#48833);
#13166=VERTEX_POINT('',#48834);
#13167=VERTEX_POINT('',#48836);
#13168=VERTEX_POINT('',#48841);
#13169=VERTEX_POINT('',#48845);
#13170=VERTEX_POINT('',#48848);
#13171=VERTEX_POINT('',#48855);
#13172=VERTEX_POINT('',#48859);
#13173=VERTEX_POINT('',#48864);
#13174=VERTEX_POINT('',#48869);
#13175=VERTEX_POINT('',#48875);
#13176=VERTEX_POINT('',#48877);
#13177=VERTEX_POINT('',#48881);
#13178=VERTEX_POINT('',#48884);
#13179=VERTEX_POINT('',#48890);
#13180=VERTEX_POINT('',#48891);
#13181=VERTEX_POINT('',#48895);
#13182=VERTEX_POINT('',#48898);
#13183=VERTEX_POINT('',#48902);
#13184=VERTEX_POINT('',#48906);
#13185=VERTEX_POINT('',#49481);
#13186=VERTEX_POINT('',#49483);
#13187=VERTEX_POINT('',#49546);
#13188=VERTEX_POINT('',#49548);
#13189=VERTEX_POINT('',#49550);
#13190=VERTEX_POINT('',#49554);
#13191=VERTEX_POINT('',#49558);
#13192=VERTEX_POINT('',#49561);
#13193=VERTEX_POINT('',#49565);
#13194=VERTEX_POINT('',#49571);
#13195=VERTEX_POINT('',#49572);
#13196=VERTEX_POINT('',#49574);
#13197=VERTEX_POINT('',#49585);
#13198=VERTEX_POINT('',#49595);
#13199=VERTEX_POINT('',#49596);
#13200=VERTEX_POINT('',#49643);
#13201=VERTEX_POINT('',#49644);
#13202=VERTEX_POINT('',#49691);
#13203=VERTEX_POINT('',#49692);
#13204=VERTEX_POINT('',#49742);
#13205=VERTEX_POINT('',#49743);
#13206=VERTEX_POINT('',#49793);
#13207=VERTEX_POINT('',#49794);
#13208=VERTEX_POINT('',#49841);
#13209=VERTEX_POINT('',#49842);
#13210=VERTEX_POINT('',#49889);
#13211=VERTEX_POINT('',#49890);
#13212=VERTEX_POINT('',#49943);
#13213=VERTEX_POINT('',#49944);
#13214=VERTEX_POINT('',#49991);
#13215=VERTEX_POINT('',#49992);
#13216=VERTEX_POINT('',#50039);
#13217=VERTEX_POINT('',#50040);
#13218=VERTEX_POINT('',#50093);
#13219=VERTEX_POINT('',#50094);
#13220=VERTEX_POINT('',#50141);
#13221=VERTEX_POINT('',#50142);
#13222=VERTEX_POINT('',#50189);
#13223=VERTEX_POINT('',#50190);
#13224=VERTEX_POINT('',#50237);
#13225=VERTEX_POINT('',#50238);
#13226=VERTEX_POINT('',#50291);
#13227=VERTEX_POINT('',#50292);
#13228=VERTEX_POINT('',#50339);
#13229=VERTEX_POINT('',#50340);
#13230=VERTEX_POINT('',#50387);
#13231=VERTEX_POINT('',#50388);
#13232=VERTEX_POINT('',#50441);
#13233=VERTEX_POINT('',#50442);
#13234=VERTEX_POINT('',#50489);
#13235=VERTEX_POINT('',#50490);
#13236=VERTEX_POINT('',#50537);
#13237=VERTEX_POINT('',#50538);
#13238=VERTEX_POINT('',#50591);
#13239=VERTEX_POINT('',#50592);
#13240=VERTEX_POINT('',#50639);
#13241=VERTEX_POINT('',#50640);
#13242=VERTEX_POINT('',#50687);
#13243=VERTEX_POINT('',#50688);
#13244=VERTEX_POINT('',#50735);
#13245=VERTEX_POINT('',#50736);
#13246=VERTEX_POINT('',#50789);
#13247=VERTEX_POINT('',#50790);
#13248=VERTEX_POINT('',#50837);
#13249=VERTEX_POINT('',#50838);
#13250=VERTEX_POINT('',#50885);
#13251=VERTEX_POINT('',#50886);
#13252=VERTEX_POINT('',#50939);
#13253=VERTEX_POINT('',#50940);
#13254=VERTEX_POINT('',#50987);
#13255=VERTEX_POINT('',#50988);
#13256=VERTEX_POINT('',#51035);
#13257=VERTEX_POINT('',#51036);
#13258=VERTEX_POINT('',#51089);
#13259=VERTEX_POINT('',#51090);
#13260=VERTEX_POINT('',#51137);
#13261=VERTEX_POINT('',#51138);
#13262=VERTEX_POINT('',#51185);
#13263=VERTEX_POINT('',#51186);
#13264=VERTEX_POINT('',#51233);
#13265=VERTEX_POINT('',#51234);
#13266=VERTEX_POINT('',#51287);
#13267=VERTEX_POINT('',#51288);
#13268=VERTEX_POINT('',#51335);
#13269=VERTEX_POINT('',#51336);
#13270=VERTEX_POINT('',#51383);
#13271=VERTEX_POINT('',#51384);
#13272=VERTEX_POINT('',#51437);
#13273=VERTEX_POINT('',#51438);
#13274=VERTEX_POINT('',#51485);
#13275=VERTEX_POINT('',#51486);
#13276=VERTEX_POINT('',#51533);
#13277=VERTEX_POINT('',#51534);
#13278=VERTEX_POINT('',#51587);
#13279=VERTEX_POINT('',#51588);
#13280=VERTEX_POINT('',#51635);
#13281=VERTEX_POINT('',#51636);
#13282=VERTEX_POINT('',#51638);
#13283=VERTEX_POINT('',#51645);
#13284=VERTEX_POINT('',#51653);
#13285=VERTEX_POINT('',#51654);
#13286=VERTEX_POINT('',#51677);
#13287=VERTEX_POINT('',#51678);
#13288=VERTEX_POINT('',#51702);
#13289=VERTEX_POINT('',#51703);
#13290=VERTEX_POINT('',#51727);
#13291=VERTEX_POINT('',#51728);
#13292=VERTEX_POINT('',#51751);
#13293=VERTEX_POINT('',#51752);
#13294=VERTEX_POINT('',#51776);
#13295=VERTEX_POINT('',#51777);
#13296=VERTEX_POINT('',#51801);
#13297=VERTEX_POINT('',#51802);
#13298=VERTEX_POINT('',#51825);
#13299=VERTEX_POINT('',#51826);
#13300=VERTEX_POINT('',#51850);
#13301=VERTEX_POINT('',#51851);
#13302=VERTEX_POINT('',#51875);
#13303=VERTEX_POINT('',#51876);
#13304=VERTEX_POINT('',#51899);
#13305=VERTEX_POINT('',#51900);
#13306=VERTEX_POINT('',#51923);
#13307=VERTEX_POINT('',#51924);
#13308=VERTEX_POINT('',#51948);
#13309=VERTEX_POINT('',#51949);
#13310=VERTEX_POINT('',#51973);
#13311=VERTEX_POINT('',#51974);
#13312=VERTEX_POINT('',#51997);
#13313=VERTEX_POINT('',#51998);
#13314=VERTEX_POINT('',#52022);
#13315=VERTEX_POINT('',#52023);
#13316=VERTEX_POINT('',#52047);
#13317=VERTEX_POINT('',#52048);
#13318=VERTEX_POINT('',#52071);
#13319=VERTEX_POINT('',#52072);
#13320=VERTEX_POINT('',#52096);
#13321=VERTEX_POINT('',#52097);
#13322=VERTEX_POINT('',#52121);
#13323=VERTEX_POINT('',#52122);
#13324=VERTEX_POINT('',#52145);
#13325=VERTEX_POINT('',#52146);
#13326=VERTEX_POINT('',#52169);
#13327=VERTEX_POINT('',#52170);
#13328=VERTEX_POINT('',#52194);
#13329=VERTEX_POINT('',#52195);
#13330=VERTEX_POINT('',#52219);
#13331=VERTEX_POINT('',#52220);
#13332=VERTEX_POINT('',#52243);
#13333=VERTEX_POINT('',#52244);
#13334=VERTEX_POINT('',#52268);
#13335=VERTEX_POINT('',#52269);
#13336=VERTEX_POINT('',#52293);
#13337=VERTEX_POINT('',#52294);
#13338=VERTEX_POINT('',#52317);
#13339=VERTEX_POINT('',#52318);
#13340=VERTEX_POINT('',#52342);
#13341=VERTEX_POINT('',#52343);
#13342=VERTEX_POINT('',#52367);
#13343=VERTEX_POINT('',#52368);
#13344=VERTEX_POINT('',#52391);
#13345=VERTEX_POINT('',#52392);
#13346=VERTEX_POINT('',#52415);
#13347=VERTEX_POINT('',#52416);
#13348=VERTEX_POINT('',#52440);
#13349=VERTEX_POINT('',#52441);
#13350=VERTEX_POINT('',#52465);
#13351=VERTEX_POINT('',#52466);
#13352=VERTEX_POINT('',#52489);
#13353=VERTEX_POINT('',#52490);
#13354=VERTEX_POINT('',#52514);
#13355=VERTEX_POINT('',#52515);
#13356=VERTEX_POINT('',#52539);
#13357=VERTEX_POINT('',#52540);
#13358=VERTEX_POINT('',#52563);
#13359=VERTEX_POINT('',#52564);
#13360=VERTEX_POINT('',#52588);
#13361=VERTEX_POINT('',#52589);
#13362=VERTEX_POINT('',#52612);
#13363=VERTEX_POINT('',#52613);
#13364=VERTEX_POINT('',#52637);
#13365=VERTEX_POINT('',#52638);
#13366=VERTEX_POINT('',#52661);
#13367=VERTEX_POINT('',#52747);
#13368=VERTEX_POINT('',#53933);
#13369=VERTEX_POINT('',#54029);
#13370=VERTEX_POINT('',#54032);
#13371=VERTEX_POINT('',#55225);
#13372=VERTEX_POINT('',#55227);
#13373=VERTEX_POINT('',#55233);
#13374=VERTEX_POINT('',#55236);
#13375=VERTEX_POINT('',#55237);
#13376=VERTEX_POINT('',#55239);
#13377=VERTEX_POINT('',#55241);
#13378=VERTEX_POINT('',#55245);
#13379=VERTEX_POINT('',#55249);
#13380=VERTEX_POINT('',#55255);
#13381=VERTEX_POINT('',#55256);
#13382=VERTEX_POINT('',#55258);
#13383=VERTEX_POINT('',#55260);
#13384=VERTEX_POINT('',#55264);
#13385=VERTEX_POINT('',#55268);
#13386=VERTEX_POINT('',#55274);
#13387=VERTEX_POINT('',#55275);
#13388=VERTEX_POINT('',#55277);
#13389=VERTEX_POINT('',#55279);
#13390=VERTEX_POINT('',#55283);
#13391=VERTEX_POINT('',#55287);
#13392=VERTEX_POINT('',#55293);
#13393=VERTEX_POINT('',#55294);
#13394=VERTEX_POINT('',#55296);
#13395=VERTEX_POINT('',#55298);
#13396=VERTEX_POINT('',#55302);
#13397=VERTEX_POINT('',#55306);
#13398=VERTEX_POINT('',#55312);
#13399=VERTEX_POINT('',#55313);
#13400=VERTEX_POINT('',#55315);
#13401=VERTEX_POINT('',#55317);
#13402=VERTEX_POINT('',#55321);
#13403=VERTEX_POINT('',#55325);
#13404=VERTEX_POINT('',#55331);
#13405=VERTEX_POINT('',#55332);
#13406=VERTEX_POINT('',#55334);
#13407=VERTEX_POINT('',#55336);
#13408=VERTEX_POINT('',#55340);
#13409=VERTEX_POINT('',#55344);
#13410=VERTEX_POINT('',#55350);
#13411=VERTEX_POINT('',#55351);
#13412=VERTEX_POINT('',#55353);
#13413=VERTEX_POINT('',#55355);
#13414=VERTEX_POINT('',#55359);
#13415=VERTEX_POINT('',#55363);
#13416=VERTEX_POINT('',#55369);
#13417=VERTEX_POINT('',#55370);
#13418=VERTEX_POINT('',#55372);
#13419=VERTEX_POINT('',#55374);
#13420=VERTEX_POINT('',#55378);
#13421=VERTEX_POINT('',#55382);
#13422=VERTEX_POINT('',#55388);
#13423=VERTEX_POINT('',#55389);
#13424=VERTEX_POINT('',#55391);
#13425=VERTEX_POINT('',#55393);
#13426=VERTEX_POINT('',#55397);
#13427=VERTEX_POINT('',#55401);
#13428=VERTEX_POINT('',#55407);
#13429=VERTEX_POINT('',#55408);
#13430=VERTEX_POINT('',#55410);
#13431=VERTEX_POINT('',#55412);
#13432=VERTEX_POINT('',#55416);
#13433=VERTEX_POINT('',#55420);
#13434=VERTEX_POINT('',#55426);
#13435=VERTEX_POINT('',#55427);
#13436=VERTEX_POINT('',#55429);
#13437=VERTEX_POINT('',#55431);
#13438=VERTEX_POINT('',#55435);
#13439=VERTEX_POINT('',#55439);
#13440=VERTEX_POINT('',#55445);
#13441=VERTEX_POINT('',#55446);
#13442=VERTEX_POINT('',#55448);
#13443=VERTEX_POINT('',#55450);
#13444=VERTEX_POINT('',#55454);
#13445=VERTEX_POINT('',#55458);
#13446=VERTEX_POINT('',#55464);
#13447=VERTEX_POINT('',#55465);
#13448=VERTEX_POINT('',#55467);
#13449=VERTEX_POINT('',#55469);
#13450=VERTEX_POINT('',#55473);
#13451=VERTEX_POINT('',#55477);
#13452=VERTEX_POINT('',#55483);
#13453=VERTEX_POINT('',#55484);
#13454=VERTEX_POINT('',#55486);
#13455=VERTEX_POINT('',#55488);
#13456=VERTEX_POINT('',#55492);
#13457=VERTEX_POINT('',#55496);
#13458=VERTEX_POINT('',#55502);
#13459=VERTEX_POINT('',#55503);
#13460=VERTEX_POINT('',#55505);
#13461=VERTEX_POINT('',#55507);
#13462=VERTEX_POINT('',#55511);
#13463=VERTEX_POINT('',#55515);
#13464=VERTEX_POINT('',#55521);
#13465=VERTEX_POINT('',#55522);
#13466=VERTEX_POINT('',#55524);
#13467=VERTEX_POINT('',#55526);
#13468=VERTEX_POINT('',#55530);
#13469=VERTEX_POINT('',#55534);
#13470=VERTEX_POINT('',#55540);
#13471=VERTEX_POINT('',#55541);
#13472=VERTEX_POINT('',#55543);
#13473=VERTEX_POINT('',#55545);
#13474=VERTEX_POINT('',#55549);
#13475=VERTEX_POINT('',#55553);
#13476=VERTEX_POINT('',#55559);
#13477=VERTEX_POINT('',#55560);
#13478=VERTEX_POINT('',#55562);
#13479=VERTEX_POINT('',#55564);
#13480=VERTEX_POINT('',#55568);
#13481=VERTEX_POINT('',#55570);
#13482=VERTEX_POINT('',#55574);
#13483=VERTEX_POINT('',#55578);
#13484=VERTEX_POINT('',#55582);
#13485=VERTEX_POINT('',#55583);
#13486=VERTEX_POINT('',#55585);
#13487=VERTEX_POINT('',#55587);
#13488=VERTEX_POINT('',#55591);
#13489=VERTEX_POINT('',#55595);
#13490=VERTEX_POINT('',#55601);
#13491=VERTEX_POINT('',#55602);
#13492=VERTEX_POINT('',#55604);
#13493=VERTEX_POINT('',#55606);
#13494=VERTEX_POINT('',#55610);
#13495=VERTEX_POINT('',#55614);
#13496=VERTEX_POINT('',#55620);
#13497=VERTEX_POINT('',#55621);
#13498=VERTEX_POINT('',#55623);
#13499=VERTEX_POINT('',#55625);
#13500=VERTEX_POINT('',#55629);
#13501=VERTEX_POINT('',#55633);
#13502=VERTEX_POINT('',#55639);
#13503=VERTEX_POINT('',#55640);
#13504=VERTEX_POINT('',#55642);
#13505=VERTEX_POINT('',#55644);
#13506=VERTEX_POINT('',#55648);
#13507=VERTEX_POINT('',#55652);
#13508=VERTEX_POINT('',#55658);
#13509=VERTEX_POINT('',#55659);
#13510=VERTEX_POINT('',#55661);
#13511=VERTEX_POINT('',#55663);
#13512=VERTEX_POINT('',#55667);
#13513=VERTEX_POINT('',#55671);
#13514=VERTEX_POINT('',#55677);
#13515=VERTEX_POINT('',#55678);
#13516=VERTEX_POINT('',#55680);
#13517=VERTEX_POINT('',#55682);
#13518=VERTEX_POINT('',#55686);
#13519=VERTEX_POINT('',#55690);
#13520=VERTEX_POINT('',#55696);
#13521=VERTEX_POINT('',#55697);
#13522=VERTEX_POINT('',#55699);
#13523=VERTEX_POINT('',#55701);
#13524=VERTEX_POINT('',#55705);
#13525=VERTEX_POINT('',#55709);
#13526=VERTEX_POINT('',#55715);
#13527=VERTEX_POINT('',#55716);
#13528=VERTEX_POINT('',#55718);
#13529=VERTEX_POINT('',#55720);
#13530=VERTEX_POINT('',#55724);
#13531=VERTEX_POINT('',#55728);
#13532=VERTEX_POINT('',#55734);
#13533=VERTEX_POINT('',#55735);
#13534=VERTEX_POINT('',#55737);
#13535=VERTEX_POINT('',#55739);
#13536=VERTEX_POINT('',#55743);
#13537=VERTEX_POINT('',#55747);
#13538=VERTEX_POINT('',#55753);
#13539=VERTEX_POINT('',#55754);
#13540=VERTEX_POINT('',#55756);
#13541=VERTEX_POINT('',#55758);
#13542=VERTEX_POINT('',#55762);
#13543=VERTEX_POINT('',#55766);
#13544=VERTEX_POINT('',#55772);
#13545=VERTEX_POINT('',#55773);
#13546=VERTEX_POINT('',#55775);
#13547=VERTEX_POINT('',#55777);
#13548=VERTEX_POINT('',#55781);
#13549=VERTEX_POINT('',#55785);
#13550=VERTEX_POINT('',#55791);
#13551=VERTEX_POINT('',#55792);
#13552=VERTEX_POINT('',#55794);
#13553=VERTEX_POINT('',#55796);
#13554=VERTEX_POINT('',#55800);
#13555=VERTEX_POINT('',#55804);
#13556=VERTEX_POINT('',#55810);
#13557=VERTEX_POINT('',#55811);
#13558=VERTEX_POINT('',#55813);
#13559=VERTEX_POINT('',#55815);
#13560=VERTEX_POINT('',#55819);
#13561=VERTEX_POINT('',#55823);
#13562=VERTEX_POINT('',#55829);
#13563=VERTEX_POINT('',#55830);
#13564=VERTEX_POINT('',#55832);
#13565=VERTEX_POINT('',#55834);
#13566=VERTEX_POINT('',#55838);
#13567=VERTEX_POINT('',#55842);
#13568=VERTEX_POINT('',#55848);
#13569=VERTEX_POINT('',#55849);
#13570=VERTEX_POINT('',#55851);
#13571=VERTEX_POINT('',#55853);
#13572=VERTEX_POINT('',#55857);
#13573=VERTEX_POINT('',#55861);
#13574=VERTEX_POINT('',#55867);
#13575=VERTEX_POINT('',#55868);
#13576=VERTEX_POINT('',#55870);
#13577=VERTEX_POINT('',#55872);
#13578=VERTEX_POINT('',#55876);
#13579=VERTEX_POINT('',#55880);
#13580=VERTEX_POINT('',#55886);
#13581=VERTEX_POINT('',#55887);
#13582=VERTEX_POINT('',#55889);
#13583=VERTEX_POINT('',#55891);
#13584=VERTEX_POINT('',#55895);
#13585=VERTEX_POINT('',#55899);
#13586=VERTEX_POINT('',#55905);
#13587=VERTEX_POINT('',#55906);
#13588=VERTEX_POINT('',#55908);
#13589=VERTEX_POINT('',#55910);
#13590=VERTEX_POINT('',#55914);
#13591=VERTEX_POINT('',#55918);
#13592=VERTEX_POINT('',#55924);
#13593=VERTEX_POINT('',#55925);
#13594=VERTEX_POINT('',#55929);
#13595=VERTEX_POINT('',#55930);
#13596=VERTEX_POINT('',#55932);
#13597=VERTEX_POINT('',#55934);
#13598=VERTEX_POINT('',#55938);
#13599=VERTEX_POINT('',#55940);
#13600=VERTEX_POINT('',#55944);
#13601=VERTEX_POINT('',#55946);
#13602=VERTEX_POINT('',#55950);
#13603=VERTEX_POINT('',#55952);
#13604=VERTEX_POINT('',#55956);
#13605=VERTEX_POINT('',#55958);
#13606=VERTEX_POINT('',#55966);
#13607=VERTEX_POINT('',#55971);
#13608=VERTEX_POINT('',#55976);
#13609=VERTEX_POINT('',#55982);
#13610=VERTEX_POINT('',#55985);
#13611=VERTEX_POINT('',#55989);
#13612=VERTEX_POINT('',#55993);
#13613=VERTEX_POINT('',#55999);
#13614=VERTEX_POINT('',#56000);
#13615=VERTEX_POINT('',#56002);
#13616=VERTEX_POINT('',#56013);
#13617=VERTEX_POINT('',#56023);
#13618=VERTEX_POINT('',#56024);
#13619=VERTEX_POINT('',#56071);
#13620=VERTEX_POINT('',#56072);
#13621=VERTEX_POINT('',#56119);
#13622=VERTEX_POINT('',#56120);
#13623=VERTEX_POINT('',#56167);
#13624=VERTEX_POINT('',#56168);
#13625=VERTEX_POINT('',#56221);
#13626=VERTEX_POINT('',#56222);
#13627=VERTEX_POINT('',#56269);
#13628=VERTEX_POINT('',#56270);
#13629=VERTEX_POINT('',#56317);
#13630=VERTEX_POINT('',#56318);
#13631=VERTEX_POINT('',#56371);
#13632=VERTEX_POINT('',#56372);
#13633=VERTEX_POINT('',#56419);
#13634=VERTEX_POINT('',#56420);
#13635=VERTEX_POINT('',#56467);
#13636=VERTEX_POINT('',#56468);
#13637=VERTEX_POINT('',#56515);
#13638=VERTEX_POINT('',#56516);
#13639=VERTEX_POINT('',#56569);
#13640=VERTEX_POINT('',#56570);
#13641=VERTEX_POINT('',#56617);
#13642=VERTEX_POINT('',#56618);
#13643=VERTEX_POINT('',#56665);
#13644=VERTEX_POINT('',#56666);
#13645=VERTEX_POINT('',#56719);
#13646=VERTEX_POINT('',#56720);
#13647=VERTEX_POINT('',#56767);
#13648=VERTEX_POINT('',#56768);
#13649=VERTEX_POINT('',#56815);
#13650=VERTEX_POINT('',#56816);
#13651=VERTEX_POINT('',#56863);
#13652=VERTEX_POINT('',#56864);
#13653=VERTEX_POINT('',#56917);
#13654=VERTEX_POINT('',#56918);
#13655=VERTEX_POINT('',#56965);
#13656=VERTEX_POINT('',#56966);
#13657=VERTEX_POINT('',#57013);
#13658=VERTEX_POINT('',#57014);
#13659=VERTEX_POINT('',#57067);
#13660=VERTEX_POINT('',#57068);
#13661=VERTEX_POINT('',#57115);
#13662=VERTEX_POINT('',#57116);
#13663=VERTEX_POINT('',#57163);
#13664=VERTEX_POINT('',#57164);
#13665=VERTEX_POINT('',#57211);
#13666=VERTEX_POINT('',#57212);
#13667=VERTEX_POINT('',#57265);
#13668=VERTEX_POINT('',#57266);
#13669=VERTEX_POINT('',#57313);
#13670=VERTEX_POINT('',#57314);
#13671=VERTEX_POINT('',#57361);
#13672=VERTEX_POINT('',#57362);
#13673=VERTEX_POINT('',#57415);
#13674=VERTEX_POINT('',#57416);
#13675=VERTEX_POINT('',#57463);
#13676=VERTEX_POINT('',#57464);
#13677=VERTEX_POINT('',#57511);
#13678=VERTEX_POINT('',#57512);
#13679=VERTEX_POINT('',#57559);
#13680=VERTEX_POINT('',#57560);
#13681=VERTEX_POINT('',#57613);
#13682=VERTEX_POINT('',#57614);
#13683=VERTEX_POINT('',#57661);
#13684=VERTEX_POINT('',#57662);
#13685=VERTEX_POINT('',#57709);
#13686=VERTEX_POINT('',#57710);
#13687=VERTEX_POINT('',#57763);
#13688=VERTEX_POINT('',#57764);
#13689=VERTEX_POINT('',#57811);
#13690=VERTEX_POINT('',#57812);
#13691=VERTEX_POINT('',#57859);
#13692=VERTEX_POINT('',#57860);
#13693=VERTEX_POINT('',#57907);
#13694=VERTEX_POINT('',#57908);
#13695=VERTEX_POINT('',#57961);
#13696=VERTEX_POINT('',#57962);
#13697=VERTEX_POINT('',#58009);
#13698=VERTEX_POINT('',#58010);
#13699=VERTEX_POINT('',#58057);
#13700=VERTEX_POINT('',#58058);
#13701=VERTEX_POINT('',#58111);
#13702=VERTEX_POINT('',#58112);
#13703=VERTEX_POINT('',#58159);
#13704=VERTEX_POINT('',#58160);
#13705=VERTEX_POINT('',#58207);
#13706=VERTEX_POINT('',#58208);
#13707=VERTEX_POINT('',#58255);
#13708=VERTEX_POINT('',#58256);
#13709=VERTEX_POINT('',#58309);
#13710=VERTEX_POINT('',#58310);
#13711=VERTEX_POINT('',#58357);
#13712=VERTEX_POINT('',#58358);
#13713=VERTEX_POINT('',#58405);
#13714=VERTEX_POINT('',#58406);
#13715=VERTEX_POINT('',#58459);
#13716=VERTEX_POINT('',#58460);
#13717=VERTEX_POINT('',#58507);
#13718=VERTEX_POINT('',#58508);
#13719=VERTEX_POINT('',#58555);
#13720=VERTEX_POINT('',#58556);
#13721=VERTEX_POINT('',#58603);
#13722=VERTEX_POINT('',#58604);
#13723=VERTEX_POINT('',#58657);
#13724=VERTEX_POINT('',#58658);
#13725=VERTEX_POINT('',#58705);
#13726=VERTEX_POINT('',#58706);
#13727=VERTEX_POINT('',#58753);
#13728=VERTEX_POINT('',#58754);
#13729=VERTEX_POINT('',#58807);
#13730=VERTEX_POINT('',#58808);
#13731=VERTEX_POINT('',#58855);
#13732=VERTEX_POINT('',#58856);
#13733=VERTEX_POINT('',#58903);
#13734=VERTEX_POINT('',#58904);
#13735=VERTEX_POINT('',#58951);
#13736=VERTEX_POINT('',#58952);
#13737=VERTEX_POINT('',#59005);
#13738=VERTEX_POINT('',#59006);
#13739=VERTEX_POINT('',#59053);
#13740=VERTEX_POINT('',#59054);
#13741=VERTEX_POINT('',#59101);
#13742=VERTEX_POINT('',#59102);
#13743=VERTEX_POINT('',#59155);
#13744=VERTEX_POINT('',#59156);
#13745=VERTEX_POINT('',#59203);
#13746=VERTEX_POINT('',#59204);
#13747=VERTEX_POINT('',#59251);
#13748=VERTEX_POINT('',#59252);
#13749=VERTEX_POINT('',#59299);
#13750=VERTEX_POINT('',#59300);
#13751=VERTEX_POINT('',#59353);
#13752=VERTEX_POINT('',#59354);
#13753=VERTEX_POINT('',#59401);
#13754=VERTEX_POINT('',#59402);
#13755=VERTEX_POINT('',#59404);
#13756=VERTEX_POINT('',#59410);
#13757=VERTEX_POINT('',#59417);
#13758=VERTEX_POINT('',#59418);
#13759=VERTEX_POINT('',#59441);
#13760=VERTEX_POINT('',#59442);
#13761=VERTEX_POINT('',#59466);
#13762=VERTEX_POINT('',#59467);
#13763=VERTEX_POINT('',#59491);
#13764=VERTEX_POINT('',#59492);
#13765=VERTEX_POINT('',#59515);
#13766=VERTEX_POINT('',#59516);
#13767=VERTEX_POINT('',#59539);
#13768=VERTEX_POINT('',#59540);
#13769=VERTEX_POINT('',#59564);
#13770=VERTEX_POINT('',#59565);
#13771=VERTEX_POINT('',#59589);
#13772=VERTEX_POINT('',#59590);
#13773=VERTEX_POINT('',#59613);
#13774=VERTEX_POINT('',#59614);
#13775=VERTEX_POINT('',#59638);
#13776=VERTEX_POINT('',#59639);
#13777=VERTEX_POINT('',#59663);
#13778=VERTEX_POINT('',#59664);
#13779=VERTEX_POINT('',#59687);
#13780=VERTEX_POINT('',#59688);
#13781=VERTEX_POINT('',#59711);
#13782=VERTEX_POINT('',#59712);
#13783=VERTEX_POINT('',#59736);
#13784=VERTEX_POINT('',#59737);
#13785=VERTEX_POINT('',#59761);
#13786=VERTEX_POINT('',#59762);
#13787=VERTEX_POINT('',#59785);
#13788=VERTEX_POINT('',#59786);
#13789=VERTEX_POINT('',#59810);
#13790=VERTEX_POINT('',#59811);
#13791=VERTEX_POINT('',#59835);
#13792=VERTEX_POINT('',#59836);
#13793=VERTEX_POINT('',#59859);
#13794=VERTEX_POINT('',#59860);
#13795=VERTEX_POINT('',#59883);
#13796=VERTEX_POINT('',#59884);
#13797=VERTEX_POINT('',#59908);
#13798=VERTEX_POINT('',#59909);
#13799=VERTEX_POINT('',#59933);
#13800=VERTEX_POINT('',#59934);
#13801=VERTEX_POINT('',#59957);
#13802=VERTEX_POINT('',#59958);
#13803=VERTEX_POINT('',#59982);
#13804=VERTEX_POINT('',#59983);
#13805=VERTEX_POINT('',#60007);
#13806=VERTEX_POINT('',#60008);
#13807=VERTEX_POINT('',#60031);
#13808=VERTEX_POINT('',#60032);
#13809=VERTEX_POINT('',#60055);
#13810=VERTEX_POINT('',#60056);
#13811=VERTEX_POINT('',#60080);
#13812=VERTEX_POINT('',#60081);
#13813=VERTEX_POINT('',#60105);
#13814=VERTEX_POINT('',#60106);
#13815=VERTEX_POINT('',#60129);
#13816=VERTEX_POINT('',#60130);
#13817=VERTEX_POINT('',#60154);
#13818=VERTEX_POINT('',#60155);
#13819=VERTEX_POINT('',#60179);
#13820=VERTEX_POINT('',#60180);
#13821=VERTEX_POINT('',#60203);
#13822=VERTEX_POINT('',#60204);
#13823=VERTEX_POINT('',#60227);
#13824=VERTEX_POINT('',#60228);
#13825=VERTEX_POINT('',#60252);
#13826=VERTEX_POINT('',#60253);
#13827=VERTEX_POINT('',#60277);
#13828=VERTEX_POINT('',#60278);
#13829=VERTEX_POINT('',#60301);
#13830=VERTEX_POINT('',#60302);
#13831=VERTEX_POINT('',#60326);
#13832=VERTEX_POINT('',#60327);
#13833=VERTEX_POINT('',#60351);
#13834=VERTEX_POINT('',#60352);
#13835=VERTEX_POINT('',#60375);
#13836=VERTEX_POINT('',#60376);
#13837=VERTEX_POINT('',#60399);
#13838=VERTEX_POINT('',#60400);
#13839=VERTEX_POINT('',#60424);
#13840=VERTEX_POINT('',#60425);
#13841=VERTEX_POINT('',#60449);
#13842=VERTEX_POINT('',#60450);
#13843=VERTEX_POINT('',#60473);
#13844=VERTEX_POINT('',#60474);
#13845=VERTEX_POINT('',#60498);
#13846=VERTEX_POINT('',#60499);
#13847=VERTEX_POINT('',#60523);
#13848=VERTEX_POINT('',#60524);
#13849=VERTEX_POINT('',#60547);
#13850=VERTEX_POINT('',#60548);
#13851=VERTEX_POINT('',#60571);
#13852=VERTEX_POINT('',#60572);
#13853=VERTEX_POINT('',#60596);
#13854=VERTEX_POINT('',#60597);
#13855=VERTEX_POINT('',#60621);
#13856=VERTEX_POINT('',#60622);
#13857=VERTEX_POINT('',#60645);
#13858=VERTEX_POINT('',#60646);
#13859=VERTEX_POINT('',#60670);
#13860=VERTEX_POINT('',#60671);
#13861=VERTEX_POINT('',#60695);
#13862=VERTEX_POINT('',#60696);
#13863=VERTEX_POINT('',#60719);
#13864=VERTEX_POINT('',#60720);
#13865=VERTEX_POINT('',#60743);
#13866=VERTEX_POINT('',#60744);
#13867=VERTEX_POINT('',#60768);
#13868=VERTEX_POINT('',#60769);
#13869=VERTEX_POINT('',#60793);
#13870=VERTEX_POINT('',#60794);
#13871=VERTEX_POINT('',#60817);
#13872=VERTEX_POINT('',#60818);
#13873=VERTEX_POINT('',#60842);
#13874=VERTEX_POINT('',#60843);
#13875=VERTEX_POINT('',#60867);
#13876=VERTEX_POINT('',#60868);
#13877=VERTEX_POINT('',#60891);
#13878=VERTEX_POINT('',#60892);
#13879=VERTEX_POINT('',#60915);
#13880=VERTEX_POINT('',#60916);
#13881=VERTEX_POINT('',#60940);
#13882=VERTEX_POINT('',#60941);
#13883=VERTEX_POINT('',#60965);
#13884=VERTEX_POINT('',#60966);
#13885=VERTEX_POINT('',#60989);
#13886=VERTEX_POINT('',#60990);
#13887=VERTEX_POINT('',#61014);
#13888=VERTEX_POINT('',#61015);
#13889=VERTEX_POINT('',#61039);
#13890=VERTEX_POINT('',#61040);
#13891=VERTEX_POINT('',#61063);
#13892=VERTEX_POINT('',#61064);
#13893=VERTEX_POINT('',#61087);
#13894=VERTEX_POINT('',#61173);
#13895=VERTEX_POINT('',#61175);
#13896=VERTEX_POINT('',#63027);
#13897=VERTEX_POINT('',#63123);
#13898=VERTEX_POINT('',#63126);
#13899=VERTEX_POINT('',#64985);
#13900=VERTEX_POINT('',#64991);
#13901=VERTEX_POINT('',#64994);
#13902=VERTEX_POINT('',#64995);
#13903=VERTEX_POINT('',#64997);
#13904=VERTEX_POINT('',#64999);
#13905=VERTEX_POINT('',#65003);
#13906=VERTEX_POINT('',#65007);
#13907=VERTEX_POINT('',#65013);
#13908=VERTEX_POINT('',#65014);
#13909=VERTEX_POINT('',#65016);
#13910=VERTEX_POINT('',#65018);
#13911=VERTEX_POINT('',#65022);
#13912=VERTEX_POINT('',#65026);
#13913=VERTEX_POINT('',#65032);
#13914=VERTEX_POINT('',#65033);
#13915=VERTEX_POINT('',#65035);
#13916=VERTEX_POINT('',#65037);
#13917=VERTEX_POINT('',#65041);
#13918=VERTEX_POINT('',#65045);
#13919=VERTEX_POINT('',#65051);
#13920=VERTEX_POINT('',#65052);
#13921=VERTEX_POINT('',#65054);
#13922=VERTEX_POINT('',#65056);
#13923=VERTEX_POINT('',#65060);
#13924=VERTEX_POINT('',#65064);
#13925=VERTEX_POINT('',#65070);
#13926=VERTEX_POINT('',#65071);
#13927=VERTEX_POINT('',#65073);
#13928=VERTEX_POINT('',#65075);
#13929=VERTEX_POINT('',#65079);
#13930=VERTEX_POINT('',#65083);
#13931=VERTEX_POINT('',#65089);
#13932=VERTEX_POINT('',#65090);
#13933=VERTEX_POINT('',#65092);
#13934=VERTEX_POINT('',#65094);
#13935=VERTEX_POINT('',#65098);
#13936=VERTEX_POINT('',#65102);
#13937=VERTEX_POINT('',#65108);
#13938=VERTEX_POINT('',#65109);
#13939=VERTEX_POINT('',#65111);
#13940=VERTEX_POINT('',#65113);
#13941=VERTEX_POINT('',#65117);
#13942=VERTEX_POINT('',#65121);
#13943=VERTEX_POINT('',#65127);
#13944=VERTEX_POINT('',#65128);
#13945=VERTEX_POINT('',#65130);
#13946=VERTEX_POINT('',#65132);
#13947=VERTEX_POINT('',#65136);
#13948=VERTEX_POINT('',#65140);
#13949=VERTEX_POINT('',#65146);
#13950=VERTEX_POINT('',#65147);
#13951=VERTEX_POINT('',#65149);
#13952=VERTEX_POINT('',#65151);
#13953=VERTEX_POINT('',#65155);
#13954=VERTEX_POINT('',#65159);
#13955=VERTEX_POINT('',#65165);
#13956=VERTEX_POINT('',#65166);
#13957=VERTEX_POINT('',#65168);
#13958=VERTEX_POINT('',#65170);
#13959=VERTEX_POINT('',#65174);
#13960=VERTEX_POINT('',#65178);
#13961=VERTEX_POINT('',#65184);
#13962=VERTEX_POINT('',#65185);
#13963=VERTEX_POINT('',#65187);
#13964=VERTEX_POINT('',#65189);
#13965=VERTEX_POINT('',#65193);
#13966=VERTEX_POINT('',#65197);
#13967=VERTEX_POINT('',#65203);
#13968=VERTEX_POINT('',#65204);
#13969=VERTEX_POINT('',#65206);
#13970=VERTEX_POINT('',#65208);
#13971=VERTEX_POINT('',#65212);
#13972=VERTEX_POINT('',#65216);
#13973=VERTEX_POINT('',#65222);
#13974=VERTEX_POINT('',#65223);
#13975=VERTEX_POINT('',#65225);
#13976=VERTEX_POINT('',#65227);
#13977=VERTEX_POINT('',#65231);
#13978=VERTEX_POINT('',#65235);
#13979=VERTEX_POINT('',#65241);
#13980=VERTEX_POINT('',#65242);
#13981=VERTEX_POINT('',#65244);
#13982=VERTEX_POINT('',#65246);
#13983=VERTEX_POINT('',#65250);
#13984=VERTEX_POINT('',#65254);
#13985=VERTEX_POINT('',#65260);
#13986=VERTEX_POINT('',#65261);
#13987=VERTEX_POINT('',#65263);
#13988=VERTEX_POINT('',#65265);
#13989=VERTEX_POINT('',#65269);
#13990=VERTEX_POINT('',#65273);
#13991=VERTEX_POINT('',#65279);
#13992=VERTEX_POINT('',#65280);
#13993=VERTEX_POINT('',#65282);
#13994=VERTEX_POINT('',#65284);
#13995=VERTEX_POINT('',#65288);
#13996=VERTEX_POINT('',#65292);
#13997=VERTEX_POINT('',#65298);
#13998=VERTEX_POINT('',#65299);
#13999=VERTEX_POINT('',#65301);
#14000=VERTEX_POINT('',#65303);
#14001=VERTEX_POINT('',#65307);
#14002=VERTEX_POINT('',#65311);
#14003=VERTEX_POINT('',#65317);
#14004=VERTEX_POINT('',#65318);
#14005=VERTEX_POINT('',#65320);
#14006=VERTEX_POINT('',#65322);
#14007=VERTEX_POINT('',#65326);
#14008=VERTEX_POINT('',#65328);
#14009=VERTEX_POINT('',#65332);
#14010=VERTEX_POINT('',#65336);
#14011=VERTEX_POINT('',#65340);
#14012=VERTEX_POINT('',#65341);
#14013=VERTEX_POINT('',#65343);
#14014=VERTEX_POINT('',#65345);
#14015=VERTEX_POINT('',#65349);
#14016=VERTEX_POINT('',#65353);
#14017=VERTEX_POINT('',#65359);
#14018=VERTEX_POINT('',#65360);
#14019=VERTEX_POINT('',#65362);
#14020=VERTEX_POINT('',#65364);
#14021=VERTEX_POINT('',#65368);
#14022=VERTEX_POINT('',#65372);
#14023=VERTEX_POINT('',#65378);
#14024=VERTEX_POINT('',#65379);
#14025=VERTEX_POINT('',#65381);
#14026=VERTEX_POINT('',#65383);
#14027=VERTEX_POINT('',#65387);
#14028=VERTEX_POINT('',#65391);
#14029=VERTEX_POINT('',#65397);
#14030=VERTEX_POINT('',#65398);
#14031=VERTEX_POINT('',#65400);
#14032=VERTEX_POINT('',#65402);
#14033=VERTEX_POINT('',#65406);
#14034=VERTEX_POINT('',#65410);
#14035=VERTEX_POINT('',#65416);
#14036=VERTEX_POINT('',#65417);
#14037=VERTEX_POINT('',#65419);
#14038=VERTEX_POINT('',#65421);
#14039=VERTEX_POINT('',#65425);
#14040=VERTEX_POINT('',#65429);
#14041=VERTEX_POINT('',#65435);
#14042=VERTEX_POINT('',#65436);
#14043=VERTEX_POINT('',#65438);
#14044=VERTEX_POINT('',#65440);
#14045=VERTEX_POINT('',#65444);
#14046=VERTEX_POINT('',#65448);
#14047=VERTEX_POINT('',#65454);
#14048=VERTEX_POINT('',#65455);
#14049=VERTEX_POINT('',#65457);
#14050=VERTEX_POINT('',#65459);
#14051=VERTEX_POINT('',#65463);
#14052=VERTEX_POINT('',#65467);
#14053=VERTEX_POINT('',#65473);
#14054=VERTEX_POINT('',#65474);
#14055=VERTEX_POINT('',#65476);
#14056=VERTEX_POINT('',#65478);
#14057=VERTEX_POINT('',#65482);
#14058=VERTEX_POINT('',#65486);
#14059=VERTEX_POINT('',#65492);
#14060=VERTEX_POINT('',#65493);
#14061=VERTEX_POINT('',#65495);
#14062=VERTEX_POINT('',#65497);
#14063=VERTEX_POINT('',#65501);
#14064=VERTEX_POINT('',#65505);
#14065=VERTEX_POINT('',#65511);
#14066=VERTEX_POINT('',#65512);
#14067=VERTEX_POINT('',#65514);
#14068=VERTEX_POINT('',#65516);
#14069=VERTEX_POINT('',#65520);
#14070=VERTEX_POINT('',#65524);
#14071=VERTEX_POINT('',#65530);
#14072=VERTEX_POINT('',#65531);
#14073=VERTEX_POINT('',#65533);
#14074=VERTEX_POINT('',#65535);
#14075=VERTEX_POINT('',#65539);
#14076=VERTEX_POINT('',#65543);
#14077=VERTEX_POINT('',#65549);
#14078=VERTEX_POINT('',#65550);
#14079=VERTEX_POINT('',#65552);
#14080=VERTEX_POINT('',#65554);
#14081=VERTEX_POINT('',#65558);
#14082=VERTEX_POINT('',#65562);
#14083=VERTEX_POINT('',#65568);
#14084=VERTEX_POINT('',#65569);
#14085=VERTEX_POINT('',#65571);
#14086=VERTEX_POINT('',#65573);
#14087=VERTEX_POINT('',#65577);
#14088=VERTEX_POINT('',#65581);
#14089=VERTEX_POINT('',#65587);
#14090=VERTEX_POINT('',#65588);
#14091=VERTEX_POINT('',#65590);
#14092=VERTEX_POINT('',#65592);
#14093=VERTEX_POINT('',#65596);
#14094=VERTEX_POINT('',#65600);
#14095=VERTEX_POINT('',#65606);
#14096=VERTEX_POINT('',#65607);
#14097=VERTEX_POINT('',#65609);
#14098=VERTEX_POINT('',#65611);
#14099=VERTEX_POINT('',#65615);
#14100=VERTEX_POINT('',#65619);
#14101=VERTEX_POINT('',#65625);
#14102=VERTEX_POINT('',#65626);
#14103=VERTEX_POINT('',#65628);
#14104=VERTEX_POINT('',#65630);
#14105=VERTEX_POINT('',#65634);
#14106=VERTEX_POINT('',#65638);
#14107=VERTEX_POINT('',#65644);
#14108=VERTEX_POINT('',#65645);
#14109=VERTEX_POINT('',#65647);
#14110=VERTEX_POINT('',#65649);
#14111=VERTEX_POINT('',#65653);
#14112=VERTEX_POINT('',#65657);
#14113=VERTEX_POINT('',#65663);
#14114=VERTEX_POINT('',#65664);
#14115=VERTEX_POINT('',#65666);
#14116=VERTEX_POINT('',#65668);
#14117=VERTEX_POINT('',#65672);
#14118=VERTEX_POINT('',#65676);
#14119=VERTEX_POINT('',#65682);
#14120=VERTEX_POINT('',#65683);
#14121=VERTEX_POINT('',#65687);
#14122=VERTEX_POINT('',#65688);
#14123=VERTEX_POINT('',#65690);
#14124=VERTEX_POINT('',#65692);
#14125=VERTEX_POINT('',#65696);
#14126=VERTEX_POINT('',#65698);
#14127=VERTEX_POINT('',#65702);
#14128=VERTEX_POINT('',#65704);
#14129=VERTEX_POINT('',#65708);
#14130=VERTEX_POINT('',#65710);
#14131=VERTEX_POINT('',#65714);
#14132=VERTEX_POINT('',#65716);
#14133=VERTEX_POINT('',#65724);
#14134=VERTEX_POINT('',#65729);
#14135=VERTEX_POINT('',#65734);
#14136=VERTEX_POINT('',#65740);
#14137=VERTEX_POINT('',#65741);
#14138=VERTEX_POINT('',#65743);
#14139=VERTEX_POINT('',#65745);
#14140=VERTEX_POINT('',#65749);
#14141=VERTEX_POINT('',#65751);
#14142=VERTEX_POINT('',#65755);
#14143=VERTEX_POINT('',#65756);
#14144=VERTEX_POINT('',#65760);
#14145=VERTEX_POINT('',#65762);
#14146=VERTEX_POINT('',#65768);
#14147=VERTEX_POINT('',#65770);
#14148=VERTEX_POINT('',#65774);
#14149=VERTEX_POINT('',#65778);
#14150=VERTEX_POINT('',#65780);
#14151=VERTEX_POINT('',#65788);
#14152=VERTEX_POINT('',#65789);
#14153=VERTEX_POINT('',#65793);
#14154=VERTEX_POINT('',#65795);
#14155=VERTEX_POINT('',#65801);
#14156=VERTEX_POINT('',#65806);
#14157=VERTEX_POINT('',#65808);
#14158=VERTEX_POINT('',#65814);
#14159=VERTEX_POINT('',#65816);
#14160=VERTEX_POINT('',#65820);
#14161=VERTEX_POINT('',#65826);
#14162=VERTEX_POINT('',#65827);
#14163=VERTEX_POINT('',#65829);
#14164=VERTEX_POINT('',#65831);
#14165=VERTEX_POINT('',#65835);
#14166=VERTEX_POINT('',#65837);
#14167=VERTEX_POINT('',#65841);
#14168=VERTEX_POINT('',#65843);
#14169=VERTEX_POINT('',#65849);
#14170=VERTEX_POINT('',#65853);
#14171=VERTEX_POINT('',#65858);
#14172=VERTEX_POINT('',#65859);
#14173=VERTEX_POINT('',#65863);
#14174=VERTEX_POINT('',#65865);
#14175=VERTEX_POINT('',#65871);
#14176=VERTEX_POINT('',#65873);
#14177=VERTEX_POINT('',#65877);
#14178=VERTEX_POINT('',#65881);
#14179=VERTEX_POINT('',#65883);
#14180=VERTEX_POINT('',#65891);
#14181=VERTEX_POINT('',#65892);
#14182=VERTEX_POINT('',#65894);
#14183=VERTEX_POINT('',#65896);
#14184=VERTEX_POINT('',#65900);
#14185=VERTEX_POINT('',#65902);
#14186=VERTEX_POINT('',#65906);
#14187=VERTEX_POINT('',#65912);
#14188=VERTEX_POINT('',#65916);
#14189=VERTEX_POINT('',#65922);
#14190=VERTEX_POINT('',#65927);
#14191=VERTEX_POINT('',#65928);
#14192=VERTEX_POINT('',#65932);
#14193=VERTEX_POINT('',#65934);
#14194=VERTEX_POINT('',#65940);
#14195=VERTEX_POINT('',#65942);
#14196=VERTEX_POINT('',#65946);
#14197=VERTEX_POINT('',#65950);
#14198=VERTEX_POINT('',#65952);
#14199=VERTEX_POINT('',#65960);
#14200=VERTEX_POINT('',#65964);
#14201=VERTEX_POINT('',#65968);
#14202=VERTEX_POINT('',#65972);
#14203=VERTEX_POINT('',#65973);
#14204=VERTEX_POINT('',#65975);
#14205=VERTEX_POINT('',#65977);
#14206=VERTEX_POINT('',#65981);
#14207=VERTEX_POINT('',#65983);
#14208=VERTEX_POINT('',#65987);
#14209=VERTEX_POINT('',#65989);
#14210=VERTEX_POINT('',#65993);
#14211=VERTEX_POINT('',#65999);
#14212=VERTEX_POINT('',#66003);
#14213=VERTEX_POINT('',#66012);
#14214=VERTEX_POINT('',#66018);
#14215=VERTEX_POINT('',#66022);
#14216=VERTEX_POINT('',#66035);
#14217=VERTEX_POINT('',#66047);
#14218=VERTEX_POINT('',#66053);
#14219=VERTEX_POINT('',#66054);
#14220=VERTEX_POINT('',#66056);
#14221=VERTEX_POINT('',#66073);
#14222=VERTEX_POINT('',#66086);
#14223=VERTEX_POINT('',#66087);
#14224=VERTEX_POINT('',#66170);
#14225=VERTEX_POINT('',#66171);
#14226=VERTEX_POINT('',#66260);
#14227=VERTEX_POINT('',#66261);
#14228=VERTEX_POINT('',#66350);
#14229=VERTEX_POINT('',#66351);
#14230=VERTEX_POINT('',#66434);
#14231=VERTEX_POINT('',#66435);
#14232=VERTEX_POINT('',#66524);
#14233=VERTEX_POINT('',#66525);
#14234=VERTEX_POINT('',#66608);
#14235=VERTEX_POINT('',#66609);
#14236=VERTEX_POINT('',#66698);
#14237=VERTEX_POINT('',#66699);
#14238=VERTEX_POINT('',#66788);
#14239=VERTEX_POINT('',#66789);
#14240=VERTEX_POINT('',#66872);
#14241=VERTEX_POINT('',#66873);
#14242=VERTEX_POINT('',#66962);
#14243=VERTEX_POINT('',#66963);
#14244=VERTEX_POINT('',#67046);
#14245=VERTEX_POINT('',#67047);
#14246=VERTEX_POINT('',#67136);
#14247=VERTEX_POINT('',#67137);
#14248=VERTEX_POINT('',#67226);
#14249=VERTEX_POINT('',#67227);
#14250=VERTEX_POINT('',#67310);
#14251=VERTEX_POINT('',#67311);
#14252=VERTEX_POINT('',#67400);
#14253=VERTEX_POINT('',#67401);
#14254=VERTEX_POINT('',#67403);
#14255=VERTEX_POINT('',#67410);
#14256=VERTEX_POINT('',#67411);
#14257=VERTEX_POINT('',#67430);
#14258=VERTEX_POINT('',#67447);
#14259=VERTEX_POINT('',#67448);
#14260=VERTEX_POINT('',#67484);
#14261=VERTEX_POINT('',#67485);
#14262=VERTEX_POINT('',#67521);
#14263=VERTEX_POINT('',#67522);
#14264=VERTEX_POINT('',#67559);
#14265=VERTEX_POINT('',#67560);
#14266=VERTEX_POINT('',#67596);
#14267=VERTEX_POINT('',#67597);
#14268=VERTEX_POINT('',#67633);
#14269=VERTEX_POINT('',#67634);
#14270=VERTEX_POINT('',#67670);
#14271=VERTEX_POINT('',#67671);
#14272=VERTEX_POINT('',#67707);
#14273=VERTEX_POINT('',#67708);
#14274=VERTEX_POINT('',#67745);
#14275=VERTEX_POINT('',#67746);
#14276=VERTEX_POINT('',#67782);
#14277=VERTEX_POINT('',#67783);
#14278=VERTEX_POINT('',#67819);
#14279=VERTEX_POINT('',#67820);
#14280=VERTEX_POINT('',#67856);
#14281=VERTEX_POINT('',#67857);
#14282=VERTEX_POINT('',#67893);
#14283=VERTEX_POINT('',#67894);
#14284=VERTEX_POINT('',#67931);
#14285=VERTEX_POINT('',#67932);
#14286=VERTEX_POINT('',#67968);
#14287=VERTEX_POINT('',#67970);
#14288=VERTEX_POINT('',#67972);
#14289=VERTEX_POINT('',#67976);
#14290=VERTEX_POINT('',#67977);
#14291=VERTEX_POINT('',#67981);
#14292=VERTEX_POINT('',#67982);
#14293=VERTEX_POINT('',#67989);
#14294=VERTEX_POINT('',#67996);
#14295=VERTEX_POINT('',#67998);
#14296=VERTEX_POINT('',#68011);
#14297=VERTEX_POINT('',#68014);
#14298=VERTEX_POINT('',#68018);
#14299=VERTEX_POINT('',#68128);
#14300=VERTEX_POINT('',#68129);
#14301=VERTEX_POINT('',#68131);
#14302=VERTEX_POINT('',#68194);
#14303=VERTEX_POINT('',#68196);
#14304=VERTEX_POINT('',#69019);
#14305=VERTEX_POINT('',#69157);
#14306=VERTEX_POINT('',#69285);
#14307=VERTEX_POINT('',#69288);
#14308=VERTEX_POINT('',#70238);
#14309=VERTEX_POINT('',#70374);
#14310=VERTEX_POINT('',#70379);
#14311=VERTEX_POINT('',#70383);
#14312=VERTEX_POINT('',#70386);
#14313=VERTEX_POINT('',#70393);
#14314=VERTEX_POINT('',#70394);
#14315=VERTEX_POINT('',#70396);
#14316=VERTEX_POINT('',#70407);
#14317=VERTEX_POINT('',#70420);
#14318=VERTEX_POINT('',#70421);
#14319=VERTEX_POINT('',#70468);
#14320=VERTEX_POINT('',#70469);
#14321=VERTEX_POINT('',#70516);
#14322=VERTEX_POINT('',#70517);
#14323=VERTEX_POINT('',#70564);
#14324=VERTEX_POINT('',#70565);
#14325=VERTEX_POINT('',#70618);
#14326=VERTEX_POINT('',#70619);
#14327=VERTEX_POINT('',#70666);
#14328=VERTEX_POINT('',#70667);
#14329=VERTEX_POINT('',#70714);
#14330=VERTEX_POINT('',#70715);
#14331=VERTEX_POINT('',#70768);
#14332=VERTEX_POINT('',#70769);
#14333=VERTEX_POINT('',#70816);
#14334=VERTEX_POINT('',#70817);
#14335=VERTEX_POINT('',#70864);
#14336=VERTEX_POINT('',#70865);
#14337=VERTEX_POINT('',#70915);
#14338=VERTEX_POINT('',#70916);
#14339=VERTEX_POINT('',#70966);
#14340=VERTEX_POINT('',#70967);
#14341=VERTEX_POINT('',#71014);
#14342=VERTEX_POINT('',#71015);
#14343=VERTEX_POINT('',#71062);
#14344=VERTEX_POINT('',#71063);
#14345=VERTEX_POINT('',#71116);
#14346=VERTEX_POINT('',#71117);
#14347=VERTEX_POINT('',#71164);
#14348=VERTEX_POINT('',#71165);
#14349=VERTEX_POINT('',#71212);
#14350=VERTEX_POINT('',#71213);
#14351=VERTEX_POINT('',#71263);
#14352=VERTEX_POINT('',#71264);
#14353=VERTEX_POINT('',#71311);
#14354=VERTEX_POINT('',#71312);
#14355=VERTEX_POINT('',#71359);
#14356=VERTEX_POINT('',#71360);
#14357=VERTEX_POINT('',#71407);
#14358=VERTEX_POINT('',#71408);
#14359=VERTEX_POINT('',#71461);
#14360=VERTEX_POINT('',#71462);
#14361=VERTEX_POINT('',#71509);
#14362=VERTEX_POINT('',#71510);
#14363=VERTEX_POINT('',#71557);
#14364=VERTEX_POINT('',#71558);
#14365=VERTEX_POINT('',#71611);
#14366=VERTEX_POINT('',#71612);
#14367=VERTEX_POINT('',#71659);
#14368=VERTEX_POINT('',#71660);
#14369=VERTEX_POINT('',#71707);
#14370=VERTEX_POINT('',#71708);
#14371=VERTEX_POINT('',#71755);
#14372=VERTEX_POINT('',#71756);
#14373=VERTEX_POINT('',#71809);
#14374=VERTEX_POINT('',#71810);
#14375=VERTEX_POINT('',#71857);
#14376=VERTEX_POINT('',#71858);
#14377=VERTEX_POINT('',#71905);
#14378=VERTEX_POINT('',#71906);
#14379=VERTEX_POINT('',#71959);
#14380=VERTEX_POINT('',#71960);
#14381=VERTEX_POINT('',#72007);
#14382=VERTEX_POINT('',#72008);
#14383=VERTEX_POINT('',#72055);
#14384=VERTEX_POINT('',#72056);
#14385=VERTEX_POINT('',#72103);
#14386=VERTEX_POINT('',#72104);
#14387=VERTEX_POINT('',#72157);
#14388=VERTEX_POINT('',#72158);
#14389=VERTEX_POINT('',#72205);
#14390=VERTEX_POINT('',#72206);
#14391=VERTEX_POINT('',#72253);
#14392=VERTEX_POINT('',#72254);
#14393=VERTEX_POINT('',#72307);
#14394=VERTEX_POINT('',#72308);
#14395=VERTEX_POINT('',#72355);
#14396=VERTEX_POINT('',#72356);
#14397=VERTEX_POINT('',#72403);
#14398=VERTEX_POINT('',#72404);
#14399=VERTEX_POINT('',#72451);
#14400=VERTEX_POINT('',#72452);
#14401=VERTEX_POINT('',#72505);
#14402=VERTEX_POINT('',#72506);
#14403=VERTEX_POINT('',#72553);
#14404=VERTEX_POINT('',#72554);
#14405=VERTEX_POINT('',#72601);
#14406=VERTEX_POINT('',#72602);
#14407=VERTEX_POINT('',#72655);
#14408=VERTEX_POINT('',#72656);
#14409=VERTEX_POINT('',#72703);
#14410=VERTEX_POINT('',#72704);
#14411=VERTEX_POINT('',#72751);
#14412=VERTEX_POINT('',#72752);
#14413=VERTEX_POINT('',#72799);
#14414=VERTEX_POINT('',#72800);
#14415=VERTEX_POINT('',#72853);
#14416=VERTEX_POINT('',#72854);
#14417=VERTEX_POINT('',#72901);
#14418=VERTEX_POINT('',#72902);
#14419=VERTEX_POINT('',#72949);
#14420=VERTEX_POINT('',#72950);
#14421=VERTEX_POINT('',#73003);
#14422=VERTEX_POINT('',#73004);
#14423=VERTEX_POINT('',#73051);
#14424=VERTEX_POINT('',#73052);
#14425=VERTEX_POINT('',#73099);
#14426=VERTEX_POINT('',#73100);
#14427=VERTEX_POINT('',#73147);
#14428=VERTEX_POINT('',#73148);
#14429=VERTEX_POINT('',#73201);
#14430=VERTEX_POINT('',#73202);
#14431=VERTEX_POINT('',#73249);
#14432=VERTEX_POINT('',#73250);
#14433=VERTEX_POINT('',#73297);
#14434=VERTEX_POINT('',#73298);
#14435=VERTEX_POINT('',#73351);
#14436=VERTEX_POINT('',#73352);
#14437=VERTEX_POINT('',#73399);
#14438=VERTEX_POINT('',#73400);
#14439=VERTEX_POINT('',#73447);
#14440=VERTEX_POINT('',#73448);
#14441=VERTEX_POINT('',#73498);
#14442=VERTEX_POINT('',#73499);
#14443=VERTEX_POINT('',#73549);
#14444=VERTEX_POINT('',#73550);
#14445=VERTEX_POINT('',#73597);
#14446=VERTEX_POINT('',#73598);
#14447=VERTEX_POINT('',#73645);
#14448=VERTEX_POINT('',#73646);
#14449=VERTEX_POINT('',#73699);
#14450=VERTEX_POINT('',#73700);
#14451=VERTEX_POINT('',#73747);
#14452=VERTEX_POINT('',#73748);
#14453=VERTEX_POINT('',#73795);
#14454=VERTEX_POINT('',#73796);
#14455=VERTEX_POINT('',#73846);
#14456=VERTEX_POINT('',#73847);
#14457=VERTEX_POINT('',#73894);
#14458=VERTEX_POINT('',#73895);
#14459=VERTEX_POINT('',#73942);
#14460=VERTEX_POINT('',#73943);
#14461=VERTEX_POINT('',#73990);
#14462=VERTEX_POINT('',#73991);
#14463=VERTEX_POINT('',#74044);
#14464=VERTEX_POINT('',#74045);
#14465=VERTEX_POINT('',#74092);
#14466=VERTEX_POINT('',#74093);
#14467=VERTEX_POINT('',#74095);
#14468=VERTEX_POINT('',#74101);
#14469=VERTEX_POINT('',#74108);
#14470=VERTEX_POINT('',#74109);
#14471=VERTEX_POINT('',#74133);
#14472=VERTEX_POINT('',#74134);
#14473=VERTEX_POINT('',#74158);
#14474=VERTEX_POINT('',#74159);
#14475=VERTEX_POINT('',#74183);
#14476=VERTEX_POINT('',#74184);
#14477=VERTEX_POINT('',#74207);
#14478=VERTEX_POINT('',#74208);
#14479=VERTEX_POINT('',#74231);
#14480=VERTEX_POINT('',#74232);
#14481=VERTEX_POINT('',#74256);
#14482=VERTEX_POINT('',#74257);
#14483=VERTEX_POINT('',#74281);
#14484=VERTEX_POINT('',#74282);
#14485=VERTEX_POINT('',#74305);
#14486=VERTEX_POINT('',#74306);
#14487=VERTEX_POINT('',#74330);
#14488=VERTEX_POINT('',#74331);
#14489=VERTEX_POINT('',#74355);
#14490=VERTEX_POINT('',#74356);
#14491=VERTEX_POINT('',#74379);
#14492=VERTEX_POINT('',#74380);
#14493=VERTEX_POINT('',#74404);
#14494=VERTEX_POINT('',#74405);
#14495=VERTEX_POINT('',#74428);
#14496=VERTEX_POINT('',#74429);
#14497=VERTEX_POINT('',#74453);
#14498=VERTEX_POINT('',#74454);
#14499=VERTEX_POINT('',#74477);
#14500=VERTEX_POINT('',#74478);
#14501=VERTEX_POINT('',#74502);
#14502=VERTEX_POINT('',#74503);
#14503=VERTEX_POINT('',#74527);
#14504=VERTEX_POINT('',#74528);
#14505=VERTEX_POINT('',#74551);
#14506=VERTEX_POINT('',#74552);
#14507=VERTEX_POINT('',#74576);
#14508=VERTEX_POINT('',#74577);
#14509=VERTEX_POINT('',#74601);
#14510=VERTEX_POINT('',#74602);
#14511=VERTEX_POINT('',#74625);
#14512=VERTEX_POINT('',#74626);
#14513=VERTEX_POINT('',#74649);
#14514=VERTEX_POINT('',#74650);
#14515=VERTEX_POINT('',#74674);
#14516=VERTEX_POINT('',#74675);
#14517=VERTEX_POINT('',#74699);
#14518=VERTEX_POINT('',#74700);
#14519=VERTEX_POINT('',#74723);
#14520=VERTEX_POINT('',#74724);
#14521=VERTEX_POINT('',#74748);
#14522=VERTEX_POINT('',#74749);
#14523=VERTEX_POINT('',#74773);
#14524=VERTEX_POINT('',#74774);
#14525=VERTEX_POINT('',#74797);
#14526=VERTEX_POINT('',#74798);
#14527=VERTEX_POINT('',#74821);
#14528=VERTEX_POINT('',#74822);
#14529=VERTEX_POINT('',#74846);
#14530=VERTEX_POINT('',#74847);
#14531=VERTEX_POINT('',#74871);
#14532=VERTEX_POINT('',#74872);
#14533=VERTEX_POINT('',#74895);
#14534=VERTEX_POINT('',#74896);
#14535=VERTEX_POINT('',#74920);
#14536=VERTEX_POINT('',#74921);
#14537=VERTEX_POINT('',#74945);
#14538=VERTEX_POINT('',#74946);
#14539=VERTEX_POINT('',#74969);
#14540=VERTEX_POINT('',#74970);
#14541=VERTEX_POINT('',#74993);
#14542=VERTEX_POINT('',#74994);
#14543=VERTEX_POINT('',#75018);
#14544=VERTEX_POINT('',#75019);
#14545=VERTEX_POINT('',#75043);
#14546=VERTEX_POINT('',#75044);
#14547=VERTEX_POINT('',#75067);
#14548=VERTEX_POINT('',#75068);
#14549=VERTEX_POINT('',#75092);
#14550=VERTEX_POINT('',#75093);
#14551=VERTEX_POINT('',#75117);
#14552=VERTEX_POINT('',#75118);
#14553=VERTEX_POINT('',#75141);
#14554=VERTEX_POINT('',#75142);
#14555=VERTEX_POINT('',#75165);
#14556=VERTEX_POINT('',#75166);
#14557=VERTEX_POINT('',#75190);
#14558=VERTEX_POINT('',#75191);
#14559=VERTEX_POINT('',#75215);
#14560=VERTEX_POINT('',#75216);
#14561=VERTEX_POINT('',#75239);
#14562=VERTEX_POINT('',#75240);
#14563=VERTEX_POINT('',#75264);
#14564=VERTEX_POINT('',#75265);
#14565=VERTEX_POINT('',#75289);
#14566=VERTEX_POINT('',#75290);
#14567=VERTEX_POINT('',#75313);
#14568=VERTEX_POINT('',#75314);
#14569=VERTEX_POINT('',#75337);
#14570=VERTEX_POINT('',#75338);
#14571=VERTEX_POINT('',#75362);
#14572=VERTEX_POINT('',#75363);
#14573=VERTEX_POINT('',#75387);
#14574=VERTEX_POINT('',#75388);
#14575=VERTEX_POINT('',#75411);
#14576=VERTEX_POINT('',#75412);
#14577=VERTEX_POINT('',#75436);
#14578=VERTEX_POINT('',#75437);
#14579=VERTEX_POINT('',#75461);
#14580=VERTEX_POINT('',#75462);
#14581=VERTEX_POINT('',#75485);
#14582=VERTEX_POINT('',#75486);
#14583=VERTEX_POINT('',#75509);
#14584=VERTEX_POINT('',#75510);
#14585=VERTEX_POINT('',#75534);
#14586=VERTEX_POINT('',#75535);
#14587=VERTEX_POINT('',#75559);
#14588=VERTEX_POINT('',#75560);
#14589=VERTEX_POINT('',#75583);
#14590=VERTEX_POINT('',#75584);
#14591=VERTEX_POINT('',#75608);
#14592=VERTEX_POINT('',#75609);
#14593=VERTEX_POINT('',#75633);
#14594=VERTEX_POINT('',#75634);
#14595=VERTEX_POINT('',#75657);
#14596=VERTEX_POINT('',#75658);
#14597=VERTEX_POINT('',#75682);
#14598=VERTEX_POINT('',#75683);
#14599=VERTEX_POINT('',#75706);
#14600=VERTEX_POINT('',#75707);
#14601=VERTEX_POINT('',#75731);
#14602=VERTEX_POINT('',#75732);
#14603=VERTEX_POINT('',#75755);
#14604=VERTEX_POINT('',#75756);
#14605=VERTEX_POINT('',#75780);
#14606=VERTEX_POINT('',#75781);
#14607=VERTEX_POINT('',#75805);
#14608=VERTEX_POINT('',#75806);
#14609=VERTEX_POINT('',#75829);
#14610=VERTEX_POINT('',#75830);
#14611=VERTEX_POINT('',#75854);
#14612=VERTEX_POINT('',#75855);
#14613=VERTEX_POINT('',#75879);
#14614=VERTEX_POINT('',#75880);
#14615=VERTEX_POINT('',#75903);
#14616=VERTEX_POINT('',#75904);
#14617=VERTEX_POINT('',#75927);
#14618=VERTEX_POINT('',#76034);
#14619=VERTEX_POINT('',#76036);
#14620=VERTEX_POINT('',#78075);
#14621=VERTEX_POINT('',#78192);
#14622=VERTEX_POINT('',#78195);
#14623=VERTEX_POINT('',#80245);
#14624=VERTEX_POINT('',#80247);
#14625=VERTEX_POINT('',#80255);
#14626=VERTEX_POINT('',#80260);
#14627=VERTEX_POINT('',#80261);
#14628=VERTEX_POINT('',#80265);
#14629=VERTEX_POINT('',#80267);
#14630=VERTEX_POINT('',#80269);
#14631=VERTEX_POINT('',#80273);
#14632=VERTEX_POINT('',#80277);
#14633=VERTEX_POINT('',#80280);
#14634=VERTEX_POINT('',#80281);
#14635=VERTEX_POINT('',#80285);
#14636=VERTEX_POINT('',#80287);
#14637=VERTEX_POINT('',#80291);
#14638=VERTEX_POINT('',#80293);
#14639=VERTEX_POINT('',#80295);
#14640=VERTEX_POINT('',#80302);
#14641=VERTEX_POINT('',#80311);
#14642=VERTEX_POINT('',#80315);
#14643=VERTEX_POINT('',#80319);
#14644=VERTEX_POINT('',#80321);
#14645=VERTEX_POINT('',#80325);
#14646=VERTEX_POINT('',#80334);
#14647=VERTEX_POINT('',#80336);
#14648=VERTEX_POINT('',#80338);
#14649=VERTEX_POINT('',#80340);
#14650=VERTEX_POINT('',#80342);
#14651=VERTEX_POINT('',#80344);
#14652=VERTEX_POINT('',#80346);
#14653=VERTEX_POINT('',#80348);
#14654=VERTEX_POINT('',#80350);
#14655=VERTEX_POINT('',#80352);
#14656=VERTEX_POINT('',#80354);
#14657=VERTEX_POINT('',#80356);
#14658=VERTEX_POINT('',#80358);
#14659=VERTEX_POINT('',#80360);
#14660=VERTEX_POINT('',#80362);
#14661=VERTEX_POINT('',#80364);
#14662=VERTEX_POINT('',#80366);
#14663=VERTEX_POINT('',#80368);
#14664=VERTEX_POINT('',#80370);
#14665=VERTEX_POINT('',#80372);
#14666=VERTEX_POINT('',#80374);
#14667=VERTEX_POINT('',#80376);
#14668=VERTEX_POINT('',#80378);
#14669=VERTEX_POINT('',#80380);
#14670=VERTEX_POINT('',#80382);
#14671=VERTEX_POINT('',#80384);
#14672=VERTEX_POINT('',#80386);
#14673=VERTEX_POINT('',#80388);
#14674=VERTEX_POINT('',#80390);
#14675=VERTEX_POINT('',#80392);
#14676=VERTEX_POINT('',#80395);
#14677=VERTEX_POINT('',#80397);
#14678=VERTEX_POINT('',#80399);
#14679=VERTEX_POINT('',#80401);
#14680=VERTEX_POINT('',#80403);
#14681=VERTEX_POINT('',#80405);
#14682=VERTEX_POINT('',#80407);
#14683=VERTEX_POINT('',#80409);
#14684=VERTEX_POINT('',#80411);
#14685=VERTEX_POINT('',#80413);
#14686=VERTEX_POINT('',#80415);
#14687=VERTEX_POINT('',#80417);
#14688=VERTEX_POINT('',#80419);
#14689=VERTEX_POINT('',#80421);
#14690=VERTEX_POINT('',#80423);
#14691=VERTEX_POINT('',#80425);
#14692=VERTEX_POINT('',#80427);
#14693=VERTEX_POINT('',#80429);
#14694=VERTEX_POINT('',#80431);
#14695=VERTEX_POINT('',#80433);
#14696=VERTEX_POINT('',#80435);
#14697=VERTEX_POINT('',#80437);
#14698=VERTEX_POINT('',#80439);
#14699=VERTEX_POINT('',#80441);
#14700=VERTEX_POINT('',#80443);
#14701=VERTEX_POINT('',#80445);
#14702=VERTEX_POINT('',#80447);
#14703=VERTEX_POINT('',#80452);
#14704=VERTEX_POINT('',#80456);
#14705=VERTEX_POINT('',#80458);
#14706=VERTEX_POINT('',#80460);
#14707=VERTEX_POINT('',#80474);
#14708=VERTEX_POINT('',#80478);
#14709=VERTEX_POINT('',#80487);
#14710=VERTEX_POINT('',#80491);
#14711=VERTEX_POINT('',#80493);
#14712=VERTEX_POINT('',#80495);
#14713=VERTEX_POINT('',#80509);
#14714=VERTEX_POINT('',#80513);
#14715=VERTEX_POINT('',#80522);
#14716=VERTEX_POINT('',#80526);
#14717=VERTEX_POINT('',#80528);
#14718=VERTEX_POINT('',#80530);
#14719=VERTEX_POINT('',#80544);
#14720=VERTEX_POINT('',#80548);
#14721=VERTEX_POINT('',#80557);
#14722=VERTEX_POINT('',#80561);
#14723=VERTEX_POINT('',#80563);
#14724=VERTEX_POINT('',#80565);
#14725=VERTEX_POINT('',#80579);
#14726=VERTEX_POINT('',#80583);
#14727=VERTEX_POINT('',#80592);
#14728=VERTEX_POINT('',#80596);
#14729=VERTEX_POINT('',#80598);
#14730=VERTEX_POINT('',#80600);
#14731=VERTEX_POINT('',#80614);
#14732=VERTEX_POINT('',#80618);
#14733=VERTEX_POINT('',#80627);
#14734=VERTEX_POINT('',#80631);
#14735=VERTEX_POINT('',#80633);
#14736=VERTEX_POINT('',#80635);
#14737=VERTEX_POINT('',#80649);
#14738=VERTEX_POINT('',#80653);
#14739=VERTEX_POINT('',#80662);
#14740=VERTEX_POINT('',#80666);
#14741=VERTEX_POINT('',#80668);
#14742=VERTEX_POINT('',#80670);
#14743=VERTEX_POINT('',#80684);
#14744=VERTEX_POINT('',#80688);
#14745=VERTEX_POINT('',#80697);
#14746=VERTEX_POINT('',#80701);
#14747=VERTEX_POINT('',#80703);
#14748=VERTEX_POINT('',#80705);
#14749=VERTEX_POINT('',#80719);
#14750=VERTEX_POINT('',#80723);
#14751=VERTEX_POINT('',#80732);
#14752=VERTEX_POINT('',#80736);
#14753=VERTEX_POINT('',#80738);
#14754=VERTEX_POINT('',#80740);
#14755=VERTEX_POINT('',#80754);
#14756=VERTEX_POINT('',#80758);
#14757=VERTEX_POINT('',#80767);
#14758=VERTEX_POINT('',#80771);
#14759=VERTEX_POINT('',#80773);
#14760=VERTEX_POINT('',#80775);
#14761=VERTEX_POINT('',#80789);
#14762=VERTEX_POINT('',#80793);
#14763=VERTEX_POINT('',#80802);
#14764=VERTEX_POINT('',#80806);
#14765=VERTEX_POINT('',#80808);
#14766=VERTEX_POINT('',#80810);
#14767=VERTEX_POINT('',#80824);
#14768=VERTEX_POINT('',#80828);
#14769=VERTEX_POINT('',#80837);
#14770=VERTEX_POINT('',#80841);
#14771=VERTEX_POINT('',#80843);
#14772=VERTEX_POINT('',#80845);
#14773=VERTEX_POINT('',#80859);
#14774=VERTEX_POINT('',#80863);
#14775=VERTEX_POINT('',#80872);
#14776=VERTEX_POINT('',#80876);
#14777=VERTEX_POINT('',#80878);
#14778=VERTEX_POINT('',#80880);
#14779=VERTEX_POINT('',#80894);
#14780=VERTEX_POINT('',#80898);
#14781=VERTEX_POINT('',#80907);
#14782=VERTEX_POINT('',#80911);
#14783=VERTEX_POINT('',#80913);
#14784=VERTEX_POINT('',#80915);
#14785=VERTEX_POINT('',#80929);
#14786=VERTEX_POINT('',#80930);
#14787=VERTEX_POINT('',#80932);
#14788=VERTEX_POINT('',#80934);
#14789=VERTEX_POINT('',#80938);
#14790=VERTEX_POINT('',#80940);
#14791=VERTEX_POINT('',#80944);
#14792=VERTEX_POINT('',#80945);
#14793=VERTEX_POINT('',#80947);
#14794=VERTEX_POINT('',#80949);
#14795=VERTEX_POINT('',#80953);
#14796=VERTEX_POINT('',#80955);
#14797=VERTEX_POINT('',#80965);
#14798=VERTEX_POINT('',#80967);
#14799=VERTEX_POINT('',#80971);
#14800=VERTEX_POINT('',#80975);
#14801=VERTEX_POINT('',#80981);
#14802=VERTEX_POINT('',#80985);
#14803=VERTEX_POINT('',#81008);
#14804=VERTEX_POINT('',#81012);
#14805=VERTEX_POINT('',#81016);
#14806=VERTEX_POINT('',#81023);
#14807=VERTEX_POINT('',#81024);
#14808=VERTEX_POINT('',#81026);
#14809=VERTEX_POINT('',#81037);
#14810=VERTEX_POINT('',#81047);
#14811=VERTEX_POINT('',#81048);
#14812=VERTEX_POINT('',#81095);
#14813=VERTEX_POINT('',#81096);
#14814=VERTEX_POINT('',#81143);
#14815=VERTEX_POINT('',#81144);
#14816=VERTEX_POINT('',#81197);
#14817=VERTEX_POINT('',#81198);
#14818=VERTEX_POINT('',#81245);
#14819=VERTEX_POINT('',#81246);
#14820=VERTEX_POINT('',#81293);
#14821=VERTEX_POINT('',#81294);
#14822=VERTEX_POINT('',#81341);
#14823=VERTEX_POINT('',#81342);
#14824=VERTEX_POINT('',#81344);
#14825=VERTEX_POINT('',#81355);
#14826=VERTEX_POINT('',#81367);
#14827=VERTEX_POINT('',#81368);
#14828=VERTEX_POINT('',#81391);
#14829=VERTEX_POINT('',#81392);
#14830=VERTEX_POINT('',#81415);
#14831=VERTEX_POINT('',#81416);
#14832=VERTEX_POINT('',#81440);
#14833=VERTEX_POINT('',#81441);
#14834=VERTEX_POINT('',#81465);
#14835=VERTEX_POINT('',#81466);
#14836=VERTEX_POINT('',#81489);
#14837=VERTEX_POINT('',#81575);
#14838=VERTEX_POINT('',#81577);
#14839=VERTEX_POINT('',#81865);
#14840=VERTEX_POINT('',#81961);
#14841=VERTEX_POINT('',#81964);
#14842=VERTEX_POINT('',#82259);
#14843=VERTEX_POINT('',#82260);
#14844=VERTEX_POINT('',#82262);
#14845=VERTEX_POINT('',#82264);
#14846=VERTEX_POINT('',#82268);
#14847=VERTEX_POINT('',#82270);
#14848=VERTEX_POINT('',#82274);
#14849=VERTEX_POINT('',#82276);
#14850=VERTEX_POINT('',#82280);
#14851=VERTEX_POINT('',#82282);
#14852=VERTEX_POINT('',#82286);
#14853=VERTEX_POINT('',#82288);
#14854=VERTEX_POINT('',#82296);
#14855=VERTEX_POINT('',#82303);
#14856=EDGE_CURVE('',#11994,#11995,#7382,.T.);
#14857=EDGE_CURVE('',#11995,#11996,#7383,.T.);
#14858=EDGE_CURVE('',#11996,#11997,#7384,.T.);
#14859=EDGE_CURVE('',#11997,#11998,#7385,.T.);
#14860=EDGE_CURVE('',#11998,#11999,#7386,.T.);
#14861=EDGE_CURVE('',#11999,#11994,#7387,.T.);
#14862=EDGE_CURVE('',#12000,#11995,#7388,.T.);
#14863=EDGE_CURVE('',#12001,#12000,#7389,.T.);
#14864=EDGE_CURVE('',#11996,#12001,#7390,.T.);
#14865=EDGE_CURVE('',#12002,#11994,#7391,.T.);
#14866=EDGE_CURVE('',#12002,#12003,#7392,.T.);
#14867=EDGE_CURVE('',#12003,#12004,#7393,.T.);
#14868=EDGE_CURVE('',#12000,#12004,#7394,.T.);
#14869=EDGE_CURVE('',#11999,#12005,#7395,.T.);
#14870=EDGE_CURVE('',#12005,#12006,#7396,.T.);
#14871=EDGE_CURVE('',#12006,#12002,#7397,.T.);
#14872=EDGE_CURVE('',#12004,#12007,#7398,.T.);
#14873=EDGE_CURVE('',#12007,#12008,#7399,.T.);
#14874=EDGE_CURVE('',#12008,#12009,#7400,.T.);
#14875=EDGE_CURVE('',#12009,#12001,#7401,.T.);
#14876=EDGE_CURVE('',#12010,#12009,#7402,.T.);
#14877=EDGE_CURVE('',#12010,#12011,#7403,.T.);
#14878=EDGE_CURVE('',#12011,#11997,#7404,.T.);
#14879=EDGE_CURVE('',#12008,#12012,#7405,.T.);
#14880=EDGE_CURVE('',#12013,#12012,#7406,.T.);
#14881=EDGE_CURVE('',#12014,#12013,#7407,.T.);
#14882=EDGE_CURVE('',#12014,#12010,#7408,.T.);
#14883=EDGE_CURVE('',#12015,#12007,#7409,.T.);
#14884=EDGE_CURVE('',#12012,#12015,#7410,.T.);
#14885=EDGE_CURVE('',#12016,#12017,#7411,.T.);
#14886=EDGE_CURVE('',#12017,#12018,#7412,.T.);
#14887=EDGE_CURVE('',#12018,#12019,#7413,.T.);
#14888=EDGE_CURVE('',#12019,#12020,#7414,.T.);
#14889=EDGE_CURVE('',#12020,#12021,#7415,.T.);
#14890=EDGE_CURVE('',#12021,#12022,#7416,.T.);
#14891=EDGE_CURVE('',#12022,#12023,#7417,.T.);
#14892=EDGE_CURVE('',#12023,#12024,#7418,.T.);
#14893=EDGE_CURVE('',#12024,#12025,#7419,.T.);
#14894=EDGE_CURVE('',#12025,#12026,#7420,.T.);
#14895=EDGE_CURVE('',#12026,#12027,#7421,.T.);
#14896=EDGE_CURVE('',#12027,#12016,#7422,.T.);
#14897=EDGE_CURVE('',#12028,#12029,#7423,.T.);
#14898=EDGE_CURVE('',#12029,#12030,#7424,.T.);
#14899=EDGE_CURVE('',#12030,#12031,#7425,.T.);
#14900=EDGE_CURVE('',#12031,#12032,#7426,.T.);
#14901=EDGE_CURVE('',#12032,#12033,#7427,.T.);
#14902=EDGE_CURVE('',#12033,#12034,#2083,.T.);
#14903=EDGE_CURVE('',#12034,#12035,#2084,.T.);
#14904=EDGE_CURVE('',#12035,#12036,#2085,.T.);
#14905=EDGE_CURVE('',#12036,#12037,#2086,.T.);
#14906=EDGE_CURVE('',#12037,#12038,#2087,.T.);
#14907=EDGE_CURVE('',#12038,#12039,#2088,.T.);
#14908=EDGE_CURVE('',#12039,#12040,#2089,.T.);
#14909=EDGE_CURVE('',#12040,#12041,#7428,.T.);
#14910=EDGE_CURVE('',#12041,#12042,#7429,.T.);
#14911=EDGE_CURVE('',#12042,#12043,#7430,.T.);
#14912=EDGE_CURVE('',#12043,#12044,#2090,.T.);
#14913=EDGE_CURVE('',#12044,#12045,#2091,.T.);
#14914=EDGE_CURVE('',#12045,#12046,#2092,.T.);
#14915=EDGE_CURVE('',#12046,#12028,#2093,.T.);
#14916=EDGE_CURVE('',#12047,#12048,#7431,.T.);
#14917=EDGE_CURVE('',#12048,#12049,#7432,.T.);
#14918=EDGE_CURVE('',#12049,#12050,#7433,.T.);
#14919=EDGE_CURVE('',#12050,#12051,#7434,.T.);
#14920=EDGE_CURVE('',#12051,#12052,#7435,.T.);
#14921=EDGE_CURVE('',#12052,#12053,#7436,.T.);
#14922=EDGE_CURVE('',#12053,#12054,#7437,.T.);
#14923=EDGE_CURVE('',#12054,#12055,#7438,.T.);
#14924=EDGE_CURVE('',#12055,#12056,#7439,.T.);
#14925=EDGE_CURVE('',#12056,#12057,#7440,.T.);
#14926=EDGE_CURVE('',#12057,#12058,#7441,.T.);
#14927=EDGE_CURVE('',#12058,#12047,#7442,.T.);
#14928=EDGE_CURVE('',#12059,#12060,#2094,.T.);
#14929=EDGE_CURVE('',#12060,#12061,#2095,.T.);
#14930=EDGE_CURVE('',#12061,#12062,#7443,.T.);
#14931=EDGE_CURVE('',#12062,#12063,#7444,.T.);
#14932=EDGE_CURVE('',#12063,#12064,#7445,.T.);
#14933=EDGE_CURVE('',#12064,#12065,#7446,.T.);
#14934=EDGE_CURVE('',#12065,#12066,#2096,.T.);
#14935=EDGE_CURVE('',#12066,#12067,#2097,.T.);
#14936=EDGE_CURVE('',#12067,#12068,#2098,.T.);
#14937=EDGE_CURVE('',#12068,#12069,#7447,.T.);
#14938=EDGE_CURVE('',#12069,#12059,#2099,.T.);
#14939=EDGE_CURVE('',#12070,#12071,#2100,.T.);
#14940=EDGE_CURVE('',#12071,#12072,#2101,.T.);
#14941=EDGE_CURVE('',#12072,#12073,#2102,.T.);
#14942=EDGE_CURVE('',#12073,#12074,#7448,.T.);
#14943=EDGE_CURVE('',#12074,#12075,#2103,.T.);
#14944=EDGE_CURVE('',#12075,#12076,#2104,.T.);
#14945=EDGE_CURVE('',#12076,#12077,#2105,.T.);
#14946=EDGE_CURVE('',#12077,#12078,#2106,.T.);
#14947=EDGE_CURVE('',#12078,#12079,#2107,.T.);
#14948=EDGE_CURVE('',#12079,#12080,#2108,.T.);
#14949=EDGE_CURVE('',#12080,#12081,#2109,.T.);
#14950=EDGE_CURVE('',#12081,#12082,#2110,.T.);
#14951=EDGE_CURVE('',#12082,#12083,#2111,.T.);
#14952=EDGE_CURVE('',#12083,#12084,#2112,.T.);
#14953=EDGE_CURVE('',#12084,#12085,#2113,.T.);
#14954=EDGE_CURVE('',#12085,#12086,#2114,.T.);
#14955=EDGE_CURVE('',#12086,#12087,#2115,.T.);
#14956=EDGE_CURVE('',#12087,#12088,#2116,.T.);
#14957=EDGE_CURVE('',#12088,#12089,#2117,.T.);
#14958=EDGE_CURVE('',#12089,#12090,#2118,.T.);
#14959=EDGE_CURVE('',#12090,#12091,#2119,.T.);
#14960=EDGE_CURVE('',#12091,#12092,#2120,.T.);
#14961=EDGE_CURVE('',#12092,#12093,#7449,.T.);
#14962=EDGE_CURVE('',#12093,#12094,#2121,.T.);
#14963=EDGE_CURVE('',#12094,#12095,#2122,.T.);
#14964=EDGE_CURVE('',#12095,#12096,#2123,.T.);
#14965=EDGE_CURVE('',#12096,#12097,#2124,.T.);
#14966=EDGE_CURVE('',#12097,#12098,#2125,.T.);
#14967=EDGE_CURVE('',#12098,#12099,#2126,.T.);
#14968=EDGE_CURVE('',#12099,#12100,#2127,.T.);
#14969=EDGE_CURVE('',#12100,#12101,#2128,.T.);
#14970=EDGE_CURVE('',#12101,#12102,#2129,.T.);
#14971=EDGE_CURVE('',#12102,#12103,#2130,.T.);
#14972=EDGE_CURVE('',#12103,#12104,#2131,.T.);
#14973=EDGE_CURVE('',#12104,#12070,#2132,.T.);
#14974=EDGE_CURVE('',#12105,#12106,#2133,.T.);
#14975=EDGE_CURVE('',#12106,#12107,#2134,.T.);
#14976=EDGE_CURVE('',#12107,#12108,#2135,.T.);
#14977=EDGE_CURVE('',#12108,#12109,#7450,.T.);
#14978=EDGE_CURVE('',#12109,#12110,#2136,.T.);
#14979=EDGE_CURVE('',#12110,#12111,#2137,.T.);
#14980=EDGE_CURVE('',#12111,#12112,#2138,.T.);
#14981=EDGE_CURVE('',#12112,#12113,#2139,.T.);
#14982=EDGE_CURVE('',#12113,#12114,#2140,.T.);
#14983=EDGE_CURVE('',#12114,#12115,#2141,.T.);
#14984=EDGE_CURVE('',#12115,#12116,#2142,.T.);
#14985=EDGE_CURVE('',#12116,#12117,#7451,.T.);
#14986=EDGE_CURVE('',#12117,#12118,#2143,.T.);
#14987=EDGE_CURVE('',#12118,#12119,#2144,.T.);
#14988=EDGE_CURVE('',#12119,#12120,#2145,.T.);
#14989=EDGE_CURVE('',#12120,#12121,#2146,.T.);
#14990=EDGE_CURVE('',#12121,#12122,#2147,.T.);
#14991=EDGE_CURVE('',#12122,#12123,#2148,.T.);
#14992=EDGE_CURVE('',#12123,#12124,#2149,.T.);
#14993=EDGE_CURVE('',#12124,#12125,#7452,.T.);
#14994=EDGE_CURVE('',#12125,#12126,#2150,.T.);
#14995=EDGE_CURVE('',#12126,#12127,#2151,.T.);
#14996=EDGE_CURVE('',#12127,#12128,#2152,.T.);
#14997=EDGE_CURVE('',#12128,#12129,#2153,.T.);
#14998=EDGE_CURVE('',#12129,#12130,#2154,.T.);
#14999=EDGE_CURVE('',#12130,#12131,#2155,.T.);
#15000=EDGE_CURVE('',#12131,#12132,#2156,.T.);
#15001=EDGE_CURVE('',#12132,#12133,#2157,.T.);
#15002=EDGE_CURVE('',#12133,#12134,#2158,.T.);
#15003=EDGE_CURVE('',#12134,#12105,#2159,.T.);
#15004=EDGE_CURVE('',#12135,#12136,#7453,.T.);
#15005=EDGE_CURVE('',#12136,#12137,#7454,.T.);
#15006=EDGE_CURVE('',#12137,#12138,#7455,.T.);
#15007=EDGE_CURVE('',#12138,#12135,#7456,.T.);
#15008=EDGE_CURVE('',#12139,#12140,#2160,.T.);
#15009=EDGE_CURVE('',#12140,#12141,#2161,.T.);
#15010=EDGE_CURVE('',#12141,#12142,#2162,.T.);
#15011=EDGE_CURVE('',#12142,#12143,#7457,.T.);
#15012=EDGE_CURVE('',#12143,#12144,#2163,.T.);
#15013=EDGE_CURVE('',#12144,#12145,#2164,.T.);
#15014=EDGE_CURVE('',#12145,#12146,#2165,.T.);
#15015=EDGE_CURVE('',#12146,#12147,#2166,.T.);
#15016=EDGE_CURVE('',#12147,#12148,#2167,.T.);
#15017=EDGE_CURVE('',#12148,#12149,#2168,.T.);
#15018=EDGE_CURVE('',#12149,#12150,#2169,.T.);
#15019=EDGE_CURVE('',#12150,#12151,#2170,.T.);
#15020=EDGE_CURVE('',#12151,#12152,#2171,.T.);
#15021=EDGE_CURVE('',#12152,#12153,#2172,.T.);
#15022=EDGE_CURVE('',#12153,#12154,#2173,.T.);
#15023=EDGE_CURVE('',#12154,#12155,#2174,.T.);
#15024=EDGE_CURVE('',#12155,#12156,#2175,.T.);
#15025=EDGE_CURVE('',#12156,#12157,#2176,.T.);
#15026=EDGE_CURVE('',#12157,#12158,#2177,.T.);
#15027=EDGE_CURVE('',#12158,#12159,#2178,.T.);
#15028=EDGE_CURVE('',#12159,#12160,#2179,.T.);
#15029=EDGE_CURVE('',#12160,#12161,#2180,.T.);
#15030=EDGE_CURVE('',#12161,#12162,#7458,.T.);
#15031=EDGE_CURVE('',#12162,#12163,#2181,.T.);
#15032=EDGE_CURVE('',#12163,#12164,#2182,.T.);
#15033=EDGE_CURVE('',#12164,#12165,#2183,.T.);
#15034=EDGE_CURVE('',#12165,#12166,#2184,.T.);
#15035=EDGE_CURVE('',#12166,#12167,#2185,.T.);
#15036=EDGE_CURVE('',#12167,#12168,#2186,.T.);
#15037=EDGE_CURVE('',#12168,#12169,#2187,.T.);
#15038=EDGE_CURVE('',#12169,#12170,#2188,.T.);
#15039=EDGE_CURVE('',#12170,#12171,#2189,.T.);
#15040=EDGE_CURVE('',#12171,#12172,#2190,.T.);
#15041=EDGE_CURVE('',#12172,#12173,#2191,.T.);
#15042=EDGE_CURVE('',#12173,#12139,#2192,.T.);
#15043=EDGE_CURVE('',#12174,#12175,#7459,.T.);
#15044=EDGE_CURVE('',#12175,#12176,#7460,.T.);
#15045=EDGE_CURVE('',#12176,#12013,#7461,.T.);
#15046=EDGE_CURVE('',#12015,#12174,#7462,.T.);
#15047=EDGE_CURVE('',#12176,#12177,#7463,.T.);
#15048=EDGE_CURVE('',#12177,#12178,#7464,.T.);
#15049=EDGE_CURVE('',#12178,#12014,#7465,.T.);
#15050=EDGE_CURVE('',#12179,#12179,#1036,.T.);
#15051=EDGE_CURVE('',#12179,#12180,#7466,.T.);
#15052=EDGE_CURVE('',#12180,#12180,#1037,.T.);
#15053=EDGE_CURVE('',#12181,#12182,#7467,.T.);
#15054=EDGE_CURVE('',#12183,#12181,#7468,.T.);
#15055=EDGE_CURVE('',#12177,#12183,#7469,.T.);
#15056=EDGE_CURVE('',#12177,#12182,#7470,.T.);
#15057=EDGE_CURVE('',#12184,#12184,#1038,.T.);
#15058=EDGE_CURVE('',#12180,#12185,#7471,.T.);
#15059=EDGE_CURVE('',#12185,#12185,#1039,.T.);
#15060=EDGE_CURVE('',#12184,#12186,#7472,.T.);
#15061=EDGE_CURVE('',#12186,#12186,#1040,.T.);
#15062=EDGE_CURVE('',#12186,#12187,#7473,.T.);
#15063=EDGE_CURVE('',#12187,#12187,#1041,.T.);
#15064=EDGE_CURVE('',#12188,#12188,#1042,.T.);
#15065=EDGE_CURVE('',#12188,#12189,#7474,.T.);
#15066=EDGE_CURVE('',#12189,#12189,#1043,.T.);
#15067=EDGE_CURVE('',#12188,#12190,#7475,.T.);
#15068=EDGE_CURVE('',#12190,#12190,#1044,.T.);
#15069=EDGE_CURVE('',#12191,#12191,#1045,.T.);
#15070=EDGE_CURVE('',#12192,#12192,#1046,.T.);
#15071=EDGE_CURVE('',#12192,#12193,#7476,.T.);
#15072=EDGE_CURVE('',#12193,#12193,#1047,.T.);
#15073=EDGE_CURVE('',#12192,#12194,#7477,.T.);
#15074=EDGE_CURVE('',#12194,#12194,#1048,.T.);
#15075=EDGE_CURVE('',#12195,#12195,#1049,.T.);
#15076=EDGE_CURVE('',#12196,#12196,#1050,.T.);
#15077=EDGE_CURVE('',#12196,#12197,#7478,.T.);
#15078=EDGE_CURVE('',#12197,#12197,#1051,.T.);
#15079=EDGE_CURVE('',#12196,#12198,#7479,.T.);
#15080=EDGE_CURVE('',#12198,#12198,#1052,.T.);
#15081=EDGE_CURVE('',#12199,#12199,#1053,.T.);
#15082=EDGE_CURVE('',#12200,#12200,#1054,.T.);
#15083=EDGE_CURVE('',#12200,#12201,#7480,.T.);
#15084=EDGE_CURVE('',#12201,#12201,#1055,.T.);
#15085=EDGE_CURVE('',#12200,#12202,#7481,.T.);
#15086=EDGE_CURVE('',#12202,#12202,#1056,.T.);
#15087=EDGE_CURVE('',#12203,#12203,#1057,.T.);
#15088=EDGE_CURVE('',#12003,#12204,#7482,.T.);
#15089=EDGE_CURVE('',#12204,#12174,#7483,.T.);
#15090=EDGE_CURVE('',#12204,#12205,#7484,.T.);
#15091=EDGE_CURVE('',#12205,#12182,#7485,.T.);
#15092=EDGE_CURVE('',#12182,#12175,#7486,.T.);
#15093=EDGE_CURVE('',#12206,#12005,#7487,.T.);
#15094=EDGE_CURVE('',#12006,#12206,#7488,.T.);
#15095=EDGE_CURVE('',#12207,#12208,#7489,.T.);
#15096=EDGE_CURVE('',#12181,#12207,#7490,.T.);
#15097=EDGE_CURVE('',#12208,#12181,#7491,.T.);
#15098=EDGE_CURVE('',#12209,#12210,#7492,.T.);
#15099=EDGE_CURVE('',#12211,#12209,#7493,.T.);
#15100=EDGE_CURVE('',#12210,#12211,#7494,.T.);
#15101=EDGE_CURVE('',#12212,#12183,#7495,.T.);
#15102=EDGE_CURVE('',#12213,#12212,#7496,.T.);
#15103=EDGE_CURVE('',#12183,#12213,#7497,.T.);
#15104=EDGE_CURVE('',#12212,#12210,#7498,.T.);
#15105=EDGE_CURVE('',#12211,#12213,#7499,.T.);
#15106=EDGE_CURVE('',#12213,#12178,#7500,.T.);
#15107=EDGE_CURVE('',#12207,#12212,#7501,.T.);
#15108=EDGE_CURVE('',#12011,#12211,#7502,.T.);
#15109=EDGE_CURVE('',#12209,#11998,#7503,.T.);
#15110=EDGE_CURVE('',#12005,#12209,#7504,.T.);
#15111=EDGE_CURVE('',#12210,#12206,#7505,.T.);
#15112=EDGE_CURVE('',#12205,#12208,#7506,.T.);
#15113=EDGE_CURVE('',#12208,#12006,#7507,.T.);
#15114=EDGE_CURVE('',#12206,#12207,#7508,.T.);
#15115=EDGE_CURVE('',#12214,#12214,#1058,.T.);
#15116=EDGE_CURVE('',#12215,#12215,#1059,.T.);
#15117=EDGE_CURVE('',#12216,#12216,#1060,.T.);
#15118=EDGE_CURVE('',#12217,#12217,#1061,.T.);
#15119=EDGE_CURVE('',#12218,#12218,#1062,.T.);
#15120=EDGE_CURVE('',#12219,#12219,#1063,.T.);
#15121=EDGE_CURVE('',#12220,#12220,#1064,.T.);
#15122=EDGE_CURVE('',#12221,#12221,#1065,.T.);
#15123=EDGE_CURVE('',#12222,#12222,#1066,.T.);
#15124=EDGE_CURVE('',#12223,#12223,#1067,.T.);
#15125=EDGE_CURVE('',#12224,#12224,#1068,.T.);
#15126=EDGE_CURVE('',#12225,#12225,#1069,.T.);
#15127=EDGE_CURVE('',#12226,#12226,#1070,.T.);
#15128=EDGE_CURVE('',#12227,#12227,#1071,.T.);
#15129=EDGE_CURVE('',#12228,#12228,#1072,.T.);
#15130=EDGE_CURVE('',#12229,#12229,#1073,.T.);
#15131=EDGE_CURVE('',#12230,#12230,#1074,.T.);
#15132=EDGE_CURVE('',#12231,#12231,#1075,.T.);
#15133=EDGE_CURVE('',#12232,#12232,#1076,.T.);
#15134=EDGE_CURVE('',#12233,#12233,#1077,.T.);
#15135=EDGE_CURVE('',#12234,#12234,#1078,.T.);
#15136=EDGE_CURVE('',#12235,#12235,#1079,.T.);
#15137=EDGE_CURVE('',#12016,#12236,#7509,.T.);
#15138=EDGE_CURVE('',#12236,#12237,#7510,.T.);
#15139=EDGE_CURVE('',#12017,#12237,#7511,.T.);
#15140=EDGE_CURVE('',#12027,#12238,#7512,.T.);
#15141=EDGE_CURVE('',#12238,#12236,#7513,.T.);
#15142=EDGE_CURVE('',#12026,#12239,#7514,.T.);
#15143=EDGE_CURVE('',#12239,#12238,#7515,.T.);
#15144=EDGE_CURVE('',#12025,#12240,#7516,.T.);
#15145=EDGE_CURVE('',#12240,#12239,#7517,.T.);
#15146=EDGE_CURVE('',#12024,#12241,#7518,.T.);
#15147=EDGE_CURVE('',#12241,#12240,#7519,.T.);
#15148=EDGE_CURVE('',#12023,#12242,#7520,.T.);
#15149=EDGE_CURVE('',#12242,#12241,#7521,.T.);
#15150=EDGE_CURVE('',#12022,#12243,#7522,.T.);
#15151=EDGE_CURVE('',#12243,#12242,#7523,.T.);
#15152=EDGE_CURVE('',#12021,#12244,#7524,.T.);
#15153=EDGE_CURVE('',#12244,#12243,#7525,.T.);
#15154=EDGE_CURVE('',#12020,#12245,#7526,.T.);
#15155=EDGE_CURVE('',#12245,#12244,#7527,.T.);
#15156=EDGE_CURVE('',#12019,#12246,#7528,.T.);
#15157=EDGE_CURVE('',#12246,#12245,#7529,.T.);
#15158=EDGE_CURVE('',#12018,#12247,#7530,.T.);
#15159=EDGE_CURVE('',#12247,#12246,#7531,.T.);
#15160=EDGE_CURVE('',#12237,#12247,#7532,.T.);
#15161=EDGE_CURVE('',#12028,#12248,#7533,.T.);
#15162=EDGE_CURVE('',#12248,#12249,#7534,.T.);
#15163=EDGE_CURVE('',#12029,#12249,#7535,.T.);
#15164=EDGE_CURVE('',#12046,#12250,#7536,.T.);
#15165=EDGE_CURVE('',#12250,#12248,#2193,.T.);
#15166=EDGE_CURVE('',#12045,#12251,#7537,.T.);
#15167=EDGE_CURVE('',#12251,#12250,#2194,.T.);
#15168=EDGE_CURVE('',#12044,#12252,#7538,.T.);
#15169=EDGE_CURVE('',#12252,#12251,#2195,.T.);
#15170=EDGE_CURVE('',#12043,#12253,#7539,.T.);
#15171=EDGE_CURVE('',#12253,#12252,#2196,.T.);
#15172=EDGE_CURVE('',#12042,#12254,#7540,.T.);
#15173=EDGE_CURVE('',#12254,#12253,#7541,.T.);
#15174=EDGE_CURVE('',#12041,#12255,#7542,.T.);
#15175=EDGE_CURVE('',#12255,#12254,#7543,.T.);
#15176=EDGE_CURVE('',#12040,#12256,#7544,.T.);
#15177=EDGE_CURVE('',#12256,#12255,#7545,.T.);
#15178=EDGE_CURVE('',#12039,#12257,#7546,.T.);
#15179=EDGE_CURVE('',#12257,#12256,#2197,.T.);
#15180=EDGE_CURVE('',#12038,#12258,#7547,.T.);
#15181=EDGE_CURVE('',#12258,#12257,#2198,.T.);
#15182=EDGE_CURVE('',#12037,#12259,#7548,.T.);
#15183=EDGE_CURVE('',#12259,#12258,#2199,.T.);
#15184=EDGE_CURVE('',#12036,#12260,#7549,.T.);
#15185=EDGE_CURVE('',#12260,#12259,#2200,.T.);
#15186=EDGE_CURVE('',#12035,#12261,#7550,.T.);
#15187=EDGE_CURVE('',#12261,#12260,#2201,.T.);
#15188=EDGE_CURVE('',#12034,#12262,#7551,.T.);
#15189=EDGE_CURVE('',#12262,#12261,#2202,.T.);
#15190=EDGE_CURVE('',#12033,#12263,#7552,.T.);
#15191=EDGE_CURVE('',#12263,#12262,#2203,.T.);
#15192=EDGE_CURVE('',#12032,#12264,#7553,.T.);
#15193=EDGE_CURVE('',#12264,#12263,#7554,.T.);
#15194=EDGE_CURVE('',#12031,#12265,#7555,.T.);
#15195=EDGE_CURVE('',#12265,#12264,#7556,.T.);
#15196=EDGE_CURVE('',#12030,#12266,#7557,.T.);
#15197=EDGE_CURVE('',#12266,#12265,#7558,.T.);
#15198=EDGE_CURVE('',#12249,#12266,#7559,.T.);
#15199=EDGE_CURVE('',#12047,#12267,#7560,.T.);
#15200=EDGE_CURVE('',#12267,#12268,#7561,.T.);
#15201=EDGE_CURVE('',#12048,#12268,#7562,.T.);
#15202=EDGE_CURVE('',#12058,#12269,#7563,.T.);
#15203=EDGE_CURVE('',#12269,#12267,#7564,.T.);
#15204=EDGE_CURVE('',#12057,#12270,#7565,.T.);
#15205=EDGE_CURVE('',#12270,#12269,#7566,.T.);
#15206=EDGE_CURVE('',#12056,#12271,#7567,.T.);
#15207=EDGE_CURVE('',#12271,#12270,#7568,.T.);
#15208=EDGE_CURVE('',#12055,#12272,#7569,.T.);
#15209=EDGE_CURVE('',#12272,#12271,#7570,.T.);
#15210=EDGE_CURVE('',#12054,#12273,#7571,.T.);
#15211=EDGE_CURVE('',#12273,#12272,#7572,.T.);
#15212=EDGE_CURVE('',#12053,#12274,#7573,.T.);
#15213=EDGE_CURVE('',#12274,#12273,#7574,.T.);
#15214=EDGE_CURVE('',#12052,#12275,#7575,.T.);
#15215=EDGE_CURVE('',#12275,#12274,#7576,.T.);
#15216=EDGE_CURVE('',#12051,#12276,#7577,.T.);
#15217=EDGE_CURVE('',#12276,#12275,#7578,.T.);
#15218=EDGE_CURVE('',#12050,#12277,#7579,.T.);
#15219=EDGE_CURVE('',#12277,#12276,#7580,.T.);
#15220=EDGE_CURVE('',#12049,#12278,#7581,.T.);
#15221=EDGE_CURVE('',#12278,#12277,#7582,.T.);
#15222=EDGE_CURVE('',#12268,#12278,#7583,.T.);
#15223=EDGE_CURVE('',#12059,#12279,#7584,.T.);
#15224=EDGE_CURVE('',#12279,#12280,#2204,.T.);
#15225=EDGE_CURVE('',#12060,#12280,#7585,.T.);
#15226=EDGE_CURVE('',#12069,#12281,#7586,.T.);
#15227=EDGE_CURVE('',#12281,#12279,#2205,.T.);
#15228=EDGE_CURVE('',#12068,#12282,#7587,.T.);
#15229=EDGE_CURVE('',#12282,#12281,#7588,.T.);
#15230=EDGE_CURVE('',#12067,#12283,#7589,.T.);
#15231=EDGE_CURVE('',#12283,#12282,#2206,.T.);
#15232=EDGE_CURVE('',#12066,#12284,#7590,.T.);
#15233=EDGE_CURVE('',#12284,#12283,#2207,.T.);
#15234=EDGE_CURVE('',#12065,#12285,#7591,.T.);
#15235=EDGE_CURVE('',#12285,#12284,#2208,.T.);
#15236=EDGE_CURVE('',#12064,#12286,#7592,.T.);
#15237=EDGE_CURVE('',#12286,#12285,#7593,.T.);
#15238=EDGE_CURVE('',#12063,#12287,#7594,.T.);
#15239=EDGE_CURVE('',#12287,#12286,#7595,.T.);
#15240=EDGE_CURVE('',#12062,#12288,#7596,.T.);
#15241=EDGE_CURVE('',#12288,#12287,#7597,.T.);
#15242=EDGE_CURVE('',#12061,#12289,#7598,.T.);
#15243=EDGE_CURVE('',#12289,#12288,#7599,.T.);
#15244=EDGE_CURVE('',#12280,#12289,#2209,.T.);
#15245=EDGE_CURVE('',#12070,#12290,#7600,.T.);
#15246=EDGE_CURVE('',#12290,#12291,#2210,.T.);
#15247=EDGE_CURVE('',#12071,#12291,#7601,.T.);
#15248=EDGE_CURVE('',#12104,#12292,#7602,.T.);
#15249=EDGE_CURVE('',#12292,#12290,#2211,.T.);
#15250=EDGE_CURVE('',#12103,#12293,#7603,.T.);
#15251=EDGE_CURVE('',#12293,#12292,#2212,.T.);
#15252=EDGE_CURVE('',#12102,#12294,#7604,.T.);
#15253=EDGE_CURVE('',#12294,#12293,#2213,.T.);
#15254=EDGE_CURVE('',#12101,#12295,#7605,.T.);
#15255=EDGE_CURVE('',#12295,#12294,#2214,.T.);
#15256=EDGE_CURVE('',#12100,#12296,#7606,.T.);
#15257=EDGE_CURVE('',#12296,#12295,#2215,.T.);
#15258=EDGE_CURVE('',#12099,#12297,#7607,.T.);
#15259=EDGE_CURVE('',#12297,#12296,#2216,.T.);
#15260=EDGE_CURVE('',#12098,#12298,#7608,.T.);
#15261=EDGE_CURVE('',#12298,#12297,#2217,.T.);
#15262=EDGE_CURVE('',#12097,#12299,#7609,.T.);
#15263=EDGE_CURVE('',#12299,#12298,#2218,.T.);
#15264=EDGE_CURVE('',#12096,#12300,#7610,.T.);
#15265=EDGE_CURVE('',#12300,#12299,#2219,.T.);
#15266=EDGE_CURVE('',#12095,#12301,#7611,.T.);
#15267=EDGE_CURVE('',#12301,#12300,#2220,.T.);
#15268=EDGE_CURVE('',#12094,#12302,#7612,.T.);
#15269=EDGE_CURVE('',#12302,#12301,#2221,.T.);
#15270=EDGE_CURVE('',#12093,#12303,#7613,.T.);
#15271=EDGE_CURVE('',#12303,#12302,#2222,.T.);
#15272=EDGE_CURVE('',#12092,#12304,#7614,.T.);
#15273=EDGE_CURVE('',#12304,#12303,#7615,.T.);
#15274=EDGE_CURVE('',#12091,#12305,#7616,.T.);
#15275=EDGE_CURVE('',#12305,#12304,#2223,.T.);
#15276=EDGE_CURVE('',#12090,#12306,#7617,.T.);
#15277=EDGE_CURVE('',#12306,#12305,#2224,.T.);
#15278=EDGE_CURVE('',#12089,#12307,#7618,.T.);
#15279=EDGE_CURVE('',#12307,#12306,#2225,.T.);
#15280=EDGE_CURVE('',#12088,#12308,#7619,.T.);
#15281=EDGE_CURVE('',#12308,#12307,#2226,.T.);
#15282=EDGE_CURVE('',#12087,#12309,#7620,.T.);
#15283=EDGE_CURVE('',#12309,#12308,#2227,.T.);
#15284=EDGE_CURVE('',#12086,#12310,#7621,.T.);
#15285=EDGE_CURVE('',#12310,#12309,#2228,.T.);
#15286=EDGE_CURVE('',#12085,#12311,#7622,.T.);
#15287=EDGE_CURVE('',#12311,#12310,#2229,.T.);
#15288=EDGE_CURVE('',#12084,#12312,#7623,.T.);
#15289=EDGE_CURVE('',#12312,#12311,#2230,.T.);
#15290=EDGE_CURVE('',#12083,#12313,#7624,.T.);
#15291=EDGE_CURVE('',#12313,#12312,#2231,.T.);
#15292=EDGE_CURVE('',#12082,#12314,#7625,.T.);
#15293=EDGE_CURVE('',#12314,#12313,#2232,.T.);
#15294=EDGE_CURVE('',#12081,#12315,#7626,.T.);
#15295=EDGE_CURVE('',#12315,#12314,#2233,.T.);
#15296=EDGE_CURVE('',#12080,#12316,#7627,.T.);
#15297=EDGE_CURVE('',#12316,#12315,#2234,.T.);
#15298=EDGE_CURVE('',#12079,#12317,#7628,.T.);
#15299=EDGE_CURVE('',#12317,#12316,#2235,.T.);
#15300=EDGE_CURVE('',#12078,#12318,#7629,.T.);
#15301=EDGE_CURVE('',#12318,#12317,#2236,.T.);
#15302=EDGE_CURVE('',#12077,#12319,#7630,.T.);
#15303=EDGE_CURVE('',#12319,#12318,#2237,.T.);
#15304=EDGE_CURVE('',#12076,#12320,#7631,.T.);
#15305=EDGE_CURVE('',#12320,#12319,#2238,.T.);
#15306=EDGE_CURVE('',#12075,#12321,#7632,.T.);
#15307=EDGE_CURVE('',#12321,#12320,#2239,.T.);
#15308=EDGE_CURVE('',#12074,#12322,#7633,.T.);
#15309=EDGE_CURVE('',#12322,#12321,#2240,.T.);
#15310=EDGE_CURVE('',#12073,#12323,#7634,.T.);
#15311=EDGE_CURVE('',#12323,#12322,#7635,.T.);
#15312=EDGE_CURVE('',#12072,#12324,#7636,.T.);
#15313=EDGE_CURVE('',#12324,#12323,#2241,.T.);
#15314=EDGE_CURVE('',#12291,#12324,#2242,.T.);
#15315=EDGE_CURVE('',#12105,#12325,#7637,.T.);
#15316=EDGE_CURVE('',#12325,#12326,#2243,.T.);
#15317=EDGE_CURVE('',#12106,#12326,#7638,.T.);
#15318=EDGE_CURVE('',#12134,#12327,#7639,.T.);
#15319=EDGE_CURVE('',#12327,#12325,#2244,.T.);
#15320=EDGE_CURVE('',#12133,#12328,#7640,.T.);
#15321=EDGE_CURVE('',#12328,#12327,#2245,.T.);
#15322=EDGE_CURVE('',#12132,#12329,#7641,.T.);
#15323=EDGE_CURVE('',#12329,#12328,#2246,.T.);
#15324=EDGE_CURVE('',#12131,#12330,#7642,.T.);
#15325=EDGE_CURVE('',#12330,#12329,#2247,.T.);
#15326=EDGE_CURVE('',#12130,#12331,#7643,.T.);
#15327=EDGE_CURVE('',#12331,#12330,#2248,.T.);
#15328=EDGE_CURVE('',#12129,#12332,#7644,.T.);
#15329=EDGE_CURVE('',#12332,#12331,#2249,.T.);
#15330=EDGE_CURVE('',#12128,#12333,#7645,.T.);
#15331=EDGE_CURVE('',#12333,#12332,#2250,.T.);
#15332=EDGE_CURVE('',#12127,#12334,#7646,.T.);
#15333=EDGE_CURVE('',#12334,#12333,#2251,.T.);
#15334=EDGE_CURVE('',#12126,#12335,#7647,.T.);
#15335=EDGE_CURVE('',#12335,#12334,#2252,.T.);
#15336=EDGE_CURVE('',#12125,#12336,#7648,.T.);
#15337=EDGE_CURVE('',#12336,#12335,#2253,.T.);
#15338=EDGE_CURVE('',#12124,#12337,#7649,.T.);
#15339=EDGE_CURVE('',#12337,#12336,#7650,.T.);
#15340=EDGE_CURVE('',#12123,#12338,#7651,.T.);
#15341=EDGE_CURVE('',#12338,#12337,#2254,.T.);
#15342=EDGE_CURVE('',#12122,#12339,#7652,.T.);
#15343=EDGE_CURVE('',#12339,#12338,#2255,.T.);
#15344=EDGE_CURVE('',#12121,#12340,#7653,.T.);
#15345=EDGE_CURVE('',#12340,#12339,#2256,.T.);
#15346=EDGE_CURVE('',#12120,#12341,#7654,.T.);
#15347=EDGE_CURVE('',#12341,#12340,#2257,.T.);
#15348=EDGE_CURVE('',#12119,#12342,#7655,.T.);
#15349=EDGE_CURVE('',#12342,#12341,#2258,.T.);
#15350=EDGE_CURVE('',#12118,#12343,#7656,.T.);
#15351=EDGE_CURVE('',#12343,#12342,#2259,.T.);
#15352=EDGE_CURVE('',#12117,#12344,#7657,.T.);
#15353=EDGE_CURVE('',#12344,#12343,#2260,.T.);
#15354=EDGE_CURVE('',#12116,#12345,#7658,.T.);
#15355=EDGE_CURVE('',#12345,#12344,#7659,.T.);
#15356=EDGE_CURVE('',#12115,#12346,#7660,.T.);
#15357=EDGE_CURVE('',#12346,#12345,#2261,.T.);
#15358=EDGE_CURVE('',#12114,#12347,#7661,.T.);
#15359=EDGE_CURVE('',#12347,#12346,#2262,.T.);
#15360=EDGE_CURVE('',#12113,#12348,#7662,.T.);
#15361=EDGE_CURVE('',#12348,#12347,#2263,.T.);
#15362=EDGE_CURVE('',#12112,#12349,#7663,.T.);
#15363=EDGE_CURVE('',#12349,#12348,#2264,.T.);
#15364=EDGE_CURVE('',#12111,#12350,#7664,.T.);
#15365=EDGE_CURVE('',#12350,#12349,#2265,.T.);
#15366=EDGE_CURVE('',#12110,#12351,#7665,.T.);
#15367=EDGE_CURVE('',#12351,#12350,#2266,.T.);
#15368=EDGE_CURVE('',#12109,#12352,#7666,.T.);
#15369=EDGE_CURVE('',#12352,#12351,#2267,.T.);
#15370=EDGE_CURVE('',#12108,#12353,#7667,.T.);
#15371=EDGE_CURVE('',#12353,#12352,#7668,.T.);
#15372=EDGE_CURVE('',#12107,#12354,#7669,.T.);
#15373=EDGE_CURVE('',#12354,#12353,#2268,.T.);
#15374=EDGE_CURVE('',#12326,#12354,#2269,.T.);
#15375=EDGE_CURVE('',#12135,#12355,#7670,.T.);
#15376=EDGE_CURVE('',#12355,#12356,#7671,.T.);
#15377=EDGE_CURVE('',#12136,#12356,#7672,.T.);
#15378=EDGE_CURVE('',#12138,#12357,#7673,.T.);
#15379=EDGE_CURVE('',#12357,#12355,#7674,.T.);
#15380=EDGE_CURVE('',#12137,#12358,#7675,.T.);
#15381=EDGE_CURVE('',#12358,#12357,#7676,.T.);
#15382=EDGE_CURVE('',#12356,#12358,#7677,.T.);
#15383=EDGE_CURVE('',#12139,#12359,#7678,.T.);
#15384=EDGE_CURVE('',#12359,#12360,#2270,.T.);
#15385=EDGE_CURVE('',#12140,#12360,#7679,.T.);
#15386=EDGE_CURVE('',#12173,#12361,#7680,.T.);
#15387=EDGE_CURVE('',#12361,#12359,#2271,.T.);
#15388=EDGE_CURVE('',#12172,#12362,#7681,.T.);
#15389=EDGE_CURVE('',#12362,#12361,#2272,.T.);
#15390=EDGE_CURVE('',#12171,#12363,#7682,.T.);
#15391=EDGE_CURVE('',#12363,#12362,#2273,.T.);
#15392=EDGE_CURVE('',#12170,#12364,#7683,.T.);
#15393=EDGE_CURVE('',#12364,#12363,#2274,.T.);
#15394=EDGE_CURVE('',#12169,#12365,#7684,.T.);
#15395=EDGE_CURVE('',#12365,#12364,#2275,.T.);
#15396=EDGE_CURVE('',#12168,#12366,#7685,.T.);
#15397=EDGE_CURVE('',#12366,#12365,#2276,.T.);
#15398=EDGE_CURVE('',#12167,#12367,#7686,.T.);
#15399=EDGE_CURVE('',#12367,#12366,#2277,.T.);
#15400=EDGE_CURVE('',#12166,#12368,#7687,.T.);
#15401=EDGE_CURVE('',#12368,#12367,#2278,.T.);
#15402=EDGE_CURVE('',#12165,#12369,#7688,.T.);
#15403=EDGE_CURVE('',#12369,#12368,#2279,.T.);
#15404=EDGE_CURVE('',#12164,#12370,#7689,.T.);
#15405=EDGE_CURVE('',#12370,#12369,#2280,.T.);
#15406=EDGE_CURVE('',#12163,#12371,#7690,.T.);
#15407=EDGE_CURVE('',#12371,#12370,#2281,.T.);
#15408=EDGE_CURVE('',#12162,#12372,#7691,.T.);
#15409=EDGE_CURVE('',#12372,#12371,#2282,.T.);
#15410=EDGE_CURVE('',#12161,#12373,#7692,.T.);
#15411=EDGE_CURVE('',#12373,#12372,#7693,.T.);
#15412=EDGE_CURVE('',#12160,#12374,#7694,.T.);
#15413=EDGE_CURVE('',#12374,#12373,#2283,.T.);
#15414=EDGE_CURVE('',#12159,#12375,#7695,.T.);
#15415=EDGE_CURVE('',#12375,#12374,#2284,.T.);
#15416=EDGE_CURVE('',#12158,#12376,#7696,.T.);
#15417=EDGE_CURVE('',#12376,#12375,#2285,.T.);
#15418=EDGE_CURVE('',#12157,#12377,#7697,.T.);
#15419=EDGE_CURVE('',#12377,#12376,#2286,.T.);
#15420=EDGE_CURVE('',#12156,#12378,#7698,.T.);
#15421=EDGE_CURVE('',#12378,#12377,#2287,.T.);
#15422=EDGE_CURVE('',#12155,#12379,#7699,.T.);
#15423=EDGE_CURVE('',#12379,#12378,#2288,.T.);
#15424=EDGE_CURVE('',#12154,#12380,#7700,.T.);
#15425=EDGE_CURVE('',#12380,#12379,#2289,.T.);
#15426=EDGE_CURVE('',#12153,#12381,#7701,.T.);
#15427=EDGE_CURVE('',#12381,#12380,#2290,.T.);
#15428=EDGE_CURVE('',#12152,#12382,#7702,.T.);
#15429=EDGE_CURVE('',#12382,#12381,#2291,.T.);
#15430=EDGE_CURVE('',#12151,#12383,#7703,.T.);
#15431=EDGE_CURVE('',#12383,#12382,#2292,.T.);
#15432=EDGE_CURVE('',#12150,#12384,#7704,.T.);
#15433=EDGE_CURVE('',#12384,#12383,#2293,.T.);
#15434=EDGE_CURVE('',#12149,#12385,#7705,.T.);
#15435=EDGE_CURVE('',#12385,#12384,#2294,.T.);
#15436=EDGE_CURVE('',#12148,#12386,#7706,.T.);
#15437=EDGE_CURVE('',#12386,#12385,#2295,.T.);
#15438=EDGE_CURVE('',#12147,#12387,#7707,.T.);
#15439=EDGE_CURVE('',#12387,#12386,#2296,.T.);
#15440=EDGE_CURVE('',#12146,#12388,#7708,.T.);
#15441=EDGE_CURVE('',#12388,#12387,#2297,.T.);
#15442=EDGE_CURVE('',#12145,#12389,#7709,.T.);
#15443=EDGE_CURVE('',#12389,#12388,#2298,.T.);
#15444=EDGE_CURVE('',#12144,#12390,#7710,.T.);
#15445=EDGE_CURVE('',#12390,#12389,#2299,.T.);
#15446=EDGE_CURVE('',#12143,#12391,#7711,.T.);
#15447=EDGE_CURVE('',#12391,#12390,#2300,.T.);
#15448=EDGE_CURVE('',#12142,#12392,#7712,.T.);
#15449=EDGE_CURVE('',#12392,#12391,#7713,.T.);
#15450=EDGE_CURVE('',#12141,#12393,#7714,.T.);
#15451=EDGE_CURVE('',#12393,#12392,#2301,.T.);
#15452=EDGE_CURVE('',#12360,#12393,#2302,.T.);
#15453=EDGE_CURVE('',#12231,#12394,#7715,.T.);
#15454=EDGE_CURVE('',#12394,#12394,#1080,.T.);
#15455=EDGE_CURVE('',#12395,#12395,#1081,.T.);
#15456=EDGE_CURVE('',#12395,#12394,#7716,.T.);
#15457=EDGE_CURVE('',#12214,#12396,#7717,.T.);
#15458=EDGE_CURVE('',#12396,#12396,#1082,.T.);
#15459=EDGE_CURVE('',#12396,#12397,#7718,.T.);
#15460=EDGE_CURVE('',#12397,#12397,#1083,.T.);
#15461=EDGE_CURVE('',#12230,#12398,#7719,.T.);
#15462=EDGE_CURVE('',#12398,#12398,#1084,.T.);
#15463=EDGE_CURVE('',#12398,#12399,#7720,.T.);
#15464=EDGE_CURVE('',#12399,#12399,#1085,.T.);
#15465=EDGE_CURVE('',#12215,#12400,#7721,.T.);
#15466=EDGE_CURVE('',#12400,#12400,#1086,.T.);
#15467=EDGE_CURVE('',#12400,#12401,#7722,.T.);
#15468=EDGE_CURVE('',#12401,#12401,#1087,.T.);
#15469=EDGE_CURVE('',#12229,#12402,#7723,.T.);
#15470=EDGE_CURVE('',#12402,#12402,#1088,.T.);
#15471=EDGE_CURVE('',#12402,#12403,#7724,.T.);
#15472=EDGE_CURVE('',#12403,#12403,#1089,.T.);
#15473=EDGE_CURVE('',#12216,#12404,#7725,.T.);
#15474=EDGE_CURVE('',#12404,#12404,#1090,.T.);
#15475=EDGE_CURVE('',#12404,#12405,#7726,.T.);
#15476=EDGE_CURVE('',#12405,#12405,#1091,.T.);
#15477=EDGE_CURVE('',#12228,#12406,#7727,.T.);
#15478=EDGE_CURVE('',#12406,#12406,#1092,.T.);
#15479=EDGE_CURVE('',#12406,#12407,#7728,.T.);
#15480=EDGE_CURVE('',#12407,#12407,#1093,.T.);
#15481=EDGE_CURVE('',#12217,#12408,#7729,.T.);
#15482=EDGE_CURVE('',#12408,#12408,#1094,.T.);
#15483=EDGE_CURVE('',#12408,#12409,#7730,.T.);
#15484=EDGE_CURVE('',#12409,#12409,#1095,.T.);
#15485=EDGE_CURVE('',#12227,#12410,#7731,.T.);
#15486=EDGE_CURVE('',#12410,#12410,#1096,.T.);
#15487=EDGE_CURVE('',#12410,#12411,#7732,.T.);
#15488=EDGE_CURVE('',#12411,#12411,#1097,.T.);
#15489=EDGE_CURVE('',#12218,#12412,#7733,.T.);
#15490=EDGE_CURVE('',#12412,#12412,#1098,.T.);
#15491=EDGE_CURVE('',#12412,#12413,#7734,.T.);
#15492=EDGE_CURVE('',#12413,#12413,#1099,.T.);
#15493=EDGE_CURVE('',#12226,#12414,#7735,.T.);
#15494=EDGE_CURVE('',#12414,#12414,#1100,.T.);
#15495=EDGE_CURVE('',#12414,#12415,#7736,.T.);
#15496=EDGE_CURVE('',#12415,#12415,#1101,.T.);
#15497=EDGE_CURVE('',#12219,#12416,#7737,.T.);
#15498=EDGE_CURVE('',#12416,#12416,#1102,.T.);
#15499=EDGE_CURVE('',#12416,#12417,#7738,.T.);
#15500=EDGE_CURVE('',#12417,#12417,#1103,.T.);
#15501=EDGE_CURVE('',#12225,#12418,#7739,.T.);
#15502=EDGE_CURVE('',#12418,#12418,#1104,.T.);
#15503=EDGE_CURVE('',#12418,#12419,#7740,.T.);
#15504=EDGE_CURVE('',#12419,#12419,#1105,.T.);
#15505=EDGE_CURVE('',#12220,#12420,#7741,.T.);
#15506=EDGE_CURVE('',#12420,#12420,#1106,.T.);
#15507=EDGE_CURVE('',#12420,#12203,#7742,.T.);
#15508=EDGE_CURVE('',#12224,#12421,#7743,.T.);
#15509=EDGE_CURVE('',#12421,#12421,#1107,.T.);
#15510=EDGE_CURVE('',#12421,#12199,#7744,.T.);
#15511=EDGE_CURVE('',#12221,#12422,#7745,.T.);
#15512=EDGE_CURVE('',#12422,#12422,#1108,.T.);
#15513=EDGE_CURVE('',#12422,#12195,#7746,.T.);
#15514=EDGE_CURVE('',#12223,#12423,#7747,.T.);
#15515=EDGE_CURVE('',#12423,#12423,#1109,.T.);
#15516=EDGE_CURVE('',#12423,#12191,#7748,.T.);
#15517=EDGE_CURVE('',#12235,#12202,#7749,.T.);
#15518=EDGE_CURVE('',#12232,#12198,#7750,.T.);
#15519=EDGE_CURVE('',#12234,#12194,#7751,.T.);
#15520=EDGE_CURVE('',#12233,#12190,#7752,.T.);
#15521=EDGE_CURVE('',#12222,#12424,#7753,.T.);
#15522=EDGE_CURVE('',#12424,#12424,#1110,.T.);
#15523=EDGE_CURVE('',#12425,#12425,#1111,.T.);
#15524=EDGE_CURVE('',#12425,#12426,#7754,.T.);
#15525=EDGE_CURVE('',#12426,#12426,#1112,.T.);
#15526=EDGE_CURVE('',#12427,#12428,#7755,.T.);
#15527=EDGE_CURVE('',#12429,#12427,#7756,.T.);
#15528=EDGE_CURVE('',#12430,#12429,#1113,.T.);
#15529=EDGE_CURVE('',#12431,#12430,#7757,.T.);
#15530=EDGE_CURVE('',#12432,#12431,#1114,.T.);
#15531=EDGE_CURVE('',#12433,#12432,#7758,.T.);
#15532=EDGE_CURVE('',#12434,#12433,#1115,.T.);
#15533=EDGE_CURVE('',#12435,#12434,#7759,.T.);
#15534=EDGE_CURVE('',#12436,#12435,#1116,.T.);
#15535=EDGE_CURVE('',#12437,#12436,#7760,.T.);
#15536=EDGE_CURVE('',#12438,#12437,#1117,.T.);
#15537=EDGE_CURVE('',#12439,#12438,#7761,.T.);
#15538=EDGE_CURVE('',#12440,#12439,#1118,.T.);
#15539=EDGE_CURVE('',#12441,#12440,#7762,.T.);
#15540=EDGE_CURVE('',#12442,#12441,#1119,.T.);
#15541=EDGE_CURVE('',#12443,#12442,#7763,.T.);
#15542=EDGE_CURVE('',#12444,#12443,#1120,.T.);
#15543=EDGE_CURVE('',#12445,#12444,#7764,.T.);
#15544=EDGE_CURVE('',#12446,#12445,#1121,.T.);
#15545=EDGE_CURVE('',#12447,#12446,#7765,.T.);
#15546=EDGE_CURVE('',#12448,#12447,#1122,.T.);
#15547=EDGE_CURVE('',#12449,#12448,#7766,.T.);
#15548=EDGE_CURVE('',#12450,#12449,#1123,.T.);
#15549=EDGE_CURVE('',#12451,#12450,#7767,.T.);
#15550=EDGE_CURVE('',#12428,#12451,#1124,.T.);
#15551=EDGE_CURVE('',#12452,#12452,#1125,.T.);
#15552=EDGE_CURVE('',#12453,#12453,#1126,.T.);
#15553=EDGE_CURVE('',#12454,#12454,#1127,.T.);
#15554=EDGE_CURVE('',#12455,#12455,#1128,.T.);
#15555=EDGE_CURVE('',#12456,#12456,#1129,.T.);
#15556=EDGE_CURVE('',#12457,#12457,#1130,.T.);
#15557=EDGE_CURVE('',#12458,#12458,#1131,.T.);
#15558=EDGE_CURVE('',#12459,#12459,#1132,.T.);
#15559=EDGE_CURVE('',#12460,#12460,#1133,.T.);
#15560=EDGE_CURVE('',#12426,#12461,#7768,.T.);
#15561=EDGE_CURVE('',#12461,#12461,#1134,.T.);
#15562=EDGE_CURVE('',#12452,#12462,#7769,.T.);
#15563=EDGE_CURVE('',#12462,#12462,#1135,.T.);
#15564=EDGE_CURVE('',#12462,#12463,#7770,.T.);
#15565=EDGE_CURVE('',#12463,#12463,#1136,.T.);
#15566=EDGE_CURVE('',#12427,#12464,#7771,.F.);
#15567=EDGE_CURVE('',#12464,#12465,#7772,.T.);
#15568=EDGE_CURVE('',#12465,#12429,#7773,.T.);
#15569=EDGE_CURVE('',#12465,#12466,#1137,.T.);
#15570=EDGE_CURVE('',#12466,#12430,#7774,.T.);
#15571=EDGE_CURVE('',#12467,#12431,#7775,.T.);
#15572=EDGE_CURVE('',#12466,#12467,#7776,.T.);
#15573=EDGE_CURVE('',#12467,#12468,#1138,.T.);
#15574=EDGE_CURVE('',#12468,#12432,#7777,.T.);
#15575=EDGE_CURVE('',#12469,#12433,#162,.T.);
#15576=EDGE_CURVE('',#12468,#12470,#7778,.T.);
#15577=EDGE_CURVE('',#12470,#12469,#7779,.T.);
#15578=EDGE_CURVE('',#12471,#12469,#163,.T.);
#15579=EDGE_CURVE('',#12471,#12472,#1139,.T.);
#15580=EDGE_CURVE('',#12473,#12472,#164,.T.);
#15581=EDGE_CURVE('',#12434,#12473,#2303,.T.);
#15582=EDGE_CURVE('',#12470,#12474,#7780,.T.);
#15583=EDGE_CURVE('',#12474,#12475,#7781,.T.);
#15584=EDGE_CURVE('',#12475,#12471,#7782,.T.);
#15585=EDGE_CURVE('',#12475,#12476,#165,.F.);
#15586=EDGE_CURVE('',#12476,#12474,#7783,.T.);
#15587=EDGE_CURVE('',#12477,#12478,#7784,.F.);
#15588=EDGE_CURVE('',#12478,#12479,#7785,.T.);
#15589=EDGE_CURVE('',#12479,#12480,#7786,.T.);
#15590=EDGE_CURVE('',#12480,#12477,#7787,.T.);
#15591=EDGE_CURVE('',#12481,#12482,#7788,.T.);
#15592=EDGE_CURVE('',#12482,#12480,#1140,.T.);
#15593=EDGE_CURVE('',#12479,#12481,#1141,.T.);
#15594=EDGE_CURVE('',#12483,#12484,#7789,.T.);
#15595=EDGE_CURVE('',#12484,#12482,#7790,.T.);
#15596=EDGE_CURVE('',#12481,#12483,#7791,.T.);
#15597=EDGE_CURVE('',#12485,#12486,#7792,.T.);
#15598=EDGE_CURVE('',#12486,#12484,#1142,.T.);
#15599=EDGE_CURVE('',#12483,#12485,#1143,.T.);
#15600=EDGE_CURVE('',#12485,#12476,#7793,.T.);
#15601=EDGE_CURVE('',#12474,#12486,#7794,.T.);
#15602=EDGE_CURVE('',#12487,#12488,#166,.T.);
#15603=EDGE_CURVE('',#12488,#12475,#1144,.T.);
#15604=EDGE_CURVE('',#12476,#12489,#1145,.T.);
#15605=EDGE_CURVE('',#12489,#12487,#167,.T.);
#15606=EDGE_CURVE('',#12482,#12466,#7795,.T.);
#15607=EDGE_CURVE('',#12467,#12484,#7796,.T.);
#15608=EDGE_CURVE('',#12486,#12468,#7797,.T.);
#15609=EDGE_CURVE('',#12472,#12488,#7798,.T.);
#15610=EDGE_CURVE('',#12490,#12487,#7799,.T.);
#15611=EDGE_CURVE('',#12490,#12491,#7800,.T.);
#15612=EDGE_CURVE('',#12491,#12473,#7801,.T.);
#15613=EDGE_CURVE('',#12489,#12492,#7802,.T.);
#15614=EDGE_CURVE('',#12492,#12493,#7803,.T.);
#15615=EDGE_CURVE('',#12493,#12490,#7804,.T.);
#15616=EDGE_CURVE('',#12494,#12494,#1146,.T.);
#15617=EDGE_CURVE('',#12494,#12495,#7805,.T.);
#15618=EDGE_CURVE('',#12495,#12495,#1147,.T.);
#15619=EDGE_CURVE('',#12478,#12496,#7806,.T.);
#15620=EDGE_CURVE('',#12497,#12496,#1148,.F.);
#15621=EDGE_CURVE('',#12497,#12498,#7807,.T.);
#15622=EDGE_CURVE('',#12499,#12498,#1149,.T.);
#15623=EDGE_CURVE('',#12500,#12499,#7808,.T.);
#15624=EDGE_CURVE('',#12501,#12500,#1150,.T.);
#15625=EDGE_CURVE('',#12502,#12501,#7809,.T.);
#15626=EDGE_CURVE('',#12503,#12502,#1151,.T.);
#15627=EDGE_CURVE('',#12504,#12503,#7810,.T.);
#15628=EDGE_CURVE('',#12505,#12504,#1152,.T.);
#15629=EDGE_CURVE('',#12506,#12505,#7811,.T.);
#15630=EDGE_CURVE('',#12507,#12506,#1153,.T.);
#15631=EDGE_CURVE('',#12508,#12507,#7812,.T.);
#15632=EDGE_CURVE('',#12492,#12508,#1154,.T.);
#15633=EDGE_CURVE('',#12509,#12509,#1155,.T.);
#15634=EDGE_CURVE('',#12510,#12510,#1156,.T.);
#15635=EDGE_CURVE('',#12511,#12511,#1157,.T.);
#15636=EDGE_CURVE('',#12512,#12512,#1158,.T.);
#15637=EDGE_CURVE('',#12512,#12495,#7813,.T.);
#15638=EDGE_CURVE('',#12509,#12513,#7814,.T.);
#15639=EDGE_CURVE('',#12513,#12513,#1159,.T.);
#15640=EDGE_CURVE('',#12514,#12514,#1160,.T.);
#15641=EDGE_CURVE('',#12514,#12513,#7815,.T.);
#15642=EDGE_CURVE('',#12511,#12515,#7816,.T.);
#15643=EDGE_CURVE('',#12515,#12515,#1161,.T.);
#15644=EDGE_CURVE('',#12516,#12516,#1162,.T.);
#15645=EDGE_CURVE('',#12516,#12515,#7817,.T.);
#15646=EDGE_CURVE('',#12508,#12517,#7818,.T.);
#15647=EDGE_CURVE('',#12517,#12493,#1163,.T.);
#15648=EDGE_CURVE('',#12507,#12518,#7819,.T.);
#15649=EDGE_CURVE('',#12518,#12517,#7820,.T.);
#15650=EDGE_CURVE('',#12506,#12519,#7821,.T.);
#15651=EDGE_CURVE('',#12519,#12518,#1164,.T.);
#15652=EDGE_CURVE('',#12505,#12520,#7822,.T.);
#15653=EDGE_CURVE('',#12520,#12519,#7823,.T.);
#15654=EDGE_CURVE('',#12504,#12521,#7824,.T.);
#15655=EDGE_CURVE('',#12521,#12520,#1165,.T.);
#15656=EDGE_CURVE('',#12503,#12522,#7825,.T.);
#15657=EDGE_CURVE('',#12522,#12521,#7826,.T.);
#15658=EDGE_CURVE('',#12502,#12523,#7827,.T.);
#15659=EDGE_CURVE('',#12523,#12522,#1166,.T.);
#15660=EDGE_CURVE('',#12501,#12524,#7828,.T.);
#15661=EDGE_CURVE('',#12524,#12523,#7829,.T.);
#15662=EDGE_CURVE('',#12500,#12525,#7830,.T.);
#15663=EDGE_CURVE('',#12525,#12524,#1167,.T.);
#15664=EDGE_CURVE('',#12499,#12526,#7831,.T.);
#15665=EDGE_CURVE('',#12526,#12525,#7832,.T.);
#15666=EDGE_CURVE('',#12498,#12527,#168,.F.);
#15667=EDGE_CURVE('',#12527,#12526,#1168,.T.);
#15668=EDGE_CURVE('',#12491,#12528,#7833,.T.);
#15669=EDGE_CURVE('',#12528,#12435,#7834,.T.);
#15670=EDGE_CURVE('',#12529,#12530,#7835,.T.);
#15671=EDGE_CURVE('',#12530,#12531,#7836,.T.);
#15672=EDGE_CURVE('',#12531,#12532,#7837,.T.);
#15673=EDGE_CURVE('',#12532,#12529,#7838,.T.);
#15674=EDGE_CURVE('',#12533,#12534,#7839,.T.);
#15675=EDGE_CURVE('',#12534,#12530,#1169,.T.);
#15676=EDGE_CURVE('',#12529,#12533,#1170,.T.);
#15677=EDGE_CURVE('',#12535,#12536,#7840,.T.);
#15678=EDGE_CURVE('',#12536,#12534,#7841,.T.);
#15679=EDGE_CURVE('',#12533,#12535,#7842,.T.);
#15680=EDGE_CURVE('',#12537,#12538,#7843,.T.);
#15681=EDGE_CURVE('',#12538,#12536,#1171,.T.);
#15682=EDGE_CURVE('',#12535,#12537,#1172,.T.);
#15683=EDGE_CURVE('',#12539,#12540,#7844,.T.);
#15684=EDGE_CURVE('',#12540,#12538,#7845,.T.);
#15685=EDGE_CURVE('',#12537,#12539,#7846,.T.);
#15686=EDGE_CURVE('',#12541,#12542,#7847,.T.);
#15687=EDGE_CURVE('',#12542,#12540,#1173,.T.);
#15688=EDGE_CURVE('',#12539,#12541,#1174,.T.);
#15689=EDGE_CURVE('',#12543,#12544,#7848,.T.);
#15690=EDGE_CURVE('',#12544,#12542,#7849,.T.);
#15691=EDGE_CURVE('',#12541,#12543,#7850,.T.);
#15692=EDGE_CURVE('',#12531,#12544,#1175,.T.);
#15693=EDGE_CURVE('',#12543,#12532,#1176,.T.);
#15694=EDGE_CURVE('',#12542,#12545,#7851,.T.);
#15695=EDGE_CURVE('',#12546,#12545,#1177,.T.);
#15696=EDGE_CURVE('',#12546,#12540,#7852,.T.);
#15697=EDGE_CURVE('',#12547,#12544,#7853,.T.);
#15698=EDGE_CURVE('',#12545,#12547,#7854,.T.);
#15699=EDGE_CURVE('',#12531,#12548,#7855,.T.);
#15700=EDGE_CURVE('',#12548,#12549,#2304,.T.);
#15701=EDGE_CURVE('',#12549,#12550,#7856,.T.);
#15702=EDGE_CURVE('',#12547,#12550,#1178,.T.);
#15703=EDGE_CURVE('',#12496,#12530,#7857,.T.);
#15704=EDGE_CURVE('',#12477,#12464,#7858,.T.);
#15705=EDGE_CURVE('',#12550,#12464,#7859,.T.);
#15706=EDGE_CURVE('',#12549,#12551,#1179,.T.);
#15707=EDGE_CURVE('',#12551,#12548,#1180,.T.);
#15708=EDGE_CURVE('',#12552,#12552,#1181,.T.);
#15709=EDGE_CURVE('',#12528,#12553,#1182,.T.);
#15710=EDGE_CURVE('',#12553,#12436,#7860,.T.);
#15711=EDGE_CURVE('',#12554,#12437,#7861,.T.);
#15712=EDGE_CURVE('',#12553,#12554,#7862,.T.);
#15713=EDGE_CURVE('',#12554,#12555,#1183,.T.);
#15714=EDGE_CURVE('',#12555,#12438,#7863,.T.);
#15715=EDGE_CURVE('',#12556,#12439,#7864,.T.);
#15716=EDGE_CURVE('',#12555,#12556,#7865,.T.);
#15717=EDGE_CURVE('',#12556,#12557,#1184,.T.);
#15718=EDGE_CURVE('',#12557,#12440,#7866,.T.);
#15719=EDGE_CURVE('',#12558,#12441,#7867,.T.);
#15720=EDGE_CURVE('',#12557,#12558,#7868,.T.);
#15721=EDGE_CURVE('',#12558,#12559,#1185,.T.);
#15722=EDGE_CURVE('',#12559,#12442,#7869,.T.);
#15723=EDGE_CURVE('',#12560,#12443,#7870,.T.);
#15724=EDGE_CURVE('',#12559,#12560,#7871,.T.);
#15725=EDGE_CURVE('',#12560,#12561,#1186,.T.);
#15726=EDGE_CURVE('',#12561,#12444,#7872,.T.);
#15727=EDGE_CURVE('',#12562,#12445,#7873,.T.);
#15728=EDGE_CURVE('',#12561,#12562,#7874,.T.);
#15729=EDGE_CURVE('',#12562,#12563,#1187,.T.);
#15730=EDGE_CURVE('',#12563,#12446,#7875,.T.);
#15731=EDGE_CURVE('',#12564,#12447,#7876,.T.);
#15732=EDGE_CURVE('',#12563,#12564,#7877,.T.);
#15733=EDGE_CURVE('',#12564,#12565,#1188,.T.);
#15734=EDGE_CURVE('',#12565,#12448,#7878,.T.);
#15735=EDGE_CURVE('',#12546,#12449,#7879,.T.);
#15736=EDGE_CURVE('',#12565,#12546,#7880,.T.);
#15737=EDGE_CURVE('',#12545,#12450,#7881,.T.);
#15738=EDGE_CURVE('',#12547,#12451,#7882,.T.);
#15739=EDGE_CURVE('',#12550,#12428,#7883,.T.);
#15740=EDGE_CURVE('',#12538,#12565,#7884,.T.);
#15741=EDGE_CURVE('',#12564,#12536,#7885,.T.);
#15742=EDGE_CURVE('',#12527,#12563,#7886,.T.);
#15743=EDGE_CURVE('',#12534,#12497,#7887,.T.);
#15744=EDGE_CURVE('',#12562,#12526,#7888,.T.);
#15745=EDGE_CURVE('',#12525,#12561,#7889,.T.);
#15746=EDGE_CURVE('',#12560,#12524,#7890,.T.);
#15747=EDGE_CURVE('',#12523,#12559,#7891,.T.);
#15748=EDGE_CURVE('',#12558,#12522,#7892,.T.);
#15749=EDGE_CURVE('',#12521,#12557,#7893,.T.);
#15750=EDGE_CURVE('',#12556,#12520,#7894,.T.);
#15751=EDGE_CURVE('',#12519,#12555,#7895,.T.);
#15752=EDGE_CURVE('',#12554,#12518,#7896,.T.);
#15753=EDGE_CURVE('',#12517,#12553,#7897,.T.);
#15754=EDGE_CURVE('',#12528,#12493,#7898,.T.);
#15755=EDGE_CURVE('',#12453,#12516,#7899,.T.);
#15756=EDGE_CURVE('',#12460,#12514,#7900,.T.);
#15757=EDGE_CURVE('',#12454,#12512,#7901,.T.);
#15758=EDGE_CURVE('',#12459,#12566,#7902,.T.);
#15759=EDGE_CURVE('',#12566,#12566,#1189,.T.);
#15760=EDGE_CURVE('',#12566,#12510,#7903,.T.);
#15761=EDGE_CURVE('',#12455,#12567,#7904,.T.);
#15762=EDGE_CURVE('',#12568,#12567,#2305,.T.);
#15763=EDGE_CURVE('',#12569,#12568,#2306,.T.);
#15764=EDGE_CURVE('',#12567,#12569,#2307,.T.);
#15765=EDGE_CURVE('',#12570,#12571,#2308,.T.);
#15766=EDGE_CURVE('',#12571,#12570,#2309,.T.);
#15767=EDGE_CURVE('',#12571,#12572,#7905,.T.);
#15768=EDGE_CURVE('',#12572,#12572,#1190,.T.);
#15769=EDGE_CURVE('',#12551,#12568,#7906,.T.);
#15770=EDGE_CURVE('',#12567,#12573,#7907,.T.);
#15771=EDGE_CURVE('',#12573,#12573,#1191,.T.);
#15772=EDGE_CURVE('',#12552,#12574,#7908,.T.);
#15773=EDGE_CURVE('',#12574,#12574,#1192,.T.);
#15774=EDGE_CURVE('',#12458,#12575,#7909,.T.);
#15775=EDGE_CURVE('',#12575,#12575,#1193,.T.);
#15776=EDGE_CURVE('',#12457,#12576,#7910,.T.);
#15777=EDGE_CURVE('',#12576,#12576,#1194,.T.);
#15778=EDGE_CURVE('',#12456,#12577,#7911,.T.);
#15779=EDGE_CURVE('',#12577,#12577,#1195,.T.);
#15780=EDGE_CURVE('',#12465,#12480,#7912,.T.);
#15781=EDGE_CURVE('',#12578,#12578,#1196,.T.);
#15782=EDGE_CURVE('',#12578,#12579,#7913,.T.);
#15783=EDGE_CURVE('',#12579,#12579,#1197,.T.);
#15784=EDGE_CURVE('',#12578,#12580,#7914,.T.);
#15785=EDGE_CURVE('',#12580,#12580,#1198,.T.);
#15786=EDGE_CURVE('',#12581,#12581,#1199,.T.);
#15787=EDGE_CURVE('',#12582,#12582,#1200,.T.);
#15788=EDGE_CURVE('',#12582,#12583,#7915,.T.);
#15789=EDGE_CURVE('',#12583,#12583,#1201,.T.);
#15790=EDGE_CURVE('',#12582,#12584,#7916,.T.);
#15791=EDGE_CURVE('',#12584,#12584,#1202,.T.);
#15792=EDGE_CURVE('',#12585,#12585,#1203,.T.);
#15793=EDGE_CURVE('',#12586,#12586,#1204,.T.);
#15794=EDGE_CURVE('',#12586,#12587,#7917,.T.);
#15795=EDGE_CURVE('',#12587,#12587,#1205,.T.);
#15796=EDGE_CURVE('',#12586,#12588,#7918,.T.);
#15797=EDGE_CURVE('',#12588,#12588,#1206,.T.);
#15798=EDGE_CURVE('',#12589,#12589,#1207,.T.);
#15799=EDGE_CURVE('',#12590,#12590,#1208,.T.);
#15800=EDGE_CURVE('',#12590,#12591,#7919,.T.);
#15801=EDGE_CURVE('',#12591,#12591,#1209,.T.);
#15802=EDGE_CURVE('',#12590,#12592,#7920,.T.);
#15803=EDGE_CURVE('',#12592,#12592,#1210,.T.);
#15804=EDGE_CURVE('',#12593,#12593,#1211,.T.);
#15805=EDGE_CURVE('',#12594,#12594,#1212,.T.);
#15806=EDGE_CURVE('',#12594,#12595,#7921,.T.);
#15807=EDGE_CURVE('',#12595,#12595,#1213,.T.);
#15808=EDGE_CURVE('',#12594,#12596,#7922,.T.);
#15809=EDGE_CURVE('',#12596,#12596,#1214,.T.);
#15810=EDGE_CURVE('',#12597,#12597,#1215,.T.);
#15811=EDGE_CURVE('',#12598,#12598,#1216,.T.);
#15812=EDGE_CURVE('',#12598,#12599,#7923,.T.);
#15813=EDGE_CURVE('',#12599,#12599,#1217,.T.);
#15814=EDGE_CURVE('',#12598,#12600,#7924,.T.);
#15815=EDGE_CURVE('',#12600,#12600,#1218,.T.);
#15816=EDGE_CURVE('',#12601,#12601,#1219,.T.);
#15817=EDGE_CURVE('',#12602,#12602,#1220,.T.);
#15818=EDGE_CURVE('',#12602,#12603,#7925,.T.);
#15819=EDGE_CURVE('',#12603,#12603,#1221,.T.);
#15820=EDGE_CURVE('',#12602,#12604,#7926,.T.);
#15821=EDGE_CURVE('',#12604,#12604,#1222,.T.);
#15822=EDGE_CURVE('',#12605,#12605,#1223,.T.);
#15823=EDGE_CURVE('',#12606,#12606,#1224,.T.);
#15824=EDGE_CURVE('',#12606,#12607,#7927,.T.);
#15825=EDGE_CURVE('',#12607,#12607,#1225,.T.);
#15826=EDGE_CURVE('',#12606,#12608,#7928,.T.);
#15827=EDGE_CURVE('',#12608,#12608,#1226,.T.);
#15828=EDGE_CURVE('',#12609,#12609,#1227,.T.);
#15829=EDGE_CURVE('',#12610,#12610,#1228,.T.);
#15830=EDGE_CURVE('',#12610,#12611,#7929,.T.);
#15831=EDGE_CURVE('',#12611,#12611,#1229,.T.);
#15832=EDGE_CURVE('',#12612,#12612,#1230,.T.);
#15833=EDGE_CURVE('',#12612,#12610,#7930,.T.);
#15834=EDGE_CURVE('',#12613,#12613,#1231,.T.);
#15835=EDGE_CURVE('',#12614,#12615,#7931,.T.);
#15836=EDGE_CURVE('',#12615,#12616,#7932,.T.);
#15837=EDGE_CURVE('',#12616,#12617,#7933,.T.);
#15838=EDGE_CURVE('',#12617,#12618,#7934,.T.);
#15839=EDGE_CURVE('',#12618,#12619,#7935,.T.);
#15840=EDGE_CURVE('',#12619,#12614,#7936,.T.);
#15841=EDGE_CURVE('',#12619,#12620,#7937,.T.);
#15842=EDGE_CURVE('',#12621,#12620,#7938,.T.);
#15843=EDGE_CURVE('',#12622,#12621,#7939,.T.);
#15844=EDGE_CURVE('',#12622,#12623,#7940,.T.);
#15845=EDGE_CURVE('',#12623,#12614,#7941,.T.);
#15846=EDGE_CURVE('',#12624,#12618,#7942,.T.);
#15847=EDGE_CURVE('',#12620,#12624,#7943,.T.);
#15848=EDGE_CURVE('',#12625,#12617,#7944,.T.);
#15849=EDGE_CURVE('',#12625,#12626,#7945,.T.);
#15850=EDGE_CURVE('',#12626,#12627,#7946,.T.);
#15851=EDGE_CURVE('',#12624,#12627,#7947,.T.);
#15852=EDGE_CURVE('',#12628,#12628,#1232,.T.);
#15853=EDGE_CURVE('',#12628,#12629,#7948,.T.);
#15854=EDGE_CURVE('',#12629,#12629,#1233,.T.);
#15855=EDGE_CURVE('',#12628,#12630,#7949,.T.);
#15856=EDGE_CURVE('',#12630,#12630,#1234,.T.);
#15857=EDGE_CURVE('',#12631,#12631,#1235,.T.);
#15858=EDGE_CURVE('',#12632,#12632,#1236,.T.);
#15859=EDGE_CURVE('',#12632,#12633,#7950,.T.);
#15860=EDGE_CURVE('',#12633,#12633,#1237,.T.);
#15861=EDGE_CURVE('',#12632,#12634,#7951,.T.);
#15862=EDGE_CURVE('',#12634,#12634,#1238,.T.);
#15863=EDGE_CURVE('',#12635,#12635,#1239,.T.);
#15864=EDGE_CURVE('',#12636,#12637,#7952,.T.);
#15865=EDGE_CURVE('',#12637,#12638,#7953,.T.);
#15866=EDGE_CURVE('',#12638,#12639,#7954,.T.);
#15867=EDGE_CURVE('',#12639,#12640,#7955,.T.);
#15868=EDGE_CURVE('',#12640,#12641,#7956,.T.);
#15869=EDGE_CURVE('',#12641,#12636,#7957,.T.);
#15870=EDGE_CURVE('',#12638,#12642,#7958,.T.);
#15871=EDGE_CURVE('',#12643,#12642,#7959,.T.);
#15872=EDGE_CURVE('',#12643,#12644,#7960,.T.);
#15873=EDGE_CURVE('',#12644,#12645,#7961,.T.);
#15874=EDGE_CURVE('',#12645,#12639,#7962,.T.);
#15875=EDGE_CURVE('',#12646,#12637,#7963,.T.);
#15876=EDGE_CURVE('',#12642,#12646,#7964,.T.);
#15877=EDGE_CURVE('',#12647,#12636,#7965,.T.);
#15878=EDGE_CURVE('',#12647,#12648,#7966,.T.);
#15879=EDGE_CURVE('',#12648,#12649,#7967,.T.);
#15880=EDGE_CURVE('',#12646,#12649,#7968,.T.);
#15881=EDGE_CURVE('',#12627,#12650,#7969,.T.);
#15882=EDGE_CURVE('',#12650,#12651,#7970,.T.);
#15883=EDGE_CURVE('',#12651,#12621,#7971,.T.);
#15884=EDGE_CURVE('',#12649,#12652,#7972,.T.);
#15885=EDGE_CURVE('',#12652,#12653,#7973,.T.);
#15886=EDGE_CURVE('',#12653,#12643,#7974,.T.);
#15887=EDGE_CURVE('',#12654,#12654,#1240,.T.);
#15888=EDGE_CURVE('',#12654,#12655,#7975,.T.);
#15889=EDGE_CURVE('',#12655,#12655,#1241,.T.);
#15890=EDGE_CURVE('',#12654,#12656,#7976,.T.);
#15891=EDGE_CURVE('',#12656,#12656,#1242,.T.);
#15892=EDGE_CURVE('',#12657,#12657,#1243,.T.);
#15893=EDGE_CURVE('',#12658,#12658,#1244,.T.);
#15894=EDGE_CURVE('',#12658,#12659,#7977,.T.);
#15895=EDGE_CURVE('',#12659,#12659,#1245,.T.);
#15896=EDGE_CURVE('',#12658,#12660,#7978,.T.);
#15897=EDGE_CURVE('',#12660,#12660,#1246,.T.);
#15898=EDGE_CURVE('',#12661,#12661,#1247,.T.);
#15899=EDGE_CURVE('',#12662,#12662,#1248,.T.);
#15900=EDGE_CURVE('',#12662,#12604,#7979,.T.);
#15901=EDGE_CURVE('',#12626,#12644,#7980,.T.);
#15902=EDGE_CURVE('',#12645,#12625,#7981,.T.);
#15903=EDGE_CURVE('',#12663,#12663,#1249,.T.);
#15904=EDGE_CURVE('',#12664,#12664,#1250,.T.);
#15905=EDGE_CURVE('',#12665,#12665,#1251,.T.);
#15906=EDGE_CURVE('',#12666,#12666,#1252,.T.);
#15907=EDGE_CURVE('',#12667,#12667,#1253,.T.);
#15908=EDGE_CURVE('',#12668,#12668,#1254,.T.);
#15909=EDGE_CURVE('',#12669,#12669,#1255,.T.);
#15910=EDGE_CURVE('',#12670,#12670,#1256,.T.);
#15911=EDGE_CURVE('',#12671,#12671,#1257,.T.);
#15912=EDGE_CURVE('',#12672,#12672,#1258,.T.);
#15913=EDGE_CURVE('',#12673,#12673,#1259,.T.);
#15914=EDGE_CURVE('',#12674,#12674,#1260,.T.);
#15915=EDGE_CURVE('',#12675,#12675,#1261,.T.);
#15916=EDGE_CURVE('',#12676,#12676,#1262,.T.);
#15917=EDGE_CURVE('',#12677,#12677,#1263,.T.);
#15918=EDGE_CURVE('',#12678,#12678,#1264,.T.);
#15919=EDGE_CURVE('',#12679,#12679,#1265,.T.);
#15920=EDGE_CURVE('',#12680,#12680,#1266,.T.);
#15921=EDGE_CURVE('',#12681,#12681,#1267,.T.);
#15922=EDGE_CURVE('',#12682,#12682,#1268,.T.);
#15923=EDGE_CURVE('',#12683,#12683,#1269,.T.);
#15924=EDGE_CURVE('',#12684,#12684,#1270,.T.);
#15925=EDGE_CURVE('',#12685,#12685,#1271,.T.);
#15926=EDGE_CURVE('',#12686,#12686,#1272,.T.);
#15927=EDGE_CURVE('',#12687,#12687,#1273,.T.);
#15928=EDGE_CURVE('',#12688,#12688,#1274,.T.);
#15929=EDGE_CURVE('',#12689,#12689,#1275,.T.);
#15930=EDGE_CURVE('',#12690,#12690,#1276,.T.);
#15931=EDGE_CURVE('',#12691,#12691,#1277,.T.);
#15932=EDGE_CURVE('',#12692,#12692,#1278,.T.);
#15933=EDGE_CURVE('',#12693,#12693,#1279,.T.);
#15934=EDGE_CURVE('',#12694,#12694,#1280,.T.);
#15935=EDGE_CURVE('',#12695,#12695,#1281,.T.);
#15936=EDGE_CURVE('',#12696,#12696,#1282,.T.);
#15937=EDGE_CURVE('',#12697,#12697,#1283,.T.);
#15938=EDGE_CURVE('',#12698,#12698,#1284,.T.);
#15939=EDGE_CURVE('',#12699,#12699,#1285,.T.);
#15940=EDGE_CURVE('',#12700,#12700,#1286,.T.);
#15941=EDGE_CURVE('',#12701,#12701,#1287,.T.);
#15942=EDGE_CURVE('',#12702,#12702,#1288,.T.);
#15943=EDGE_CURVE('',#12703,#12703,#1289,.T.);
#15944=EDGE_CURVE('',#12663,#12600,#7982,.T.);
#15945=EDGE_CURVE('',#12703,#12596,#7983,.T.);
#15946=EDGE_CURVE('',#12664,#12592,#7984,.T.);
#15947=EDGE_CURVE('',#12702,#12588,#7985,.T.);
#15948=EDGE_CURVE('',#12665,#12584,#7986,.T.);
#15949=EDGE_CURVE('',#12701,#12580,#7987,.T.);
#15950=EDGE_CURVE('',#12666,#12608,#7988,.T.);
#15951=EDGE_CURVE('',#12700,#12704,#7989,.T.);
#15952=EDGE_CURVE('',#12704,#12704,#1290,.T.);
#15953=EDGE_CURVE('',#12705,#12705,#1291,.T.);
#15954=EDGE_CURVE('',#12705,#12704,#7990,.T.);
#15955=EDGE_CURVE('',#12667,#12706,#7991,.T.);
#15956=EDGE_CURVE('',#12706,#12706,#1292,.T.);
#15957=EDGE_CURVE('',#12707,#12707,#1293,.T.);
#15958=EDGE_CURVE('',#12707,#12706,#7992,.T.);
#15959=EDGE_CURVE('',#12699,#12660,#7993,.T.);
#15960=EDGE_CURVE('',#12668,#12656,#7994,.T.);
#15961=EDGE_CURVE('',#12653,#12650,#7995,.T.);
#15962=EDGE_CURVE('',#12616,#12640,#7996,.T.);
#15963=EDGE_CURVE('',#12651,#12652,#7997,.T.);
#15964=EDGE_CURVE('',#12669,#12708,#7998,.T.);
#15965=EDGE_CURVE('',#12708,#12708,#1294,.T.);
#15966=EDGE_CURVE('',#12709,#12709,#1295,.T.);
#15967=EDGE_CURVE('',#12709,#12708,#7999,.T.);
#15968=EDGE_CURVE('',#12698,#12710,#8000,.T.);
#15969=EDGE_CURVE('',#12710,#12710,#1296,.T.);
#15970=EDGE_CURVE('',#12711,#12711,#1297,.T.);
#15971=EDGE_CURVE('',#12711,#12710,#8001,.T.);
#15972=EDGE_CURVE('',#12670,#12712,#8002,.T.);
#15973=EDGE_CURVE('',#12712,#12712,#1298,.T.);
#15974=EDGE_CURVE('',#12713,#12713,#1299,.T.);
#15975=EDGE_CURVE('',#12713,#12712,#8003,.T.);
#15976=EDGE_CURVE('',#12697,#12714,#8004,.T.);
#15977=EDGE_CURVE('',#12714,#12714,#1300,.T.);
#15978=EDGE_CURVE('',#12715,#12715,#1301,.T.);
#15979=EDGE_CURVE('',#12715,#12714,#8005,.T.);
#15980=EDGE_CURVE('',#12671,#12716,#8006,.T.);
#15981=EDGE_CURVE('',#12716,#12716,#1302,.T.);
#15982=EDGE_CURVE('',#12717,#12717,#1303,.T.);
#15983=EDGE_CURVE('',#12717,#12716,#8007,.T.);
#15984=EDGE_CURVE('',#12696,#12718,#8008,.T.);
#15985=EDGE_CURVE('',#12718,#12718,#1304,.T.);
#15986=EDGE_CURVE('',#12719,#12719,#1305,.T.);
#15987=EDGE_CURVE('',#12719,#12718,#8009,.T.);
#15988=EDGE_CURVE('',#12672,#12720,#8010,.T.);
#15989=EDGE_CURVE('',#12720,#12720,#1306,.T.);
#15990=EDGE_CURVE('',#12721,#12721,#1307,.T.);
#15991=EDGE_CURVE('',#12721,#12720,#8011,.T.);
#15992=EDGE_CURVE('',#12695,#12722,#8012,.T.);
#15993=EDGE_CURVE('',#12722,#12722,#1308,.T.);
#15994=EDGE_CURVE('',#12723,#12723,#1309,.T.);
#15995=EDGE_CURVE('',#12723,#12722,#8013,.T.);
#15996=EDGE_CURVE('',#12673,#12724,#8014,.T.);
#15997=EDGE_CURVE('',#12724,#12724,#1310,.T.);
#15998=EDGE_CURVE('',#12725,#12725,#1311,.T.);
#15999=EDGE_CURVE('',#12725,#12724,#8015,.T.);
#16000=EDGE_CURVE('',#12694,#12726,#8016,.T.);
#16001=EDGE_CURVE('',#12726,#12726,#1312,.T.);
#16002=EDGE_CURVE('',#12727,#12727,#1313,.T.);
#16003=EDGE_CURVE('',#12727,#12726,#8017,.T.);
#16004=EDGE_CURVE('',#12674,#12728,#8018,.T.);
#16005=EDGE_CURVE('',#12728,#12728,#1314,.T.);
#16006=EDGE_CURVE('',#12729,#12729,#1315,.T.);
#16007=EDGE_CURVE('',#12729,#12728,#8019,.T.);
#16008=EDGE_CURVE('',#12693,#12730,#8020,.T.);
#16009=EDGE_CURVE('',#12730,#12730,#1316,.T.);
#16010=EDGE_CURVE('',#12731,#12731,#1317,.T.);
#16011=EDGE_CURVE('',#12731,#12730,#8021,.T.);
#16012=EDGE_CURVE('',#12675,#12634,#8022,.T.);
#16013=EDGE_CURVE('',#12692,#12630,#8023,.T.);
#16014=EDGE_CURVE('',#12676,#12732,#8024,.T.);
#16015=EDGE_CURVE('',#12732,#12732,#1318,.T.);
#16016=EDGE_CURVE('',#12733,#12733,#1319,.T.);
#16017=EDGE_CURVE('',#12733,#12732,#8025,.T.);
#16018=EDGE_CURVE('',#12691,#12734,#8026,.T.);
#16019=EDGE_CURVE('',#12734,#12734,#1320,.T.);
#16020=EDGE_CURVE('',#12735,#12735,#1321,.T.);
#16021=EDGE_CURVE('',#12735,#12734,#8027,.T.);
#16022=EDGE_CURVE('',#12677,#12736,#8028,.T.);
#16023=EDGE_CURVE('',#12736,#12736,#1322,.T.);
#16024=EDGE_CURVE('',#12737,#12737,#1323,.T.);
#16025=EDGE_CURVE('',#12737,#12736,#8029,.T.);
#16026=EDGE_CURVE('',#12690,#12738,#8030,.T.);
#16027=EDGE_CURVE('',#12738,#12738,#1324,.T.);
#16028=EDGE_CURVE('',#12739,#12739,#1325,.T.);
#16029=EDGE_CURVE('',#12739,#12738,#8031,.T.);
#16030=EDGE_CURVE('',#12678,#12740,#8032,.T.);
#16031=EDGE_CURVE('',#12740,#12740,#1326,.T.);
#16032=EDGE_CURVE('',#12741,#12741,#1327,.T.);
#16033=EDGE_CURVE('',#12741,#12740,#8033,.T.);
#16034=EDGE_CURVE('',#12689,#12742,#8034,.T.);
#16035=EDGE_CURVE('',#12742,#12742,#1328,.T.);
#16036=EDGE_CURVE('',#12743,#12743,#1329,.T.);
#16037=EDGE_CURVE('',#12743,#12742,#8035,.T.);
#16038=EDGE_CURVE('',#12679,#12744,#8036,.T.);
#16039=EDGE_CURVE('',#12744,#12744,#1330,.T.);
#16040=EDGE_CURVE('',#12745,#12745,#1331,.T.);
#16041=EDGE_CURVE('',#12745,#12744,#8037,.T.);
#16042=EDGE_CURVE('',#12688,#12746,#8038,.T.);
#16043=EDGE_CURVE('',#12746,#12746,#1332,.T.);
#16044=EDGE_CURVE('',#12747,#12747,#1333,.T.);
#16045=EDGE_CURVE('',#12747,#12746,#8039,.T.);
#16046=EDGE_CURVE('',#12680,#12748,#8040,.T.);
#16047=EDGE_CURVE('',#12748,#12748,#1334,.T.);
#16048=EDGE_CURVE('',#12749,#12749,#1335,.T.);
#16049=EDGE_CURVE('',#12749,#12748,#8041,.T.);
#16050=EDGE_CURVE('',#12687,#12750,#8042,.T.);
#16051=EDGE_CURVE('',#12750,#12750,#1336,.T.);
#16052=EDGE_CURVE('',#12751,#12751,#1337,.T.);
#16053=EDGE_CURVE('',#12751,#12750,#8043,.T.);
#16054=EDGE_CURVE('',#12681,#12752,#8044,.T.);
#16055=EDGE_CURVE('',#12752,#12752,#1338,.T.);
#16056=EDGE_CURVE('',#12753,#12753,#1339,.T.);
#16057=EDGE_CURVE('',#12753,#12752,#8045,.T.);
#16058=EDGE_CURVE('',#12686,#12754,#8046,.T.);
#16059=EDGE_CURVE('',#12754,#12754,#1340,.T.);
#16060=EDGE_CURVE('',#12755,#12755,#1341,.T.);
#16061=EDGE_CURVE('',#12755,#12754,#8047,.T.);
#16062=EDGE_CURVE('',#12682,#12756,#8048,.T.);
#16063=EDGE_CURVE('',#12756,#12756,#1342,.T.);
#16064=EDGE_CURVE('',#12757,#12757,#1343,.T.);
#16065=EDGE_CURVE('',#12757,#12756,#8049,.T.);
#16066=EDGE_CURVE('',#12685,#12758,#8050,.T.);
#16067=EDGE_CURVE('',#12758,#12758,#1344,.T.);
#16068=EDGE_CURVE('',#12759,#12759,#1345,.T.);
#16069=EDGE_CURVE('',#12759,#12758,#8051,.T.);
#16070=EDGE_CURVE('',#12683,#12760,#8052,.T.);
#16071=EDGE_CURVE('',#12760,#12760,#1346,.T.);
#16072=EDGE_CURVE('',#12761,#12761,#1347,.T.);
#16073=EDGE_CURVE('',#12761,#12760,#8053,.T.);
#16074=EDGE_CURVE('',#12623,#12647,#8054,.T.);
#16075=EDGE_CURVE('',#12641,#12615,#8055,.T.);
#16076=EDGE_CURVE('',#12648,#12622,#8056,.T.);
#16077=EDGE_CURVE('',#12762,#12762,#1348,.T.);
#16078=EDGE_CURVE('',#12763,#12763,#1349,.T.);
#16079=EDGE_CURVE('',#12764,#12764,#1350,.T.);
#16080=EDGE_CURVE('',#12765,#12765,#1351,.T.);
#16081=EDGE_CURVE('',#12766,#12766,#1352,.T.);
#16082=EDGE_CURVE('',#12767,#12767,#1353,.T.);
#16083=EDGE_CURVE('',#12768,#12768,#1354,.T.);
#16084=EDGE_CURVE('',#12769,#12769,#1355,.T.);
#16085=EDGE_CURVE('',#12770,#12770,#1356,.T.);
#16086=EDGE_CURVE('',#12771,#12771,#1357,.T.);
#16087=EDGE_CURVE('',#12772,#12772,#1358,.T.);
#16088=EDGE_CURVE('',#12773,#12773,#1359,.T.);
#16089=EDGE_CURVE('',#12774,#12774,#1360,.T.);
#16090=EDGE_CURVE('',#12775,#12775,#1361,.T.);
#16091=EDGE_CURVE('',#12776,#12776,#1362,.T.);
#16092=EDGE_CURVE('',#12777,#12777,#1363,.T.);
#16093=EDGE_CURVE('',#12778,#12778,#1364,.T.);
#16094=EDGE_CURVE('',#12779,#12779,#1365,.T.);
#16095=EDGE_CURVE('',#12780,#12780,#1366,.T.);
#16096=EDGE_CURVE('',#12781,#12781,#1367,.T.);
#16097=EDGE_CURVE('',#12782,#12782,#1368,.T.);
#16098=EDGE_CURVE('',#12783,#12783,#1369,.T.);
#16099=EDGE_CURVE('',#12784,#12784,#1370,.T.);
#16100=EDGE_CURVE('',#12785,#12785,#1371,.T.);
#16101=EDGE_CURVE('',#12786,#12786,#1372,.T.);
#16102=EDGE_CURVE('',#12787,#12787,#1373,.T.);
#16103=EDGE_CURVE('',#12788,#12788,#1374,.T.);
#16104=EDGE_CURVE('',#12789,#12789,#1375,.T.);
#16105=EDGE_CURVE('',#12790,#12790,#1376,.T.);
#16106=EDGE_CURVE('',#12791,#12791,#1377,.T.);
#16107=EDGE_CURVE('',#12792,#12792,#1378,.T.);
#16108=EDGE_CURVE('',#12793,#12793,#1379,.T.);
#16109=EDGE_CURVE('',#12794,#12794,#1380,.T.);
#16110=EDGE_CURVE('',#12795,#12795,#1381,.T.);
#16111=EDGE_CURVE('',#12796,#12796,#1382,.T.);
#16112=EDGE_CURVE('',#12797,#12797,#1383,.T.);
#16113=EDGE_CURVE('',#12798,#12798,#1384,.T.);
#16114=EDGE_CURVE('',#12799,#12799,#1385,.T.);
#16115=EDGE_CURVE('',#12800,#12800,#1386,.T.);
#16116=EDGE_CURVE('',#12801,#12801,#1387,.T.);
#16117=EDGE_CURVE('',#12802,#12802,#1388,.T.);
#16118=EDGE_CURVE('',#12803,#12803,#1389,.T.);
#16119=EDGE_CURVE('',#12762,#12612,#8057,.T.);
#16120=EDGE_CURVE('',#12803,#12761,#8058,.T.);
#16121=EDGE_CURVE('',#12763,#12759,#8059,.T.);
#16122=EDGE_CURVE('',#12802,#12757,#8060,.T.);
#16123=EDGE_CURVE('',#12764,#12755,#8061,.T.);
#16124=EDGE_CURVE('',#12801,#12753,#8062,.T.);
#16125=EDGE_CURVE('',#12765,#12751,#8063,.T.);
#16126=EDGE_CURVE('',#12800,#12749,#8064,.T.);
#16127=EDGE_CURVE('',#12766,#12804,#8065,.T.);
#16128=EDGE_CURVE('',#12804,#12804,#1390,.T.);
#16129=EDGE_CURVE('',#12804,#12657,#8066,.T.);
#16130=EDGE_CURVE('',#12799,#12805,#8067,.T.);
#16131=EDGE_CURVE('',#12805,#12805,#1391,.T.);
#16132=EDGE_CURVE('',#12805,#12661,#8068,.T.);
#16133=EDGE_CURVE('',#12767,#12806,#8069,.T.);
#16134=EDGE_CURVE('',#12806,#12806,#1392,.T.);
#16135=EDGE_CURVE('',#12806,#12605,#8070,.T.);
#16136=EDGE_CURVE('',#12798,#12807,#8071,.T.);
#16137=EDGE_CURVE('',#12807,#12807,#1393,.T.);
#16138=EDGE_CURVE('',#12807,#12601,#8072,.T.);
#16139=EDGE_CURVE('',#12768,#12808,#8073,.T.);
#16140=EDGE_CURVE('',#12808,#12808,#1394,.T.);
#16141=EDGE_CURVE('',#12808,#12597,#8074,.T.);
#16142=EDGE_CURVE('',#12797,#12809,#8075,.T.);
#16143=EDGE_CURVE('',#12809,#12809,#1395,.T.);
#16144=EDGE_CURVE('',#12809,#12593,#8076,.T.);
#16145=EDGE_CURVE('',#12769,#12810,#8077,.T.);
#16146=EDGE_CURVE('',#12810,#12810,#1396,.T.);
#16147=EDGE_CURVE('',#12810,#12589,#8078,.T.);
#16148=EDGE_CURVE('',#12796,#12811,#8079,.T.);
#16149=EDGE_CURVE('',#12811,#12811,#1397,.T.);
#16150=EDGE_CURVE('',#12811,#12585,#8080,.T.);
#16151=EDGE_CURVE('',#12770,#12812,#8081,.T.);
#16152=EDGE_CURVE('',#12812,#12812,#1398,.T.);
#16153=EDGE_CURVE('',#12812,#12581,#8082,.T.);
#16154=EDGE_CURVE('',#12795,#12813,#8083,.T.);
#16155=EDGE_CURVE('',#12813,#12813,#1399,.T.);
#16156=EDGE_CURVE('',#12813,#12609,#8084,.T.);
#16157=EDGE_CURVE('',#12771,#12747,#8085,.T.);
#16158=EDGE_CURVE('',#12794,#12745,#8086,.T.);
#16159=EDGE_CURVE('',#12772,#12743,#8087,.T.);
#16160=EDGE_CURVE('',#12793,#12741,#8088,.T.);
#16161=EDGE_CURVE('',#12773,#12739,#8089,.T.);
#16162=EDGE_CURVE('',#12792,#12737,#8090,.T.);
#16163=EDGE_CURVE('',#12774,#12735,#8091,.T.);
#16164=EDGE_CURVE('',#12791,#12733,#8092,.T.);
#16165=EDGE_CURVE('',#12775,#12709,#8093,.T.);
#16166=EDGE_CURVE('',#12790,#12711,#8094,.T.);
#16167=EDGE_CURVE('',#12776,#12713,#8095,.T.);
#16168=EDGE_CURVE('',#12789,#12715,#8096,.T.);
#16169=EDGE_CURVE('',#12777,#12717,#8097,.T.);
#16170=EDGE_CURVE('',#12788,#12719,#8098,.T.);
#16171=EDGE_CURVE('',#12778,#12721,#8099,.T.);
#16172=EDGE_CURVE('',#12787,#12723,#8100,.T.);
#16173=EDGE_CURVE('',#12779,#12725,#8101,.T.);
#16174=EDGE_CURVE('',#12786,#12727,#8102,.T.);
#16175=EDGE_CURVE('',#12780,#12729,#8103,.T.);
#16176=EDGE_CURVE('',#12785,#12731,#8104,.T.);
#16177=EDGE_CURVE('',#12781,#12705,#8105,.T.);
#16178=EDGE_CURVE('',#12784,#12707,#8106,.T.);
#16179=EDGE_CURVE('',#12782,#12814,#8107,.T.);
#16180=EDGE_CURVE('',#12814,#12814,#1400,.T.);
#16181=EDGE_CURVE('',#12814,#12635,#8108,.T.);
#16182=EDGE_CURVE('',#12783,#12815,#8109,.T.);
#16183=EDGE_CURVE('',#12815,#12815,#1401,.T.);
#16184=EDGE_CURVE('',#12815,#12631,#8110,.T.);
#16185=EDGE_CURVE('',#12684,#12613,#8111,.T.);
#16186=EDGE_CURVE('',#12816,#12817,#2310,.T.);
#16187=EDGE_CURVE('',#12817,#12818,#1402,.T.);
#16188=EDGE_CURVE('',#12818,#12819,#8112,.T.);
#16189=EDGE_CURVE('',#12819,#12819,#1403,.T.);
#16190=EDGE_CURVE('',#12818,#12816,#1404,.T.);
#16191=EDGE_CURVE('',#12816,#12820,#1405,.T.);
#16192=EDGE_CURVE('',#12820,#12821,#8113,.T.);
#16193=EDGE_CURVE('',#12821,#12821,#1406,.T.);
#16194=EDGE_CURVE('',#12820,#12822,#1407,.T.);
#16195=EDGE_CURVE('',#12822,#12823,#169,.T.);
#16196=EDGE_CURVE('',#12823,#12817,#1408,.T.);
#16197=EDGE_CURVE('',#12819,#12824,#8114,.T.);
#16198=EDGE_CURVE('',#12824,#12824,#1409,.T.);
#16199=EDGE_CURVE('',#12822,#12825,#8115,.T.);
#16200=EDGE_CURVE('',#12825,#12826,#8116,.T.);
#16201=EDGE_CURVE('',#12826,#12827,#8117,.T.);
#16202=EDGE_CURVE('',#12828,#12827,#8118,.T.);
#16203=EDGE_CURVE('',#12828,#12829,#8119,.T.);
#16204=EDGE_CURVE('',#12829,#12823,#8120,.T.);
#16205=EDGE_CURVE('',#12821,#12830,#8121,.T.);
#16206=EDGE_CURVE('',#12830,#12830,#1410,.T.);
#16207=EDGE_CURVE('',#12831,#12825,#8122,.T.);
#16208=EDGE_CURVE('',#12826,#12831,#8123,.T.);
#16209=EDGE_CURVE('',#12832,#12833,#8124,.T.);
#16210=EDGE_CURVE('',#12834,#12832,#8125,.T.);
#16211=EDGE_CURVE('',#12833,#12834,#8126,.T.);
#16212=EDGE_CURVE('',#12831,#12834,#8127,.T.);
#16213=EDGE_CURVE('',#12832,#12826,#8128,.T.);
#16214=EDGE_CURVE('',#12835,#12836,#8129,.T.);
#16215=EDGE_CURVE('',#12836,#12833,#8130,.T.);
#16216=EDGE_CURVE('',#12834,#12837,#8131,.T.);
#16217=EDGE_CURVE('',#12837,#12835,#8132,.T.);
#16218=EDGE_CURVE('',#12838,#12839,#8133,.T.);
#16219=EDGE_CURVE('',#12840,#12838,#8134,.T.);
#16220=EDGE_CURVE('',#12839,#12840,#8135,.T.);
#16221=EDGE_CURVE('',#12827,#12840,#8136,.T.);
#16222=EDGE_CURVE('',#12838,#12841,#8137,.T.);
#16223=EDGE_CURVE('',#12841,#12828,#8138,.T.);
#16224=EDGE_CURVE('',#12833,#12839,#8139,.T.);
#16225=EDGE_CURVE('',#12840,#12832,#8140,.T.);
#16226=EDGE_CURVE('',#12842,#12843,#8141,.T.);
#16227=EDGE_CURVE('',#12843,#12838,#8142,.T.);
#16228=EDGE_CURVE('',#12839,#12844,#8143,.T.);
#16229=EDGE_CURVE('',#12844,#12842,#8144,.T.);
#16230=EDGE_CURVE('',#12845,#12846,#8145,.T.);
#16231=EDGE_CURVE('',#12846,#12831,#8146,.T.);
#16232=EDGE_CURVE('',#12825,#12847,#8147,.T.);
#16233=EDGE_CURVE('',#12847,#12845,#8148,.T.);
#16234=EDGE_CURVE('',#12844,#12836,#8149,.T.);
#16235=EDGE_CURVE('',#12848,#12848,#1411,.T.);
#16236=EDGE_CURVE('',#12849,#12849,#1412,.T.);
#16237=EDGE_CURVE('',#12837,#12846,#8150,.T.);
#16238=EDGE_CURVE('',#12850,#12850,#1413,.T.);
#16239=EDGE_CURVE('',#12851,#12851,#1414,.T.);
#16240=EDGE_CURVE('',#12852,#12845,#8151,.T.);
#16241=EDGE_CURVE('',#12852,#12853,#8152,.T.);
#16242=EDGE_CURVE('',#12853,#12835,#8153,.T.);
#16243=EDGE_CURVE('',#12847,#12854,#8154,.T.);
#16244=EDGE_CURVE('',#12854,#12855,#8155,.T.);
#16245=EDGE_CURVE('',#12855,#12852,#8156,.T.);
#16246=EDGE_CURVE('',#12856,#12854,#8157,.T.);
#16247=EDGE_CURVE('',#12855,#12856,#8158,.T.);
#16248=EDGE_CURVE('',#12841,#12856,#8159,.T.);
#16249=EDGE_CURVE('',#12854,#12829,#8160,.T.);
#16250=EDGE_CURVE('',#12853,#12857,#8161,.T.);
#16251=EDGE_CURVE('',#12857,#12842,#8162,.T.);
#16252=EDGE_CURVE('',#12857,#12855,#8163,.T.);
#16253=EDGE_CURVE('',#12856,#12843,#8164,.T.);
#16254=EDGE_CURVE('',#12858,#12858,#1415,.T.);
#16255=EDGE_CURVE('',#12859,#12859,#1416,.T.);
#16256=EDGE_CURVE('',#12860,#12860,#1417,.T.);
#16257=EDGE_CURVE('',#12861,#12861,#1418,.T.);
#16258=EDGE_CURVE('',#12860,#12849,#8165,.T.);
#16259=EDGE_CURVE('',#12861,#12848,#8166,.T.);
#16260=EDGE_CURVE('',#12859,#12862,#8167,.T.);
#16261=EDGE_CURVE('',#12863,#12862,#2311,.T.);
#16262=EDGE_CURVE('',#12864,#12863,#2312,.T.);
#16263=EDGE_CURVE('',#12862,#12864,#2313,.T.);
#16264=EDGE_CURVE('',#12865,#12866,#2314,.T.);
#16265=EDGE_CURVE('',#12866,#12865,#2315,.T.);
#16266=EDGE_CURVE('',#12866,#12867,#8168,.T.);
#16267=EDGE_CURVE('',#12867,#12867,#1419,.T.);
#16268=EDGE_CURVE('',#12851,#12862,#8169,.T.);
#16269=EDGE_CURVE('',#12864,#12868,#8170,.T.);
#16270=EDGE_CURVE('',#12868,#12868,#1420,.T.);
#16271=EDGE_CURVE('',#12858,#12850,#8171,.T.);
#16272=EDGE_CURVE('',#12869,#12870,#2316,.T.);
#16273=EDGE_CURVE('',#12871,#12869,#2317,.T.);
#16274=EDGE_CURVE('',#12872,#12871,#1421,.T.);
#16275=EDGE_CURVE('',#12872,#12873,#8172,.T.);
#16276=EDGE_CURVE('',#12874,#12873,#2318,.T.);
#16277=EDGE_CURVE('',#12873,#12874,#2319,.T.);
#16278=EDGE_CURVE('',#12870,#12872,#1422,.T.);
#16279=EDGE_CURVE('',#12870,#12871,#8173,.T.);
#16280=EDGE_CURVE('',#12875,#12875,#1423,.T.);
#16281=EDGE_CURVE('',#12875,#12875,#1424,.T.);
#16282=EDGE_CURVE('',#12871,#12870,#1425,.T.);
#16283=EDGE_CURVE('',#12876,#12877,#2320,.T.);
#16284=EDGE_CURVE('',#12878,#12876,#2321,.T.);
#16285=EDGE_CURVE('',#12879,#12878,#1426,.T.);
#16286=EDGE_CURVE('',#12877,#12879,#2322,.T.);
#16287=EDGE_CURVE('',#12877,#12880,#8174,.T.);
#16288=EDGE_CURVE('',#12881,#12880,#2323,.T.);
#16289=EDGE_CURVE('',#12880,#12881,#2324,.T.);
#16290=EDGE_CURVE('',#12879,#12878,#8175,.T.);
#16291=EDGE_CURVE('',#12882,#12882,#1427,.T.);
#16292=EDGE_CURVE('',#12882,#12882,#1428,.T.);
#16293=EDGE_CURVE('',#12879,#12878,#1429,.T.);
#16294=EDGE_CURVE('',#12876,#12869,#2325,.T.);
#16295=EDGE_CURVE('',#12883,#12884,#8176,.T.);
#16296=EDGE_CURVE('',#12883,#12885,#2326,.T.);
#16297=EDGE_CURVE('',#12885,#12886,#1430,.T.);
#16298=EDGE_CURVE('',#12886,#12884,#2327,.T.);
#16299=EDGE_CURVE('',#12887,#12888,#8177,.T.);
#16300=EDGE_CURVE('',#12887,#12883,#2328,.T.);
#16301=EDGE_CURVE('',#12884,#12888,#2329,.T.);
#16302=EDGE_CURVE('',#12889,#12890,#8178,.T.);
#16303=EDGE_CURVE('',#12889,#12887,#2330,.T.);
#16304=EDGE_CURVE('',#12888,#12890,#2331,.T.);
#16305=EDGE_CURVE('',#12891,#12892,#8179,.T.);
#16306=EDGE_CURVE('',#12891,#12889,#2332,.T.);
#16307=EDGE_CURVE('',#12890,#12892,#2333,.T.);
#16308=EDGE_CURVE('',#12893,#12894,#8180,.T.);
#16309=EDGE_CURVE('',#12893,#12891,#2334,.T.);
#16310=EDGE_CURVE('',#12892,#12894,#2335,.T.);
#16311=EDGE_CURVE('',#12895,#12896,#8181,.T.);
#16312=EDGE_CURVE('',#12895,#12893,#2336,.T.);
#16313=EDGE_CURVE('',#12894,#12896,#2337,.T.);
#16314=EDGE_CURVE('',#12897,#12898,#8182,.T.);
#16315=EDGE_CURVE('',#12897,#12895,#2338,.T.);
#16316=EDGE_CURVE('',#12896,#12898,#2339,.T.);
#16317=EDGE_CURVE('',#12899,#12900,#8183,.T.);
#16318=EDGE_CURVE('',#12899,#12897,#2340,.T.);
#16319=EDGE_CURVE('',#12898,#12900,#2341,.T.);
#16320=EDGE_CURVE('',#12901,#12902,#8184,.T.);
#16321=EDGE_CURVE('',#12901,#12899,#2342,.T.);
#16322=EDGE_CURVE('',#12900,#12902,#2343,.T.);
#16323=EDGE_CURVE('',#12903,#12904,#8185,.T.);
#16324=EDGE_CURVE('',#12903,#12901,#2344,.T.);
#16325=EDGE_CURVE('',#12902,#12904,#2345,.T.);
#16326=EDGE_CURVE('',#12905,#12906,#8186,.T.);
#16327=EDGE_CURVE('',#12905,#12907,#2346,.T.);
#16328=EDGE_CURVE('',#12908,#12907,#1431,.T.);
#16329=EDGE_CURVE('',#12906,#12908,#2347,.T.);
#16330=EDGE_CURVE('',#12909,#12910,#8187,.T.);
#16331=EDGE_CURVE('',#12909,#12905,#2348,.T.);
#16332=EDGE_CURVE('',#12910,#12906,#2349,.T.);
#16333=EDGE_CURVE('',#12911,#12912,#8188,.T.);
#16334=EDGE_CURVE('',#12911,#12909,#2350,.T.);
#16335=EDGE_CURVE('',#12912,#12910,#2351,.T.);
#16336=EDGE_CURVE('',#12913,#12914,#8189,.T.);
#16337=EDGE_CURVE('',#12913,#12911,#2352,.T.);
#16338=EDGE_CURVE('',#12914,#12912,#2353,.T.);
#16339=EDGE_CURVE('',#12915,#12916,#8190,.T.);
#16340=EDGE_CURVE('',#12915,#12913,#2354,.T.);
#16341=EDGE_CURVE('',#12916,#12914,#2355,.T.);
#16342=EDGE_CURVE('',#12917,#12918,#8191,.T.);
#16343=EDGE_CURVE('',#12917,#12915,#2356,.T.);
#16344=EDGE_CURVE('',#12918,#12916,#2357,.T.);
#16345=EDGE_CURVE('',#12919,#12920,#8192,.T.);
#16346=EDGE_CURVE('',#12919,#12917,#2358,.T.);
#16347=EDGE_CURVE('',#12920,#12918,#2359,.T.);
#16348=EDGE_CURVE('',#12921,#12922,#8193,.T.);
#16349=EDGE_CURVE('',#12921,#12919,#2360,.T.);
#16350=EDGE_CURVE('',#12922,#12920,#2361,.T.);
#16351=EDGE_CURVE('',#12923,#12924,#8194,.T.);
#16352=EDGE_CURVE('',#12923,#12921,#2362,.T.);
#16353=EDGE_CURVE('',#12924,#12922,#2363,.T.);
#16354=EDGE_CURVE('',#12925,#12926,#8195,.T.);
#16355=EDGE_CURVE('',#12925,#12923,#2364,.T.);
#16356=EDGE_CURVE('',#12926,#12924,#2365,.T.);
#16357=EDGE_CURVE('',#12907,#12927,#2366,.T.);
#16358=EDGE_CURVE('',#12928,#12927,#1432,.F.);
#16359=EDGE_CURVE('',#12929,#12928,#1433,.F.);
#16360=EDGE_CURVE('',#12929,#12908,#2367,.T.);
#16361=EDGE_CURVE('',#12904,#12929,#2368,.T.);
#16362=EDGE_CURVE('',#12930,#12886,#2369,.T.);
#16363=EDGE_CURVE('',#12930,#12926,#2370,.T.);
#16364=EDGE_CURVE('',#12886,#12931,#1434,.T.);
#16365=EDGE_CURVE('',#12931,#12885,#1435,.T.);
#16366=EDGE_CURVE('',#12885,#12932,#2371,.T.);
#16367=EDGE_CURVE('',#12932,#12930,#1436,.T.);
#16368=EDGE_CURVE('',#12932,#12925,#2372,.T.);
#16369=EDGE_CURVE('',#12927,#12903,#2373,.T.);
#16370=EDGE_CURVE('',#12933,#12934,#8196,.T.);
#16371=EDGE_CURVE('',#12933,#12935,#8197,.T.);
#16372=EDGE_CURVE('',#12936,#12935,#8198,.T.);
#16373=EDGE_CURVE('',#12934,#12936,#8199,.T.);
#16374=EDGE_CURVE('',#12934,#12937,#1437,.T.);
#16375=EDGE_CURVE('',#12936,#12937,#8200,.T.);
#16376=EDGE_CURVE('',#12937,#12938,#8201,.T.);
#16377=EDGE_CURVE('',#12935,#12938,#8202,.T.);
#16378=EDGE_CURVE('',#12938,#12933,#1438,.T.);
#16379=EDGE_CURVE('',#12939,#12940,#8203,.T.);
#16380=EDGE_CURVE('',#12939,#12941,#8204,.T.);
#16381=EDGE_CURVE('',#12942,#12941,#8205,.T.);
#16382=EDGE_CURVE('',#12940,#12942,#8206,.T.);
#16383=EDGE_CURVE('',#12940,#12943,#1439,.T.);
#16384=EDGE_CURVE('',#12942,#12943,#8207,.T.);
#16385=EDGE_CURVE('',#12943,#12944,#8208,.T.);
#16386=EDGE_CURVE('',#12941,#12944,#8209,.T.);
#16387=EDGE_CURVE('',#12944,#12939,#1440,.T.);
#16388=EDGE_CURVE('',#12945,#12946,#8210,.T.);
#16389=EDGE_CURVE('',#12945,#12947,#8211,.T.);
#16390=EDGE_CURVE('',#12948,#12947,#8212,.T.);
#16391=EDGE_CURVE('',#12946,#12948,#8213,.T.);
#16392=EDGE_CURVE('',#12946,#12949,#1441,.T.);
#16393=EDGE_CURVE('',#12948,#12949,#8214,.T.);
#16394=EDGE_CURVE('',#12949,#12950,#8215,.T.);
#16395=EDGE_CURVE('',#12947,#12950,#8216,.T.);
#16396=EDGE_CURVE('',#12950,#12945,#1442,.T.);
#16397=EDGE_CURVE('',#12951,#12952,#8217,.T.);
#16398=EDGE_CURVE('',#12951,#12953,#8218,.T.);
#16399=EDGE_CURVE('',#12954,#12953,#8219,.T.);
#16400=EDGE_CURVE('',#12952,#12954,#8220,.T.);
#16401=EDGE_CURVE('',#12952,#12955,#1443,.T.);
#16402=EDGE_CURVE('',#12954,#12955,#8221,.T.);
#16403=EDGE_CURVE('',#12955,#12956,#8222,.T.);
#16404=EDGE_CURVE('',#12953,#12956,#8223,.T.);
#16405=EDGE_CURVE('',#12956,#12951,#1444,.T.);
#16406=EDGE_CURVE('',#12957,#12958,#8224,.T.);
#16407=EDGE_CURVE('',#12957,#12959,#8225,.T.);
#16408=EDGE_CURVE('',#12960,#12959,#8226,.T.);
#16409=EDGE_CURVE('',#12958,#12960,#8227,.T.);
#16410=EDGE_CURVE('',#12958,#12961,#1445,.T.);
#16411=EDGE_CURVE('',#12960,#12961,#8228,.T.);
#16412=EDGE_CURVE('',#12961,#12962,#8229,.T.);
#16413=EDGE_CURVE('',#12959,#12962,#8230,.T.);
#16414=EDGE_CURVE('',#12962,#12957,#1446,.T.);
#16415=EDGE_CURVE('',#12963,#12964,#8231,.T.);
#16416=EDGE_CURVE('',#12963,#12965,#8232,.T.);
#16417=EDGE_CURVE('',#12966,#12965,#8233,.T.);
#16418=EDGE_CURVE('',#12964,#12966,#8234,.T.);
#16419=EDGE_CURVE('',#12964,#12967,#1447,.T.);
#16420=EDGE_CURVE('',#12966,#12967,#8235,.T.);
#16421=EDGE_CURVE('',#12967,#12968,#8236,.T.);
#16422=EDGE_CURVE('',#12965,#12968,#8237,.T.);
#16423=EDGE_CURVE('',#12968,#12963,#1448,.T.);
#16424=EDGE_CURVE('',#12969,#12970,#8238,.T.);
#16425=EDGE_CURVE('',#12969,#12971,#8239,.T.);
#16426=EDGE_CURVE('',#12972,#12971,#8240,.T.);
#16427=EDGE_CURVE('',#12970,#12972,#8241,.T.);
#16428=EDGE_CURVE('',#12970,#12973,#1449,.T.);
#16429=EDGE_CURVE('',#12972,#12973,#8242,.T.);
#16430=EDGE_CURVE('',#12973,#12974,#8243,.T.);
#16431=EDGE_CURVE('',#12971,#12974,#8244,.T.);
#16432=EDGE_CURVE('',#12974,#12969,#1450,.T.);
#16433=EDGE_CURVE('',#12975,#12976,#8245,.T.);
#16434=EDGE_CURVE('',#12975,#12977,#8246,.T.);
#16435=EDGE_CURVE('',#12978,#12977,#8247,.T.);
#16436=EDGE_CURVE('',#12976,#12978,#8248,.T.);
#16437=EDGE_CURVE('',#12976,#12979,#1451,.T.);
#16438=EDGE_CURVE('',#12978,#12979,#8249,.T.);
#16439=EDGE_CURVE('',#12979,#12980,#8250,.T.);
#16440=EDGE_CURVE('',#12977,#12980,#8251,.T.);
#16441=EDGE_CURVE('',#12980,#12975,#1452,.T.);
#16442=EDGE_CURVE('',#12981,#12982,#8252,.T.);
#16443=EDGE_CURVE('',#12981,#12983,#8253,.T.);
#16444=EDGE_CURVE('',#12984,#12983,#8254,.T.);
#16445=EDGE_CURVE('',#12982,#12984,#8255,.T.);
#16446=EDGE_CURVE('',#12982,#12985,#1453,.T.);
#16447=EDGE_CURVE('',#12984,#12985,#8256,.T.);
#16448=EDGE_CURVE('',#12985,#12986,#8257,.T.);
#16449=EDGE_CURVE('',#12983,#12986,#8258,.T.);
#16450=EDGE_CURVE('',#12986,#12981,#1454,.T.);
#16451=EDGE_CURVE('',#12987,#12988,#8259,.T.);
#16452=EDGE_CURVE('',#12987,#12989,#8260,.T.);
#16453=EDGE_CURVE('',#12990,#12989,#8261,.T.);
#16454=EDGE_CURVE('',#12988,#12990,#8262,.T.);
#16455=EDGE_CURVE('',#12988,#12991,#1455,.T.);
#16456=EDGE_CURVE('',#12990,#12991,#8263,.T.);
#16457=EDGE_CURVE('',#12991,#12992,#8264,.T.);
#16458=EDGE_CURVE('',#12989,#12992,#8265,.T.);
#16459=EDGE_CURVE('',#12992,#12987,#1456,.T.);
#16460=EDGE_CURVE('',#12993,#12994,#8266,.T.);
#16461=EDGE_CURVE('',#12993,#12995,#8267,.T.);
#16462=EDGE_CURVE('',#12996,#12995,#8268,.T.);
#16463=EDGE_CURVE('',#12994,#12996,#8269,.T.);
#16464=EDGE_CURVE('',#12994,#12997,#1457,.T.);
#16465=EDGE_CURVE('',#12996,#12997,#8270,.T.);
#16466=EDGE_CURVE('',#12997,#12998,#8271,.T.);
#16467=EDGE_CURVE('',#12995,#12998,#8272,.T.);
#16468=EDGE_CURVE('',#12998,#12993,#1458,.T.);
#16469=EDGE_CURVE('',#12999,#13000,#8273,.T.);
#16470=EDGE_CURVE('',#12999,#13001,#8274,.T.);
#16471=EDGE_CURVE('',#13002,#13001,#8275,.T.);
#16472=EDGE_CURVE('',#13000,#13002,#8276,.T.);
#16473=EDGE_CURVE('',#13000,#13003,#1459,.T.);
#16474=EDGE_CURVE('',#13002,#13003,#8277,.T.);
#16475=EDGE_CURVE('',#13003,#13004,#8278,.T.);
#16476=EDGE_CURVE('',#13001,#13004,#8279,.T.);
#16477=EDGE_CURVE('',#13004,#12999,#1460,.T.);
#16478=EDGE_CURVE('',#13005,#13006,#8280,.T.);
#16479=EDGE_CURVE('',#13005,#13007,#8281,.T.);
#16480=EDGE_CURVE('',#13008,#13007,#8282,.T.);
#16481=EDGE_CURVE('',#13006,#13008,#8283,.T.);
#16482=EDGE_CURVE('',#13006,#13009,#1461,.T.);
#16483=EDGE_CURVE('',#13008,#13009,#8284,.T.);
#16484=EDGE_CURVE('',#13009,#13010,#8285,.T.);
#16485=EDGE_CURVE('',#13007,#13010,#8286,.T.);
#16486=EDGE_CURVE('',#13010,#13005,#1462,.T.);
#16487=EDGE_CURVE('',#13011,#13012,#8287,.T.);
#16488=EDGE_CURVE('',#13011,#13013,#8288,.T.);
#16489=EDGE_CURVE('',#13014,#13013,#8289,.T.);
#16490=EDGE_CURVE('',#13012,#13014,#8290,.T.);
#16491=EDGE_CURVE('',#13012,#13015,#1463,.T.);
#16492=EDGE_CURVE('',#13014,#13015,#8291,.T.);
#16493=EDGE_CURVE('',#13015,#13016,#8292,.T.);
#16494=EDGE_CURVE('',#13013,#13016,#8293,.T.);
#16495=EDGE_CURVE('',#13016,#13011,#1464,.T.);
#16496=EDGE_CURVE('',#13017,#13018,#8294,.T.);
#16497=EDGE_CURVE('',#13017,#13019,#8295,.T.);
#16498=EDGE_CURVE('',#13020,#13019,#8296,.T.);
#16499=EDGE_CURVE('',#13018,#13020,#8297,.T.);
#16500=EDGE_CURVE('',#13018,#13021,#1465,.T.);
#16501=EDGE_CURVE('',#13020,#13021,#8298,.T.);
#16502=EDGE_CURVE('',#13021,#13022,#8299,.T.);
#16503=EDGE_CURVE('',#13019,#13022,#8300,.T.);
#16504=EDGE_CURVE('',#13022,#13017,#1466,.T.);
#16505=EDGE_CURVE('',#13023,#13024,#8301,.T.);
#16506=EDGE_CURVE('',#13023,#13025,#8302,.T.);
#16507=EDGE_CURVE('',#13026,#13025,#8303,.T.);
#16508=EDGE_CURVE('',#13024,#13026,#8304,.T.);
#16509=EDGE_CURVE('',#13024,#13027,#1467,.T.);
#16510=EDGE_CURVE('',#13026,#13027,#8305,.T.);
#16511=EDGE_CURVE('',#13027,#13028,#8306,.T.);
#16512=EDGE_CURVE('',#13025,#13028,#8307,.T.);
#16513=EDGE_CURVE('',#13028,#13023,#1468,.T.);
#16514=EDGE_CURVE('',#13029,#13030,#8308,.T.);
#16515=EDGE_CURVE('',#13029,#13031,#8309,.T.);
#16516=EDGE_CURVE('',#13032,#13031,#8310,.T.);
#16517=EDGE_CURVE('',#13030,#13032,#8311,.T.);
#16518=EDGE_CURVE('',#13030,#13033,#1469,.T.);
#16519=EDGE_CURVE('',#13032,#13033,#8312,.T.);
#16520=EDGE_CURVE('',#13033,#13034,#8313,.T.);
#16521=EDGE_CURVE('',#13031,#13034,#8314,.T.);
#16522=EDGE_CURVE('',#13034,#13029,#1470,.T.);
#16523=EDGE_CURVE('',#13035,#13036,#8315,.T.);
#16524=EDGE_CURVE('',#13035,#13037,#8316,.T.);
#16525=EDGE_CURVE('',#13038,#13037,#8317,.T.);
#16526=EDGE_CURVE('',#13036,#13038,#8318,.T.);
#16527=EDGE_CURVE('',#13036,#13039,#1471,.T.);
#16528=EDGE_CURVE('',#13038,#13040,#8319,.T.);
#16529=EDGE_CURVE('',#13039,#13040,#1472,.T.);
#16530=EDGE_CURVE('',#13040,#13041,#8320,.T.);
#16531=EDGE_CURVE('',#13037,#13041,#8321,.T.);
#16532=EDGE_CURVE('',#13041,#13042,#1473,.T.);
#16533=EDGE_CURVE('',#13042,#13035,#1474,.T.);
#16534=EDGE_CURVE('',#13043,#13044,#8322,.T.);
#16535=EDGE_CURVE('',#13043,#13045,#8323,.T.);
#16536=EDGE_CURVE('',#13046,#13045,#8324,.T.);
#16537=EDGE_CURVE('',#13044,#13046,#8325,.T.);
#16538=EDGE_CURVE('',#13044,#13047,#1475,.T.);
#16539=EDGE_CURVE('',#13046,#13047,#8326,.T.);
#16540=EDGE_CURVE('',#13047,#13048,#8327,.T.);
#16541=EDGE_CURVE('',#13045,#13048,#8328,.T.);
#16542=EDGE_CURVE('',#13048,#13043,#1476,.T.);
#16543=EDGE_CURVE('',#13049,#13050,#8329,.T.);
#16544=EDGE_CURVE('',#13049,#13051,#8330,.T.);
#16545=EDGE_CURVE('',#13052,#13051,#8331,.T.);
#16546=EDGE_CURVE('',#13050,#13052,#8332,.T.);
#16547=EDGE_CURVE('',#13050,#13053,#1477,.T.);
#16548=EDGE_CURVE('',#13052,#13053,#8333,.T.);
#16549=EDGE_CURVE('',#13053,#13054,#8334,.T.);
#16550=EDGE_CURVE('',#13051,#13054,#8335,.T.);
#16551=EDGE_CURVE('',#13054,#13049,#1478,.T.);
#16552=EDGE_CURVE('',#13055,#13056,#8336,.T.);
#16553=EDGE_CURVE('',#13055,#13057,#8337,.T.);
#16554=EDGE_CURVE('',#13058,#13057,#8338,.T.);
#16555=EDGE_CURVE('',#13056,#13058,#8339,.T.);
#16556=EDGE_CURVE('',#13056,#13059,#1479,.T.);
#16557=EDGE_CURVE('',#13058,#13059,#8340,.T.);
#16558=EDGE_CURVE('',#13059,#13060,#8341,.T.);
#16559=EDGE_CURVE('',#13057,#13060,#8342,.T.);
#16560=EDGE_CURVE('',#13060,#13055,#1480,.T.);
#16561=EDGE_CURVE('',#13061,#13062,#8343,.T.);
#16562=EDGE_CURVE('',#13061,#13063,#8344,.T.);
#16563=EDGE_CURVE('',#13064,#13063,#8345,.T.);
#16564=EDGE_CURVE('',#13062,#13064,#8346,.T.);
#16565=EDGE_CURVE('',#13062,#13065,#1481,.T.);
#16566=EDGE_CURVE('',#13064,#13065,#8347,.T.);
#16567=EDGE_CURVE('',#13065,#13066,#8348,.T.);
#16568=EDGE_CURVE('',#13063,#13066,#8349,.T.);
#16569=EDGE_CURVE('',#13066,#13061,#1482,.T.);
#16570=EDGE_CURVE('',#13067,#13068,#8350,.T.);
#16571=EDGE_CURVE('',#13067,#13069,#8351,.T.);
#16572=EDGE_CURVE('',#13070,#13069,#8352,.T.);
#16573=EDGE_CURVE('',#13068,#13070,#8353,.T.);
#16574=EDGE_CURVE('',#13068,#13071,#1483,.T.);
#16575=EDGE_CURVE('',#13070,#13071,#8354,.T.);
#16576=EDGE_CURVE('',#13071,#13072,#8355,.T.);
#16577=EDGE_CURVE('',#13069,#13072,#8356,.T.);
#16578=EDGE_CURVE('',#13072,#13067,#1484,.T.);
#16579=EDGE_CURVE('',#13073,#13074,#8357,.T.);
#16580=EDGE_CURVE('',#13073,#13075,#8358,.T.);
#16581=EDGE_CURVE('',#13076,#13075,#8359,.T.);
#16582=EDGE_CURVE('',#13074,#13076,#8360,.T.);
#16583=EDGE_CURVE('',#13074,#13077,#1485,.T.);
#16584=EDGE_CURVE('',#13076,#13077,#8361,.T.);
#16585=EDGE_CURVE('',#13077,#13078,#8362,.T.);
#16586=EDGE_CURVE('',#13075,#13078,#8363,.T.);
#16587=EDGE_CURVE('',#13078,#13073,#1486,.T.);
#16588=EDGE_CURVE('',#13079,#13080,#8364,.T.);
#16589=EDGE_CURVE('',#13079,#13081,#8365,.T.);
#16590=EDGE_CURVE('',#13082,#13081,#8366,.T.);
#16591=EDGE_CURVE('',#13080,#13082,#8367,.T.);
#16592=EDGE_CURVE('',#13080,#13083,#1487,.T.);
#16593=EDGE_CURVE('',#13082,#13083,#8368,.T.);
#16594=EDGE_CURVE('',#13083,#13084,#8369,.T.);
#16595=EDGE_CURVE('',#13081,#13084,#8370,.T.);
#16596=EDGE_CURVE('',#13084,#13079,#1488,.T.);
#16597=EDGE_CURVE('',#13085,#13086,#8371,.T.);
#16598=EDGE_CURVE('',#13085,#13087,#8372,.T.);
#16599=EDGE_CURVE('',#13088,#13087,#8373,.T.);
#16600=EDGE_CURVE('',#13086,#13088,#8374,.T.);
#16601=EDGE_CURVE('',#13086,#13089,#1489,.T.);
#16602=EDGE_CURVE('',#13088,#13089,#8375,.T.);
#16603=EDGE_CURVE('',#13089,#13090,#8376,.T.);
#16604=EDGE_CURVE('',#13087,#13090,#8377,.T.);
#16605=EDGE_CURVE('',#13090,#13085,#1490,.T.);
#16606=EDGE_CURVE('',#13091,#13092,#8378,.T.);
#16607=EDGE_CURVE('',#13091,#13093,#8379,.T.);
#16608=EDGE_CURVE('',#13094,#13093,#8380,.T.);
#16609=EDGE_CURVE('',#13092,#13094,#8381,.T.);
#16610=EDGE_CURVE('',#13092,#13095,#1491,.T.);
#16611=EDGE_CURVE('',#13094,#13095,#8382,.T.);
#16612=EDGE_CURVE('',#13095,#13096,#8383,.T.);
#16613=EDGE_CURVE('',#13093,#13096,#8384,.T.);
#16614=EDGE_CURVE('',#13096,#13091,#1492,.T.);
#16615=EDGE_CURVE('',#13097,#13098,#8385,.T.);
#16616=EDGE_CURVE('',#13097,#13099,#8386,.T.);
#16617=EDGE_CURVE('',#13100,#13099,#8387,.T.);
#16618=EDGE_CURVE('',#13098,#13100,#8388,.T.);
#16619=EDGE_CURVE('',#13098,#13101,#1493,.T.);
#16620=EDGE_CURVE('',#13100,#13101,#8389,.T.);
#16621=EDGE_CURVE('',#13101,#13102,#8390,.T.);
#16622=EDGE_CURVE('',#13099,#13102,#8391,.T.);
#16623=EDGE_CURVE('',#13102,#13097,#1494,.T.);
#16624=EDGE_CURVE('',#13103,#13104,#8392,.T.);
#16625=EDGE_CURVE('',#13103,#13105,#8393,.T.);
#16626=EDGE_CURVE('',#13106,#13105,#8394,.T.);
#16627=EDGE_CURVE('',#13104,#13106,#8395,.T.);
#16628=EDGE_CURVE('',#13104,#13107,#1495,.T.);
#16629=EDGE_CURVE('',#13106,#13107,#8396,.T.);
#16630=EDGE_CURVE('',#13107,#13108,#8397,.T.);
#16631=EDGE_CURVE('',#13105,#13108,#8398,.T.);
#16632=EDGE_CURVE('',#13108,#13103,#1496,.T.);
#16633=EDGE_CURVE('',#13109,#13110,#8399,.T.);
#16634=EDGE_CURVE('',#13109,#13111,#8400,.T.);
#16635=EDGE_CURVE('',#13112,#13111,#8401,.T.);
#16636=EDGE_CURVE('',#13110,#13112,#8402,.T.);
#16637=EDGE_CURVE('',#13110,#13113,#1497,.T.);
#16638=EDGE_CURVE('',#13112,#13113,#8403,.T.);
#16639=EDGE_CURVE('',#13113,#13114,#8404,.T.);
#16640=EDGE_CURVE('',#13111,#13114,#8405,.T.);
#16641=EDGE_CURVE('',#13114,#13109,#1498,.T.);
#16642=EDGE_CURVE('',#13115,#13116,#8406,.T.);
#16643=EDGE_CURVE('',#13115,#13117,#8407,.T.);
#16644=EDGE_CURVE('',#13118,#13117,#8408,.T.);
#16645=EDGE_CURVE('',#13116,#13118,#8409,.T.);
#16646=EDGE_CURVE('',#13116,#13119,#1499,.T.);
#16647=EDGE_CURVE('',#13118,#13119,#8410,.T.);
#16648=EDGE_CURVE('',#13119,#13120,#8411,.T.);
#16649=EDGE_CURVE('',#13117,#13120,#8412,.T.);
#16650=EDGE_CURVE('',#13120,#13115,#1500,.T.);
#16651=EDGE_CURVE('',#13121,#13122,#8413,.T.);
#16652=EDGE_CURVE('',#13121,#13123,#8414,.T.);
#16653=EDGE_CURVE('',#13124,#13123,#8415,.T.);
#16654=EDGE_CURVE('',#13122,#13124,#8416,.T.);
#16655=EDGE_CURVE('',#13122,#13125,#1501,.T.);
#16656=EDGE_CURVE('',#13124,#13125,#8417,.T.);
#16657=EDGE_CURVE('',#13125,#13126,#8418,.T.);
#16658=EDGE_CURVE('',#13123,#13126,#8419,.T.);
#16659=EDGE_CURVE('',#13126,#13121,#1502,.T.);
#16660=EDGE_CURVE('',#13127,#13128,#8420,.T.);
#16661=EDGE_CURVE('',#13127,#13129,#8421,.T.);
#16662=EDGE_CURVE('',#13130,#13129,#8422,.T.);
#16663=EDGE_CURVE('',#13128,#13130,#8423,.T.);
#16664=EDGE_CURVE('',#13128,#13131,#1503,.T.);
#16665=EDGE_CURVE('',#13130,#13131,#8424,.T.);
#16666=EDGE_CURVE('',#13131,#13132,#8425,.T.);
#16667=EDGE_CURVE('',#13129,#13132,#8426,.T.);
#16668=EDGE_CURVE('',#13132,#13127,#1504,.T.);
#16669=EDGE_CURVE('',#13133,#13134,#8427,.T.);
#16670=EDGE_CURVE('',#13133,#13135,#8428,.T.);
#16671=EDGE_CURVE('',#13136,#13135,#8429,.T.);
#16672=EDGE_CURVE('',#13134,#13136,#8430,.T.);
#16673=EDGE_CURVE('',#13134,#13137,#1505,.T.);
#16674=EDGE_CURVE('',#13136,#13137,#8431,.T.);
#16675=EDGE_CURVE('',#13137,#13138,#8432,.T.);
#16676=EDGE_CURVE('',#13135,#13138,#8433,.T.);
#16677=EDGE_CURVE('',#13138,#13133,#1506,.T.);
#16678=EDGE_CURVE('',#13139,#13140,#8434,.T.);
#16679=EDGE_CURVE('',#13139,#13141,#8435,.T.);
#16680=EDGE_CURVE('',#13142,#13141,#8436,.T.);
#16681=EDGE_CURVE('',#13140,#13142,#8437,.T.);
#16682=EDGE_CURVE('',#13140,#13143,#1507,.T.);
#16683=EDGE_CURVE('',#13142,#13143,#8438,.T.);
#16684=EDGE_CURVE('',#13143,#13144,#8439,.T.);
#16685=EDGE_CURVE('',#13141,#13144,#8440,.T.);
#16686=EDGE_CURVE('',#13144,#13139,#1508,.T.);
#16687=EDGE_CURVE('',#13145,#13146,#8441,.T.);
#16688=EDGE_CURVE('',#13145,#13147,#8442,.T.);
#16689=EDGE_CURVE('',#13148,#13147,#8443,.T.);
#16690=EDGE_CURVE('',#13146,#13148,#8444,.T.);
#16691=EDGE_CURVE('',#13146,#13149,#1509,.T.);
#16692=EDGE_CURVE('',#13148,#13149,#8445,.T.);
#16693=EDGE_CURVE('',#13149,#13150,#8446,.T.);
#16694=EDGE_CURVE('',#13147,#13150,#8447,.T.);
#16695=EDGE_CURVE('',#13150,#13145,#1510,.T.);
#16696=EDGE_CURVE('',#13151,#13152,#8448,.T.);
#16697=EDGE_CURVE('',#13152,#13152,#1511,.T.);
#16698=EDGE_CURVE('',#13153,#13154,#8449,.T.);
#16699=EDGE_CURVE('',#13153,#13155,#8450,.T.);
#16700=EDGE_CURVE('',#13155,#13156,#8451,.T.);
#16701=EDGE_CURVE('',#13154,#13156,#8452,.T.);
#16702=EDGE_CURVE('',#13157,#13153,#8453,.T.);
#16703=EDGE_CURVE('',#13157,#13158,#8454,.T.);
#16704=EDGE_CURVE('',#13158,#13155,#8455,.T.);
#16705=EDGE_CURVE('',#13159,#13157,#8456,.T.);
#16706=EDGE_CURVE('',#13159,#13160,#8457,.T.);
#16707=EDGE_CURVE('',#13160,#13158,#8458,.T.);
#16708=EDGE_CURVE('',#13161,#13159,#8459,.T.);
#16709=EDGE_CURVE('',#13161,#13162,#8460,.T.);
#16710=EDGE_CURVE('',#13162,#13160,#8461,.T.);
#16711=EDGE_CURVE('',#13163,#13161,#8462,.T.);
#16712=EDGE_CURVE('',#13163,#13164,#8463,.T.);
#16713=EDGE_CURVE('',#13164,#13162,#8464,.T.);
#16714=EDGE_CURVE('',#13154,#13163,#8465,.T.);
#16715=EDGE_CURVE('',#13156,#13164,#8466,.T.);
#16716=EDGE_CURVE('',#13165,#13166,#1512,.T.);
#16717=EDGE_CURVE('',#13166,#13167,#1513,.T.);
#16718=EDGE_CURVE('',#13167,#13167,#1514,.T.);
#16719=EDGE_CURVE('',#13166,#13165,#1515,.T.);
#16720=EDGE_CURVE('',#13165,#13168,#8467,.T.);
#16721=EDGE_CURVE('',#13168,#13168,#1516,.T.);
#16722=EDGE_CURVE('',#13169,#13169,#1517,.T.);
#16723=EDGE_CURVE('',#13170,#13170,#1518,.T.);
#16724=EDGE_CURVE('',#12931,#13170,#8468,.T.);
#16725=EDGE_CURVE('',#12927,#12929,#1519,.F.);
#16726=EDGE_CURVE('',#13171,#13171,#1520,.T.);
#16727=EDGE_CURVE('',#13171,#12928,#8469,.T.);
#16728=EDGE_CURVE('',#13172,#13172,#1521,.T.);
#16729=EDGE_CURVE('',#13172,#13171,#8470,.T.);
#16730=EDGE_CURVE('',#13173,#13173,#1522,.T.);
#16731=EDGE_CURVE('',#13173,#13042,#8471,.T.);
#16732=EDGE_CURVE('',#13039,#13169,#8472,.T.);
#16733=EDGE_CURVE('',#13174,#13174,#1523,.T.);
#16734=EDGE_CURVE('',#13174,#13173,#8473,.T.);
#16735=EDGE_CURVE('',#13175,#13175,#1524,.T.);
#16736=EDGE_CURVE('',#13175,#13176,#8474,.T.);
#16737=EDGE_CURVE('',#13176,#13176,#1525,.T.);
#16738=EDGE_CURVE('',#13177,#13177,#1526,.T.);
#16739=EDGE_CURVE('',#13178,#13178,#1527,.T.);
#16740=EDGE_CURVE('',#13178,#13177,#8475,.T.);
#16741=EDGE_CURVE('',#13179,#13180,#1528,.T.);
#16742=EDGE_CURVE('',#13181,#13181,#1529,.T.);
#16743=EDGE_CURVE('',#13182,#13182,#1530,.T.);
#16744=EDGE_CURVE('',#13182,#13181,#8476,.T.);
#16745=EDGE_CURVE('',#13183,#13183,#1531,.T.);
#16746=EDGE_CURVE('',#13183,#13182,#8477,.T.);
#16747=EDGE_CURVE('',#13184,#13184,#1532,.T.);
#16748=EDGE_CURVE('',#13184,#13183,#8478,.T.);
#16749=EDGE_CURVE('',#13185,#13185,#1533,.T.);
#16750=EDGE_CURVE('',#13185,#13186,#2374,.T.);
#16751=EDGE_CURVE('',#13186,#13186,#1534,.T.);
#16752=EDGE_CURVE('',#13187,#13187,#1535,.T.);
#16753=EDGE_CURVE('',#13187,#13188,#8479,.T.);
#16754=EDGE_CURVE('',#13188,#13189,#1536,.T.);
#16755=EDGE_CURVE('',#13189,#13188,#1537,.T.);
#16756=EDGE_CURVE('',#13189,#13190,#8480,.T.);
#16757=EDGE_CURVE('',#13190,#13190,#1538,.T.);
#16758=EDGE_CURVE('',#13191,#13191,#1539,.T.);
#16759=EDGE_CURVE('',#13191,#13192,#8481,.T.);
#16760=EDGE_CURVE('',#13192,#13192,#1540,.T.);
#16761=EDGE_CURVE('',#13193,#13193,#1541,.T.);
#16762=EDGE_CURVE('',#13190,#13193,#8482,.T.);
#16763=EDGE_CURVE('',#13194,#13195,#8483,.T.);
#16764=EDGE_CURVE('',#13194,#13196,#2375,.T.);
#16765=EDGE_CURVE('',#13196,#13197,#1542,.T.);
#16766=EDGE_CURVE('',#13197,#13195,#2376,.T.);
#16767=EDGE_CURVE('',#13198,#13199,#8484,.T.);
#16768=EDGE_CURVE('',#13198,#13194,#2377,.T.);
#16769=EDGE_CURVE('',#13195,#13199,#2378,.T.);
#16770=EDGE_CURVE('',#13200,#13201,#8485,.T.);
#16771=EDGE_CURVE('',#13200,#13198,#2379,.T.);
#16772=EDGE_CURVE('',#13199,#13201,#2380,.T.);
#16773=EDGE_CURVE('',#13202,#13203,#8486,.T.);
#16774=EDGE_CURVE('',#13202,#13200,#2381,.T.);
#16775=EDGE_CURVE('',#13201,#13203,#2382,.T.);
#16776=EDGE_CURVE('',#13204,#13205,#8487,.T.);
#16777=EDGE_CURVE('',#13204,#13202,#2383,.T.);
#16778=EDGE_CURVE('',#13203,#13205,#2384,.T.);
#16779=EDGE_CURVE('',#13206,#13207,#8488,.T.);
#16780=EDGE_CURVE('',#13206,#13204,#2385,.T.);
#16781=EDGE_CURVE('',#13205,#13207,#2386,.T.);
#16782=EDGE_CURVE('',#13208,#13209,#8489,.T.);
#16783=EDGE_CURVE('',#13208,#13206,#2387,.T.);
#16784=EDGE_CURVE('',#13207,#13209,#2388,.T.);
#16785=EDGE_CURVE('',#13210,#13211,#8490,.T.);
#16786=EDGE_CURVE('',#13210,#13208,#2389,.T.);
#16787=EDGE_CURVE('',#13209,#13211,#2390,.T.);
#16788=EDGE_CURVE('',#13212,#13213,#8491,.T.);
#16789=EDGE_CURVE('',#13212,#13210,#2391,.T.);
#16790=EDGE_CURVE('',#13211,#13213,#2392,.T.);
#16791=EDGE_CURVE('',#13214,#13215,#8492,.T.);
#16792=EDGE_CURVE('',#13214,#13212,#2393,.T.);
#16793=EDGE_CURVE('',#13213,#13215,#2394,.T.);
#16794=EDGE_CURVE('',#13216,#13217,#8493,.T.);
#16795=EDGE_CURVE('',#13216,#13214,#2395,.T.);
#16796=EDGE_CURVE('',#13215,#13217,#2396,.T.);
#16797=EDGE_CURVE('',#13218,#13219,#8494,.T.);
#16798=EDGE_CURVE('',#13218,#13216,#2397,.T.);
#16799=EDGE_CURVE('',#13217,#13219,#2398,.T.);
#16800=EDGE_CURVE('',#13220,#13221,#8495,.T.);
#16801=EDGE_CURVE('',#13220,#13218,#2399,.T.);
#16802=EDGE_CURVE('',#13219,#13221,#2400,.T.);
#16803=EDGE_CURVE('',#13222,#13223,#8496,.T.);
#16804=EDGE_CURVE('',#13222,#13220,#2401,.T.);
#16805=EDGE_CURVE('',#13221,#13223,#2402,.T.);
#16806=EDGE_CURVE('',#13224,#13225,#8497,.T.);
#16807=EDGE_CURVE('',#13224,#13222,#2403,.T.);
#16808=EDGE_CURVE('',#13223,#13225,#2404,.T.);
#16809=EDGE_CURVE('',#13226,#13227,#8498,.T.);
#16810=EDGE_CURVE('',#13226,#13224,#2405,.T.);
#16811=EDGE_CURVE('',#13225,#13227,#2406,.T.);
#16812=EDGE_CURVE('',#13228,#13229,#8499,.T.);
#16813=EDGE_CURVE('',#13228,#13226,#2407,.T.);
#16814=EDGE_CURVE('',#13227,#13229,#2408,.T.);
#16815=EDGE_CURVE('',#13230,#13231,#8500,.T.);
#16816=EDGE_CURVE('',#13230,#13228,#2409,.T.);
#16817=EDGE_CURVE('',#13229,#13231,#2410,.T.);
#16818=EDGE_CURVE('',#13232,#13233,#8501,.T.);
#16819=EDGE_CURVE('',#13232,#13230,#2411,.T.);
#16820=EDGE_CURVE('',#13231,#13233,#2412,.T.);
#16821=EDGE_CURVE('',#13234,#13235,#8502,.T.);
#16822=EDGE_CURVE('',#13234,#13232,#2413,.T.);
#16823=EDGE_CURVE('',#13233,#13235,#2414,.T.);
#16824=EDGE_CURVE('',#13236,#13237,#8503,.T.);
#16825=EDGE_CURVE('',#13236,#13234,#2415,.T.);
#16826=EDGE_CURVE('',#13235,#13237,#2416,.T.);
#16827=EDGE_CURVE('',#13238,#13239,#8504,.T.);
#16828=EDGE_CURVE('',#13238,#13236,#2417,.T.);
#16829=EDGE_CURVE('',#13237,#13239,#2418,.T.);
#16830=EDGE_CURVE('',#13240,#13241,#8505,.T.);
#16831=EDGE_CURVE('',#13240,#13238,#2419,.T.);
#16832=EDGE_CURVE('',#13239,#13241,#2420,.T.);
#16833=EDGE_CURVE('',#13242,#13243,#8506,.T.);
#16834=EDGE_CURVE('',#13242,#13240,#2421,.T.);
#16835=EDGE_CURVE('',#13241,#13243,#2422,.T.);
#16836=EDGE_CURVE('',#13244,#13245,#8507,.T.);
#16837=EDGE_CURVE('',#13244,#13242,#2423,.T.);
#16838=EDGE_CURVE('',#13243,#13245,#2424,.T.);
#16839=EDGE_CURVE('',#13246,#13247,#8508,.T.);
#16840=EDGE_CURVE('',#13246,#13244,#2425,.T.);
#16841=EDGE_CURVE('',#13245,#13247,#2426,.T.);
#16842=EDGE_CURVE('',#13248,#13249,#8509,.T.);
#16843=EDGE_CURVE('',#13248,#13246,#2427,.T.);
#16844=EDGE_CURVE('',#13247,#13249,#2428,.T.);
#16845=EDGE_CURVE('',#13250,#13251,#8510,.T.);
#16846=EDGE_CURVE('',#13250,#13248,#2429,.T.);
#16847=EDGE_CURVE('',#13249,#13251,#2430,.T.);
#16848=EDGE_CURVE('',#13252,#13253,#8511,.T.);
#16849=EDGE_CURVE('',#13252,#13250,#2431,.T.);
#16850=EDGE_CURVE('',#13251,#13253,#2432,.T.);
#16851=EDGE_CURVE('',#13254,#13255,#8512,.T.);
#16852=EDGE_CURVE('',#13254,#13252,#2433,.T.);
#16853=EDGE_CURVE('',#13253,#13255,#2434,.T.);
#16854=EDGE_CURVE('',#13256,#13257,#8513,.T.);
#16855=EDGE_CURVE('',#13256,#13254,#2435,.T.);
#16856=EDGE_CURVE('',#13255,#13257,#2436,.T.);
#16857=EDGE_CURVE('',#13258,#13259,#8514,.T.);
#16858=EDGE_CURVE('',#13258,#13256,#2437,.T.);
#16859=EDGE_CURVE('',#13257,#13259,#2438,.T.);
#16860=EDGE_CURVE('',#13260,#13261,#8515,.T.);
#16861=EDGE_CURVE('',#13260,#13258,#2439,.T.);
#16862=EDGE_CURVE('',#13259,#13261,#2440,.T.);
#16863=EDGE_CURVE('',#13262,#13263,#8516,.T.);
#16864=EDGE_CURVE('',#13262,#13260,#2441,.T.);
#16865=EDGE_CURVE('',#13261,#13263,#2442,.T.);
#16866=EDGE_CURVE('',#13264,#13265,#8517,.T.);
#16867=EDGE_CURVE('',#13264,#13262,#2443,.T.);
#16868=EDGE_CURVE('',#13263,#13265,#2444,.T.);
#16869=EDGE_CURVE('',#13266,#13267,#8518,.T.);
#16870=EDGE_CURVE('',#13266,#13264,#2445,.T.);
#16871=EDGE_CURVE('',#13265,#13267,#2446,.T.);
#16872=EDGE_CURVE('',#13268,#13269,#8519,.T.);
#16873=EDGE_CURVE('',#13268,#13266,#2447,.T.);
#16874=EDGE_CURVE('',#13267,#13269,#2448,.T.);
#16875=EDGE_CURVE('',#13270,#13271,#8520,.T.);
#16876=EDGE_CURVE('',#13270,#13268,#2449,.T.);
#16877=EDGE_CURVE('',#13269,#13271,#2450,.T.);
#16878=EDGE_CURVE('',#13272,#13273,#8521,.T.);
#16879=EDGE_CURVE('',#13272,#13270,#2451,.T.);
#16880=EDGE_CURVE('',#13271,#13273,#2452,.T.);
#16881=EDGE_CURVE('',#13274,#13275,#8522,.T.);
#16882=EDGE_CURVE('',#13274,#13272,#2453,.T.);
#16883=EDGE_CURVE('',#13273,#13275,#2454,.T.);
#16884=EDGE_CURVE('',#13276,#13277,#8523,.T.);
#16885=EDGE_CURVE('',#13276,#13274,#2455,.T.);
#16886=EDGE_CURVE('',#13275,#13277,#2456,.T.);
#16887=EDGE_CURVE('',#13278,#13279,#8524,.T.);
#16888=EDGE_CURVE('',#13278,#13276,#2457,.T.);
#16889=EDGE_CURVE('',#13277,#13279,#2458,.T.);
#16890=EDGE_CURVE('',#13280,#13281,#8525,.T.);
#16891=EDGE_CURVE('',#13280,#13282,#2459,.T.);
#16892=EDGE_CURVE('',#13283,#13282,#1543,.T.);
#16893=EDGE_CURVE('',#13281,#13283,#2460,.T.);
#16894=EDGE_CURVE('',#13284,#13285,#8526,.T.);
#16895=EDGE_CURVE('',#13284,#13280,#2461,.T.);
#16896=EDGE_CURVE('',#13285,#13281,#2462,.T.);
#16897=EDGE_CURVE('',#13286,#13287,#8527,.T.);
#16898=EDGE_CURVE('',#13286,#13284,#2463,.T.);
#16899=EDGE_CURVE('',#13287,#13285,#2464,.T.);
#16900=EDGE_CURVE('',#13288,#13289,#8528,.T.);
#16901=EDGE_CURVE('',#13288,#13286,#2465,.T.);
#16902=EDGE_CURVE('',#13289,#13287,#2466,.T.);
#16903=EDGE_CURVE('',#13290,#13291,#8529,.T.);
#16904=EDGE_CURVE('',#13290,#13288,#2467,.T.);
#16905=EDGE_CURVE('',#13291,#13289,#2468,.T.);
#16906=EDGE_CURVE('',#13292,#13293,#8530,.T.);
#16907=EDGE_CURVE('',#13292,#13290,#2469,.T.);
#16908=EDGE_CURVE('',#13293,#13291,#2470,.T.);
#16909=EDGE_CURVE('',#13294,#13295,#8531,.T.);
#16910=EDGE_CURVE('',#13294,#13292,#2471,.T.);
#16911=EDGE_CURVE('',#13295,#13293,#2472,.T.);
#16912=EDGE_CURVE('',#13296,#13297,#8532,.T.);
#16913=EDGE_CURVE('',#13296,#13294,#2473,.T.);
#16914=EDGE_CURVE('',#13297,#13295,#2474,.T.);
#16915=EDGE_CURVE('',#13298,#13299,#8533,.T.);
#16916=EDGE_CURVE('',#13298,#13296,#2475,.T.);
#16917=EDGE_CURVE('',#13299,#13297,#2476,.T.);
#16918=EDGE_CURVE('',#13300,#13301,#8534,.T.);
#16919=EDGE_CURVE('',#13300,#13298,#2477,.T.);
#16920=EDGE_CURVE('',#13301,#13299,#2478,.T.);
#16921=EDGE_CURVE('',#13302,#13303,#8535,.T.);
#16922=EDGE_CURVE('',#13302,#13300,#2479,.T.);
#16923=EDGE_CURVE('',#13303,#13301,#2480,.T.);
#16924=EDGE_CURVE('',#13304,#13305,#8536,.T.);
#16925=EDGE_CURVE('',#13304,#13302,#2481,.T.);
#16926=EDGE_CURVE('',#13305,#13303,#2482,.T.);
#16927=EDGE_CURVE('',#13306,#13307,#8537,.T.);
#16928=EDGE_CURVE('',#13306,#13304,#2483,.T.);
#16929=EDGE_CURVE('',#13307,#13305,#2484,.T.);
#16930=EDGE_CURVE('',#13308,#13309,#8538,.T.);
#16931=EDGE_CURVE('',#13308,#13306,#2485,.T.);
#16932=EDGE_CURVE('',#13309,#13307,#2486,.T.);
#16933=EDGE_CURVE('',#13310,#13311,#8539,.T.);
#16934=EDGE_CURVE('',#13310,#13308,#2487,.T.);
#16935=EDGE_CURVE('',#13311,#13309,#2488,.T.);
#16936=EDGE_CURVE('',#13312,#13313,#8540,.T.);
#16937=EDGE_CURVE('',#13312,#13310,#2489,.T.);
#16938=EDGE_CURVE('',#13313,#13311,#2490,.T.);
#16939=EDGE_CURVE('',#13314,#13315,#8541,.T.);
#16940=EDGE_CURVE('',#13314,#13312,#2491,.T.);
#16941=EDGE_CURVE('',#13315,#13313,#2492,.T.);
#16942=EDGE_CURVE('',#13316,#13317,#8542,.T.);
#16943=EDGE_CURVE('',#13316,#13314,#2493,.T.);
#16944=EDGE_CURVE('',#13317,#13315,#2494,.T.);
#16945=EDGE_CURVE('',#13318,#13319,#8543,.T.);
#16946=EDGE_CURVE('',#13318,#13316,#2495,.T.);
#16947=EDGE_CURVE('',#13319,#13317,#2496,.T.);
#16948=EDGE_CURVE('',#13320,#13321,#8544,.T.);
#16949=EDGE_CURVE('',#13320,#13318,#2497,.T.);
#16950=EDGE_CURVE('',#13321,#13319,#2498,.T.);
#16951=EDGE_CURVE('',#13322,#13323,#8545,.T.);
#16952=EDGE_CURVE('',#13322,#13320,#2499,.T.);
#16953=EDGE_CURVE('',#13323,#13321,#2500,.T.);
#16954=EDGE_CURVE('',#13324,#13325,#8546,.T.);
#16955=EDGE_CURVE('',#13324,#13322,#2501,.T.);
#16956=EDGE_CURVE('',#13325,#13323,#2502,.T.);
#16957=EDGE_CURVE('',#13326,#13327,#8547,.T.);
#16958=EDGE_CURVE('',#13326,#13324,#2503,.T.);
#16959=EDGE_CURVE('',#13327,#13325,#2504,.T.);
#16960=EDGE_CURVE('',#13328,#13329,#8548,.T.);
#16961=EDGE_CURVE('',#13328,#13326,#2505,.T.);
#16962=EDGE_CURVE('',#13329,#13327,#2506,.T.);
#16963=EDGE_CURVE('',#13330,#13331,#8549,.T.);
#16964=EDGE_CURVE('',#13330,#13328,#2507,.T.);
#16965=EDGE_CURVE('',#13331,#13329,#2508,.T.);
#16966=EDGE_CURVE('',#13332,#13333,#8550,.T.);
#16967=EDGE_CURVE('',#13332,#13330,#2509,.T.);
#16968=EDGE_CURVE('',#13333,#13331,#2510,.T.);
#16969=EDGE_CURVE('',#13334,#13335,#8551,.T.);
#16970=EDGE_CURVE('',#13334,#13332,#2511,.T.);
#16971=EDGE_CURVE('',#13335,#13333,#2512,.T.);
#16972=EDGE_CURVE('',#13336,#13337,#8552,.T.);
#16973=EDGE_CURVE('',#13336,#13334,#2513,.T.);
#16974=EDGE_CURVE('',#13337,#13335,#2514,.T.);
#16975=EDGE_CURVE('',#13338,#13339,#8553,.T.);
#16976=EDGE_CURVE('',#13338,#13336,#2515,.T.);
#16977=EDGE_CURVE('',#13339,#13337,#2516,.T.);
#16978=EDGE_CURVE('',#13340,#13341,#8554,.T.);
#16979=EDGE_CURVE('',#13340,#13338,#2517,.T.);
#16980=EDGE_CURVE('',#13341,#13339,#2518,.T.);
#16981=EDGE_CURVE('',#13342,#13343,#8555,.T.);
#16982=EDGE_CURVE('',#13342,#13340,#2519,.T.);
#16983=EDGE_CURVE('',#13343,#13341,#2520,.T.);
#16984=EDGE_CURVE('',#13344,#13345,#8556,.T.);
#16985=EDGE_CURVE('',#13344,#13342,#2521,.T.);
#16986=EDGE_CURVE('',#13345,#13343,#2522,.T.);
#16987=EDGE_CURVE('',#13346,#13347,#8557,.T.);
#16988=EDGE_CURVE('',#13346,#13344,#2523,.T.);
#16989=EDGE_CURVE('',#13347,#13345,#2524,.T.);
#16990=EDGE_CURVE('',#13348,#13349,#8558,.T.);
#16991=EDGE_CURVE('',#13348,#13346,#2525,.T.);
#16992=EDGE_CURVE('',#13349,#13347,#2526,.T.);
#16993=EDGE_CURVE('',#13350,#13351,#8559,.T.);
#16994=EDGE_CURVE('',#13350,#13348,#2527,.T.);
#16995=EDGE_CURVE('',#13351,#13349,#2528,.T.);
#16996=EDGE_CURVE('',#13352,#13353,#8560,.T.);
#16997=EDGE_CURVE('',#13352,#13350,#2529,.T.);
#16998=EDGE_CURVE('',#13353,#13351,#2530,.T.);
#16999=EDGE_CURVE('',#13354,#13355,#8561,.T.);
#17000=EDGE_CURVE('',#13354,#13352,#2531,.T.);
#17001=EDGE_CURVE('',#13355,#13353,#2532,.T.);
#17002=EDGE_CURVE('',#13356,#13357,#8562,.T.);
#17003=EDGE_CURVE('',#13356,#13354,#2533,.T.);
#17004=EDGE_CURVE('',#13357,#13355,#2534,.T.);
#17005=EDGE_CURVE('',#13358,#13359,#8563,.T.);
#17006=EDGE_CURVE('',#13358,#13356,#2535,.T.);
#17007=EDGE_CURVE('',#13359,#13357,#2536,.T.);
#17008=EDGE_CURVE('',#13360,#13361,#8564,.T.);
#17009=EDGE_CURVE('',#13360,#13358,#2537,.T.);
#17010=EDGE_CURVE('',#13361,#13359,#2538,.T.);
#17011=EDGE_CURVE('',#13362,#13363,#8565,.T.);
#17012=EDGE_CURVE('',#13362,#13360,#2539,.T.);
#17013=EDGE_CURVE('',#13363,#13361,#2540,.T.);
#17014=EDGE_CURVE('',#13364,#13365,#8566,.T.);
#17015=EDGE_CURVE('',#13364,#13362,#2541,.T.);
#17016=EDGE_CURVE('',#13365,#13363,#2542,.T.);
#17017=EDGE_CURVE('',#13282,#13366,#2543,.T.);
#17018=EDGE_CURVE('',#13367,#13366,#1544,.T.);
#17019=EDGE_CURVE('',#13367,#13283,#2544,.T.);
#17020=EDGE_CURVE('',#13279,#13367,#2545,.T.);
#17021=EDGE_CURVE('',#13368,#13197,#2546,.T.);
#17022=EDGE_CURVE('',#13368,#13365,#2547,.T.);
#17023=EDGE_CURVE('',#13197,#13369,#1545,.T.);
#17024=EDGE_CURVE('',#13369,#13196,#1546,.T.);
#17025=EDGE_CURVE('',#13196,#13370,#2548,.T.);
#17026=EDGE_CURVE('',#13370,#13368,#1547,.T.);
#17027=EDGE_CURVE('',#13370,#13364,#2549,.T.);
#17028=EDGE_CURVE('',#13366,#13278,#2550,.T.);
#17029=EDGE_CURVE('',#13366,#13371,#1548,.T.);
#17030=EDGE_CURVE('',#13371,#13372,#1549,.T.);
#17031=EDGE_CURVE('',#13372,#13372,#1550,.T.);
#17032=EDGE_CURVE('',#13371,#13367,#1551,.T.);
#17033=EDGE_CURVE('',#13373,#13373,#1552,.T.);
#17034=EDGE_CURVE('',#13374,#13375,#8567,.T.);
#17035=EDGE_CURVE('',#13374,#13376,#8568,.T.);
#17036=EDGE_CURVE('',#13377,#13376,#8569,.T.);
#17037=EDGE_CURVE('',#13375,#13377,#8570,.T.);
#17038=EDGE_CURVE('',#13375,#13378,#1553,.T.);
#17039=EDGE_CURVE('',#13377,#13378,#8571,.T.);
#17040=EDGE_CURVE('',#13378,#13379,#8572,.T.);
#17041=EDGE_CURVE('',#13376,#13379,#8573,.T.);
#17042=EDGE_CURVE('',#13379,#13374,#1554,.T.);
#17043=EDGE_CURVE('',#13380,#13381,#8574,.T.);
#17044=EDGE_CURVE('',#13380,#13382,#8575,.T.);
#17045=EDGE_CURVE('',#13383,#13382,#8576,.T.);
#17046=EDGE_CURVE('',#13381,#13383,#8577,.T.);
#17047=EDGE_CURVE('',#13381,#13384,#1555,.T.);
#17048=EDGE_CURVE('',#13383,#13384,#8578,.T.);
#17049=EDGE_CURVE('',#13384,#13385,#8579,.T.);
#17050=EDGE_CURVE('',#13382,#13385,#8580,.T.);
#17051=EDGE_CURVE('',#13385,#13380,#1556,.T.);
#17052=EDGE_CURVE('',#13386,#13387,#8581,.T.);
#17053=EDGE_CURVE('',#13386,#13388,#8582,.T.);
#17054=EDGE_CURVE('',#13389,#13388,#8583,.T.);
#17055=EDGE_CURVE('',#13387,#13389,#8584,.T.);
#17056=EDGE_CURVE('',#13387,#13390,#1557,.T.);
#17057=EDGE_CURVE('',#13389,#13390,#8585,.T.);
#17058=EDGE_CURVE('',#13390,#13391,#8586,.T.);
#17059=EDGE_CURVE('',#13388,#13391,#8587,.T.);
#17060=EDGE_CURVE('',#13391,#13386,#1558,.T.);
#17061=EDGE_CURVE('',#13392,#13393,#8588,.T.);
#17062=EDGE_CURVE('',#13392,#13394,#8589,.T.);
#17063=EDGE_CURVE('',#13395,#13394,#8590,.T.);
#17064=EDGE_CURVE('',#13393,#13395,#8591,.T.);
#17065=EDGE_CURVE('',#13393,#13396,#1559,.T.);
#17066=EDGE_CURVE('',#13395,#13396,#8592,.T.);
#17067=EDGE_CURVE('',#13396,#13397,#8593,.T.);
#17068=EDGE_CURVE('',#13394,#13397,#8594,.T.);
#17069=EDGE_CURVE('',#13397,#13392,#1560,.T.);
#17070=EDGE_CURVE('',#13398,#13399,#8595,.T.);
#17071=EDGE_CURVE('',#13398,#13400,#8596,.T.);
#17072=EDGE_CURVE('',#13401,#13400,#8597,.T.);
#17073=EDGE_CURVE('',#13399,#13401,#8598,.T.);
#17074=EDGE_CURVE('',#13399,#13402,#1561,.T.);
#17075=EDGE_CURVE('',#13401,#13402,#8599,.T.);
#17076=EDGE_CURVE('',#13402,#13403,#8600,.T.);
#17077=EDGE_CURVE('',#13400,#13403,#8601,.T.);
#17078=EDGE_CURVE('',#13403,#13398,#1562,.T.);
#17079=EDGE_CURVE('',#13404,#13405,#8602,.T.);
#17080=EDGE_CURVE('',#13404,#13406,#8603,.T.);
#17081=EDGE_CURVE('',#13407,#13406,#8604,.T.);
#17082=EDGE_CURVE('',#13405,#13407,#8605,.T.);
#17083=EDGE_CURVE('',#13405,#13408,#1563,.T.);
#17084=EDGE_CURVE('',#13407,#13408,#8606,.T.);
#17085=EDGE_CURVE('',#13408,#13409,#8607,.T.);
#17086=EDGE_CURVE('',#13406,#13409,#8608,.T.);
#17087=EDGE_CURVE('',#13409,#13404,#1564,.T.);
#17088=EDGE_CURVE('',#13410,#13411,#8609,.T.);
#17089=EDGE_CURVE('',#13410,#13412,#8610,.T.);
#17090=EDGE_CURVE('',#13413,#13412,#8611,.T.);
#17091=EDGE_CURVE('',#13411,#13413,#8612,.T.);
#17092=EDGE_CURVE('',#13411,#13414,#1565,.T.);
#17093=EDGE_CURVE('',#13413,#13414,#8613,.T.);
#17094=EDGE_CURVE('',#13414,#13415,#8614,.T.);
#17095=EDGE_CURVE('',#13412,#13415,#8615,.T.);
#17096=EDGE_CURVE('',#13415,#13410,#1566,.T.);
#17097=EDGE_CURVE('',#13416,#13417,#8616,.T.);
#17098=EDGE_CURVE('',#13416,#13418,#8617,.T.);
#17099=EDGE_CURVE('',#13419,#13418,#8618,.T.);
#17100=EDGE_CURVE('',#13417,#13419,#8619,.T.);
#17101=EDGE_CURVE('',#13417,#13420,#1567,.T.);
#17102=EDGE_CURVE('',#13419,#13420,#8620,.T.);
#17103=EDGE_CURVE('',#13420,#13421,#8621,.T.);
#17104=EDGE_CURVE('',#13418,#13421,#8622,.T.);
#17105=EDGE_CURVE('',#13421,#13416,#1568,.T.);
#17106=EDGE_CURVE('',#13422,#13423,#8623,.T.);
#17107=EDGE_CURVE('',#13422,#13424,#8624,.T.);
#17108=EDGE_CURVE('',#13425,#13424,#8625,.T.);
#17109=EDGE_CURVE('',#13423,#13425,#8626,.T.);
#17110=EDGE_CURVE('',#13423,#13426,#1569,.T.);
#17111=EDGE_CURVE('',#13425,#13426,#8627,.T.);
#17112=EDGE_CURVE('',#13426,#13427,#8628,.T.);
#17113=EDGE_CURVE('',#13424,#13427,#8629,.T.);
#17114=EDGE_CURVE('',#13427,#13422,#1570,.T.);
#17115=EDGE_CURVE('',#13428,#13429,#8630,.T.);
#17116=EDGE_CURVE('',#13428,#13430,#8631,.T.);
#17117=EDGE_CURVE('',#13431,#13430,#8632,.T.);
#17118=EDGE_CURVE('',#13429,#13431,#8633,.T.);
#17119=EDGE_CURVE('',#13429,#13432,#1571,.T.);
#17120=EDGE_CURVE('',#13431,#13432,#8634,.T.);
#17121=EDGE_CURVE('',#13432,#13433,#8635,.T.);
#17122=EDGE_CURVE('',#13430,#13433,#8636,.T.);
#17123=EDGE_CURVE('',#13433,#13428,#1572,.T.);
#17124=EDGE_CURVE('',#13434,#13435,#8637,.T.);
#17125=EDGE_CURVE('',#13434,#13436,#8638,.T.);
#17126=EDGE_CURVE('',#13437,#13436,#8639,.T.);
#17127=EDGE_CURVE('',#13435,#13437,#8640,.T.);
#17128=EDGE_CURVE('',#13435,#13438,#1573,.T.);
#17129=EDGE_CURVE('',#13437,#13438,#8641,.T.);
#17130=EDGE_CURVE('',#13438,#13439,#8642,.T.);
#17131=EDGE_CURVE('',#13436,#13439,#8643,.T.);
#17132=EDGE_CURVE('',#13439,#13434,#1574,.T.);
#17133=EDGE_CURVE('',#13440,#13441,#8644,.T.);
#17134=EDGE_CURVE('',#13440,#13442,#8645,.T.);
#17135=EDGE_CURVE('',#13443,#13442,#8646,.T.);
#17136=EDGE_CURVE('',#13441,#13443,#8647,.T.);
#17137=EDGE_CURVE('',#13441,#13444,#1575,.T.);
#17138=EDGE_CURVE('',#13443,#13444,#8648,.T.);
#17139=EDGE_CURVE('',#13444,#13445,#8649,.T.);
#17140=EDGE_CURVE('',#13442,#13445,#8650,.T.);
#17141=EDGE_CURVE('',#13445,#13440,#1576,.T.);
#17142=EDGE_CURVE('',#13446,#13447,#8651,.T.);
#17143=EDGE_CURVE('',#13446,#13448,#8652,.T.);
#17144=EDGE_CURVE('',#13449,#13448,#8653,.T.);
#17145=EDGE_CURVE('',#13447,#13449,#8654,.T.);
#17146=EDGE_CURVE('',#13447,#13450,#1577,.T.);
#17147=EDGE_CURVE('',#13449,#13450,#8655,.T.);
#17148=EDGE_CURVE('',#13450,#13451,#8656,.T.);
#17149=EDGE_CURVE('',#13448,#13451,#8657,.T.);
#17150=EDGE_CURVE('',#13451,#13446,#1578,.T.);
#17151=EDGE_CURVE('',#13452,#13453,#8658,.T.);
#17152=EDGE_CURVE('',#13452,#13454,#8659,.T.);
#17153=EDGE_CURVE('',#13455,#13454,#8660,.T.);
#17154=EDGE_CURVE('',#13453,#13455,#8661,.T.);
#17155=EDGE_CURVE('',#13453,#13456,#1579,.T.);
#17156=EDGE_CURVE('',#13455,#13456,#8662,.T.);
#17157=EDGE_CURVE('',#13456,#13457,#8663,.T.);
#17158=EDGE_CURVE('',#13454,#13457,#8664,.T.);
#17159=EDGE_CURVE('',#13457,#13452,#1580,.T.);
#17160=EDGE_CURVE('',#13458,#13459,#8665,.T.);
#17161=EDGE_CURVE('',#13458,#13460,#8666,.T.);
#17162=EDGE_CURVE('',#13461,#13460,#8667,.T.);
#17163=EDGE_CURVE('',#13459,#13461,#8668,.T.);
#17164=EDGE_CURVE('',#13459,#13462,#1581,.T.);
#17165=EDGE_CURVE('',#13461,#13462,#8669,.T.);
#17166=EDGE_CURVE('',#13462,#13463,#8670,.T.);
#17167=EDGE_CURVE('',#13460,#13463,#8671,.T.);
#17168=EDGE_CURVE('',#13463,#13458,#1582,.T.);
#17169=EDGE_CURVE('',#13464,#13465,#8672,.T.);
#17170=EDGE_CURVE('',#13464,#13466,#8673,.T.);
#17171=EDGE_CURVE('',#13467,#13466,#8674,.T.);
#17172=EDGE_CURVE('',#13465,#13467,#8675,.T.);
#17173=EDGE_CURVE('',#13465,#13468,#1583,.T.);
#17174=EDGE_CURVE('',#13467,#13468,#8676,.T.);
#17175=EDGE_CURVE('',#13468,#13469,#8677,.T.);
#17176=EDGE_CURVE('',#13466,#13469,#8678,.T.);
#17177=EDGE_CURVE('',#13469,#13464,#1584,.T.);
#17178=EDGE_CURVE('',#13470,#13471,#8679,.T.);
#17179=EDGE_CURVE('',#13470,#13472,#8680,.T.);
#17180=EDGE_CURVE('',#13473,#13472,#8681,.T.);
#17181=EDGE_CURVE('',#13471,#13473,#8682,.T.);
#17182=EDGE_CURVE('',#13471,#13474,#1585,.T.);
#17183=EDGE_CURVE('',#13473,#13474,#8683,.T.);
#17184=EDGE_CURVE('',#13474,#13475,#8684,.T.);
#17185=EDGE_CURVE('',#13472,#13475,#8685,.T.);
#17186=EDGE_CURVE('',#13475,#13470,#1586,.T.);
#17187=EDGE_CURVE('',#13476,#13477,#8686,.T.);
#17188=EDGE_CURVE('',#13476,#13478,#8687,.T.);
#17189=EDGE_CURVE('',#13479,#13478,#8688,.T.);
#17190=EDGE_CURVE('',#13477,#13479,#8689,.T.);
#17191=EDGE_CURVE('',#13477,#13480,#1587,.T.);
#17192=EDGE_CURVE('',#13479,#13481,#8690,.T.);
#17193=EDGE_CURVE('',#13480,#13481,#1588,.T.);
#17194=EDGE_CURVE('',#13481,#13482,#8691,.T.);
#17195=EDGE_CURVE('',#13478,#13482,#8692,.T.);
#17196=EDGE_CURVE('',#13482,#13483,#1589,.T.);
#17197=EDGE_CURVE('',#13483,#13476,#1590,.T.);
#17198=EDGE_CURVE('',#13484,#13485,#8693,.T.);
#17199=EDGE_CURVE('',#13484,#13486,#8694,.T.);
#17200=EDGE_CURVE('',#13487,#13486,#8695,.T.);
#17201=EDGE_CURVE('',#13485,#13487,#8696,.T.);
#17202=EDGE_CURVE('',#13485,#13488,#1591,.T.);
#17203=EDGE_CURVE('',#13487,#13488,#8697,.T.);
#17204=EDGE_CURVE('',#13488,#13489,#8698,.T.);
#17205=EDGE_CURVE('',#13486,#13489,#8699,.T.);
#17206=EDGE_CURVE('',#13489,#13484,#1592,.T.);
#17207=EDGE_CURVE('',#13490,#13491,#8700,.T.);
#17208=EDGE_CURVE('',#13490,#13492,#8701,.T.);
#17209=EDGE_CURVE('',#13493,#13492,#8702,.T.);
#17210=EDGE_CURVE('',#13491,#13493,#8703,.T.);
#17211=EDGE_CURVE('',#13491,#13494,#1593,.T.);
#17212=EDGE_CURVE('',#13493,#13494,#8704,.T.);
#17213=EDGE_CURVE('',#13494,#13495,#8705,.T.);
#17214=EDGE_CURVE('',#13492,#13495,#8706,.T.);
#17215=EDGE_CURVE('',#13495,#13490,#1594,.T.);
#17216=EDGE_CURVE('',#13496,#13497,#8707,.T.);
#17217=EDGE_CURVE('',#13496,#13498,#8708,.T.);
#17218=EDGE_CURVE('',#13499,#13498,#8709,.T.);
#17219=EDGE_CURVE('',#13497,#13499,#8710,.T.);
#17220=EDGE_CURVE('',#13497,#13500,#1595,.T.);
#17221=EDGE_CURVE('',#13499,#13500,#8711,.T.);
#17222=EDGE_CURVE('',#13500,#13501,#8712,.T.);
#17223=EDGE_CURVE('',#13498,#13501,#8713,.T.);
#17224=EDGE_CURVE('',#13501,#13496,#1596,.T.);
#17225=EDGE_CURVE('',#13502,#13503,#8714,.T.);
#17226=EDGE_CURVE('',#13502,#13504,#8715,.T.);
#17227=EDGE_CURVE('',#13505,#13504,#8716,.T.);
#17228=EDGE_CURVE('',#13503,#13505,#8717,.T.);
#17229=EDGE_CURVE('',#13503,#13506,#1597,.T.);
#17230=EDGE_CURVE('',#13505,#13506,#8718,.T.);
#17231=EDGE_CURVE('',#13506,#13507,#8719,.T.);
#17232=EDGE_CURVE('',#13504,#13507,#8720,.T.);
#17233=EDGE_CURVE('',#13507,#13502,#1598,.T.);
#17234=EDGE_CURVE('',#13508,#13509,#8721,.T.);
#17235=EDGE_CURVE('',#13508,#13510,#8722,.T.);
#17236=EDGE_CURVE('',#13511,#13510,#8723,.T.);
#17237=EDGE_CURVE('',#13509,#13511,#8724,.T.);
#17238=EDGE_CURVE('',#13509,#13512,#1599,.T.);
#17239=EDGE_CURVE('',#13511,#13512,#8725,.T.);
#17240=EDGE_CURVE('',#13512,#13513,#8726,.T.);
#17241=EDGE_CURVE('',#13510,#13513,#8727,.T.);
#17242=EDGE_CURVE('',#13513,#13508,#1600,.T.);
#17243=EDGE_CURVE('',#13514,#13515,#8728,.T.);
#17244=EDGE_CURVE('',#13514,#13516,#8729,.T.);
#17245=EDGE_CURVE('',#13517,#13516,#8730,.T.);
#17246=EDGE_CURVE('',#13515,#13517,#8731,.T.);
#17247=EDGE_CURVE('',#13515,#13518,#1601,.T.);
#17248=EDGE_CURVE('',#13517,#13518,#8732,.T.);
#17249=EDGE_CURVE('',#13518,#13519,#8733,.T.);
#17250=EDGE_CURVE('',#13516,#13519,#8734,.T.);
#17251=EDGE_CURVE('',#13519,#13514,#1602,.T.);
#17252=EDGE_CURVE('',#13520,#13521,#8735,.T.);
#17253=EDGE_CURVE('',#13520,#13522,#8736,.T.);
#17254=EDGE_CURVE('',#13523,#13522,#8737,.T.);
#17255=EDGE_CURVE('',#13521,#13523,#8738,.T.);
#17256=EDGE_CURVE('',#13521,#13524,#1603,.T.);
#17257=EDGE_CURVE('',#13523,#13524,#8739,.T.);
#17258=EDGE_CURVE('',#13524,#13525,#8740,.T.);
#17259=EDGE_CURVE('',#13522,#13525,#8741,.T.);
#17260=EDGE_CURVE('',#13525,#13520,#1604,.T.);
#17261=EDGE_CURVE('',#13526,#13527,#8742,.T.);
#17262=EDGE_CURVE('',#13526,#13528,#8743,.T.);
#17263=EDGE_CURVE('',#13529,#13528,#8744,.T.);
#17264=EDGE_CURVE('',#13527,#13529,#8745,.T.);
#17265=EDGE_CURVE('',#13527,#13530,#1605,.T.);
#17266=EDGE_CURVE('',#13529,#13530,#8746,.T.);
#17267=EDGE_CURVE('',#13530,#13531,#8747,.T.);
#17268=EDGE_CURVE('',#13528,#13531,#8748,.T.);
#17269=EDGE_CURVE('',#13531,#13526,#1606,.T.);
#17270=EDGE_CURVE('',#13532,#13533,#8749,.T.);
#17271=EDGE_CURVE('',#13532,#13534,#8750,.T.);
#17272=EDGE_CURVE('',#13535,#13534,#8751,.T.);
#17273=EDGE_CURVE('',#13533,#13535,#8752,.T.);
#17274=EDGE_CURVE('',#13533,#13536,#1607,.T.);
#17275=EDGE_CURVE('',#13535,#13536,#8753,.T.);
#17276=EDGE_CURVE('',#13536,#13537,#8754,.T.);
#17277=EDGE_CURVE('',#13534,#13537,#8755,.T.);
#17278=EDGE_CURVE('',#13537,#13532,#1608,.T.);
#17279=EDGE_CURVE('',#13538,#13539,#8756,.T.);
#17280=EDGE_CURVE('',#13538,#13540,#8757,.T.);
#17281=EDGE_CURVE('',#13541,#13540,#8758,.T.);
#17282=EDGE_CURVE('',#13539,#13541,#8759,.T.);
#17283=EDGE_CURVE('',#13539,#13542,#1609,.T.);
#17284=EDGE_CURVE('',#13541,#13542,#8760,.T.);
#17285=EDGE_CURVE('',#13542,#13543,#8761,.T.);
#17286=EDGE_CURVE('',#13540,#13543,#8762,.T.);
#17287=EDGE_CURVE('',#13543,#13538,#1610,.T.);
#17288=EDGE_CURVE('',#13544,#13545,#8763,.T.);
#17289=EDGE_CURVE('',#13544,#13546,#8764,.T.);
#17290=EDGE_CURVE('',#13547,#13546,#8765,.T.);
#17291=EDGE_CURVE('',#13545,#13547,#8766,.T.);
#17292=EDGE_CURVE('',#13545,#13548,#1611,.T.);
#17293=EDGE_CURVE('',#13547,#13548,#8767,.T.);
#17294=EDGE_CURVE('',#13548,#13549,#8768,.T.);
#17295=EDGE_CURVE('',#13546,#13549,#8769,.T.);
#17296=EDGE_CURVE('',#13549,#13544,#1612,.T.);
#17297=EDGE_CURVE('',#13550,#13551,#8770,.T.);
#17298=EDGE_CURVE('',#13550,#13552,#8771,.T.);
#17299=EDGE_CURVE('',#13553,#13552,#8772,.T.);
#17300=EDGE_CURVE('',#13551,#13553,#8773,.T.);
#17301=EDGE_CURVE('',#13551,#13554,#1613,.T.);
#17302=EDGE_CURVE('',#13553,#13554,#8774,.T.);
#17303=EDGE_CURVE('',#13554,#13555,#8775,.T.);
#17304=EDGE_CURVE('',#13552,#13555,#8776,.T.);
#17305=EDGE_CURVE('',#13555,#13550,#1614,.T.);
#17306=EDGE_CURVE('',#13556,#13557,#8777,.T.);
#17307=EDGE_CURVE('',#13556,#13558,#8778,.T.);
#17308=EDGE_CURVE('',#13559,#13558,#8779,.T.);
#17309=EDGE_CURVE('',#13557,#13559,#8780,.T.);
#17310=EDGE_CURVE('',#13557,#13560,#1615,.T.);
#17311=EDGE_CURVE('',#13559,#13560,#8781,.T.);
#17312=EDGE_CURVE('',#13560,#13561,#8782,.T.);
#17313=EDGE_CURVE('',#13558,#13561,#8783,.T.);
#17314=EDGE_CURVE('',#13561,#13556,#1616,.T.);
#17315=EDGE_CURVE('',#13562,#13563,#8784,.T.);
#17316=EDGE_CURVE('',#13562,#13564,#8785,.T.);
#17317=EDGE_CURVE('',#13565,#13564,#8786,.T.);
#17318=EDGE_CURVE('',#13563,#13565,#8787,.T.);
#17319=EDGE_CURVE('',#13563,#13566,#1617,.T.);
#17320=EDGE_CURVE('',#13565,#13566,#8788,.T.);
#17321=EDGE_CURVE('',#13566,#13567,#8789,.T.);
#17322=EDGE_CURVE('',#13564,#13567,#8790,.T.);
#17323=EDGE_CURVE('',#13567,#13562,#1618,.T.);
#17324=EDGE_CURVE('',#13568,#13569,#8791,.T.);
#17325=EDGE_CURVE('',#13568,#13570,#8792,.T.);
#17326=EDGE_CURVE('',#13571,#13570,#8793,.T.);
#17327=EDGE_CURVE('',#13569,#13571,#8794,.T.);
#17328=EDGE_CURVE('',#13569,#13572,#1619,.T.);
#17329=EDGE_CURVE('',#13571,#13572,#8795,.T.);
#17330=EDGE_CURVE('',#13572,#13573,#8796,.T.);
#17331=EDGE_CURVE('',#13570,#13573,#8797,.T.);
#17332=EDGE_CURVE('',#13573,#13568,#1620,.T.);
#17333=EDGE_CURVE('',#13574,#13575,#8798,.T.);
#17334=EDGE_CURVE('',#13574,#13576,#8799,.T.);
#17335=EDGE_CURVE('',#13577,#13576,#8800,.T.);
#17336=EDGE_CURVE('',#13575,#13577,#8801,.T.);
#17337=EDGE_CURVE('',#13575,#13578,#1621,.T.);
#17338=EDGE_CURVE('',#13577,#13578,#8802,.T.);
#17339=EDGE_CURVE('',#13578,#13579,#8803,.T.);
#17340=EDGE_CURVE('',#13576,#13579,#8804,.T.);
#17341=EDGE_CURVE('',#13579,#13574,#1622,.T.);
#17342=EDGE_CURVE('',#13580,#13581,#8805,.T.);
#17343=EDGE_CURVE('',#13580,#13582,#8806,.T.);
#17344=EDGE_CURVE('',#13583,#13582,#8807,.T.);
#17345=EDGE_CURVE('',#13581,#13583,#8808,.T.);
#17346=EDGE_CURVE('',#13581,#13584,#1623,.T.);
#17347=EDGE_CURVE('',#13583,#13584,#8809,.T.);
#17348=EDGE_CURVE('',#13584,#13585,#8810,.T.);
#17349=EDGE_CURVE('',#13582,#13585,#8811,.T.);
#17350=EDGE_CURVE('',#13585,#13580,#1624,.T.);
#17351=EDGE_CURVE('',#13586,#13587,#8812,.T.);
#17352=EDGE_CURVE('',#13586,#13588,#8813,.T.);
#17353=EDGE_CURVE('',#13589,#13588,#8814,.T.);
#17354=EDGE_CURVE('',#13587,#13589,#8815,.T.);
#17355=EDGE_CURVE('',#13587,#13590,#1625,.T.);
#17356=EDGE_CURVE('',#13589,#13590,#8816,.T.);
#17357=EDGE_CURVE('',#13590,#13591,#8817,.T.);
#17358=EDGE_CURVE('',#13588,#13591,#8818,.T.);
#17359=EDGE_CURVE('',#13591,#13586,#1626,.T.);
#17360=EDGE_CURVE('',#13592,#13593,#8819,.T.);
#17361=EDGE_CURVE('',#13593,#13593,#1627,.T.);
#17362=EDGE_CURVE('',#13594,#13595,#8820,.T.);
#17363=EDGE_CURVE('',#13594,#13596,#8821,.T.);
#17364=EDGE_CURVE('',#13596,#13597,#8822,.T.);
#17365=EDGE_CURVE('',#13595,#13597,#8823,.T.);
#17366=EDGE_CURVE('',#13598,#13594,#8824,.T.);
#17367=EDGE_CURVE('',#13598,#13599,#8825,.T.);
#17368=EDGE_CURVE('',#13599,#13596,#8826,.T.);
#17369=EDGE_CURVE('',#13600,#13598,#8827,.T.);
#17370=EDGE_CURVE('',#13600,#13601,#8828,.T.);
#17371=EDGE_CURVE('',#13601,#13599,#8829,.T.);
#17372=EDGE_CURVE('',#13602,#13600,#8830,.T.);
#17373=EDGE_CURVE('',#13602,#13603,#8831,.T.);
#17374=EDGE_CURVE('',#13603,#13601,#8832,.T.);
#17375=EDGE_CURVE('',#13604,#13602,#8833,.T.);
#17376=EDGE_CURVE('',#13604,#13605,#8834,.T.);
#17377=EDGE_CURVE('',#13605,#13603,#8835,.T.);
#17378=EDGE_CURVE('',#13595,#13604,#8836,.T.);
#17379=EDGE_CURVE('',#13597,#13605,#8837,.T.);
#17380=EDGE_CURVE('',#13606,#13606,#1628,.T.);
#17381=EDGE_CURVE('',#13369,#13606,#8838,.T.);
#17382=EDGE_CURVE('',#13607,#13607,#1629,.T.);
#17383=EDGE_CURVE('',#13607,#13483,#8839,.T.);
#17384=EDGE_CURVE('',#13480,#13373,#8840,.T.);
#17385=EDGE_CURVE('',#13608,#13608,#1630,.T.);
#17386=EDGE_CURVE('',#13608,#13607,#8841,.T.);
#17387=EDGE_CURVE('',#13609,#13609,#1631,.T.);
#17388=EDGE_CURVE('',#13610,#13610,#1632,.T.);
#17389=EDGE_CURVE('',#13610,#13609,#8842,.T.);
#17390=EDGE_CURVE('',#13611,#13611,#1633,.T.);
#17391=EDGE_CURVE('',#13611,#13610,#8843,.T.);
#17392=EDGE_CURVE('',#13612,#13612,#1634,.T.);
#17393=EDGE_CURVE('',#13612,#13611,#8844,.T.);
#17394=EDGE_CURVE('',#13613,#13614,#8845,.T.);
#17395=EDGE_CURVE('',#13613,#13615,#2551,.T.);
#17396=EDGE_CURVE('',#13615,#13616,#1635,.T.);
#17397=EDGE_CURVE('',#13616,#13614,#2552,.T.);
#17398=EDGE_CURVE('',#13617,#13618,#8846,.T.);
#17399=EDGE_CURVE('',#13617,#13613,#2553,.T.);
#17400=EDGE_CURVE('',#13614,#13618,#2554,.T.);
#17401=EDGE_CURVE('',#13619,#13620,#8847,.T.);
#17402=EDGE_CURVE('',#13619,#13617,#2555,.T.);
#17403=EDGE_CURVE('',#13618,#13620,#2556,.T.);
#17404=EDGE_CURVE('',#13621,#13622,#8848,.T.);
#17405=EDGE_CURVE('',#13621,#13619,#2557,.T.);
#17406=EDGE_CURVE('',#13620,#13622,#2558,.T.);
#17407=EDGE_CURVE('',#13623,#13624,#8849,.T.);
#17408=EDGE_CURVE('',#13623,#13621,#2559,.T.);
#17409=EDGE_CURVE('',#13622,#13624,#2560,.T.);
#17410=EDGE_CURVE('',#13625,#13626,#8850,.T.);
#17411=EDGE_CURVE('',#13625,#13623,#2561,.T.);
#17412=EDGE_CURVE('',#13624,#13626,#2562,.T.);
#17413=EDGE_CURVE('',#13627,#13628,#8851,.T.);
#17414=EDGE_CURVE('',#13627,#13625,#2563,.T.);
#17415=EDGE_CURVE('',#13626,#13628,#2564,.T.);
#17416=EDGE_CURVE('',#13629,#13630,#8852,.T.);
#17417=EDGE_CURVE('',#13629,#13627,#2565,.T.);
#17418=EDGE_CURVE('',#13628,#13630,#2566,.T.);
#17419=EDGE_CURVE('',#13631,#13632,#8853,.T.);
#17420=EDGE_CURVE('',#13631,#13629,#2567,.T.);
#17421=EDGE_CURVE('',#13630,#13632,#2568,.T.);
#17422=EDGE_CURVE('',#13633,#13634,#8854,.T.);
#17423=EDGE_CURVE('',#13633,#13631,#2569,.T.);
#17424=EDGE_CURVE('',#13632,#13634,#2570,.T.);
#17425=EDGE_CURVE('',#13635,#13636,#8855,.T.);
#17426=EDGE_CURVE('',#13635,#13633,#2571,.T.);
#17427=EDGE_CURVE('',#13634,#13636,#2572,.T.);
#17428=EDGE_CURVE('',#13637,#13638,#8856,.T.);
#17429=EDGE_CURVE('',#13637,#13635,#2573,.T.);
#17430=EDGE_CURVE('',#13636,#13638,#2574,.T.);
#17431=EDGE_CURVE('',#13639,#13640,#8857,.T.);
#17432=EDGE_CURVE('',#13639,#13637,#2575,.T.);
#17433=EDGE_CURVE('',#13638,#13640,#2576,.T.);
#17434=EDGE_CURVE('',#13641,#13642,#8858,.T.);
#17435=EDGE_CURVE('',#13641,#13639,#2577,.T.);
#17436=EDGE_CURVE('',#13640,#13642,#2578,.T.);
#17437=EDGE_CURVE('',#13643,#13644,#8859,.T.);
#17438=EDGE_CURVE('',#13643,#13641,#2579,.T.);
#17439=EDGE_CURVE('',#13642,#13644,#2580,.T.);
#17440=EDGE_CURVE('',#13645,#13646,#8860,.T.);
#17441=EDGE_CURVE('',#13645,#13643,#2581,.T.);
#17442=EDGE_CURVE('',#13644,#13646,#2582,.T.);
#17443=EDGE_CURVE('',#13647,#13648,#8861,.T.);
#17444=EDGE_CURVE('',#13647,#13645,#2583,.T.);
#17445=EDGE_CURVE('',#13646,#13648,#2584,.T.);
#17446=EDGE_CURVE('',#13649,#13650,#8862,.T.);
#17447=EDGE_CURVE('',#13649,#13647,#2585,.T.);
#17448=EDGE_CURVE('',#13648,#13650,#2586,.T.);
#17449=EDGE_CURVE('',#13651,#13652,#8863,.T.);
#17450=EDGE_CURVE('',#13651,#13649,#2587,.T.);
#17451=EDGE_CURVE('',#13650,#13652,#2588,.T.);
#17452=EDGE_CURVE('',#13653,#13654,#8864,.T.);
#17453=EDGE_CURVE('',#13653,#13651,#2589,.T.);
#17454=EDGE_CURVE('',#13652,#13654,#2590,.T.);
#17455=EDGE_CURVE('',#13655,#13656,#8865,.T.);
#17456=EDGE_CURVE('',#13655,#13653,#2591,.T.);
#17457=EDGE_CURVE('',#13654,#13656,#2592,.T.);
#17458=EDGE_CURVE('',#13657,#13658,#8866,.T.);
#17459=EDGE_CURVE('',#13657,#13655,#2593,.T.);
#17460=EDGE_CURVE('',#13656,#13658,#2594,.T.);
#17461=EDGE_CURVE('',#13659,#13660,#8867,.T.);
#17462=EDGE_CURVE('',#13659,#13657,#2595,.T.);
#17463=EDGE_CURVE('',#13658,#13660,#2596,.T.);
#17464=EDGE_CURVE('',#13661,#13662,#8868,.T.);
#17465=EDGE_CURVE('',#13661,#13659,#2597,.T.);
#17466=EDGE_CURVE('',#13660,#13662,#2598,.T.);
#17467=EDGE_CURVE('',#13663,#13664,#8869,.T.);
#17468=EDGE_CURVE('',#13663,#13661,#2599,.T.);
#17469=EDGE_CURVE('',#13662,#13664,#2600,.T.);
#17470=EDGE_CURVE('',#13665,#13666,#8870,.T.);
#17471=EDGE_CURVE('',#13665,#13663,#2601,.T.);
#17472=EDGE_CURVE('',#13664,#13666,#2602,.T.);
#17473=EDGE_CURVE('',#13667,#13668,#8871,.T.);
#17474=EDGE_CURVE('',#13667,#13665,#2603,.T.);
#17475=EDGE_CURVE('',#13666,#13668,#2604,.T.);
#17476=EDGE_CURVE('',#13669,#13670,#8872,.T.);
#17477=EDGE_CURVE('',#13669,#13667,#2605,.T.);
#17478=EDGE_CURVE('',#13668,#13670,#2606,.T.);
#17479=EDGE_CURVE('',#13671,#13672,#8873,.T.);
#17480=EDGE_CURVE('',#13671,#13669,#2607,.T.);
#17481=EDGE_CURVE('',#13670,#13672,#2608,.T.);
#17482=EDGE_CURVE('',#13673,#13674,#8874,.T.);
#17483=EDGE_CURVE('',#13673,#13671,#2609,.T.);
#17484=EDGE_CURVE('',#13672,#13674,#2610,.T.);
#17485=EDGE_CURVE('',#13675,#13676,#8875,.T.);
#17486=EDGE_CURVE('',#13675,#13673,#2611,.T.);
#17487=EDGE_CURVE('',#13674,#13676,#2612,.T.);
#17488=EDGE_CURVE('',#13677,#13678,#8876,.T.);
#17489=EDGE_CURVE('',#13677,#13675,#2613,.T.);
#17490=EDGE_CURVE('',#13676,#13678,#2614,.T.);
#17491=EDGE_CURVE('',#13679,#13680,#8877,.T.);
#17492=EDGE_CURVE('',#13679,#13677,#2615,.T.);
#17493=EDGE_CURVE('',#13678,#13680,#2616,.T.);
#17494=EDGE_CURVE('',#13681,#13682,#8878,.T.);
#17495=EDGE_CURVE('',#13681,#13679,#2617,.T.);
#17496=EDGE_CURVE('',#13680,#13682,#2618,.T.);
#17497=EDGE_CURVE('',#13683,#13684,#8879,.T.);
#17498=EDGE_CURVE('',#13683,#13681,#2619,.T.);
#17499=EDGE_CURVE('',#13682,#13684,#2620,.T.);
#17500=EDGE_CURVE('',#13685,#13686,#8880,.T.);
#17501=EDGE_CURVE('',#13685,#13683,#2621,.T.);
#17502=EDGE_CURVE('',#13684,#13686,#2622,.T.);
#17503=EDGE_CURVE('',#13687,#13688,#8881,.T.);
#17504=EDGE_CURVE('',#13687,#13685,#2623,.T.);
#17505=EDGE_CURVE('',#13686,#13688,#2624,.T.);
#17506=EDGE_CURVE('',#13689,#13690,#8882,.T.);
#17507=EDGE_CURVE('',#13689,#13687,#2625,.T.);
#17508=EDGE_CURVE('',#13688,#13690,#2626,.T.);
#17509=EDGE_CURVE('',#13691,#13692,#8883,.T.);
#17510=EDGE_CURVE('',#13691,#13689,#2627,.T.);
#17511=EDGE_CURVE('',#13690,#13692,#2628,.T.);
#17512=EDGE_CURVE('',#13693,#13694,#8884,.T.);
#17513=EDGE_CURVE('',#13693,#13691,#2629,.T.);
#17514=EDGE_CURVE('',#13692,#13694,#2630,.T.);
#17515=EDGE_CURVE('',#13695,#13696,#8885,.T.);
#17516=EDGE_CURVE('',#13695,#13693,#2631,.T.);
#17517=EDGE_CURVE('',#13694,#13696,#2632,.T.);
#17518=EDGE_CURVE('',#13697,#13698,#8886,.T.);
#17519=EDGE_CURVE('',#13697,#13695,#2633,.T.);
#17520=EDGE_CURVE('',#13696,#13698,#2634,.T.);
#17521=EDGE_CURVE('',#13699,#13700,#8887,.T.);
#17522=EDGE_CURVE('',#13699,#13697,#2635,.T.);
#17523=EDGE_CURVE('',#13698,#13700,#2636,.T.);
#17524=EDGE_CURVE('',#13701,#13702,#8888,.T.);
#17525=EDGE_CURVE('',#13701,#13699,#2637,.T.);
#17526=EDGE_CURVE('',#13700,#13702,#2638,.T.);
#17527=EDGE_CURVE('',#13703,#13704,#8889,.T.);
#17528=EDGE_CURVE('',#13703,#13701,#2639,.T.);
#17529=EDGE_CURVE('',#13702,#13704,#2640,.T.);
#17530=EDGE_CURVE('',#13705,#13706,#8890,.T.);
#17531=EDGE_CURVE('',#13705,#13703,#2641,.T.);
#17532=EDGE_CURVE('',#13704,#13706,#2642,.T.);
#17533=EDGE_CURVE('',#13707,#13708,#8891,.T.);
#17534=EDGE_CURVE('',#13707,#13705,#2643,.T.);
#17535=EDGE_CURVE('',#13706,#13708,#2644,.T.);
#17536=EDGE_CURVE('',#13709,#13710,#8892,.T.);
#17537=EDGE_CURVE('',#13709,#13707,#2645,.T.);
#17538=EDGE_CURVE('',#13708,#13710,#2646,.T.);
#17539=EDGE_CURVE('',#13711,#13712,#8893,.T.);
#17540=EDGE_CURVE('',#13711,#13709,#2647,.T.);
#17541=EDGE_CURVE('',#13710,#13712,#2648,.T.);
#17542=EDGE_CURVE('',#13713,#13714,#8894,.T.);
#17543=EDGE_CURVE('',#13713,#13711,#2649,.T.);
#17544=EDGE_CURVE('',#13712,#13714,#2650,.T.);
#17545=EDGE_CURVE('',#13715,#13716,#8895,.T.);
#17546=EDGE_CURVE('',#13715,#13713,#2651,.T.);
#17547=EDGE_CURVE('',#13714,#13716,#2652,.T.);
#17548=EDGE_CURVE('',#13717,#13718,#8896,.T.);
#17549=EDGE_CURVE('',#13717,#13715,#2653,.T.);
#17550=EDGE_CURVE('',#13716,#13718,#2654,.T.);
#17551=EDGE_CURVE('',#13719,#13720,#8897,.T.);
#17552=EDGE_CURVE('',#13719,#13717,#2655,.T.);
#17553=EDGE_CURVE('',#13718,#13720,#2656,.T.);
#17554=EDGE_CURVE('',#13721,#13722,#8898,.T.);
#17555=EDGE_CURVE('',#13721,#13719,#2657,.T.);
#17556=EDGE_CURVE('',#13720,#13722,#2658,.T.);
#17557=EDGE_CURVE('',#13723,#13724,#8899,.T.);
#17558=EDGE_CURVE('',#13723,#13721,#2659,.T.);
#17559=EDGE_CURVE('',#13722,#13724,#2660,.T.);
#17560=EDGE_CURVE('',#13725,#13726,#8900,.T.);
#17561=EDGE_CURVE('',#13725,#13723,#2661,.T.);
#17562=EDGE_CURVE('',#13724,#13726,#2662,.T.);
#17563=EDGE_CURVE('',#13727,#13728,#8901,.T.);
#17564=EDGE_CURVE('',#13727,#13725,#2663,.T.);
#17565=EDGE_CURVE('',#13726,#13728,#2664,.T.);
#17566=EDGE_CURVE('',#13729,#13730,#8902,.T.);
#17567=EDGE_CURVE('',#13729,#13727,#2665,.T.);
#17568=EDGE_CURVE('',#13728,#13730,#2666,.T.);
#17569=EDGE_CURVE('',#13731,#13732,#8903,.T.);
#17570=EDGE_CURVE('',#13731,#13729,#2667,.T.);
#17571=EDGE_CURVE('',#13730,#13732,#2668,.T.);
#17572=EDGE_CURVE('',#13733,#13734,#8904,.T.);
#17573=EDGE_CURVE('',#13733,#13731,#2669,.T.);
#17574=EDGE_CURVE('',#13732,#13734,#2670,.T.);
#17575=EDGE_CURVE('',#13735,#13736,#8905,.T.);
#17576=EDGE_CURVE('',#13735,#13733,#2671,.T.);
#17577=EDGE_CURVE('',#13734,#13736,#2672,.T.);
#17578=EDGE_CURVE('',#13737,#13738,#8906,.T.);
#17579=EDGE_CURVE('',#13737,#13735,#2673,.T.);
#17580=EDGE_CURVE('',#13736,#13738,#2674,.T.);
#17581=EDGE_CURVE('',#13739,#13740,#8907,.T.);
#17582=EDGE_CURVE('',#13739,#13737,#2675,.T.);
#17583=EDGE_CURVE('',#13738,#13740,#2676,.T.);
#17584=EDGE_CURVE('',#13741,#13742,#8908,.T.);
#17585=EDGE_CURVE('',#13741,#13739,#2677,.T.);
#17586=EDGE_CURVE('',#13740,#13742,#2678,.T.);
#17587=EDGE_CURVE('',#13743,#13744,#8909,.T.);
#17588=EDGE_CURVE('',#13743,#13741,#2679,.T.);
#17589=EDGE_CURVE('',#13742,#13744,#2680,.T.);
#17590=EDGE_CURVE('',#13745,#13746,#8910,.T.);
#17591=EDGE_CURVE('',#13745,#13743,#2681,.T.);
#17592=EDGE_CURVE('',#13744,#13746,#2682,.T.);
#17593=EDGE_CURVE('',#13747,#13748,#8911,.T.);
#17594=EDGE_CURVE('',#13747,#13745,#2683,.T.);
#17595=EDGE_CURVE('',#13746,#13748,#2684,.T.);
#17596=EDGE_CURVE('',#13749,#13750,#8912,.T.);
#17597=EDGE_CURVE('',#13749,#13747,#2685,.T.);
#17598=EDGE_CURVE('',#13748,#13750,#2686,.T.);
#17599=EDGE_CURVE('',#13751,#13752,#8913,.T.);
#17600=EDGE_CURVE('',#13751,#13749,#2687,.T.);
#17601=EDGE_CURVE('',#13750,#13752,#2688,.T.);
#17602=EDGE_CURVE('',#13753,#13754,#8914,.T.);
#17603=EDGE_CURVE('',#13753,#13755,#2689,.T.);
#17604=EDGE_CURVE('',#13756,#13755,#1636,.T.);
#17605=EDGE_CURVE('',#13754,#13756,#2690,.T.);
#17606=EDGE_CURVE('',#13757,#13758,#8915,.T.);
#17607=EDGE_CURVE('',#13757,#13753,#2691,.T.);
#17608=EDGE_CURVE('',#13758,#13754,#2692,.T.);
#17609=EDGE_CURVE('',#13759,#13760,#8916,.T.);
#17610=EDGE_CURVE('',#13759,#13757,#2693,.T.);
#17611=EDGE_CURVE('',#13760,#13758,#2694,.T.);
#17612=EDGE_CURVE('',#13761,#13762,#8917,.T.);
#17613=EDGE_CURVE('',#13761,#13759,#2695,.T.);
#17614=EDGE_CURVE('',#13762,#13760,#2696,.T.);
#17615=EDGE_CURVE('',#13763,#13764,#8918,.T.);
#17616=EDGE_CURVE('',#13763,#13761,#2697,.T.);
#17617=EDGE_CURVE('',#13764,#13762,#2698,.T.);
#17618=EDGE_CURVE('',#13765,#13766,#8919,.T.);
#17619=EDGE_CURVE('',#13765,#13763,#2699,.T.);
#17620=EDGE_CURVE('',#13766,#13764,#2700,.T.);
#17621=EDGE_CURVE('',#13767,#13768,#8920,.T.);
#17622=EDGE_CURVE('',#13767,#13765,#2701,.T.);
#17623=EDGE_CURVE('',#13768,#13766,#2702,.T.);
#17624=EDGE_CURVE('',#13769,#13770,#8921,.T.);
#17625=EDGE_CURVE('',#13769,#13767,#2703,.T.);
#17626=EDGE_CURVE('',#13770,#13768,#2704,.T.);
#17627=EDGE_CURVE('',#13771,#13772,#8922,.T.);
#17628=EDGE_CURVE('',#13771,#13769,#2705,.T.);
#17629=EDGE_CURVE('',#13772,#13770,#2706,.T.);
#17630=EDGE_CURVE('',#13773,#13774,#8923,.T.);
#17631=EDGE_CURVE('',#13773,#13771,#2707,.T.);
#17632=EDGE_CURVE('',#13774,#13772,#2708,.T.);
#17633=EDGE_CURVE('',#13775,#13776,#8924,.T.);
#17634=EDGE_CURVE('',#13775,#13773,#2709,.T.);
#17635=EDGE_CURVE('',#13776,#13774,#2710,.T.);
#17636=EDGE_CURVE('',#13777,#13778,#8925,.T.);
#17637=EDGE_CURVE('',#13777,#13775,#2711,.T.);
#17638=EDGE_CURVE('',#13778,#13776,#2712,.T.);
#17639=EDGE_CURVE('',#13779,#13780,#8926,.T.);
#17640=EDGE_CURVE('',#13779,#13777,#2713,.T.);
#17641=EDGE_CURVE('',#13780,#13778,#2714,.T.);
#17642=EDGE_CURVE('',#13781,#13782,#8927,.T.);
#17643=EDGE_CURVE('',#13781,#13779,#2715,.T.);
#17644=EDGE_CURVE('',#13782,#13780,#2716,.T.);
#17645=EDGE_CURVE('',#13783,#13784,#8928,.T.);
#17646=EDGE_CURVE('',#13783,#13781,#2717,.T.);
#17647=EDGE_CURVE('',#13784,#13782,#2718,.T.);
#17648=EDGE_CURVE('',#13785,#13786,#8929,.T.);
#17649=EDGE_CURVE('',#13785,#13783,#2719,.T.);
#17650=EDGE_CURVE('',#13786,#13784,#2720,.T.);
#17651=EDGE_CURVE('',#13787,#13788,#8930,.T.);
#17652=EDGE_CURVE('',#13787,#13785,#2721,.T.);
#17653=EDGE_CURVE('',#13788,#13786,#2722,.T.);
#17654=EDGE_CURVE('',#13789,#13790,#8931,.T.);
#17655=EDGE_CURVE('',#13789,#13787,#2723,.T.);
#17656=EDGE_CURVE('',#13790,#13788,#2724,.T.);
#17657=EDGE_CURVE('',#13791,#13792,#8932,.T.);
#17658=EDGE_CURVE('',#13791,#13789,#2725,.T.);
#17659=EDGE_CURVE('',#13792,#13790,#2726,.T.);
#17660=EDGE_CURVE('',#13793,#13794,#8933,.T.);
#17661=EDGE_CURVE('',#13793,#13791,#2727,.T.);
#17662=EDGE_CURVE('',#13794,#13792,#2728,.T.);
#17663=EDGE_CURVE('',#13795,#13796,#8934,.T.);
#17664=EDGE_CURVE('',#13795,#13793,#2729,.T.);
#17665=EDGE_CURVE('',#13796,#13794,#2730,.T.);
#17666=EDGE_CURVE('',#13797,#13798,#8935,.T.);
#17667=EDGE_CURVE('',#13797,#13795,#2731,.T.);
#17668=EDGE_CURVE('',#13798,#13796,#2732,.T.);
#17669=EDGE_CURVE('',#13799,#13800,#8936,.T.);
#17670=EDGE_CURVE('',#13799,#13797,#2733,.T.);
#17671=EDGE_CURVE('',#13800,#13798,#2734,.T.);
#17672=EDGE_CURVE('',#13801,#13802,#8937,.T.);
#17673=EDGE_CURVE('',#13801,#13799,#2735,.T.);
#17674=EDGE_CURVE('',#13802,#13800,#2736,.T.);
#17675=EDGE_CURVE('',#13803,#13804,#8938,.T.);
#17676=EDGE_CURVE('',#13803,#13801,#2737,.T.);
#17677=EDGE_CURVE('',#13804,#13802,#2738,.T.);
#17678=EDGE_CURVE('',#13805,#13806,#8939,.T.);
#17679=EDGE_CURVE('',#13805,#13803,#2739,.T.);
#17680=EDGE_CURVE('',#13806,#13804,#2740,.T.);
#17681=EDGE_CURVE('',#13807,#13808,#8940,.T.);
#17682=EDGE_CURVE('',#13807,#13805,#2741,.T.);
#17683=EDGE_CURVE('',#13808,#13806,#2742,.T.);
#17684=EDGE_CURVE('',#13809,#13810,#8941,.T.);
#17685=EDGE_CURVE('',#13809,#13807,#2743,.T.);
#17686=EDGE_CURVE('',#13810,#13808,#2744,.T.);
#17687=EDGE_CURVE('',#13811,#13812,#8942,.T.);
#17688=EDGE_CURVE('',#13811,#13809,#2745,.T.);
#17689=EDGE_CURVE('',#13812,#13810,#2746,.T.);
#17690=EDGE_CURVE('',#13813,#13814,#8943,.T.);
#17691=EDGE_CURVE('',#13813,#13811,#2747,.T.);
#17692=EDGE_CURVE('',#13814,#13812,#2748,.T.);
#17693=EDGE_CURVE('',#13815,#13816,#8944,.T.);
#17694=EDGE_CURVE('',#13815,#13813,#2749,.T.);
#17695=EDGE_CURVE('',#13816,#13814,#2750,.T.);
#17696=EDGE_CURVE('',#13817,#13818,#8945,.T.);
#17697=EDGE_CURVE('',#13817,#13815,#2751,.T.);
#17698=EDGE_CURVE('',#13818,#13816,#2752,.T.);
#17699=EDGE_CURVE('',#13819,#13820,#8946,.T.);
#17700=EDGE_CURVE('',#13819,#13817,#2753,.T.);
#17701=EDGE_CURVE('',#13820,#13818,#2754,.T.);
#17702=EDGE_CURVE('',#13821,#13822,#8947,.T.);
#17703=EDGE_CURVE('',#13821,#13819,#2755,.T.);
#17704=EDGE_CURVE('',#13822,#13820,#2756,.T.);
#17705=EDGE_CURVE('',#13823,#13824,#8948,.T.);
#17706=EDGE_CURVE('',#13823,#13821,#2757,.T.);
#17707=EDGE_CURVE('',#13824,#13822,#2758,.T.);
#17708=EDGE_CURVE('',#13825,#13826,#8949,.T.);
#17709=EDGE_CURVE('',#13825,#13823,#2759,.T.);
#17710=EDGE_CURVE('',#13826,#13824,#2760,.T.);
#17711=EDGE_CURVE('',#13827,#13828,#8950,.T.);
#17712=EDGE_CURVE('',#13827,#13825,#2761,.T.);
#17713=EDGE_CURVE('',#13828,#13826,#2762,.T.);
#17714=EDGE_CURVE('',#13829,#13830,#8951,.T.);
#17715=EDGE_CURVE('',#13829,#13827,#2763,.T.);
#17716=EDGE_CURVE('',#13830,#13828,#2764,.T.);
#17717=EDGE_CURVE('',#13831,#13832,#8952,.T.);
#17718=EDGE_CURVE('',#13831,#13829,#2765,.T.);
#17719=EDGE_CURVE('',#13832,#13830,#2766,.T.);
#17720=EDGE_CURVE('',#13833,#13834,#8953,.T.);
#17721=EDGE_CURVE('',#13833,#13831,#2767,.T.);
#17722=EDGE_CURVE('',#13834,#13832,#2768,.T.);
#17723=EDGE_CURVE('',#13835,#13836,#8954,.T.);
#17724=EDGE_CURVE('',#13835,#13833,#2769,.T.);
#17725=EDGE_CURVE('',#13836,#13834,#2770,.T.);
#17726=EDGE_CURVE('',#13837,#13838,#8955,.T.);
#17727=EDGE_CURVE('',#13837,#13835,#2771,.T.);
#17728=EDGE_CURVE('',#13838,#13836,#2772,.T.);
#17729=EDGE_CURVE('',#13839,#13840,#8956,.T.);
#17730=EDGE_CURVE('',#13839,#13837,#2773,.T.);
#17731=EDGE_CURVE('',#13840,#13838,#2774,.T.);
#17732=EDGE_CURVE('',#13841,#13842,#8957,.T.);
#17733=EDGE_CURVE('',#13841,#13839,#2775,.T.);
#17734=EDGE_CURVE('',#13842,#13840,#2776,.T.);
#17735=EDGE_CURVE('',#13843,#13844,#8958,.T.);
#17736=EDGE_CURVE('',#13843,#13841,#2777,.T.);
#17737=EDGE_CURVE('',#13844,#13842,#2778,.T.);
#17738=EDGE_CURVE('',#13845,#13846,#8959,.T.);
#17739=EDGE_CURVE('',#13845,#13843,#2779,.T.);
#17740=EDGE_CURVE('',#13846,#13844,#2780,.T.);
#17741=EDGE_CURVE('',#13847,#13848,#8960,.T.);
#17742=EDGE_CURVE('',#13847,#13845,#2781,.T.);
#17743=EDGE_CURVE('',#13848,#13846,#2782,.T.);
#17744=EDGE_CURVE('',#13849,#13850,#8961,.T.);
#17745=EDGE_CURVE('',#13849,#13847,#2783,.T.);
#17746=EDGE_CURVE('',#13850,#13848,#2784,.T.);
#17747=EDGE_CURVE('',#13851,#13852,#8962,.T.);
#17748=EDGE_CURVE('',#13851,#13849,#2785,.T.);
#17749=EDGE_CURVE('',#13852,#13850,#2786,.T.);
#17750=EDGE_CURVE('',#13853,#13854,#8963,.T.);
#17751=EDGE_CURVE('',#13853,#13851,#2787,.T.);
#17752=EDGE_CURVE('',#13854,#13852,#2788,.T.);
#17753=EDGE_CURVE('',#13855,#13856,#8964,.T.);
#17754=EDGE_CURVE('',#13855,#13853,#2789,.T.);
#17755=EDGE_CURVE('',#13856,#13854,#2790,.T.);
#17756=EDGE_CURVE('',#13857,#13858,#8965,.T.);
#17757=EDGE_CURVE('',#13857,#13855,#2791,.T.);
#17758=EDGE_CURVE('',#13858,#13856,#2792,.T.);
#17759=EDGE_CURVE('',#13859,#13860,#8966,.T.);
#17760=EDGE_CURVE('',#13859,#13857,#2793,.T.);
#17761=EDGE_CURVE('',#13860,#13858,#2794,.T.);
#17762=EDGE_CURVE('',#13861,#13862,#8967,.T.);
#17763=EDGE_CURVE('',#13861,#13859,#2795,.T.);
#17764=EDGE_CURVE('',#13862,#13860,#2796,.T.);
#17765=EDGE_CURVE('',#13863,#13864,#8968,.T.);
#17766=EDGE_CURVE('',#13863,#13861,#2797,.T.);
#17767=EDGE_CURVE('',#13864,#13862,#2798,.T.);
#17768=EDGE_CURVE('',#13865,#13866,#8969,.T.);
#17769=EDGE_CURVE('',#13865,#13863,#2799,.T.);
#17770=EDGE_CURVE('',#13866,#13864,#2800,.T.);
#17771=EDGE_CURVE('',#13867,#13868,#8970,.T.);
#17772=EDGE_CURVE('',#13867,#13865,#2801,.T.);
#17773=EDGE_CURVE('',#13868,#13866,#2802,.T.);
#17774=EDGE_CURVE('',#13869,#13870,#8971,.T.);
#17775=EDGE_CURVE('',#13869,#13867,#2803,.T.);
#17776=EDGE_CURVE('',#13870,#13868,#2804,.T.);
#17777=EDGE_CURVE('',#13871,#13872,#8972,.T.);
#17778=EDGE_CURVE('',#13871,#13869,#2805,.T.);
#17779=EDGE_CURVE('',#13872,#13870,#2806,.T.);
#17780=EDGE_CURVE('',#13873,#13874,#8973,.T.);
#17781=EDGE_CURVE('',#13873,#13871,#2807,.T.);
#17782=EDGE_CURVE('',#13874,#13872,#2808,.T.);
#17783=EDGE_CURVE('',#13875,#13876,#8974,.T.);
#17784=EDGE_CURVE('',#13875,#13873,#2809,.T.);
#17785=EDGE_CURVE('',#13876,#13874,#2810,.T.);
#17786=EDGE_CURVE('',#13877,#13878,#8975,.T.);
#17787=EDGE_CURVE('',#13877,#13875,#2811,.T.);
#17788=EDGE_CURVE('',#13878,#13876,#2812,.T.);
#17789=EDGE_CURVE('',#13879,#13880,#8976,.T.);
#17790=EDGE_CURVE('',#13879,#13877,#2813,.T.);
#17791=EDGE_CURVE('',#13880,#13878,#2814,.T.);
#17792=EDGE_CURVE('',#13881,#13882,#8977,.T.);
#17793=EDGE_CURVE('',#13881,#13879,#2815,.T.);
#17794=EDGE_CURVE('',#13882,#13880,#2816,.T.);
#17795=EDGE_CURVE('',#13883,#13884,#8978,.T.);
#17796=EDGE_CURVE('',#13883,#13881,#2817,.T.);
#17797=EDGE_CURVE('',#13884,#13882,#2818,.T.);
#17798=EDGE_CURVE('',#13885,#13886,#8979,.T.);
#17799=EDGE_CURVE('',#13885,#13883,#2819,.T.);
#17800=EDGE_CURVE('',#13886,#13884,#2820,.T.);
#17801=EDGE_CURVE('',#13887,#13888,#8980,.T.);
#17802=EDGE_CURVE('',#13887,#13885,#2821,.T.);
#17803=EDGE_CURVE('',#13888,#13886,#2822,.T.);
#17804=EDGE_CURVE('',#13889,#13890,#8981,.T.);
#17805=EDGE_CURVE('',#13889,#13887,#2823,.T.);
#17806=EDGE_CURVE('',#13890,#13888,#2824,.T.);
#17807=EDGE_CURVE('',#13891,#13892,#8982,.T.);
#17808=EDGE_CURVE('',#13891,#13889,#2825,.T.);
#17809=EDGE_CURVE('',#13892,#13890,#2826,.T.);
#17810=EDGE_CURVE('',#13755,#13893,#2827,.T.);
#17811=EDGE_CURVE('',#13894,#13893,#1637,.T.);
#17812=EDGE_CURVE('',#13895,#13894,#1638,.T.);
#17813=EDGE_CURVE('',#13895,#13756,#2828,.T.);
#17814=EDGE_CURVE('',#13752,#13895,#2829,.T.);
#17815=EDGE_CURVE('',#13896,#13616,#2830,.T.);
#17816=EDGE_CURVE('',#13896,#13892,#2831,.T.);
#17817=EDGE_CURVE('',#13616,#13897,#1639,.T.);
#17818=EDGE_CURVE('',#13897,#13615,#1640,.T.);
#17819=EDGE_CURVE('',#13615,#13898,#2832,.T.);
#17820=EDGE_CURVE('',#13898,#13896,#1641,.T.);
#17821=EDGE_CURVE('',#13898,#13891,#2833,.T.);
#17822=EDGE_CURVE('',#13893,#13751,#2834,.T.);
#17823=EDGE_CURVE('',#13894,#13899,#1642,.T.);
#17824=EDGE_CURVE('',#13899,#13899,#1643,.T.);
#17825=EDGE_CURVE('',#13893,#13895,#1644,.T.);
#17826=EDGE_CURVE('',#13900,#13900,#1645,.T.);
#17827=EDGE_CURVE('',#13901,#13902,#8983,.T.);
#17828=EDGE_CURVE('',#13901,#13903,#8984,.T.);
#17829=EDGE_CURVE('',#13904,#13903,#8985,.T.);
#17830=EDGE_CURVE('',#13902,#13904,#8986,.T.);
#17831=EDGE_CURVE('',#13902,#13905,#1646,.T.);
#17832=EDGE_CURVE('',#13904,#13905,#8987,.T.);
#17833=EDGE_CURVE('',#13905,#13906,#8988,.T.);
#17834=EDGE_CURVE('',#13903,#13906,#8989,.T.);
#17835=EDGE_CURVE('',#13906,#13901,#1647,.T.);
#17836=EDGE_CURVE('',#13907,#13908,#8990,.T.);
#17837=EDGE_CURVE('',#13907,#13909,#8991,.T.);
#17838=EDGE_CURVE('',#13910,#13909,#8992,.T.);
#17839=EDGE_CURVE('',#13908,#13910,#8993,.T.);
#17840=EDGE_CURVE('',#13908,#13911,#1648,.T.);
#17841=EDGE_CURVE('',#13910,#13911,#8994,.T.);
#17842=EDGE_CURVE('',#13911,#13912,#8995,.T.);
#17843=EDGE_CURVE('',#13909,#13912,#8996,.T.);
#17844=EDGE_CURVE('',#13912,#13907,#1649,.T.);
#17845=EDGE_CURVE('',#13913,#13914,#8997,.T.);
#17846=EDGE_CURVE('',#13913,#13915,#8998,.T.);
#17847=EDGE_CURVE('',#13916,#13915,#8999,.T.);
#17848=EDGE_CURVE('',#13914,#13916,#9000,.T.);
#17849=EDGE_CURVE('',#13914,#13917,#1650,.T.);
#17850=EDGE_CURVE('',#13916,#13917,#9001,.T.);
#17851=EDGE_CURVE('',#13917,#13918,#9002,.T.);
#17852=EDGE_CURVE('',#13915,#13918,#9003,.T.);
#17853=EDGE_CURVE('',#13918,#13913,#1651,.T.);
#17854=EDGE_CURVE('',#13919,#13920,#9004,.T.);
#17855=EDGE_CURVE('',#13919,#13921,#9005,.T.);
#17856=EDGE_CURVE('',#13922,#13921,#9006,.T.);
#17857=EDGE_CURVE('',#13920,#13922,#9007,.T.);
#17858=EDGE_CURVE('',#13920,#13923,#1652,.T.);
#17859=EDGE_CURVE('',#13922,#13923,#9008,.T.);
#17860=EDGE_CURVE('',#13923,#13924,#9009,.T.);
#17861=EDGE_CURVE('',#13921,#13924,#9010,.T.);
#17862=EDGE_CURVE('',#13924,#13919,#1653,.T.);
#17863=EDGE_CURVE('',#13925,#13926,#9011,.T.);
#17864=EDGE_CURVE('',#13925,#13927,#9012,.T.);
#17865=EDGE_CURVE('',#13928,#13927,#9013,.T.);
#17866=EDGE_CURVE('',#13926,#13928,#9014,.T.);
#17867=EDGE_CURVE('',#13926,#13929,#1654,.T.);
#17868=EDGE_CURVE('',#13928,#13929,#9015,.T.);
#17869=EDGE_CURVE('',#13929,#13930,#9016,.T.);
#17870=EDGE_CURVE('',#13927,#13930,#9017,.T.);
#17871=EDGE_CURVE('',#13930,#13925,#1655,.T.);
#17872=EDGE_CURVE('',#13931,#13932,#9018,.T.);
#17873=EDGE_CURVE('',#13931,#13933,#9019,.T.);
#17874=EDGE_CURVE('',#13934,#13933,#9020,.T.);
#17875=EDGE_CURVE('',#13932,#13934,#9021,.T.);
#17876=EDGE_CURVE('',#13932,#13935,#1656,.T.);
#17877=EDGE_CURVE('',#13934,#13935,#9022,.T.);
#17878=EDGE_CURVE('',#13935,#13936,#9023,.T.);
#17879=EDGE_CURVE('',#13933,#13936,#9024,.T.);
#17880=EDGE_CURVE('',#13936,#13931,#1657,.T.);
#17881=EDGE_CURVE('',#13937,#13938,#9025,.T.);
#17882=EDGE_CURVE('',#13937,#13939,#9026,.T.);
#17883=EDGE_CURVE('',#13940,#13939,#9027,.T.);
#17884=EDGE_CURVE('',#13938,#13940,#9028,.T.);
#17885=EDGE_CURVE('',#13938,#13941,#1658,.T.);
#17886=EDGE_CURVE('',#13940,#13941,#9029,.T.);
#17887=EDGE_CURVE('',#13941,#13942,#9030,.T.);
#17888=EDGE_CURVE('',#13939,#13942,#9031,.T.);
#17889=EDGE_CURVE('',#13942,#13937,#1659,.T.);
#17890=EDGE_CURVE('',#13943,#13944,#9032,.T.);
#17891=EDGE_CURVE('',#13943,#13945,#9033,.T.);
#17892=EDGE_CURVE('',#13946,#13945,#9034,.T.);
#17893=EDGE_CURVE('',#13944,#13946,#9035,.T.);
#17894=EDGE_CURVE('',#13944,#13947,#1660,.T.);
#17895=EDGE_CURVE('',#13946,#13947,#9036,.T.);
#17896=EDGE_CURVE('',#13947,#13948,#9037,.T.);
#17897=EDGE_CURVE('',#13945,#13948,#9038,.T.);
#17898=EDGE_CURVE('',#13948,#13943,#1661,.T.);
#17899=EDGE_CURVE('',#13949,#13950,#9039,.T.);
#17900=EDGE_CURVE('',#13949,#13951,#9040,.T.);
#17901=EDGE_CURVE('',#13952,#13951,#9041,.T.);
#17902=EDGE_CURVE('',#13950,#13952,#9042,.T.);
#17903=EDGE_CURVE('',#13950,#13953,#1662,.T.);
#17904=EDGE_CURVE('',#13952,#13953,#9043,.T.);
#17905=EDGE_CURVE('',#13953,#13954,#9044,.T.);
#17906=EDGE_CURVE('',#13951,#13954,#9045,.T.);
#17907=EDGE_CURVE('',#13954,#13949,#1663,.T.);
#17908=EDGE_CURVE('',#13955,#13956,#9046,.T.);
#17909=EDGE_CURVE('',#13955,#13957,#9047,.T.);
#17910=EDGE_CURVE('',#13958,#13957,#9048,.T.);
#17911=EDGE_CURVE('',#13956,#13958,#9049,.T.);
#17912=EDGE_CURVE('',#13956,#13959,#1664,.T.);
#17913=EDGE_CURVE('',#13958,#13959,#9050,.T.);
#17914=EDGE_CURVE('',#13959,#13960,#9051,.T.);
#17915=EDGE_CURVE('',#13957,#13960,#9052,.T.);
#17916=EDGE_CURVE('',#13960,#13955,#1665,.T.);
#17917=EDGE_CURVE('',#13961,#13962,#9053,.T.);
#17918=EDGE_CURVE('',#13961,#13963,#9054,.T.);
#17919=EDGE_CURVE('',#13964,#13963,#9055,.T.);
#17920=EDGE_CURVE('',#13962,#13964,#9056,.T.);
#17921=EDGE_CURVE('',#13962,#13965,#1666,.T.);
#17922=EDGE_CURVE('',#13964,#13965,#9057,.T.);
#17923=EDGE_CURVE('',#13965,#13966,#9058,.T.);
#17924=EDGE_CURVE('',#13963,#13966,#9059,.T.);
#17925=EDGE_CURVE('',#13966,#13961,#1667,.T.);
#17926=EDGE_CURVE('',#13967,#13968,#9060,.T.);
#17927=EDGE_CURVE('',#13967,#13969,#9061,.T.);
#17928=EDGE_CURVE('',#13970,#13969,#9062,.T.);
#17929=EDGE_CURVE('',#13968,#13970,#9063,.T.);
#17930=EDGE_CURVE('',#13968,#13971,#1668,.T.);
#17931=EDGE_CURVE('',#13970,#13971,#9064,.T.);
#17932=EDGE_CURVE('',#13971,#13972,#9065,.T.);
#17933=EDGE_CURVE('',#13969,#13972,#9066,.T.);
#17934=EDGE_CURVE('',#13972,#13967,#1669,.T.);
#17935=EDGE_CURVE('',#13973,#13974,#9067,.T.);
#17936=EDGE_CURVE('',#13973,#13975,#9068,.T.);
#17937=EDGE_CURVE('',#13976,#13975,#9069,.T.);
#17938=EDGE_CURVE('',#13974,#13976,#9070,.T.);
#17939=EDGE_CURVE('',#13974,#13977,#1670,.T.);
#17940=EDGE_CURVE('',#13976,#13977,#9071,.T.);
#17941=EDGE_CURVE('',#13977,#13978,#9072,.T.);
#17942=EDGE_CURVE('',#13975,#13978,#9073,.T.);
#17943=EDGE_CURVE('',#13978,#13973,#1671,.T.);
#17944=EDGE_CURVE('',#13979,#13980,#9074,.T.);
#17945=EDGE_CURVE('',#13979,#13981,#9075,.T.);
#17946=EDGE_CURVE('',#13982,#13981,#9076,.T.);
#17947=EDGE_CURVE('',#13980,#13982,#9077,.T.);
#17948=EDGE_CURVE('',#13980,#13983,#1672,.T.);
#17949=EDGE_CURVE('',#13982,#13983,#9078,.T.);
#17950=EDGE_CURVE('',#13983,#13984,#9079,.T.);
#17951=EDGE_CURVE('',#13981,#13984,#9080,.T.);
#17952=EDGE_CURVE('',#13984,#13979,#1673,.T.);
#17953=EDGE_CURVE('',#13985,#13986,#9081,.T.);
#17954=EDGE_CURVE('',#13985,#13987,#9082,.T.);
#17955=EDGE_CURVE('',#13988,#13987,#9083,.T.);
#17956=EDGE_CURVE('',#13986,#13988,#9084,.T.);
#17957=EDGE_CURVE('',#13986,#13989,#1674,.T.);
#17958=EDGE_CURVE('',#13988,#13989,#9085,.T.);
#17959=EDGE_CURVE('',#13989,#13990,#9086,.T.);
#17960=EDGE_CURVE('',#13987,#13990,#9087,.T.);
#17961=EDGE_CURVE('',#13990,#13985,#1675,.T.);
#17962=EDGE_CURVE('',#13991,#13992,#9088,.T.);
#17963=EDGE_CURVE('',#13991,#13993,#9089,.T.);
#17964=EDGE_CURVE('',#13994,#13993,#9090,.T.);
#17965=EDGE_CURVE('',#13992,#13994,#9091,.T.);
#17966=EDGE_CURVE('',#13992,#13995,#1676,.T.);
#17967=EDGE_CURVE('',#13994,#13995,#9092,.T.);
#17968=EDGE_CURVE('',#13995,#13996,#9093,.T.);
#17969=EDGE_CURVE('',#13993,#13996,#9094,.T.);
#17970=EDGE_CURVE('',#13996,#13991,#1677,.T.);
#17971=EDGE_CURVE('',#13997,#13998,#9095,.T.);
#17972=EDGE_CURVE('',#13997,#13999,#9096,.T.);
#17973=EDGE_CURVE('',#14000,#13999,#9097,.T.);
#17974=EDGE_CURVE('',#13998,#14000,#9098,.T.);
#17975=EDGE_CURVE('',#13998,#14001,#1678,.T.);
#17976=EDGE_CURVE('',#14000,#14001,#9099,.T.);
#17977=EDGE_CURVE('',#14001,#14002,#9100,.T.);
#17978=EDGE_CURVE('',#13999,#14002,#9101,.T.);
#17979=EDGE_CURVE('',#14002,#13997,#1679,.T.);
#17980=EDGE_CURVE('',#14003,#14004,#9102,.T.);
#17981=EDGE_CURVE('',#14003,#14005,#9103,.T.);
#17982=EDGE_CURVE('',#14006,#14005,#9104,.T.);
#17983=EDGE_CURVE('',#14004,#14006,#9105,.T.);
#17984=EDGE_CURVE('',#14004,#14007,#1680,.T.);
#17985=EDGE_CURVE('',#14006,#14008,#9106,.T.);
#17986=EDGE_CURVE('',#14007,#14008,#1681,.T.);
#17987=EDGE_CURVE('',#14008,#14009,#9107,.T.);
#17988=EDGE_CURVE('',#14005,#14009,#9108,.T.);
#17989=EDGE_CURVE('',#14009,#14010,#1682,.T.);
#17990=EDGE_CURVE('',#14010,#14003,#1683,.T.);
#17991=EDGE_CURVE('',#14011,#14012,#9109,.T.);
#17992=EDGE_CURVE('',#14011,#14013,#9110,.T.);
#17993=EDGE_CURVE('',#14014,#14013,#9111,.T.);
#17994=EDGE_CURVE('',#14012,#14014,#9112,.T.);
#17995=EDGE_CURVE('',#14012,#14015,#1684,.T.);
#17996=EDGE_CURVE('',#14014,#14015,#9113,.T.);
#17997=EDGE_CURVE('',#14015,#14016,#9114,.T.);
#17998=EDGE_CURVE('',#14013,#14016,#9115,.T.);
#17999=EDGE_CURVE('',#14016,#14011,#1685,.T.);
#18000=EDGE_CURVE('',#14017,#14018,#9116,.T.);
#18001=EDGE_CURVE('',#14017,#14019,#9117,.T.);
#18002=EDGE_CURVE('',#14020,#14019,#9118,.T.);
#18003=EDGE_CURVE('',#14018,#14020,#9119,.T.);
#18004=EDGE_CURVE('',#14018,#14021,#1686,.T.);
#18005=EDGE_CURVE('',#14020,#14021,#9120,.T.);
#18006=EDGE_CURVE('',#14021,#14022,#9121,.T.);
#18007=EDGE_CURVE('',#14019,#14022,#9122,.T.);
#18008=EDGE_CURVE('',#14022,#14017,#1687,.T.);
#18009=EDGE_CURVE('',#14023,#14024,#9123,.T.);
#18010=EDGE_CURVE('',#14023,#14025,#9124,.T.);
#18011=EDGE_CURVE('',#14026,#14025,#9125,.T.);
#18012=EDGE_CURVE('',#14024,#14026,#9126,.T.);
#18013=EDGE_CURVE('',#14024,#14027,#1688,.T.);
#18014=EDGE_CURVE('',#14026,#14027,#9127,.T.);
#18015=EDGE_CURVE('',#14027,#14028,#9128,.T.);
#18016=EDGE_CURVE('',#14025,#14028,#9129,.T.);
#18017=EDGE_CURVE('',#14028,#14023,#1689,.T.);
#18018=EDGE_CURVE('',#14029,#14030,#9130,.T.);
#18019=EDGE_CURVE('',#14029,#14031,#9131,.T.);
#18020=EDGE_CURVE('',#14032,#14031,#9132,.T.);
#18021=EDGE_CURVE('',#14030,#14032,#9133,.T.);
#18022=EDGE_CURVE('',#14030,#14033,#1690,.T.);
#18023=EDGE_CURVE('',#14032,#14033,#9134,.T.);
#18024=EDGE_CURVE('',#14033,#14034,#9135,.T.);
#18025=EDGE_CURVE('',#14031,#14034,#9136,.T.);
#18026=EDGE_CURVE('',#14034,#14029,#1691,.T.);
#18027=EDGE_CURVE('',#14035,#14036,#9137,.T.);
#18028=EDGE_CURVE('',#14035,#14037,#9138,.T.);
#18029=EDGE_CURVE('',#14038,#14037,#9139,.T.);
#18030=EDGE_CURVE('',#14036,#14038,#9140,.T.);
#18031=EDGE_CURVE('',#14036,#14039,#1692,.T.);
#18032=EDGE_CURVE('',#14038,#14039,#9141,.T.);
#18033=EDGE_CURVE('',#14039,#14040,#9142,.T.);
#18034=EDGE_CURVE('',#14037,#14040,#9143,.T.);
#18035=EDGE_CURVE('',#14040,#14035,#1693,.T.);
#18036=EDGE_CURVE('',#14041,#14042,#9144,.T.);
#18037=EDGE_CURVE('',#14041,#14043,#9145,.T.);
#18038=EDGE_CURVE('',#14044,#14043,#9146,.T.);
#18039=EDGE_CURVE('',#14042,#14044,#9147,.T.);
#18040=EDGE_CURVE('',#14042,#14045,#1694,.T.);
#18041=EDGE_CURVE('',#14044,#14045,#9148,.T.);
#18042=EDGE_CURVE('',#14045,#14046,#9149,.T.);
#18043=EDGE_CURVE('',#14043,#14046,#9150,.T.);
#18044=EDGE_CURVE('',#14046,#14041,#1695,.T.);
#18045=EDGE_CURVE('',#14047,#14048,#9151,.T.);
#18046=EDGE_CURVE('',#14047,#14049,#9152,.T.);
#18047=EDGE_CURVE('',#14050,#14049,#9153,.T.);
#18048=EDGE_CURVE('',#14048,#14050,#9154,.T.);
#18049=EDGE_CURVE('',#14048,#14051,#1696,.T.);
#18050=EDGE_CURVE('',#14050,#14051,#9155,.T.);
#18051=EDGE_CURVE('',#14051,#14052,#9156,.T.);
#18052=EDGE_CURVE('',#14049,#14052,#9157,.T.);
#18053=EDGE_CURVE('',#14052,#14047,#1697,.T.);
#18054=EDGE_CURVE('',#14053,#14054,#9158,.T.);
#18055=EDGE_CURVE('',#14053,#14055,#9159,.T.);
#18056=EDGE_CURVE('',#14056,#14055,#9160,.T.);
#18057=EDGE_CURVE('',#14054,#14056,#9161,.T.);
#18058=EDGE_CURVE('',#14054,#14057,#1698,.T.);
#18059=EDGE_CURVE('',#14056,#14057,#9162,.T.);
#18060=EDGE_CURVE('',#14057,#14058,#9163,.T.);
#18061=EDGE_CURVE('',#14055,#14058,#9164,.T.);
#18062=EDGE_CURVE('',#14058,#14053,#1699,.T.);
#18063=EDGE_CURVE('',#14059,#14060,#9165,.T.);
#18064=EDGE_CURVE('',#14059,#14061,#9166,.T.);
#18065=EDGE_CURVE('',#14062,#14061,#9167,.T.);
#18066=EDGE_CURVE('',#14060,#14062,#9168,.T.);
#18067=EDGE_CURVE('',#14060,#14063,#1700,.T.);
#18068=EDGE_CURVE('',#14062,#14063,#9169,.T.);
#18069=EDGE_CURVE('',#14063,#14064,#9170,.T.);
#18070=EDGE_CURVE('',#14061,#14064,#9171,.T.);
#18071=EDGE_CURVE('',#14064,#14059,#1701,.T.);
#18072=EDGE_CURVE('',#14065,#14066,#9172,.T.);
#18073=EDGE_CURVE('',#14065,#14067,#9173,.T.);
#18074=EDGE_CURVE('',#14068,#14067,#9174,.T.);
#18075=EDGE_CURVE('',#14066,#14068,#9175,.T.);
#18076=EDGE_CURVE('',#14066,#14069,#1702,.T.);
#18077=EDGE_CURVE('',#14068,#14069,#9176,.T.);
#18078=EDGE_CURVE('',#14069,#14070,#9177,.T.);
#18079=EDGE_CURVE('',#14067,#14070,#9178,.T.);
#18080=EDGE_CURVE('',#14070,#14065,#1703,.T.);
#18081=EDGE_CURVE('',#14071,#14072,#9179,.T.);
#18082=EDGE_CURVE('',#14071,#14073,#9180,.T.);
#18083=EDGE_CURVE('',#14074,#14073,#9181,.T.);
#18084=EDGE_CURVE('',#14072,#14074,#9182,.T.);
#18085=EDGE_CURVE('',#14072,#14075,#1704,.T.);
#18086=EDGE_CURVE('',#14074,#14075,#9183,.T.);
#18087=EDGE_CURVE('',#14075,#14076,#9184,.T.);
#18088=EDGE_CURVE('',#14073,#14076,#9185,.T.);
#18089=EDGE_CURVE('',#14076,#14071,#1705,.T.);
#18090=EDGE_CURVE('',#14077,#14078,#9186,.T.);
#18091=EDGE_CURVE('',#14077,#14079,#9187,.T.);
#18092=EDGE_CURVE('',#14080,#14079,#9188,.T.);
#18093=EDGE_CURVE('',#14078,#14080,#9189,.T.);
#18094=EDGE_CURVE('',#14078,#14081,#1706,.T.);
#18095=EDGE_CURVE('',#14080,#14081,#9190,.T.);
#18096=EDGE_CURVE('',#14081,#14082,#9191,.T.);
#18097=EDGE_CURVE('',#14079,#14082,#9192,.T.);
#18098=EDGE_CURVE('',#14082,#14077,#1707,.T.);
#18099=EDGE_CURVE('',#14083,#14084,#9193,.T.);
#18100=EDGE_CURVE('',#14083,#14085,#9194,.T.);
#18101=EDGE_CURVE('',#14086,#14085,#9195,.T.);
#18102=EDGE_CURVE('',#14084,#14086,#9196,.T.);
#18103=EDGE_CURVE('',#14084,#14087,#1708,.T.);
#18104=EDGE_CURVE('',#14086,#14087,#9197,.T.);
#18105=EDGE_CURVE('',#14087,#14088,#9198,.T.);
#18106=EDGE_CURVE('',#14085,#14088,#9199,.T.);
#18107=EDGE_CURVE('',#14088,#14083,#1709,.T.);
#18108=EDGE_CURVE('',#14089,#14090,#9200,.T.);
#18109=EDGE_CURVE('',#14089,#14091,#9201,.T.);
#18110=EDGE_CURVE('',#14092,#14091,#9202,.T.);
#18111=EDGE_CURVE('',#14090,#14092,#9203,.T.);
#18112=EDGE_CURVE('',#14090,#14093,#1710,.T.);
#18113=EDGE_CURVE('',#14092,#14093,#9204,.T.);
#18114=EDGE_CURVE('',#14093,#14094,#9205,.T.);
#18115=EDGE_CURVE('',#14091,#14094,#9206,.T.);
#18116=EDGE_CURVE('',#14094,#14089,#1711,.T.);
#18117=EDGE_CURVE('',#14095,#14096,#9207,.T.);
#18118=EDGE_CURVE('',#14095,#14097,#9208,.T.);
#18119=EDGE_CURVE('',#14098,#14097,#9209,.T.);
#18120=EDGE_CURVE('',#14096,#14098,#9210,.T.);
#18121=EDGE_CURVE('',#14096,#14099,#1712,.T.);
#18122=EDGE_CURVE('',#14098,#14099,#9211,.T.);
#18123=EDGE_CURVE('',#14099,#14100,#9212,.T.);
#18124=EDGE_CURVE('',#14097,#14100,#9213,.T.);
#18125=EDGE_CURVE('',#14100,#14095,#1713,.T.);
#18126=EDGE_CURVE('',#14101,#14102,#9214,.T.);
#18127=EDGE_CURVE('',#14101,#14103,#9215,.T.);
#18128=EDGE_CURVE('',#14104,#14103,#9216,.T.);
#18129=EDGE_CURVE('',#14102,#14104,#9217,.T.);
#18130=EDGE_CURVE('',#14102,#14105,#1714,.T.);
#18131=EDGE_CURVE('',#14104,#14105,#9218,.T.);
#18132=EDGE_CURVE('',#14105,#14106,#9219,.T.);
#18133=EDGE_CURVE('',#14103,#14106,#9220,.T.);
#18134=EDGE_CURVE('',#14106,#14101,#1715,.T.);
#18135=EDGE_CURVE('',#14107,#14108,#9221,.T.);
#18136=EDGE_CURVE('',#14107,#14109,#9222,.T.);
#18137=EDGE_CURVE('',#14110,#14109,#9223,.T.);
#18138=EDGE_CURVE('',#14108,#14110,#9224,.T.);
#18139=EDGE_CURVE('',#14108,#14111,#1716,.T.);
#18140=EDGE_CURVE('',#14110,#14111,#9225,.T.);
#18141=EDGE_CURVE('',#14111,#14112,#9226,.T.);
#18142=EDGE_CURVE('',#14109,#14112,#9227,.T.);
#18143=EDGE_CURVE('',#14112,#14107,#1717,.T.);
#18144=EDGE_CURVE('',#14113,#14114,#9228,.T.);
#18145=EDGE_CURVE('',#14113,#14115,#9229,.T.);
#18146=EDGE_CURVE('',#14116,#14115,#9230,.T.);
#18147=EDGE_CURVE('',#14114,#14116,#9231,.T.);
#18148=EDGE_CURVE('',#14114,#14117,#1718,.T.);
#18149=EDGE_CURVE('',#14116,#14117,#9232,.T.);
#18150=EDGE_CURVE('',#14117,#14118,#9233,.T.);
#18151=EDGE_CURVE('',#14115,#14118,#9234,.T.);
#18152=EDGE_CURVE('',#14118,#14113,#1719,.T.);
#18153=EDGE_CURVE('',#14119,#14120,#9235,.T.);
#18154=EDGE_CURVE('',#14120,#14120,#1720,.T.);
#18155=EDGE_CURVE('',#14121,#14122,#9236,.T.);
#18156=EDGE_CURVE('',#14121,#14123,#9237,.T.);
#18157=EDGE_CURVE('',#14123,#14124,#9238,.T.);
#18158=EDGE_CURVE('',#14122,#14124,#9239,.T.);
#18159=EDGE_CURVE('',#14125,#14121,#9240,.T.);
#18160=EDGE_CURVE('',#14125,#14126,#9241,.T.);
#18161=EDGE_CURVE('',#14126,#14123,#9242,.T.);
#18162=EDGE_CURVE('',#14127,#14125,#9243,.T.);
#18163=EDGE_CURVE('',#14127,#14128,#9244,.T.);
#18164=EDGE_CURVE('',#14128,#14126,#9245,.T.);
#18165=EDGE_CURVE('',#14129,#14127,#9246,.T.);
#18166=EDGE_CURVE('',#14129,#14130,#9247,.T.);
#18167=EDGE_CURVE('',#14130,#14128,#9248,.T.);
#18168=EDGE_CURVE('',#14131,#14129,#9249,.T.);
#18169=EDGE_CURVE('',#14131,#14132,#9250,.T.);
#18170=EDGE_CURVE('',#14132,#14130,#9251,.T.);
#18171=EDGE_CURVE('',#14122,#14131,#9252,.T.);
#18172=EDGE_CURVE('',#14124,#14132,#9253,.T.);
#18173=EDGE_CURVE('',#14133,#14133,#1721,.T.);
#18174=EDGE_CURVE('',#13897,#14133,#9254,.T.);
#18175=EDGE_CURVE('',#14134,#14134,#1722,.T.);
#18176=EDGE_CURVE('',#14134,#14010,#9255,.T.);
#18177=EDGE_CURVE('',#14007,#13900,#9256,.T.);
#18178=EDGE_CURVE('',#14135,#14135,#1723,.T.);
#18179=EDGE_CURVE('',#14135,#14134,#9257,.T.);
#18180=EDGE_CURVE('',#14136,#14137,#9258,.F.);
#18181=EDGE_CURVE('',#14137,#14138,#9259,.T.);
#18182=EDGE_CURVE('',#14138,#14139,#9260,.F.);
#18183=EDGE_CURVE('',#14139,#14136,#9261,.T.);
#18184=EDGE_CURVE('',#14140,#14137,#9262,.T.);
#18185=EDGE_CURVE('',#14141,#14140,#9263,.T.);
#18186=EDGE_CURVE('',#14141,#14138,#9264,.T.);
#18187=EDGE_CURVE('',#14142,#14143,#170,.T.);
#18188=EDGE_CURVE('',#14143,#14144,#9265,.T.);
#18189=EDGE_CURVE('',#14144,#14145,#171,.T.);
#18190=EDGE_CURVE('',#14145,#14142,#9266,.T.);
#18191=EDGE_CURVE('',#14146,#14143,#1724,.T.);
#18192=EDGE_CURVE('',#14147,#14146,#9267,.T.);
#18193=EDGE_CURVE('',#14147,#14144,#1725,.T.);
#18194=EDGE_CURVE('',#14142,#14148,#172,.T.);
#18195=EDGE_CURVE('',#14149,#14148,#1726,.T.);
#18196=EDGE_CURVE('',#14149,#14150,#173,.T.);
#18197=EDGE_CURVE('',#14146,#14150,#174,.T.);
#18198=EDGE_CURVE('',#14151,#14152,#175,.T.);
#18199=EDGE_CURVE('',#14152,#14153,#9268,.T.);
#18200=EDGE_CURVE('',#14153,#14154,#176,.T.);
#18201=EDGE_CURVE('',#14154,#14151,#9269,.T.);
#18202=EDGE_CURVE('',#14155,#14154,#177,.T.);
#18203=EDGE_CURVE('',#14139,#14155,#9270,.T.);
#18204=EDGE_CURVE('',#14156,#14141,#9271,.F.);
#18205=EDGE_CURVE('',#14157,#14156,#9272,.T.);
#18206=EDGE_CURVE('',#14151,#14157,#178,.T.);
#18207=EDGE_CURVE('',#14153,#14158,#1727,.T.);
#18208=EDGE_CURVE('',#14159,#14158,#179,.T.);
#18209=EDGE_CURVE('',#14159,#14160,#180,.T.);
#18210=EDGE_CURVE('',#14155,#14160,#1728,.T.);
#18211=EDGE_CURVE('',#14161,#14162,#9273,.F.);
#18212=EDGE_CURVE('',#14162,#14163,#9274,.T.);
#18213=EDGE_CURVE('',#14163,#14164,#9275,.F.);
#18214=EDGE_CURVE('',#14164,#14161,#9276,.T.);
#18215=EDGE_CURVE('',#14165,#14162,#9277,.T.);
#18216=EDGE_CURVE('',#14166,#14165,#9278,.T.);
#18217=EDGE_CURVE('',#14166,#14163,#9279,.T.);
#18218=EDGE_CURVE('',#14158,#14167,#9280,.T.);
#18219=EDGE_CURVE('',#14167,#14168,#181,.T.);
#18220=EDGE_CURVE('',#14168,#14159,#9281,.T.);
#18221=EDGE_CURVE('',#14169,#14168,#182,.T.);
#18222=EDGE_CURVE('',#14170,#14169,#9282,.T.);
#18223=EDGE_CURVE('',#14165,#14170,#9283,.F.);
#18224=EDGE_CURVE('',#14160,#14161,#9284,.T.);
#18225=EDGE_CURVE('',#14171,#14172,#183,.T.);
#18226=EDGE_CURVE('',#14172,#14173,#9285,.T.);
#18227=EDGE_CURVE('',#14173,#14174,#184,.T.);
#18228=EDGE_CURVE('',#14174,#14171,#9286,.T.);
#18229=EDGE_CURVE('',#14172,#14175,#1729,.T.);
#18230=EDGE_CURVE('',#14176,#14175,#9287,.T.);
#18231=EDGE_CURVE('',#14173,#14176,#1730,.T.);
#18232=EDGE_CURVE('',#14171,#14177,#185,.T.);
#18233=EDGE_CURVE('',#14177,#14178,#1731,.T.);
#18234=EDGE_CURVE('',#14178,#14179,#186,.T.);
#18235=EDGE_CURVE('',#14175,#14179,#187,.T.);
#18236=EDGE_CURVE('',#14180,#14181,#9288,.F.);
#18237=EDGE_CURVE('',#14181,#14182,#9289,.T.);
#18238=EDGE_CURVE('',#14182,#14183,#9290,.F.);
#18239=EDGE_CURVE('',#14183,#14180,#9291,.T.);
#18240=EDGE_CURVE('',#14184,#14181,#9292,.T.);
#18241=EDGE_CURVE('',#14185,#14184,#9293,.T.);
#18242=EDGE_CURVE('',#14185,#14182,#9294,.T.);
#18243=EDGE_CURVE('',#14186,#14176,#188,.T.);
#18244=EDGE_CURVE('',#14179,#14186,#9295,.T.);
#18245=EDGE_CURVE('',#14186,#14187,#189,.T.);
#18246=EDGE_CURVE('',#14188,#14187,#1732,.T.);
#18247=EDGE_CURVE('',#14188,#14174,#190,.T.);
#18248=EDGE_CURVE('',#14189,#14178,#9296,.T.);
#18249=EDGE_CURVE('',#14184,#14189,#9297,.F.);
#18250=EDGE_CURVE('',#14187,#14180,#9298,.T.);
#18251=EDGE_CURVE('',#14190,#14191,#191,.T.);
#18252=EDGE_CURVE('',#14191,#14192,#9299,.T.);
#18253=EDGE_CURVE('',#14192,#14193,#192,.T.);
#18254=EDGE_CURVE('',#14193,#14190,#9300,.T.);
#18255=EDGE_CURVE('',#14191,#14194,#1733,.T.);
#18256=EDGE_CURVE('',#14195,#14194,#9301,.T.);
#18257=EDGE_CURVE('',#14192,#14195,#1734,.T.);
#18258=EDGE_CURVE('',#14190,#14196,#193,.T.);
#18259=EDGE_CURVE('',#14196,#14197,#1735,.T.);
#18260=EDGE_CURVE('',#14197,#14198,#194,.T.);
#18261=EDGE_CURVE('',#14194,#14198,#195,.T.);
#18262=EDGE_CURVE('',#14140,#14199,#9302,.F.);
#18263=EDGE_CURVE('',#14199,#14156,#9303,.T.);
#18264=EDGE_CURVE('',#14200,#14166,#9304,.F.);
#18265=EDGE_CURVE('',#14170,#14200,#9305,.T.);
#18266=EDGE_CURVE('',#14201,#14185,#9306,.F.);
#18267=EDGE_CURVE('',#14189,#14201,#9307,.T.);
#18268=EDGE_CURVE('',#14202,#14203,#9308,.F.);
#18269=EDGE_CURVE('',#14203,#14204,#9309,.T.);
#18270=EDGE_CURVE('',#14204,#14205,#9310,.F.);
#18271=EDGE_CURVE('',#14205,#14202,#9311,.T.);
#18272=EDGE_CURVE('',#14206,#14203,#9312,.T.);
#18273=EDGE_CURVE('',#14207,#14206,#9313,.T.);
#18274=EDGE_CURVE('',#14207,#14204,#9314,.T.);
#18275=EDGE_CURVE('',#14208,#14207,#9315,.F.);
#18276=EDGE_CURVE('',#14206,#14209,#9316,.F.);
#18277=EDGE_CURVE('',#14209,#14208,#9317,.T.);
#18278=EDGE_CURVE('',#14210,#14147,#196,.T.);
#18279=EDGE_CURVE('',#14150,#14210,#9318,.T.);
#18280=EDGE_CURVE('',#14210,#14211,#197,.T.);
#18281=EDGE_CURVE('',#14211,#14212,#1736,.T.);
#18282=EDGE_CURVE('',#14212,#14145,#198,.T.);
#18283=EDGE_CURVE('',#14205,#14149,#9319,.T.);
#18284=EDGE_CURVE('',#14211,#14208,#9320,.T.);
#18285=EDGE_CURVE('',#14213,#14195,#199,.T.);
#18286=EDGE_CURVE('',#14198,#14213,#9321,.T.);
#18287=EDGE_CURVE('',#14213,#14214,#200,.T.);
#18288=EDGE_CURVE('',#14215,#14214,#1737,.T.);
#18289=EDGE_CURVE('',#14215,#14193,#201,.T.);
#18290=EDGE_CURVE('',#14209,#14197,#9322,.T.);
#18291=EDGE_CURVE('',#14214,#14202,#9323,.T.);
#18292=EDGE_CURVE('',#14199,#14212,#9324,.T.);
#18293=EDGE_CURVE('',#14196,#14201,#9325,.T.);
#18294=EDGE_CURVE('',#14177,#14200,#9326,.T.);
#18295=EDGE_CURVE('',#14157,#14169,#1738,.T.);
#18296=EDGE_CURVE('',#14216,#14216,#1739,.T.);
#18297=EDGE_CURVE('',#14183,#14215,#9327,.T.);
#18298=EDGE_CURVE('',#14164,#14188,#9328,.T.);
#18299=EDGE_CURVE('',#14152,#14167,#1740,.T.);
#18300=EDGE_CURVE('',#14148,#14136,#9329,.T.);
#18301=EDGE_CURVE('',#14217,#14217,#1741,.T.);
#18302=EDGE_CURVE('',#14217,#14216,#9330,.T.);
#18303=EDGE_CURVE('',#14218,#14219,#9331,.T.);
#18304=EDGE_CURVE('',#14218,#14220,#2835,.T.);
#18305=EDGE_CURVE('',#14220,#14221,#1742,.T.);
#18306=EDGE_CURVE('',#14221,#14219,#2836,.T.);
#18307=EDGE_CURVE('',#14222,#14223,#9332,.T.);
#18308=EDGE_CURVE('',#14222,#14218,#2837,.T.);
#18309=EDGE_CURVE('',#14219,#14223,#2838,.T.);
#18310=EDGE_CURVE('',#14224,#14225,#9333,.T.);
#18311=EDGE_CURVE('',#14224,#14222,#2839,.T.);
#18312=EDGE_CURVE('',#14223,#14225,#2840,.T.);
#18313=EDGE_CURVE('',#14226,#14227,#9334,.T.);
#18314=EDGE_CURVE('',#14226,#14224,#2841,.T.);
#18315=EDGE_CURVE('',#14225,#14227,#2842,.T.);
#18316=EDGE_CURVE('',#14228,#14229,#9335,.T.);
#18317=EDGE_CURVE('',#14228,#14226,#2843,.T.);
#18318=EDGE_CURVE('',#14227,#14229,#2844,.T.);
#18319=EDGE_CURVE('',#14230,#14231,#9336,.T.);
#18320=EDGE_CURVE('',#14230,#14228,#2845,.T.);
#18321=EDGE_CURVE('',#14229,#14231,#2846,.T.);
#18322=EDGE_CURVE('',#14232,#14233,#9337,.T.);
#18323=EDGE_CURVE('',#14232,#14230,#2847,.T.);
#18324=EDGE_CURVE('',#14231,#14233,#2848,.T.);
#18325=EDGE_CURVE('',#14234,#14235,#9338,.T.);
#18326=EDGE_CURVE('',#14234,#14232,#2849,.T.);
#18327=EDGE_CURVE('',#14233,#14235,#2850,.T.);
#18328=EDGE_CURVE('',#14236,#14237,#9339,.T.);
#18329=EDGE_CURVE('',#14236,#14234,#2851,.T.);
#18330=EDGE_CURVE('',#14235,#14237,#2852,.T.);
#18331=EDGE_CURVE('',#14238,#14239,#9340,.T.);
#18332=EDGE_CURVE('',#14238,#14236,#2853,.T.);
#18333=EDGE_CURVE('',#14237,#14239,#2854,.T.);
#18334=EDGE_CURVE('',#14240,#14241,#9341,.T.);
#18335=EDGE_CURVE('',#14240,#14238,#2855,.T.);
#18336=EDGE_CURVE('',#14239,#14241,#2856,.T.);
#18337=EDGE_CURVE('',#14242,#14243,#9342,.T.);
#18338=EDGE_CURVE('',#14242,#14240,#2857,.T.);
#18339=EDGE_CURVE('',#14241,#14243,#2858,.T.);
#18340=EDGE_CURVE('',#14244,#14245,#9343,.T.);
#18341=EDGE_CURVE('',#14244,#14242,#2859,.T.);
#18342=EDGE_CURVE('',#14243,#14245,#2860,.T.);
#18343=EDGE_CURVE('',#14246,#14247,#9344,.T.);
#18344=EDGE_CURVE('',#14246,#14244,#2861,.T.);
#18345=EDGE_CURVE('',#14245,#14247,#2862,.T.);
#18346=EDGE_CURVE('',#14248,#14249,#9345,.T.);
#18347=EDGE_CURVE('',#14248,#14246,#2863,.T.);
#18348=EDGE_CURVE('',#14247,#14249,#2864,.T.);
#18349=EDGE_CURVE('',#14250,#14251,#9346,.T.);
#18350=EDGE_CURVE('',#14250,#14248,#2865,.T.);
#18351=EDGE_CURVE('',#14249,#14251,#2866,.T.);
#18352=EDGE_CURVE('',#14252,#14253,#9347,.T.);
#18353=EDGE_CURVE('',#14252,#14254,#2867,.T.);
#18354=EDGE_CURVE('',#14253,#14254,#1743,.T.);
#18355=EDGE_CURVE('',#14255,#14256,#9348,.T.);
#18356=EDGE_CURVE('',#14255,#14252,#2868,.T.);
#18357=EDGE_CURVE('',#14257,#14253,#1744,.T.);
#18358=EDGE_CURVE('',#14256,#14257,#2869,.T.);
#18359=EDGE_CURVE('',#14258,#14259,#9349,.T.);
#18360=EDGE_CURVE('',#14258,#14255,#2870,.T.);
#18361=EDGE_CURVE('',#14259,#14256,#2871,.T.);
#18362=EDGE_CURVE('',#14260,#14261,#9350,.T.);
#18363=EDGE_CURVE('',#14260,#14258,#2872,.T.);
#18364=EDGE_CURVE('',#14261,#14259,#2873,.T.);
#18365=EDGE_CURVE('',#14262,#14263,#9351,.T.);
#18366=EDGE_CURVE('',#14262,#14260,#2874,.T.);
#18367=EDGE_CURVE('',#14263,#14261,#2875,.T.);
#18368=EDGE_CURVE('',#14264,#14265,#9352,.T.);
#18369=EDGE_CURVE('',#14264,#14262,#2876,.T.);
#18370=EDGE_CURVE('',#14265,#14263,#2877,.T.);
#18371=EDGE_CURVE('',#14266,#14267,#9353,.T.);
#18372=EDGE_CURVE('',#14266,#14264,#2878,.T.);
#18373=EDGE_CURVE('',#14267,#14265,#2879,.T.);
#18374=EDGE_CURVE('',#14268,#14269,#9354,.T.);
#18375=EDGE_CURVE('',#14268,#14266,#2880,.T.);
#18376=EDGE_CURVE('',#14269,#14267,#2881,.T.);
#18377=EDGE_CURVE('',#14270,#14271,#9355,.T.);
#18378=EDGE_CURVE('',#14270,#14268,#2882,.T.);
#18379=EDGE_CURVE('',#14271,#14269,#2883,.T.);
#18380=EDGE_CURVE('',#14272,#14273,#9356,.T.);
#18381=EDGE_CURVE('',#14272,#14270,#2884,.T.);
#18382=EDGE_CURVE('',#14273,#14271,#2885,.T.);
#18383=EDGE_CURVE('',#14274,#14275,#9357,.T.);
#18384=EDGE_CURVE('',#14274,#14272,#2886,.T.);
#18385=EDGE_CURVE('',#14275,#14273,#2887,.T.);
#18386=EDGE_CURVE('',#14276,#14277,#9358,.T.);
#18387=EDGE_CURVE('',#14276,#14274,#2888,.T.);
#18388=EDGE_CURVE('',#14277,#14275,#2889,.T.);
#18389=EDGE_CURVE('',#14278,#14279,#9359,.T.);
#18390=EDGE_CURVE('',#14278,#14276,#2890,.T.);
#18391=EDGE_CURVE('',#14279,#14277,#2891,.T.);
#18392=EDGE_CURVE('',#14280,#14281,#9360,.T.);
#18393=EDGE_CURVE('',#14280,#14278,#2892,.T.);
#18394=EDGE_CURVE('',#14281,#14279,#2893,.T.);
#18395=EDGE_CURVE('',#14282,#14283,#9361,.T.);
#18396=EDGE_CURVE('',#14282,#14280,#2894,.T.);
#18397=EDGE_CURVE('',#14283,#14281,#2895,.T.);
#18398=EDGE_CURVE('',#14284,#14285,#9362,.T.);
#18399=EDGE_CURVE('',#14284,#14282,#2896,.T.);
#18400=EDGE_CURVE('',#14285,#14283,#2897,.T.);
#18401=EDGE_CURVE('',#14286,#14286,#1745,.T.);
#18402=EDGE_CURVE('',#14286,#14287,#9363,.T.);
#18403=EDGE_CURVE('',#14287,#14288,#1746,.T.);
#18404=EDGE_CURVE('',#14288,#14287,#1747,.T.);
#18405=EDGE_CURVE('',#14289,#14290,#1748,.T.);
#18406=EDGE_CURVE('',#14290,#14289,#1749,.T.);
#18407=EDGE_CURVE('',#14290,#14288,#9364,.T.);
#18408=EDGE_CURVE('',#14291,#14292,#2898,.T.);
#18409=EDGE_CURVE('',#14292,#14293,#2899,.T.);
#18410=EDGE_CURVE('',#14293,#14294,#9365,.T.);
#18411=EDGE_CURVE('',#14294,#14295,#2900,.T.);
#18412=EDGE_CURVE('',#14295,#14291,#9366,.T.);
#18413=EDGE_CURVE('',#14296,#14296,#1750,.T.);
#18414=EDGE_CURVE('',#14289,#14297,#9367,.T.);
#18415=EDGE_CURVE('',#14297,#14297,#1751,.T.);
#18416=EDGE_CURVE('',#14298,#14298,#1752,.T.);
#18417=EDGE_CURVE('',#14299,#14300,#9368,.T.);
#18418=EDGE_CURVE('',#14300,#14301,#2901,.T.);
#18419=EDGE_CURVE('',#14301,#14300,#2902,.T.);
#18420=EDGE_CURVE('',#14299,#14299,#2903,.T.);
#18421=EDGE_CURVE('',#14301,#14292,#9369,.T.);
#18422=EDGE_CURVE('',#14291,#14295,#1753,.T.);
#18423=EDGE_CURVE('',#14294,#14293,#1754,.T.);
#18424=EDGE_CURVE('',#14302,#14302,#1755,.T.);
#18425=EDGE_CURVE('',#14302,#14303,#9370,.T.);
#18426=EDGE_CURVE('',#14303,#14303,#1756,.T.);
#18427=EDGE_CURVE('',#14304,#14257,#2904,.T.);
#18428=EDGE_CURVE('',#14251,#14304,#2905,.T.);
#18429=EDGE_CURVE('',#14305,#14221,#2906,.T.);
#18430=EDGE_CURVE('',#14305,#14285,#2907,.T.);
#18431=EDGE_CURVE('',#14221,#14306,#1757,.T.);
#18432=EDGE_CURVE('',#14306,#14220,#1758,.T.);
#18433=EDGE_CURVE('',#14220,#14307,#2908,.T.);
#18434=EDGE_CURVE('',#14307,#14305,#1759,.T.);
#18435=EDGE_CURVE('',#14307,#14284,#2909,.T.);
#18436=EDGE_CURVE('',#14254,#14308,#2910,.T.);
#18437=EDGE_CURVE('',#14308,#14250,#2911,.T.);
#18438=EDGE_CURVE('',#14306,#14296,#9371,.T.);
#18439=EDGE_CURVE('',#14308,#14304,#1760,.T.);
#18440=EDGE_CURVE('',#14309,#14309,#1761,.T.);
#18441=EDGE_CURVE('',#14303,#14309,#9372,.T.);
#18442=EDGE_CURVE('',#14310,#14310,#1762,.T.);
#18443=EDGE_CURVE('',#14310,#14302,#9373,.T.);
#18444=EDGE_CURVE('',#14311,#14311,#1763,.T.);
#18445=EDGE_CURVE('',#14312,#14312,#1764,.T.);
#18446=EDGE_CURVE('',#14312,#14311,#9374,.T.);
#18447=EDGE_CURVE('',#14298,#14312,#9375,.T.);
#18448=EDGE_CURVE('',#14313,#14314,#9376,.T.);
#18449=EDGE_CURVE('',#14313,#14315,#2912,.T.);
#18450=EDGE_CURVE('',#14315,#14316,#1765,.T.);
#18451=EDGE_CURVE('',#14316,#14314,#2913,.T.);
#18452=EDGE_CURVE('',#14317,#14318,#9377,.T.);
#18453=EDGE_CURVE('',#14317,#14313,#2914,.T.);
#18454=EDGE_CURVE('',#14314,#14318,#2915,.T.);
#18455=EDGE_CURVE('',#14319,#14320,#9378,.T.);
#18456=EDGE_CURVE('',#14319,#14317,#2916,.T.);
#18457=EDGE_CURVE('',#14318,#14320,#2917,.T.);
#18458=EDGE_CURVE('',#14321,#14322,#9379,.T.);
#18459=EDGE_CURVE('',#14321,#14319,#2918,.T.);
#18460=EDGE_CURVE('',#14320,#14322,#2919,.T.);
#18461=EDGE_CURVE('',#14323,#14324,#9380,.T.);
#18462=EDGE_CURVE('',#14323,#14321,#2920,.T.);
#18463=EDGE_CURVE('',#14322,#14324,#2921,.T.);
#18464=EDGE_CURVE('',#14325,#14326,#9381,.T.);
#18465=EDGE_CURVE('',#14325,#14323,#2922,.T.);
#18466=EDGE_CURVE('',#14324,#14326,#2923,.T.);
#18467=EDGE_CURVE('',#14327,#14328,#9382,.T.);
#18468=EDGE_CURVE('',#14327,#14325,#2924,.T.);
#18469=EDGE_CURVE('',#14326,#14328,#2925,.T.);
#18470=EDGE_CURVE('',#14329,#14330,#9383,.T.);
#18471=EDGE_CURVE('',#14329,#14327,#2926,.T.);
#18472=EDGE_CURVE('',#14328,#14330,#2927,.T.);
#18473=EDGE_CURVE('',#14331,#14332,#9384,.T.);
#18474=EDGE_CURVE('',#14331,#14329,#2928,.T.);
#18475=EDGE_CURVE('',#14330,#14332,#2929,.T.);
#18476=EDGE_CURVE('',#14333,#14334,#9385,.T.);
#18477=EDGE_CURVE('',#14333,#14331,#2930,.T.);
#18478=EDGE_CURVE('',#14332,#14334,#2931,.T.);
#18479=EDGE_CURVE('',#14335,#14336,#9386,.T.);
#18480=EDGE_CURVE('',#14335,#14333,#2932,.T.);
#18481=EDGE_CURVE('',#14334,#14336,#2933,.T.);
#18482=EDGE_CURVE('',#14337,#14338,#9387,.T.);
#18483=EDGE_CURVE('',#14337,#14335,#2934,.T.);
#18484=EDGE_CURVE('',#14336,#14338,#2935,.T.);
#18485=EDGE_CURVE('',#14339,#14340,#9388,.T.);
#18486=EDGE_CURVE('',#14339,#14337,#2936,.T.);
#18487=EDGE_CURVE('',#14338,#14340,#2937,.T.);
#18488=EDGE_CURVE('',#14341,#14342,#9389,.T.);
#18489=EDGE_CURVE('',#14341,#14339,#2938,.T.);
#18490=EDGE_CURVE('',#14340,#14342,#2939,.T.);
#18491=EDGE_CURVE('',#14343,#14344,#9390,.T.);
#18492=EDGE_CURVE('',#14343,#14341,#2940,.T.);
#18493=EDGE_CURVE('',#14342,#14344,#2941,.T.);
#18494=EDGE_CURVE('',#14345,#14346,#9391,.T.);
#18495=EDGE_CURVE('',#14345,#14343,#2942,.T.);
#18496=EDGE_CURVE('',#14344,#14346,#2943,.T.);
#18497=EDGE_CURVE('',#14347,#14348,#9392,.T.);
#18498=EDGE_CURVE('',#14347,#14345,#2944,.T.);
#18499=EDGE_CURVE('',#14346,#14348,#2945,.T.);
#18500=EDGE_CURVE('',#14349,#14350,#9393,.T.);
#18501=EDGE_CURVE('',#14349,#14347,#2946,.T.);
#18502=EDGE_CURVE('',#14348,#14350,#2947,.T.);
#18503=EDGE_CURVE('',#14351,#14352,#9394,.T.);
#18504=EDGE_CURVE('',#14351,#14349,#2948,.T.);
#18505=EDGE_CURVE('',#14350,#14352,#2949,.T.);
#18506=EDGE_CURVE('',#14353,#14354,#9395,.T.);
#18507=EDGE_CURVE('',#14353,#14351,#2950,.T.);
#18508=EDGE_CURVE('',#14352,#14354,#2951,.T.);
#18509=EDGE_CURVE('',#14355,#14356,#9396,.T.);
#18510=EDGE_CURVE('',#14355,#14353,#2952,.T.);
#18511=EDGE_CURVE('',#14354,#14356,#2953,.T.);
#18512=EDGE_CURVE('',#14357,#14358,#9397,.T.);
#18513=EDGE_CURVE('',#14357,#14355,#2954,.T.);
#18514=EDGE_CURVE('',#14356,#14358,#2955,.T.);
#18515=EDGE_CURVE('',#14359,#14360,#9398,.T.);
#18516=EDGE_CURVE('',#14359,#14357,#2956,.T.);
#18517=EDGE_CURVE('',#14358,#14360,#2957,.T.);
#18518=EDGE_CURVE('',#14361,#14362,#9399,.T.);
#18519=EDGE_CURVE('',#14361,#14359,#2958,.T.);
#18520=EDGE_CURVE('',#14360,#14362,#2959,.T.);
#18521=EDGE_CURVE('',#14363,#14364,#9400,.T.);
#18522=EDGE_CURVE('',#14363,#14361,#2960,.T.);
#18523=EDGE_CURVE('',#14362,#14364,#2961,.T.);
#18524=EDGE_CURVE('',#14365,#14366,#9401,.T.);
#18525=EDGE_CURVE('',#14365,#14363,#2962,.T.);
#18526=EDGE_CURVE('',#14364,#14366,#2963,.T.);
#18527=EDGE_CURVE('',#14367,#14368,#9402,.T.);
#18528=EDGE_CURVE('',#14367,#14365,#2964,.T.);
#18529=EDGE_CURVE('',#14366,#14368,#2965,.T.);
#18530=EDGE_CURVE('',#14369,#14370,#9403,.T.);
#18531=EDGE_CURVE('',#14369,#14367,#2966,.T.);
#18532=EDGE_CURVE('',#14368,#14370,#2967,.T.);
#18533=EDGE_CURVE('',#14371,#14372,#9404,.T.);
#18534=EDGE_CURVE('',#14371,#14369,#2968,.T.);
#18535=EDGE_CURVE('',#14370,#14372,#2969,.T.);
#18536=EDGE_CURVE('',#14373,#14374,#9405,.T.);
#18537=EDGE_CURVE('',#14373,#14371,#2970,.T.);
#18538=EDGE_CURVE('',#14372,#14374,#2971,.T.);
#18539=EDGE_CURVE('',#14375,#14376,#9406,.T.);
#18540=EDGE_CURVE('',#14375,#14373,#2972,.T.);
#18541=EDGE_CURVE('',#14374,#14376,#2973,.T.);
#18542=EDGE_CURVE('',#14377,#14378,#9407,.T.);
#18543=EDGE_CURVE('',#14377,#14375,#2974,.T.);
#18544=EDGE_CURVE('',#14376,#14378,#2975,.T.);
#18545=EDGE_CURVE('',#14379,#14380,#9408,.T.);
#18546=EDGE_CURVE('',#14379,#14377,#2976,.T.);
#18547=EDGE_CURVE('',#14378,#14380,#2977,.T.);
#18548=EDGE_CURVE('',#14381,#14382,#9409,.T.);
#18549=EDGE_CURVE('',#14381,#14379,#2978,.T.);
#18550=EDGE_CURVE('',#14380,#14382,#2979,.T.);
#18551=EDGE_CURVE('',#14383,#14384,#9410,.T.);
#18552=EDGE_CURVE('',#14383,#14381,#2980,.T.);
#18553=EDGE_CURVE('',#14382,#14384,#2981,.T.);
#18554=EDGE_CURVE('',#14385,#14386,#9411,.T.);
#18555=EDGE_CURVE('',#14385,#14383,#2982,.T.);
#18556=EDGE_CURVE('',#14384,#14386,#2983,.T.);
#18557=EDGE_CURVE('',#14387,#14388,#9412,.T.);
#18558=EDGE_CURVE('',#14387,#14385,#2984,.T.);
#18559=EDGE_CURVE('',#14386,#14388,#2985,.T.);
#18560=EDGE_CURVE('',#14389,#14390,#9413,.T.);
#18561=EDGE_CURVE('',#14389,#14387,#2986,.T.);
#18562=EDGE_CURVE('',#14388,#14390,#2987,.T.);
#18563=EDGE_CURVE('',#14391,#14392,#9414,.T.);
#18564=EDGE_CURVE('',#14391,#14389,#2988,.T.);
#18565=EDGE_CURVE('',#14390,#14392,#2989,.T.);
#18566=EDGE_CURVE('',#14393,#14394,#9415,.T.);
#18567=EDGE_CURVE('',#14393,#14391,#2990,.T.);
#18568=EDGE_CURVE('',#14392,#14394,#2991,.T.);
#18569=EDGE_CURVE('',#14395,#14396,#9416,.T.);
#18570=EDGE_CURVE('',#14395,#14393,#2992,.T.);
#18571=EDGE_CURVE('',#14394,#14396,#2993,.T.);
#18572=EDGE_CURVE('',#14397,#14398,#9417,.T.);
#18573=EDGE_CURVE('',#14397,#14395,#2994,.T.);
#18574=EDGE_CURVE('',#14396,#14398,#2995,.T.);
#18575=EDGE_CURVE('',#14399,#14400,#9418,.T.);
#18576=EDGE_CURVE('',#14399,#14397,#2996,.T.);
#18577=EDGE_CURVE('',#14398,#14400,#2997,.T.);
#18578=EDGE_CURVE('',#14401,#14402,#9419,.T.);
#18579=EDGE_CURVE('',#14401,#14399,#2998,.T.);
#18580=EDGE_CURVE('',#14400,#14402,#2999,.T.);
#18581=EDGE_CURVE('',#14403,#14404,#9420,.T.);
#18582=EDGE_CURVE('',#14403,#14401,#3000,.T.);
#18583=EDGE_CURVE('',#14402,#14404,#3001,.T.);
#18584=EDGE_CURVE('',#14405,#14406,#9421,.T.);
#18585=EDGE_CURVE('',#14405,#14403,#3002,.T.);
#18586=EDGE_CURVE('',#14404,#14406,#3003,.T.);
#18587=EDGE_CURVE('',#14407,#14408,#9422,.T.);
#18588=EDGE_CURVE('',#14407,#14405,#3004,.T.);
#18589=EDGE_CURVE('',#14406,#14408,#3005,.T.);
#18590=EDGE_CURVE('',#14409,#14410,#9423,.T.);
#18591=EDGE_CURVE('',#14409,#14407,#3006,.T.);
#18592=EDGE_CURVE('',#14408,#14410,#3007,.T.);
#18593=EDGE_CURVE('',#14411,#14412,#9424,.T.);
#18594=EDGE_CURVE('',#14411,#14409,#3008,.T.);
#18595=EDGE_CURVE('',#14410,#14412,#3009,.T.);
#18596=EDGE_CURVE('',#14413,#14414,#9425,.T.);
#18597=EDGE_CURVE('',#14413,#14411,#3010,.T.);
#18598=EDGE_CURVE('',#14412,#14414,#3011,.T.);
#18599=EDGE_CURVE('',#14415,#14416,#9426,.T.);
#18600=EDGE_CURVE('',#14415,#14413,#3012,.T.);
#18601=EDGE_CURVE('',#14414,#14416,#3013,.T.);
#18602=EDGE_CURVE('',#14417,#14418,#9427,.T.);
#18603=EDGE_CURVE('',#14417,#14415,#3014,.T.);
#18604=EDGE_CURVE('',#14416,#14418,#3015,.T.);
#18605=EDGE_CURVE('',#14419,#14420,#9428,.T.);
#18606=EDGE_CURVE('',#14419,#14417,#3016,.T.);
#18607=EDGE_CURVE('',#14418,#14420,#3017,.T.);
#18608=EDGE_CURVE('',#14421,#14422,#9429,.T.);
#18609=EDGE_CURVE('',#14421,#14419,#3018,.T.);
#18610=EDGE_CURVE('',#14420,#14422,#3019,.T.);
#18611=EDGE_CURVE('',#14423,#14424,#9430,.T.);
#18612=EDGE_CURVE('',#14423,#14421,#3020,.T.);
#18613=EDGE_CURVE('',#14422,#14424,#3021,.T.);
#18614=EDGE_CURVE('',#14425,#14426,#9431,.T.);
#18615=EDGE_CURVE('',#14425,#14423,#3022,.T.);
#18616=EDGE_CURVE('',#14424,#14426,#3023,.T.);
#18617=EDGE_CURVE('',#14427,#14428,#9432,.T.);
#18618=EDGE_CURVE('',#14427,#14425,#3024,.T.);
#18619=EDGE_CURVE('',#14426,#14428,#3025,.T.);
#18620=EDGE_CURVE('',#14429,#14430,#9433,.T.);
#18621=EDGE_CURVE('',#14429,#14427,#3026,.T.);
#18622=EDGE_CURVE('',#14428,#14430,#3027,.T.);
#18623=EDGE_CURVE('',#14431,#14432,#9434,.T.);
#18624=EDGE_CURVE('',#14431,#14429,#3028,.T.);
#18625=EDGE_CURVE('',#14430,#14432,#3029,.T.);
#18626=EDGE_CURVE('',#14433,#14434,#9435,.T.);
#18627=EDGE_CURVE('',#14433,#14431,#3030,.T.);
#18628=EDGE_CURVE('',#14432,#14434,#3031,.T.);
#18629=EDGE_CURVE('',#14435,#14436,#9436,.T.);
#18630=EDGE_CURVE('',#14435,#14433,#3032,.T.);
#18631=EDGE_CURVE('',#14434,#14436,#3033,.T.);
#18632=EDGE_CURVE('',#14437,#14438,#9437,.T.);
#18633=EDGE_CURVE('',#14437,#14435,#3034,.T.);
#18634=EDGE_CURVE('',#14436,#14438,#3035,.T.);
#18635=EDGE_CURVE('',#14439,#14440,#9438,.T.);
#18636=EDGE_CURVE('',#14439,#14437,#3036,.T.);
#18637=EDGE_CURVE('',#14438,#14440,#3037,.T.);
#18638=EDGE_CURVE('',#14441,#14442,#9439,.T.);
#18639=EDGE_CURVE('',#14441,#14439,#3038,.T.);
#18640=EDGE_CURVE('',#14440,#14442,#3039,.T.);
#18641=EDGE_CURVE('',#14443,#14444,#9440,.T.);
#18642=EDGE_CURVE('',#14443,#14441,#3040,.T.);
#18643=EDGE_CURVE('',#14442,#14444,#3041,.T.);
#18644=EDGE_CURVE('',#14445,#14446,#9441,.T.);
#18645=EDGE_CURVE('',#14445,#14443,#3042,.T.);
#18646=EDGE_CURVE('',#14444,#14446,#3043,.T.);
#18647=EDGE_CURVE('',#14447,#14448,#9442,.T.);
#18648=EDGE_CURVE('',#14447,#14445,#3044,.T.);
#18649=EDGE_CURVE('',#14446,#14448,#3045,.T.);
#18650=EDGE_CURVE('',#14449,#14450,#9443,.T.);
#18651=EDGE_CURVE('',#14449,#14447,#3046,.T.);
#18652=EDGE_CURVE('',#14448,#14450,#3047,.T.);
#18653=EDGE_CURVE('',#14451,#14452,#9444,.T.);
#18654=EDGE_CURVE('',#14451,#14449,#3048,.T.);
#18655=EDGE_CURVE('',#14450,#14452,#3049,.T.);
#18656=EDGE_CURVE('',#14453,#14454,#9445,.T.);
#18657=EDGE_CURVE('',#14453,#14451,#3050,.T.);
#18658=EDGE_CURVE('',#14452,#14454,#3051,.T.);
#18659=EDGE_CURVE('',#14455,#14456,#9446,.T.);
#18660=EDGE_CURVE('',#14455,#14453,#3052,.T.);
#18661=EDGE_CURVE('',#14454,#14456,#3053,.T.);
#18662=EDGE_CURVE('',#14457,#14458,#9447,.T.);
#18663=EDGE_CURVE('',#14457,#14455,#3054,.T.);
#18664=EDGE_CURVE('',#14456,#14458,#3055,.T.);
#18665=EDGE_CURVE('',#14459,#14460,#9448,.T.);
#18666=EDGE_CURVE('',#14459,#14457,#3056,.T.);
#18667=EDGE_CURVE('',#14458,#14460,#3057,.T.);
#18668=EDGE_CURVE('',#14461,#14462,#9449,.T.);
#18669=EDGE_CURVE('',#14461,#14459,#3058,.T.);
#18670=EDGE_CURVE('',#14460,#14462,#3059,.T.);
#18671=EDGE_CURVE('',#14463,#14464,#9450,.T.);
#18672=EDGE_CURVE('',#14463,#14461,#3060,.T.);
#18673=EDGE_CURVE('',#14462,#14464,#3061,.T.);
#18674=EDGE_CURVE('',#14465,#14466,#9451,.T.);
#18675=EDGE_CURVE('',#14465,#14467,#3062,.T.);
#18676=EDGE_CURVE('',#14468,#14467,#1766,.T.);
#18677=EDGE_CURVE('',#14466,#14468,#3063,.T.);
#18678=EDGE_CURVE('',#14469,#14470,#9452,.T.);
#18679=EDGE_CURVE('',#14469,#14465,#3064,.T.);
#18680=EDGE_CURVE('',#14470,#14466,#3065,.T.);
#18681=EDGE_CURVE('',#14471,#14472,#9453,.T.);
#18682=EDGE_CURVE('',#14471,#14469,#3066,.T.);
#18683=EDGE_CURVE('',#14472,#14470,#3067,.T.);
#18684=EDGE_CURVE('',#14473,#14474,#9454,.T.);
#18685=EDGE_CURVE('',#14473,#14471,#3068,.T.);
#18686=EDGE_CURVE('',#14474,#14472,#3069,.T.);
#18687=EDGE_CURVE('',#14475,#14476,#9455,.T.);
#18688=EDGE_CURVE('',#14475,#14473,#3070,.T.);
#18689=EDGE_CURVE('',#14476,#14474,#3071,.T.);
#18690=EDGE_CURVE('',#14477,#14478,#9456,.T.);
#18691=EDGE_CURVE('',#14477,#14475,#3072,.T.);
#18692=EDGE_CURVE('',#14478,#14476,#3073,.T.);
#18693=EDGE_CURVE('',#14479,#14480,#9457,.T.);
#18694=EDGE_CURVE('',#14479,#14477,#3074,.T.);
#18695=EDGE_CURVE('',#14480,#14478,#3075,.T.);
#18696=EDGE_CURVE('',#14481,#14482,#9458,.T.);
#18697=EDGE_CURVE('',#14481,#14479,#3076,.T.);
#18698=EDGE_CURVE('',#14482,#14480,#3077,.T.);
#18699=EDGE_CURVE('',#14483,#14484,#9459,.T.);
#18700=EDGE_CURVE('',#14483,#14481,#3078,.T.);
#18701=EDGE_CURVE('',#14484,#14482,#3079,.T.);
#18702=EDGE_CURVE('',#14485,#14486,#9460,.T.);
#18703=EDGE_CURVE('',#14485,#14483,#3080,.T.);
#18704=EDGE_CURVE('',#14486,#14484,#3081,.T.);
#18705=EDGE_CURVE('',#14487,#14488,#9461,.T.);
#18706=EDGE_CURVE('',#14487,#14485,#3082,.T.);
#18707=EDGE_CURVE('',#14488,#14486,#3083,.T.);
#18708=EDGE_CURVE('',#14489,#14490,#9462,.T.);
#18709=EDGE_CURVE('',#14489,#14487,#3084,.T.);
#18710=EDGE_CURVE('',#14490,#14488,#3085,.T.);
#18711=EDGE_CURVE('',#14491,#14492,#9463,.T.);
#18712=EDGE_CURVE('',#14491,#14489,#3086,.T.);
#18713=EDGE_CURVE('',#14492,#14490,#3087,.T.);
#18714=EDGE_CURVE('',#14493,#14494,#9464,.T.);
#18715=EDGE_CURVE('',#14493,#14491,#3088,.T.);
#18716=EDGE_CURVE('',#14494,#14492,#3089,.T.);
#18717=EDGE_CURVE('',#14495,#14496,#9465,.T.);
#18718=EDGE_CURVE('',#14495,#14493,#3090,.T.);
#18719=EDGE_CURVE('',#14496,#14494,#3091,.T.);
#18720=EDGE_CURVE('',#14497,#14498,#9466,.T.);
#18721=EDGE_CURVE('',#14497,#14495,#3092,.T.);
#18722=EDGE_CURVE('',#14498,#14496,#3093,.T.);
#18723=EDGE_CURVE('',#14499,#14500,#9467,.T.);
#18724=EDGE_CURVE('',#14499,#14497,#3094,.T.);
#18725=EDGE_CURVE('',#14500,#14498,#3095,.T.);
#18726=EDGE_CURVE('',#14501,#14502,#9468,.T.);
#18727=EDGE_CURVE('',#14501,#14499,#3096,.T.);
#18728=EDGE_CURVE('',#14502,#14500,#3097,.T.);
#18729=EDGE_CURVE('',#14503,#14504,#9469,.T.);
#18730=EDGE_CURVE('',#14503,#14501,#3098,.T.);
#18731=EDGE_CURVE('',#14504,#14502,#3099,.T.);
#18732=EDGE_CURVE('',#14505,#14506,#9470,.T.);
#18733=EDGE_CURVE('',#14505,#14503,#3100,.T.);
#18734=EDGE_CURVE('',#14506,#14504,#3101,.T.);
#18735=EDGE_CURVE('',#14507,#14508,#9471,.T.);
#18736=EDGE_CURVE('',#14507,#14505,#3102,.T.);
#18737=EDGE_CURVE('',#14508,#14506,#3103,.T.);
#18738=EDGE_CURVE('',#14509,#14510,#9472,.T.);
#18739=EDGE_CURVE('',#14509,#14507,#3104,.T.);
#18740=EDGE_CURVE('',#14510,#14508,#3105,.T.);
#18741=EDGE_CURVE('',#14511,#14512,#9473,.T.);
#18742=EDGE_CURVE('',#14511,#14509,#3106,.T.);
#18743=EDGE_CURVE('',#14512,#14510,#3107,.T.);
#18744=EDGE_CURVE('',#14513,#14514,#9474,.T.);
#18745=EDGE_CURVE('',#14513,#14511,#3108,.T.);
#18746=EDGE_CURVE('',#14514,#14512,#3109,.T.);
#18747=EDGE_CURVE('',#14515,#14516,#9475,.T.);
#18748=EDGE_CURVE('',#14515,#14513,#3110,.T.);
#18749=EDGE_CURVE('',#14516,#14514,#3111,.T.);
#18750=EDGE_CURVE('',#14517,#14518,#9476,.T.);
#18751=EDGE_CURVE('',#14517,#14515,#3112,.T.);
#18752=EDGE_CURVE('',#14518,#14516,#3113,.T.);
#18753=EDGE_CURVE('',#14519,#14520,#9477,.T.);
#18754=EDGE_CURVE('',#14519,#14517,#3114,.T.);
#18755=EDGE_CURVE('',#14520,#14518,#3115,.T.);
#18756=EDGE_CURVE('',#14521,#14522,#9478,.T.);
#18757=EDGE_CURVE('',#14521,#14519,#3116,.T.);
#18758=EDGE_CURVE('',#14522,#14520,#3117,.T.);
#18759=EDGE_CURVE('',#14523,#14524,#9479,.T.);
#18760=EDGE_CURVE('',#14523,#14521,#3118,.T.);
#18761=EDGE_CURVE('',#14524,#14522,#3119,.T.);
#18762=EDGE_CURVE('',#14525,#14526,#9480,.T.);
#18763=EDGE_CURVE('',#14525,#14523,#3120,.T.);
#18764=EDGE_CURVE('',#14526,#14524,#3121,.T.);
#18765=EDGE_CURVE('',#14527,#14528,#9481,.T.);
#18766=EDGE_CURVE('',#14527,#14525,#3122,.T.);
#18767=EDGE_CURVE('',#14528,#14526,#3123,.T.);
#18768=EDGE_CURVE('',#14529,#14530,#9482,.T.);
#18769=EDGE_CURVE('',#14529,#14527,#3124,.T.);
#18770=EDGE_CURVE('',#14530,#14528,#3125,.T.);
#18771=EDGE_CURVE('',#14531,#14532,#9483,.T.);
#18772=EDGE_CURVE('',#14531,#14529,#3126,.T.);
#18773=EDGE_CURVE('',#14532,#14530,#3127,.T.);
#18774=EDGE_CURVE('',#14533,#14534,#9484,.T.);
#18775=EDGE_CURVE('',#14533,#14531,#3128,.T.);
#18776=EDGE_CURVE('',#14534,#14532,#3129,.T.);
#18777=EDGE_CURVE('',#14535,#14536,#9485,.T.);
#18778=EDGE_CURVE('',#14535,#14533,#3130,.T.);
#18779=EDGE_CURVE('',#14536,#14534,#3131,.T.);
#18780=EDGE_CURVE('',#14537,#14538,#9486,.T.);
#18781=EDGE_CURVE('',#14537,#14535,#3132,.T.);
#18782=EDGE_CURVE('',#14538,#14536,#3133,.T.);
#18783=EDGE_CURVE('',#14539,#14540,#9487,.T.);
#18784=EDGE_CURVE('',#14539,#14537,#3134,.T.);
#18785=EDGE_CURVE('',#14540,#14538,#3135,.T.);
#18786=EDGE_CURVE('',#14541,#14542,#9488,.T.);
#18787=EDGE_CURVE('',#14541,#14539,#3136,.T.);
#18788=EDGE_CURVE('',#14542,#14540,#3137,.T.);
#18789=EDGE_CURVE('',#14543,#14544,#9489,.T.);
#18790=EDGE_CURVE('',#14543,#14541,#3138,.T.);
#18791=EDGE_CURVE('',#14544,#14542,#3139,.T.);
#18792=EDGE_CURVE('',#14545,#14546,#9490,.T.);
#18793=EDGE_CURVE('',#14545,#14543,#3140,.T.);
#18794=EDGE_CURVE('',#14546,#14544,#3141,.T.);
#18795=EDGE_CURVE('',#14547,#14548,#9491,.T.);
#18796=EDGE_CURVE('',#14547,#14545,#3142,.T.);
#18797=EDGE_CURVE('',#14548,#14546,#3143,.T.);
#18798=EDGE_CURVE('',#14549,#14550,#9492,.T.);
#18799=EDGE_CURVE('',#14549,#14547,#3144,.T.);
#18800=EDGE_CURVE('',#14550,#14548,#3145,.T.);
#18801=EDGE_CURVE('',#14551,#14552,#9493,.T.);
#18802=EDGE_CURVE('',#14551,#14549,#3146,.T.);
#18803=EDGE_CURVE('',#14552,#14550,#3147,.T.);
#18804=EDGE_CURVE('',#14553,#14554,#9494,.T.);
#18805=EDGE_CURVE('',#14553,#14551,#3148,.T.);
#18806=EDGE_CURVE('',#14554,#14552,#3149,.T.);
#18807=EDGE_CURVE('',#14555,#14556,#9495,.T.);
#18808=EDGE_CURVE('',#14555,#14553,#3150,.T.);
#18809=EDGE_CURVE('',#14556,#14554,#3151,.T.);
#18810=EDGE_CURVE('',#14557,#14558,#9496,.T.);
#18811=EDGE_CURVE('',#14557,#14555,#3152,.T.);
#18812=EDGE_CURVE('',#14558,#14556,#3153,.T.);
#18813=EDGE_CURVE('',#14559,#14560,#9497,.T.);
#18814=EDGE_CURVE('',#14559,#14557,#3154,.T.);
#18815=EDGE_CURVE('',#14560,#14558,#3155,.T.);
#18816=EDGE_CURVE('',#14561,#14562,#9498,.T.);
#18817=EDGE_CURVE('',#14561,#14559,#3156,.T.);
#18818=EDGE_CURVE('',#14562,#14560,#3157,.T.);
#18819=EDGE_CURVE('',#14563,#14564,#9499,.T.);
#18820=EDGE_CURVE('',#14563,#14561,#3158,.T.);
#18821=EDGE_CURVE('',#14564,#14562,#3159,.T.);
#18822=EDGE_CURVE('',#14565,#14566,#9500,.T.);
#18823=EDGE_CURVE('',#14565,#14563,#3160,.T.);
#18824=EDGE_CURVE('',#14566,#14564,#3161,.T.);
#18825=EDGE_CURVE('',#14567,#14568,#9501,.T.);
#18826=EDGE_CURVE('',#14567,#14565,#3162,.T.);
#18827=EDGE_CURVE('',#14568,#14566,#3163,.T.);
#18828=EDGE_CURVE('',#14569,#14570,#9502,.T.);
#18829=EDGE_CURVE('',#14569,#14567,#3164,.T.);
#18830=EDGE_CURVE('',#14570,#14568,#3165,.T.);
#18831=EDGE_CURVE('',#14571,#14572,#9503,.T.);
#18832=EDGE_CURVE('',#14571,#14569,#3166,.T.);
#18833=EDGE_CURVE('',#14572,#14570,#3167,.T.);
#18834=EDGE_CURVE('',#14573,#14574,#9504,.T.);
#18835=EDGE_CURVE('',#14573,#14571,#3168,.T.);
#18836=EDGE_CURVE('',#14574,#14572,#3169,.T.);
#18837=EDGE_CURVE('',#14575,#14576,#9505,.T.);
#18838=EDGE_CURVE('',#14575,#14573,#3170,.T.);
#18839=EDGE_CURVE('',#14576,#14574,#3171,.T.);
#18840=EDGE_CURVE('',#14577,#14578,#9506,.T.);
#18841=EDGE_CURVE('',#14577,#14575,#3172,.T.);
#18842=EDGE_CURVE('',#14578,#14576,#3173,.T.);
#18843=EDGE_CURVE('',#14579,#14580,#9507,.T.);
#18844=EDGE_CURVE('',#14579,#14577,#3174,.T.);
#18845=EDGE_CURVE('',#14580,#14578,#3175,.T.);
#18846=EDGE_CURVE('',#14581,#14582,#9508,.T.);
#18847=EDGE_CURVE('',#14581,#14579,#3176,.T.);
#18848=EDGE_CURVE('',#14582,#14580,#3177,.T.);
#18849=EDGE_CURVE('',#14583,#14584,#9509,.T.);
#18850=EDGE_CURVE('',#14583,#14581,#3178,.T.);
#18851=EDGE_CURVE('',#14584,#14582,#3179,.T.);
#18852=EDGE_CURVE('',#14585,#14586,#9510,.T.);
#18853=EDGE_CURVE('',#14585,#14583,#3180,.T.);
#18854=EDGE_CURVE('',#14586,#14584,#3181,.T.);
#18855=EDGE_CURVE('',#14587,#14588,#9511,.T.);
#18856=EDGE_CURVE('',#14587,#14585,#3182,.T.);
#18857=EDGE_CURVE('',#14588,#14586,#3183,.T.);
#18858=EDGE_CURVE('',#14589,#14590,#9512,.T.);
#18859=EDGE_CURVE('',#14589,#14587,#3184,.T.);
#18860=EDGE_CURVE('',#14590,#14588,#3185,.T.);
#18861=EDGE_CURVE('',#14591,#14592,#9513,.T.);
#18862=EDGE_CURVE('',#14591,#14589,#3186,.T.);
#18863=EDGE_CURVE('',#14592,#14590,#3187,.T.);
#18864=EDGE_CURVE('',#14593,#14594,#9514,.T.);
#18865=EDGE_CURVE('',#14593,#14591,#3188,.T.);
#18866=EDGE_CURVE('',#14594,#14592,#3189,.T.);
#18867=EDGE_CURVE('',#14595,#14596,#9515,.T.);
#18868=EDGE_CURVE('',#14595,#14593,#3190,.T.);
#18869=EDGE_CURVE('',#14596,#14594,#3191,.T.);
#18870=EDGE_CURVE('',#14597,#14598,#9516,.T.);
#18871=EDGE_CURVE('',#14597,#14595,#3192,.T.);
#18872=EDGE_CURVE('',#14598,#14596,#3193,.T.);
#18873=EDGE_CURVE('',#14599,#14600,#9517,.T.);
#18874=EDGE_CURVE('',#14599,#14597,#3194,.T.);
#18875=EDGE_CURVE('',#14600,#14598,#3195,.T.);
#18876=EDGE_CURVE('',#14601,#14602,#9518,.T.);
#18877=EDGE_CURVE('',#14601,#14599,#3196,.T.);
#18878=EDGE_CURVE('',#14602,#14600,#3197,.T.);
#18879=EDGE_CURVE('',#14603,#14604,#9519,.T.);
#18880=EDGE_CURVE('',#14603,#14601,#3198,.T.);
#18881=EDGE_CURVE('',#14604,#14602,#3199,.T.);
#18882=EDGE_CURVE('',#14605,#14606,#9520,.T.);
#18883=EDGE_CURVE('',#14605,#14603,#3200,.T.);
#18884=EDGE_CURVE('',#14606,#14604,#3201,.T.);
#18885=EDGE_CURVE('',#14607,#14608,#9521,.T.);
#18886=EDGE_CURVE('',#14607,#14605,#3202,.T.);
#18887=EDGE_CURVE('',#14608,#14606,#3203,.T.);
#18888=EDGE_CURVE('',#14609,#14610,#9522,.T.);
#18889=EDGE_CURVE('',#14609,#14607,#3204,.T.);
#18890=EDGE_CURVE('',#14610,#14608,#3205,.T.);
#18891=EDGE_CURVE('',#14611,#14612,#9523,.T.);
#18892=EDGE_CURVE('',#14611,#14609,#3206,.T.);
#18893=EDGE_CURVE('',#14612,#14610,#3207,.T.);
#18894=EDGE_CURVE('',#14613,#14614,#9524,.T.);
#18895=EDGE_CURVE('',#14613,#14611,#3208,.T.);
#18896=EDGE_CURVE('',#14614,#14612,#3209,.T.);
#18897=EDGE_CURVE('',#14615,#14616,#9525,.T.);
#18898=EDGE_CURVE('',#14615,#14613,#3210,.T.);
#18899=EDGE_CURVE('',#14616,#14614,#3211,.T.);
#18900=EDGE_CURVE('',#14467,#14617,#3212,.T.);
#18901=EDGE_CURVE('',#14618,#14617,#1767,.F.);
#18902=EDGE_CURVE('',#14619,#14618,#1768,.F.);
#18903=EDGE_CURVE('',#14619,#14468,#3213,.T.);
#18904=EDGE_CURVE('',#14464,#14619,#3214,.T.);
#18905=EDGE_CURVE('',#14620,#14316,#3215,.T.);
#18906=EDGE_CURVE('',#14620,#14616,#3216,.T.);
#18907=EDGE_CURVE('',#14316,#14621,#1769,.T.);
#18908=EDGE_CURVE('',#14621,#14315,#1770,.T.);
#18909=EDGE_CURVE('',#14315,#14622,#3217,.T.);
#18910=EDGE_CURVE('',#14622,#14620,#1771,.T.);
#18911=EDGE_CURVE('',#14622,#14615,#3218,.T.);
#18912=EDGE_CURVE('',#14617,#14463,#3219,.T.);
#18913=EDGE_CURVE('',#14623,#14623,#1772,.T.);
#18914=EDGE_CURVE('',#14623,#14624,#9526,.T.);
#18915=EDGE_CURVE('',#14624,#14624,#1773,.T.);
#18916=EDGE_CURVE('',#14621,#14623,#9527,.T.);
#18917=EDGE_CURVE('',#14617,#14619,#1774,.F.);
#18918=EDGE_CURVE('',#14625,#14625,#1775,.T.);
#18919=EDGE_CURVE('',#14625,#14618,#9528,.T.);
#18920=EDGE_CURVE('',#14626,#14627,#1776,.T.);
#18921=EDGE_CURVE('',#14628,#14628,#1777,.T.);
#18922=EDGE_CURVE('',#14628,#14629,#9529,.T.);
#18923=EDGE_CURVE('',#14629,#14630,#1778,.T.);
#18924=EDGE_CURVE('',#14630,#14629,#1779,.T.);
#18925=EDGE_CURVE('',#14631,#14631,#1780,.T.);
#18926=EDGE_CURVE('',#14631,#14630,#9530,.T.);
#18927=EDGE_CURVE('',#14632,#14632,#1781,.T.);
#18928=EDGE_CURVE('',#14633,#14634,#202,.T.);
#18929=EDGE_CURVE('',#14634,#14635,#9531,.T.);
#18930=EDGE_CURVE('',#14635,#14636,#9532,.F.);
#18931=EDGE_CURVE('',#14636,#14633,#9533,.T.);
#18932=EDGE_CURVE('',#14637,#14636,#1782,.T.);
#18933=EDGE_CURVE('',#14638,#14637,#9534,.T.);
#18934=EDGE_CURVE('',#14639,#14638,#3220,.T.);
#18935=EDGE_CURVE('',#14640,#14639,#1783,.T.);
#18936=EDGE_CURVE('',#14633,#14640,#3221,.T.);
#18937=EDGE_CURVE('',#14641,#14638,#203,.T.);
#18938=EDGE_CURVE('',#14637,#14642,#9535,.F.);
#18939=EDGE_CURVE('',#14642,#14641,#9536,.T.);
#18940=EDGE_CURVE('',#14641,#14643,#1784,.T.);
#18941=EDGE_CURVE('',#14644,#14643,#204,.T.);
#18942=EDGE_CURVE('',#14644,#14645,#3222,.T.);
#18943=EDGE_CURVE('',#14639,#14645,#1785,.T.);
#18944=EDGE_CURVE('',#14646,#14634,#1786,.T.);
#18945=EDGE_CURVE('',#14647,#14646,#9537,.T.);
#18946=EDGE_CURVE('',#14647,#14648,#1787,.T.);
#18947=EDGE_CURVE('',#14649,#14648,#9538,.T.);
#18948=EDGE_CURVE('',#14650,#14649,#1788,.T.);
#18949=EDGE_CURVE('',#14651,#14650,#9539,.T.);
#18950=EDGE_CURVE('',#14651,#14652,#1789,.T.);
#18951=EDGE_CURVE('',#14653,#14652,#9540,.T.);
#18952=EDGE_CURVE('',#14654,#14653,#1790,.T.);
#18953=EDGE_CURVE('',#14655,#14654,#9541,.T.);
#18954=EDGE_CURVE('',#14655,#14656,#1791,.T.);
#18955=EDGE_CURVE('',#14657,#14656,#9542,.T.);
#18956=EDGE_CURVE('',#14658,#14657,#1792,.T.);
#18957=EDGE_CURVE('',#14659,#14658,#9543,.T.);
#18958=EDGE_CURVE('',#14659,#14660,#1793,.T.);
#18959=EDGE_CURVE('',#14661,#14660,#9544,.T.);
#18960=EDGE_CURVE('',#14662,#14661,#1794,.T.);
#18961=EDGE_CURVE('',#14663,#14662,#9545,.T.);
#18962=EDGE_CURVE('',#14663,#14664,#1795,.T.);
#18963=EDGE_CURVE('',#14665,#14664,#9546,.T.);
#18964=EDGE_CURVE('',#14666,#14665,#1796,.T.);
#18965=EDGE_CURVE('',#14667,#14666,#9547,.T.);
#18966=EDGE_CURVE('',#14667,#14668,#1797,.T.);
#18967=EDGE_CURVE('',#14669,#14668,#9548,.T.);
#18968=EDGE_CURVE('',#14670,#14669,#1798,.T.);
#18969=EDGE_CURVE('',#14671,#14670,#9549,.T.);
#18970=EDGE_CURVE('',#14671,#14672,#1799,.T.);
#18971=EDGE_CURVE('',#14673,#14672,#9550,.T.);
#18972=EDGE_CURVE('',#14674,#14673,#1800,.T.);
#18973=EDGE_CURVE('',#14674,#14675,#9551,.T.);
#18974=EDGE_CURVE('',#14675,#14675,#1801,.T.);
#18975=EDGE_CURVE('',#14676,#14674,#1802,.T.);
#18976=EDGE_CURVE('',#14677,#14676,#9552,.T.);
#18977=EDGE_CURVE('',#14677,#14678,#1803,.T.);
#18978=EDGE_CURVE('',#14679,#14678,#9553,.T.);
#18979=EDGE_CURVE('',#14680,#14679,#1804,.T.);
#18980=EDGE_CURVE('',#14681,#14680,#9554,.T.);
#18981=EDGE_CURVE('',#14681,#14682,#1805,.T.);
#18982=EDGE_CURVE('',#14683,#14682,#9555,.T.);
#18983=EDGE_CURVE('',#14684,#14683,#1806,.T.);
#18984=EDGE_CURVE('',#14685,#14684,#9556,.T.);
#18985=EDGE_CURVE('',#14685,#14686,#1807,.T.);
#18986=EDGE_CURVE('',#14687,#14686,#9557,.T.);
#18987=EDGE_CURVE('',#14688,#14687,#1808,.T.);
#18988=EDGE_CURVE('',#14689,#14688,#9558,.T.);
#18989=EDGE_CURVE('',#14689,#14690,#1809,.T.);
#18990=EDGE_CURVE('',#14691,#14690,#9559,.T.);
#18991=EDGE_CURVE('',#14692,#14691,#1810,.T.);
#18992=EDGE_CURVE('',#14693,#14692,#9560,.T.);
#18993=EDGE_CURVE('',#14693,#14694,#1811,.T.);
#18994=EDGE_CURVE('',#14695,#14694,#9561,.T.);
#18995=EDGE_CURVE('',#14696,#14695,#1812,.T.);
#18996=EDGE_CURVE('',#14697,#14696,#9562,.T.);
#18997=EDGE_CURVE('',#14697,#14698,#1813,.T.);
#18998=EDGE_CURVE('',#14699,#14698,#9563,.T.);
#18999=EDGE_CURVE('',#14700,#14699,#1814,.T.);
#19000=EDGE_CURVE('',#14701,#14700,#9564,.T.);
#19001=EDGE_CURVE('',#14701,#14702,#1815,.T.);
#19002=EDGE_CURVE('',#14643,#14702,#9565,.T.);
#19003=EDGE_CURVE('',#14642,#14635,#1816,.T.);
#19004=EDGE_CURVE('',#14702,#14703,#9566,.F.);
#19005=EDGE_CURVE('',#14703,#14644,#9567,.T.);
#19006=EDGE_CURVE('',#14704,#14703,#1817,.T.);
#19007=EDGE_CURVE('',#14705,#14704,#9568,.T.);
#19008=EDGE_CURVE('',#14706,#14705,#3223,.T.);
#19009=EDGE_CURVE('',#14645,#14706,#1818,.T.);
#19010=EDGE_CURVE('',#14700,#14705,#205,.T.);
#19011=EDGE_CURVE('',#14704,#14701,#9569,.F.);
#19012=EDGE_CURVE('',#14707,#14699,#206,.T.);
#19013=EDGE_CURVE('',#14707,#14708,#3224,.T.);
#19014=EDGE_CURVE('',#14706,#14708,#1819,.T.);
#19015=EDGE_CURVE('',#14698,#14709,#9570,.F.);
#19016=EDGE_CURVE('',#14709,#14707,#9571,.T.);
#19017=EDGE_CURVE('',#14710,#14709,#1820,.T.);
#19018=EDGE_CURVE('',#14711,#14710,#9572,.T.);
#19019=EDGE_CURVE('',#14712,#14711,#3225,.T.);
#19020=EDGE_CURVE('',#14708,#14712,#1821,.T.);
#19021=EDGE_CURVE('',#14696,#14711,#207,.T.);
#19022=EDGE_CURVE('',#14710,#14697,#9573,.F.);
#19023=EDGE_CURVE('',#14713,#14695,#208,.T.);
#19024=EDGE_CURVE('',#14713,#14714,#3226,.T.);
#19025=EDGE_CURVE('',#14712,#14714,#1822,.T.);
#19026=EDGE_CURVE('',#14694,#14715,#9574,.F.);
#19027=EDGE_CURVE('',#14715,#14713,#9575,.T.);
#19028=EDGE_CURVE('',#14716,#14715,#1823,.T.);
#19029=EDGE_CURVE('',#14717,#14716,#9576,.T.);
#19030=EDGE_CURVE('',#14718,#14717,#3227,.T.);
#19031=EDGE_CURVE('',#14714,#14718,#1824,.T.);
#19032=EDGE_CURVE('',#14692,#14717,#209,.T.);
#19033=EDGE_CURVE('',#14716,#14693,#9577,.F.);
#19034=EDGE_CURVE('',#14719,#14691,#210,.T.);
#19035=EDGE_CURVE('',#14719,#14720,#3228,.T.);
#19036=EDGE_CURVE('',#14718,#14720,#1825,.T.);
#19037=EDGE_CURVE('',#14690,#14721,#9578,.F.);
#19038=EDGE_CURVE('',#14721,#14719,#9579,.T.);
#19039=EDGE_CURVE('',#14722,#14721,#1826,.T.);
#19040=EDGE_CURVE('',#14723,#14722,#9580,.T.);
#19041=EDGE_CURVE('',#14724,#14723,#3229,.T.);
#19042=EDGE_CURVE('',#14720,#14724,#1827,.T.);
#19043=EDGE_CURVE('',#14688,#14723,#211,.T.);
#19044=EDGE_CURVE('',#14722,#14689,#9581,.F.);
#19045=EDGE_CURVE('',#14725,#14687,#212,.T.);
#19046=EDGE_CURVE('',#14725,#14726,#3230,.T.);
#19047=EDGE_CURVE('',#14724,#14726,#1828,.T.);
#19048=EDGE_CURVE('',#14686,#14727,#9582,.F.);
#19049=EDGE_CURVE('',#14727,#14725,#9583,.T.);
#19050=EDGE_CURVE('',#14728,#14727,#1829,.T.);
#19051=EDGE_CURVE('',#14729,#14728,#9584,.T.);
#19052=EDGE_CURVE('',#14730,#14729,#3231,.T.);
#19053=EDGE_CURVE('',#14726,#14730,#1830,.T.);
#19054=EDGE_CURVE('',#14684,#14729,#213,.T.);
#19055=EDGE_CURVE('',#14728,#14685,#9585,.F.);
#19056=EDGE_CURVE('',#14731,#14683,#214,.T.);
#19057=EDGE_CURVE('',#14731,#14732,#3232,.T.);
#19058=EDGE_CURVE('',#14730,#14732,#1831,.T.);
#19059=EDGE_CURVE('',#14682,#14733,#9586,.F.);
#19060=EDGE_CURVE('',#14733,#14731,#9587,.T.);
#19061=EDGE_CURVE('',#14734,#14733,#1832,.T.);
#19062=EDGE_CURVE('',#14735,#14734,#9588,.T.);
#19063=EDGE_CURVE('',#14736,#14735,#3233,.T.);
#19064=EDGE_CURVE('',#14732,#14736,#1833,.T.);
#19065=EDGE_CURVE('',#14680,#14735,#215,.T.);
#19066=EDGE_CURVE('',#14734,#14681,#9589,.F.);
#19067=EDGE_CURVE('',#14737,#14679,#216,.T.);
#19068=EDGE_CURVE('',#14737,#14738,#3234,.T.);
#19069=EDGE_CURVE('',#14736,#14738,#1834,.T.);
#19070=EDGE_CURVE('',#14678,#14739,#9590,.F.);
#19071=EDGE_CURVE('',#14739,#14737,#9591,.T.);
#19072=EDGE_CURVE('',#14740,#14739,#1835,.T.);
#19073=EDGE_CURVE('',#14741,#14740,#9592,.T.);
#19074=EDGE_CURVE('',#14742,#14741,#3235,.T.);
#19075=EDGE_CURVE('',#14738,#14742,#1836,.T.);
#19076=EDGE_CURVE('',#14676,#14741,#217,.T.);
#19077=EDGE_CURVE('',#14740,#14677,#9593,.F.);
#19078=EDGE_CURVE('',#14743,#14673,#218,.T.);
#19079=EDGE_CURVE('',#14743,#14744,#3236,.T.);
#19080=EDGE_CURVE('',#14742,#14744,#1837,.T.);
#19081=EDGE_CURVE('',#14672,#14745,#9594,.F.);
#19082=EDGE_CURVE('',#14745,#14743,#9595,.T.);
#19083=EDGE_CURVE('',#14746,#14745,#1838,.T.);
#19084=EDGE_CURVE('',#14747,#14746,#9596,.T.);
#19085=EDGE_CURVE('',#14748,#14747,#3237,.T.);
#19086=EDGE_CURVE('',#14744,#14748,#1839,.T.);
#19087=EDGE_CURVE('',#14670,#14747,#219,.T.);
#19088=EDGE_CURVE('',#14746,#14671,#9597,.F.);
#19089=EDGE_CURVE('',#14749,#14669,#220,.T.);
#19090=EDGE_CURVE('',#14749,#14750,#3238,.T.);
#19091=EDGE_CURVE('',#14748,#14750,#1840,.T.);
#19092=EDGE_CURVE('',#14668,#14751,#9598,.F.);
#19093=EDGE_CURVE('',#14751,#14749,#9599,.T.);
#19094=EDGE_CURVE('',#14752,#14751,#1841,.T.);
#19095=EDGE_CURVE('',#14753,#14752,#9600,.T.);
#19096=EDGE_CURVE('',#14754,#14753,#3239,.T.);
#19097=EDGE_CURVE('',#14750,#14754,#1842,.T.);
#19098=EDGE_CURVE('',#14666,#14753,#221,.T.);
#19099=EDGE_CURVE('',#14752,#14667,#9601,.F.);
#19100=EDGE_CURVE('',#14755,#14665,#222,.T.);
#19101=EDGE_CURVE('',#14755,#14756,#3240,.T.);
#19102=EDGE_CURVE('',#14754,#14756,#1843,.T.);
#19103=EDGE_CURVE('',#14664,#14757,#9602,.F.);
#19104=EDGE_CURVE('',#14757,#14755,#9603,.T.);
#19105=EDGE_CURVE('',#14758,#14757,#1844,.T.);
#19106=EDGE_CURVE('',#14759,#14758,#9604,.T.);
#19107=EDGE_CURVE('',#14760,#14759,#3241,.T.);
#19108=EDGE_CURVE('',#14756,#14760,#1845,.T.);
#19109=EDGE_CURVE('',#14662,#14759,#223,.T.);
#19110=EDGE_CURVE('',#14758,#14663,#9605,.F.);
#19111=EDGE_CURVE('',#14761,#14661,#224,.T.);
#19112=EDGE_CURVE('',#14761,#14762,#3242,.T.);
#19113=EDGE_CURVE('',#14760,#14762,#1846,.T.);
#19114=EDGE_CURVE('',#14660,#14763,#9606,.F.);
#19115=EDGE_CURVE('',#14763,#14761,#9607,.T.);
#19116=EDGE_CURVE('',#14764,#14763,#1847,.T.);
#19117=EDGE_CURVE('',#14765,#14764,#9608,.T.);
#19118=EDGE_CURVE('',#14766,#14765,#3243,.T.);
#19119=EDGE_CURVE('',#14762,#14766,#1848,.T.);
#19120=EDGE_CURVE('',#14658,#14765,#225,.T.);
#19121=EDGE_CURVE('',#14764,#14659,#9609,.F.);
#19122=EDGE_CURVE('',#14767,#14657,#226,.T.);
#19123=EDGE_CURVE('',#14767,#14768,#3244,.T.);
#19124=EDGE_CURVE('',#14766,#14768,#1849,.T.);
#19125=EDGE_CURVE('',#14656,#14769,#9610,.F.);
#19126=EDGE_CURVE('',#14769,#14767,#9611,.T.);
#19127=EDGE_CURVE('',#14770,#14769,#1850,.T.);
#19128=EDGE_CURVE('',#14771,#14770,#9612,.T.);
#19129=EDGE_CURVE('',#14772,#14771,#3245,.T.);
#19130=EDGE_CURVE('',#14768,#14772,#1851,.T.);
#19131=EDGE_CURVE('',#14654,#14771,#227,.T.);
#19132=EDGE_CURVE('',#14770,#14655,#9613,.F.);
#19133=EDGE_CURVE('',#14773,#14653,#228,.T.);
#19134=EDGE_CURVE('',#14773,#14774,#3246,.T.);
#19135=EDGE_CURVE('',#14772,#14774,#1852,.T.);
#19136=EDGE_CURVE('',#14652,#14775,#9614,.F.);
#19137=EDGE_CURVE('',#14775,#14773,#9615,.T.);
#19138=EDGE_CURVE('',#14776,#14775,#1853,.T.);
#19139=EDGE_CURVE('',#14777,#14776,#9616,.T.);
#19140=EDGE_CURVE('',#14778,#14777,#3247,.T.);
#19141=EDGE_CURVE('',#14774,#14778,#1854,.T.);
#19142=EDGE_CURVE('',#14650,#14777,#229,.T.);
#19143=EDGE_CURVE('',#14776,#14651,#9617,.F.);
#19144=EDGE_CURVE('',#14779,#14649,#230,.T.);
#19145=EDGE_CURVE('',#14779,#14780,#3248,.T.);
#19146=EDGE_CURVE('',#14778,#14780,#1855,.T.);
#19147=EDGE_CURVE('',#14648,#14781,#9618,.F.);
#19148=EDGE_CURVE('',#14781,#14779,#9619,.T.);
#19149=EDGE_CURVE('',#14782,#14781,#1856,.T.);
#19150=EDGE_CURVE('',#14783,#14782,#9620,.T.);
#19151=EDGE_CURVE('',#14784,#14783,#3249,.T.);
#19152=EDGE_CURVE('',#14780,#14784,#1857,.T.);
#19153=EDGE_CURVE('',#14646,#14783,#231,.T.);
#19154=EDGE_CURVE('',#14782,#14647,#9621,.F.);
#19155=EDGE_CURVE('',#14785,#14786,#9622,.T.);
#19156=EDGE_CURVE('',#14786,#14787,#9623,.T.);
#19157=EDGE_CURVE('',#14787,#14788,#9624,.T.);
#19158=EDGE_CURVE('',#14785,#14788,#9625,.T.);
#19159=EDGE_CURVE('',#14786,#14789,#9626,.T.);
#19160=EDGE_CURVE('',#14789,#14790,#9627,.T.);
#19161=EDGE_CURVE('',#14790,#14787,#9628,.T.);
#19162=EDGE_CURVE('',#14791,#14792,#9629,.T.);
#19163=EDGE_CURVE('',#14792,#14793,#9630,.T.);
#19164=EDGE_CURVE('',#14793,#14794,#9631,.T.);
#19165=EDGE_CURVE('',#14794,#14791,#9632,.T.);
#19166=EDGE_CURVE('',#14795,#14793,#9633,.T.);
#19167=EDGE_CURVE('',#14792,#14796,#9634,.T.);
#19168=EDGE_CURVE('',#14796,#14795,#9635,.T.);
#19169=EDGE_CURVE('',#14789,#14791,#9636,.T.);
#19170=EDGE_CURVE('',#14794,#14790,#9637,.T.);
#19171=EDGE_CURVE('',#14788,#14795,#9638,.T.);
#19172=EDGE_CURVE('',#14796,#14785,#9639,.T.);
#19173=EDGE_CURVE('',#14790,#14797,#9640,.T.);
#19174=EDGE_CURVE('',#14797,#14798,#9641,.T.);
#19175=EDGE_CURVE('',#14787,#14798,#9642,.T.);
#19176=EDGE_CURVE('',#14794,#14799,#9643,.T.);
#19177=EDGE_CURVE('',#14799,#14797,#9644,.T.);
#19178=EDGE_CURVE('',#14793,#14800,#9645,.T.);
#19179=EDGE_CURVE('',#14800,#14799,#9646,.T.);
#19180=EDGE_CURVE('',#14784,#14640,#1858,.T.);
#19181=EDGE_CURVE('',#14795,#14801,#9647,.T.);
#19182=EDGE_CURVE('',#14801,#14800,#9648,.T.);
#19183=EDGE_CURVE('',#14788,#14802,#9649,.T.);
#19184=EDGE_CURVE('',#14802,#14801,#9650,.T.);
#19185=EDGE_CURVE('',#14798,#14802,#9651,.T.);
#19186=EDGE_CURVE('',#14803,#14803,#1859,.T.);
#19187=EDGE_CURVE('',#14803,#14632,#9652,.T.);
#19188=EDGE_CURVE('',#14804,#14804,#1860,.T.);
#19189=EDGE_CURVE('',#14804,#14803,#9653,.T.);
#19190=EDGE_CURVE('',#14805,#14805,#1861,.T.);
#19191=EDGE_CURVE('',#14675,#14805,#9654,.T.);
#19192=EDGE_CURVE('',#14806,#14807,#9655,.T.);
#19193=EDGE_CURVE('',#14806,#14808,#3250,.T.);
#19194=EDGE_CURVE('',#14808,#14809,#1862,.T.);
#19195=EDGE_CURVE('',#14809,#14807,#3251,.T.);
#19196=EDGE_CURVE('',#14810,#14811,#9656,.T.);
#19197=EDGE_CURVE('',#14810,#14806,#3252,.T.);
#19198=EDGE_CURVE('',#14807,#14811,#3253,.T.);
#19199=EDGE_CURVE('',#14812,#14813,#9657,.T.);
#19200=EDGE_CURVE('',#14812,#14810,#3254,.T.);
#19201=EDGE_CURVE('',#14811,#14813,#3255,.T.);
#19202=EDGE_CURVE('',#14814,#14815,#9658,.T.);
#19203=EDGE_CURVE('',#14814,#14812,#3256,.T.);
#19204=EDGE_CURVE('',#14813,#14815,#3257,.T.);
#19205=EDGE_CURVE('',#14816,#14817,#9659,.T.);
#19206=EDGE_CURVE('',#14816,#14814,#3258,.T.);
#19207=EDGE_CURVE('',#14815,#14817,#3259,.T.);
#19208=EDGE_CURVE('',#14818,#14819,#9660,.T.);
#19209=EDGE_CURVE('',#14818,#14816,#3260,.T.);
#19210=EDGE_CURVE('',#14817,#14819,#3261,.T.);
#19211=EDGE_CURVE('',#14820,#14821,#9661,.T.);
#19212=EDGE_CURVE('',#14820,#14818,#3262,.T.);
#19213=EDGE_CURVE('',#14819,#14821,#3263,.T.);
#19214=EDGE_CURVE('',#14822,#14823,#9662,.T.);
#19215=EDGE_CURVE('',#14822,#14824,#3264,.T.);
#19216=EDGE_CURVE('',#14825,#14824,#1863,.T.);
#19217=EDGE_CURVE('',#14823,#14825,#3265,.T.);
#19218=EDGE_CURVE('',#14826,#14827,#9663,.T.);
#19219=EDGE_CURVE('',#14826,#14822,#3266,.T.);
#19220=EDGE_CURVE('',#14827,#14823,#3267,.T.);
#19221=EDGE_CURVE('',#14828,#14829,#9664,.T.);
#19222=EDGE_CURVE('',#14828,#14826,#3268,.T.);
#19223=EDGE_CURVE('',#14829,#14827,#3269,.T.);
#19224=EDGE_CURVE('',#14830,#14831,#9665,.T.);
#19225=EDGE_CURVE('',#14830,#14828,#3270,.T.);
#19226=EDGE_CURVE('',#14831,#14829,#3271,.T.);
#19227=EDGE_CURVE('',#14832,#14833,#9666,.T.);
#19228=EDGE_CURVE('',#14832,#14830,#3272,.T.);
#19229=EDGE_CURVE('',#14833,#14831,#3273,.T.);
#19230=EDGE_CURVE('',#14834,#14835,#9667,.T.);
#19231=EDGE_CURVE('',#14834,#14832,#3274,.T.);
#19232=EDGE_CURVE('',#14835,#14833,#3275,.T.);
#19233=EDGE_CURVE('',#14824,#14836,#3276,.T.);
#19234=EDGE_CURVE('',#14837,#14836,#1864,.F.);
#19235=EDGE_CURVE('',#14838,#14837,#1865,.F.);
#19236=EDGE_CURVE('',#14838,#14825,#3277,.T.);
#19237=EDGE_CURVE('',#14821,#14838,#3278,.T.);
#19238=EDGE_CURVE('',#14839,#14809,#3279,.T.);
#19239=EDGE_CURVE('',#14839,#14835,#3280,.T.);
#19240=EDGE_CURVE('',#14809,#14840,#1866,.T.);
#19241=EDGE_CURVE('',#14840,#14808,#1867,.T.);
#19242=EDGE_CURVE('',#14808,#14841,#3281,.T.);
#19243=EDGE_CURVE('',#14841,#14839,#1868,.T.);
#19244=EDGE_CURVE('',#14841,#14834,#3282,.T.);
#19245=EDGE_CURVE('',#14836,#14820,#3283,.T.);
#19246=EDGE_CURVE('',#14842,#14843,#9668,.T.);
#19247=EDGE_CURVE('',#14842,#14844,#9669,.T.);
#19248=EDGE_CURVE('',#14844,#14845,#9670,.T.);
#19249=EDGE_CURVE('',#14843,#14845,#9671,.T.);
#19250=EDGE_CURVE('',#14846,#14842,#9672,.T.);
#19251=EDGE_CURVE('',#14846,#14847,#9673,.T.);
#19252=EDGE_CURVE('',#14847,#14844,#9674,.T.);
#19253=EDGE_CURVE('',#14848,#14846,#9675,.T.);
#19254=EDGE_CURVE('',#14848,#14849,#9676,.T.);
#19255=EDGE_CURVE('',#14849,#14847,#9677,.T.);
#19256=EDGE_CURVE('',#14850,#14848,#9678,.T.);
#19257=EDGE_CURVE('',#14850,#14851,#9679,.T.);
#19258=EDGE_CURVE('',#14851,#14849,#9680,.T.);
#19259=EDGE_CURVE('',#14852,#14850,#9681,.T.);
#19260=EDGE_CURVE('',#14852,#14853,#9682,.T.);
#19261=EDGE_CURVE('',#14853,#14851,#9683,.T.);
#19262=EDGE_CURVE('',#14843,#14852,#9684,.T.);
#19263=EDGE_CURVE('',#14845,#14853,#9685,.T.);
#19264=EDGE_CURVE('',#14854,#14854,#1869,.T.);
#19265=EDGE_CURVE('',#14840,#14854,#9686,.T.);
#19266=EDGE_CURVE('',#14836,#14838,#1870,.F.);
#19267=EDGE_CURVE('',#14855,#14855,#1871,.T.);
#19268=EDGE_CURVE('',#14855,#14837,#9687,.T.);
#19269=ORIENTED_EDGE('',*,*,#14856,.T.);
#19270=ORIENTED_EDGE('',*,*,#14857,.T.);
#19271=ORIENTED_EDGE('',*,*,#14858,.T.);
#19272=ORIENTED_EDGE('',*,*,#14859,.T.);
#19273=ORIENTED_EDGE('',*,*,#14860,.T.);
#19274=ORIENTED_EDGE('',*,*,#14861,.T.);
#19275=ORIENTED_EDGE('',*,*,#14857,.F.);
#19276=ORIENTED_EDGE('',*,*,#14862,.F.);
#19277=ORIENTED_EDGE('',*,*,#14863,.F.);
#19278=ORIENTED_EDGE('',*,*,#14864,.F.);
#19279=ORIENTED_EDGE('',*,*,#14856,.F.);
#19280=ORIENTED_EDGE('',*,*,#14865,.F.);
#19281=ORIENTED_EDGE('',*,*,#14866,.T.);
#19282=ORIENTED_EDGE('',*,*,#14867,.T.);
#19283=ORIENTED_EDGE('',*,*,#14868,.F.);
#19284=ORIENTED_EDGE('',*,*,#14862,.T.);
#19285=ORIENTED_EDGE('',*,*,#14861,.F.);
#19286=ORIENTED_EDGE('',*,*,#14869,.T.);
#19287=ORIENTED_EDGE('',*,*,#14870,.T.);
#19288=ORIENTED_EDGE('',*,*,#14871,.T.);
#19289=ORIENTED_EDGE('',*,*,#14865,.T.);
#19290=ORIENTED_EDGE('',*,*,#14872,.T.);
#19291=ORIENTED_EDGE('',*,*,#14873,.T.);
#19292=ORIENTED_EDGE('',*,*,#14874,.T.);
#19293=ORIENTED_EDGE('',*,*,#14875,.T.);
#19294=ORIENTED_EDGE('',*,*,#14863,.T.);
#19295=ORIENTED_EDGE('',*,*,#14868,.T.);
#19296=ORIENTED_EDGE('',*,*,#14858,.F.);
#19297=ORIENTED_EDGE('',*,*,#14864,.T.);
#19298=ORIENTED_EDGE('',*,*,#14875,.F.);
#19299=ORIENTED_EDGE('',*,*,#14876,.F.);
#19300=ORIENTED_EDGE('',*,*,#14877,.T.);
#19301=ORIENTED_EDGE('',*,*,#14878,.T.);
#19302=ORIENTED_EDGE('',*,*,#14874,.F.);
#19303=ORIENTED_EDGE('',*,*,#14879,.T.);
#19304=ORIENTED_EDGE('',*,*,#14880,.F.);
#19305=ORIENTED_EDGE('',*,*,#14881,.F.);
#19306=ORIENTED_EDGE('',*,*,#14882,.T.);
#19307=ORIENTED_EDGE('',*,*,#14876,.T.);
#19308=ORIENTED_EDGE('',*,*,#14873,.F.);
#19309=ORIENTED_EDGE('',*,*,#14883,.F.);
#19310=ORIENTED_EDGE('',*,*,#14884,.F.);
#19311=ORIENTED_EDGE('',*,*,#14879,.F.);
#19312=ORIENTED_EDGE('',*,*,#14885,.T.);
#19313=ORIENTED_EDGE('',*,*,#14886,.T.);
#19314=ORIENTED_EDGE('',*,*,#14887,.T.);
#19315=ORIENTED_EDGE('',*,*,#14888,.T.);
#19316=ORIENTED_EDGE('',*,*,#14889,.T.);
#19317=ORIENTED_EDGE('',*,*,#14890,.T.);
#19318=ORIENTED_EDGE('',*,*,#14891,.T.);
#19319=ORIENTED_EDGE('',*,*,#14892,.T.);
#19320=ORIENTED_EDGE('',*,*,#14893,.T.);
#19321=ORIENTED_EDGE('',*,*,#14894,.T.);
#19322=ORIENTED_EDGE('',*,*,#14895,.T.);
#19323=ORIENTED_EDGE('',*,*,#14896,.T.);
#19324=ORIENTED_EDGE('',*,*,#14897,.T.);
#19325=ORIENTED_EDGE('',*,*,#14898,.T.);
#19326=ORIENTED_EDGE('',*,*,#14899,.T.);
#19327=ORIENTED_EDGE('',*,*,#14900,.T.);
#19328=ORIENTED_EDGE('',*,*,#14901,.T.);
#19329=ORIENTED_EDGE('',*,*,#14902,.T.);
#19330=ORIENTED_EDGE('',*,*,#14903,.T.);
#19331=ORIENTED_EDGE('',*,*,#14904,.T.);
#19332=ORIENTED_EDGE('',*,*,#14905,.T.);
#19333=ORIENTED_EDGE('',*,*,#14906,.T.);
#19334=ORIENTED_EDGE('',*,*,#14907,.T.);
#19335=ORIENTED_EDGE('',*,*,#14908,.T.);
#19336=ORIENTED_EDGE('',*,*,#14909,.T.);
#19337=ORIENTED_EDGE('',*,*,#14910,.T.);
#19338=ORIENTED_EDGE('',*,*,#14911,.T.);
#19339=ORIENTED_EDGE('',*,*,#14912,.T.);
#19340=ORIENTED_EDGE('',*,*,#14913,.T.);
#19341=ORIENTED_EDGE('',*,*,#14914,.T.);
#19342=ORIENTED_EDGE('',*,*,#14915,.T.);
#19343=ORIENTED_EDGE('',*,*,#14916,.T.);
#19344=ORIENTED_EDGE('',*,*,#14917,.T.);
#19345=ORIENTED_EDGE('',*,*,#14918,.T.);
#19346=ORIENTED_EDGE('',*,*,#14919,.T.);
#19347=ORIENTED_EDGE('',*,*,#14920,.T.);
#19348=ORIENTED_EDGE('',*,*,#14921,.T.);
#19349=ORIENTED_EDGE('',*,*,#14922,.T.);
#19350=ORIENTED_EDGE('',*,*,#14923,.T.);
#19351=ORIENTED_EDGE('',*,*,#14924,.T.);
#19352=ORIENTED_EDGE('',*,*,#14925,.T.);
#19353=ORIENTED_EDGE('',*,*,#14926,.T.);
#19354=ORIENTED_EDGE('',*,*,#14927,.T.);
#19355=ORIENTED_EDGE('',*,*,#14928,.T.);
#19356=ORIENTED_EDGE('',*,*,#14929,.T.);
#19357=ORIENTED_EDGE('',*,*,#14930,.T.);
#19358=ORIENTED_EDGE('',*,*,#14931,.T.);
#19359=ORIENTED_EDGE('',*,*,#14932,.T.);
#19360=ORIENTED_EDGE('',*,*,#14933,.T.);
#19361=ORIENTED_EDGE('',*,*,#14934,.T.);
#19362=ORIENTED_EDGE('',*,*,#14935,.T.);
#19363=ORIENTED_EDGE('',*,*,#14936,.T.);
#19364=ORIENTED_EDGE('',*,*,#14937,.T.);
#19365=ORIENTED_EDGE('',*,*,#14938,.T.);
#19366=ORIENTED_EDGE('',*,*,#14939,.T.);
#19367=ORIENTED_EDGE('',*,*,#14940,.T.);
#19368=ORIENTED_EDGE('',*,*,#14941,.T.);
#19369=ORIENTED_EDGE('',*,*,#14942,.T.);
#19370=ORIENTED_EDGE('',*,*,#14943,.T.);
#19371=ORIENTED_EDGE('',*,*,#14944,.T.);
#19372=ORIENTED_EDGE('',*,*,#14945,.T.);
#19373=ORIENTED_EDGE('',*,*,#14946,.T.);
#19374=ORIENTED_EDGE('',*,*,#14947,.T.);
#19375=ORIENTED_EDGE('',*,*,#14948,.T.);
#19376=ORIENTED_EDGE('',*,*,#14949,.T.);
#19377=ORIENTED_EDGE('',*,*,#14950,.T.);
#19378=ORIENTED_EDGE('',*,*,#14951,.T.);
#19379=ORIENTED_EDGE('',*,*,#14952,.T.);
#19380=ORIENTED_EDGE('',*,*,#14953,.T.);
#19381=ORIENTED_EDGE('',*,*,#14954,.T.);
#19382=ORIENTED_EDGE('',*,*,#14955,.T.);
#19383=ORIENTED_EDGE('',*,*,#14956,.T.);
#19384=ORIENTED_EDGE('',*,*,#14957,.T.);
#19385=ORIENTED_EDGE('',*,*,#14958,.T.);
#19386=ORIENTED_EDGE('',*,*,#14959,.T.);
#19387=ORIENTED_EDGE('',*,*,#14960,.T.);
#19388=ORIENTED_EDGE('',*,*,#14961,.T.);
#19389=ORIENTED_EDGE('',*,*,#14962,.T.);
#19390=ORIENTED_EDGE('',*,*,#14963,.T.);
#19391=ORIENTED_EDGE('',*,*,#14964,.T.);
#19392=ORIENTED_EDGE('',*,*,#14965,.T.);
#19393=ORIENTED_EDGE('',*,*,#14966,.T.);
#19394=ORIENTED_EDGE('',*,*,#14967,.T.);
#19395=ORIENTED_EDGE('',*,*,#14968,.T.);
#19396=ORIENTED_EDGE('',*,*,#14969,.T.);
#19397=ORIENTED_EDGE('',*,*,#14970,.T.);
#19398=ORIENTED_EDGE('',*,*,#14971,.T.);
#19399=ORIENTED_EDGE('',*,*,#14972,.T.);
#19400=ORIENTED_EDGE('',*,*,#14973,.T.);
#19401=ORIENTED_EDGE('',*,*,#14974,.T.);
#19402=ORIENTED_EDGE('',*,*,#14975,.T.);
#19403=ORIENTED_EDGE('',*,*,#14976,.T.);
#19404=ORIENTED_EDGE('',*,*,#14977,.T.);
#19405=ORIENTED_EDGE('',*,*,#14978,.T.);
#19406=ORIENTED_EDGE('',*,*,#14979,.T.);
#19407=ORIENTED_EDGE('',*,*,#14980,.T.);
#19408=ORIENTED_EDGE('',*,*,#14981,.T.);
#19409=ORIENTED_EDGE('',*,*,#14982,.T.);
#19410=ORIENTED_EDGE('',*,*,#14983,.T.);
#19411=ORIENTED_EDGE('',*,*,#14984,.T.);
#19412=ORIENTED_EDGE('',*,*,#14985,.T.);
#19413=ORIENTED_EDGE('',*,*,#14986,.T.);
#19414=ORIENTED_EDGE('',*,*,#14987,.T.);
#19415=ORIENTED_EDGE('',*,*,#14988,.T.);
#19416=ORIENTED_EDGE('',*,*,#14989,.T.);
#19417=ORIENTED_EDGE('',*,*,#14990,.T.);
#19418=ORIENTED_EDGE('',*,*,#14991,.T.);
#19419=ORIENTED_EDGE('',*,*,#14992,.T.);
#19420=ORIENTED_EDGE('',*,*,#14993,.T.);
#19421=ORIENTED_EDGE('',*,*,#14994,.T.);
#19422=ORIENTED_EDGE('',*,*,#14995,.T.);
#19423=ORIENTED_EDGE('',*,*,#14996,.T.);
#19424=ORIENTED_EDGE('',*,*,#14997,.T.);
#19425=ORIENTED_EDGE('',*,*,#14998,.T.);
#19426=ORIENTED_EDGE('',*,*,#14999,.T.);
#19427=ORIENTED_EDGE('',*,*,#15000,.T.);
#19428=ORIENTED_EDGE('',*,*,#15001,.T.);
#19429=ORIENTED_EDGE('',*,*,#15002,.T.);
#19430=ORIENTED_EDGE('',*,*,#15003,.T.);
#19431=ORIENTED_EDGE('',*,*,#15004,.T.);
#19432=ORIENTED_EDGE('',*,*,#15005,.T.);
#19433=ORIENTED_EDGE('',*,*,#15006,.T.);
#19434=ORIENTED_EDGE('',*,*,#15007,.T.);
#19435=ORIENTED_EDGE('',*,*,#15008,.T.);
#19436=ORIENTED_EDGE('',*,*,#15009,.T.);
#19437=ORIENTED_EDGE('',*,*,#15010,.T.);
#19438=ORIENTED_EDGE('',*,*,#15011,.T.);
#19439=ORIENTED_EDGE('',*,*,#15012,.T.);
#19440=ORIENTED_EDGE('',*,*,#15013,.T.);
#19441=ORIENTED_EDGE('',*,*,#15014,.T.);
#19442=ORIENTED_EDGE('',*,*,#15015,.T.);
#19443=ORIENTED_EDGE('',*,*,#15016,.T.);
#19444=ORIENTED_EDGE('',*,*,#15017,.T.);
#19445=ORIENTED_EDGE('',*,*,#15018,.T.);
#19446=ORIENTED_EDGE('',*,*,#15019,.T.);
#19447=ORIENTED_EDGE('',*,*,#15020,.T.);
#19448=ORIENTED_EDGE('',*,*,#15021,.T.);
#19449=ORIENTED_EDGE('',*,*,#15022,.T.);
#19450=ORIENTED_EDGE('',*,*,#15023,.T.);
#19451=ORIENTED_EDGE('',*,*,#15024,.T.);
#19452=ORIENTED_EDGE('',*,*,#15025,.T.);
#19453=ORIENTED_EDGE('',*,*,#15026,.T.);
#19454=ORIENTED_EDGE('',*,*,#15027,.T.);
#19455=ORIENTED_EDGE('',*,*,#15028,.T.);
#19456=ORIENTED_EDGE('',*,*,#15029,.T.);
#19457=ORIENTED_EDGE('',*,*,#15030,.T.);
#19458=ORIENTED_EDGE('',*,*,#15031,.T.);
#19459=ORIENTED_EDGE('',*,*,#15032,.T.);
#19460=ORIENTED_EDGE('',*,*,#15033,.T.);
#19461=ORIENTED_EDGE('',*,*,#15034,.T.);
#19462=ORIENTED_EDGE('',*,*,#15035,.T.);
#19463=ORIENTED_EDGE('',*,*,#15036,.T.);
#19464=ORIENTED_EDGE('',*,*,#15037,.T.);
#19465=ORIENTED_EDGE('',*,*,#15038,.T.);
#19466=ORIENTED_EDGE('',*,*,#15039,.T.);
#19467=ORIENTED_EDGE('',*,*,#15040,.T.);
#19468=ORIENTED_EDGE('',*,*,#15041,.T.);
#19469=ORIENTED_EDGE('',*,*,#15042,.T.);
#19470=ORIENTED_EDGE('',*,*,#15043,.T.);
#19471=ORIENTED_EDGE('',*,*,#15044,.T.);
#19472=ORIENTED_EDGE('',*,*,#15045,.T.);
#19473=ORIENTED_EDGE('',*,*,#14880,.T.);
#19474=ORIENTED_EDGE('',*,*,#14884,.T.);
#19475=ORIENTED_EDGE('',*,*,#15046,.T.);
#19476=ORIENTED_EDGE('',*,*,#15045,.F.);
#19477=ORIENTED_EDGE('',*,*,#15047,.T.);
#19478=ORIENTED_EDGE('',*,*,#15048,.T.);
#19479=ORIENTED_EDGE('',*,*,#15049,.T.);
#19480=ORIENTED_EDGE('',*,*,#14881,.T.);
#19481=ORIENTED_EDGE('',*,*,#15050,.T.);
#19482=ORIENTED_EDGE('',*,*,#15051,.T.);
#19483=ORIENTED_EDGE('',*,*,#15052,.T.);
#19484=ORIENTED_EDGE('',*,*,#15051,.F.);
#19485=ORIENTED_EDGE('',*,*,#15053,.F.);
#19486=ORIENTED_EDGE('',*,*,#15054,.F.);
#19487=ORIENTED_EDGE('',*,*,#15055,.F.);
#19488=ORIENTED_EDGE('',*,*,#15056,.T.);
#19489=ORIENTED_EDGE('',*,*,#15057,.F.);
#19490=ORIENTED_EDGE('',*,*,#15050,.F.);
#19491=ORIENTED_EDGE('',*,*,#15052,.F.);
#19492=ORIENTED_EDGE('',*,*,#15058,.T.);
#19493=ORIENTED_EDGE('',*,*,#15059,.T.);
#19494=ORIENTED_EDGE('',*,*,#15058,.F.);
#19495=ORIENTED_EDGE('',*,*,#15057,.T.);
#19496=ORIENTED_EDGE('',*,*,#15060,.T.);
#19497=ORIENTED_EDGE('',*,*,#15061,.T.);
#19498=ORIENTED_EDGE('',*,*,#15060,.F.);
#19499=ORIENTED_EDGE('',*,*,#15061,.F.);
#19500=ORIENTED_EDGE('',*,*,#15062,.T.);
#19501=ORIENTED_EDGE('',*,*,#15063,.T.);
#19502=ORIENTED_EDGE('',*,*,#15062,.F.);
#19503=ORIENTED_EDGE('',*,*,#15064,.T.);
#19504=ORIENTED_EDGE('',*,*,#15065,.T.);
#19505=ORIENTED_EDGE('',*,*,#15066,.T.);
#19506=ORIENTED_EDGE('',*,*,#15065,.F.);
#19507=ORIENTED_EDGE('',*,*,#15064,.F.);
#19508=ORIENTED_EDGE('',*,*,#15067,.T.);
#19509=ORIENTED_EDGE('',*,*,#15068,.F.);
#19510=ORIENTED_EDGE('',*,*,#15067,.F.);
#19511=ORIENTED_EDGE('',*,*,#15069,.F.);
#19512=ORIENTED_EDGE('',*,*,#15066,.F.);
#19513=ORIENTED_EDGE('',*,*,#15070,.T.);
#19514=ORIENTED_EDGE('',*,*,#15071,.T.);
#19515=ORIENTED_EDGE('',*,*,#15072,.T.);
#19516=ORIENTED_EDGE('',*,*,#15071,.F.);
#19517=ORIENTED_EDGE('',*,*,#15070,.F.);
#19518=ORIENTED_EDGE('',*,*,#15073,.T.);
#19519=ORIENTED_EDGE('',*,*,#15074,.F.);
#19520=ORIENTED_EDGE('',*,*,#15073,.F.);
#19521=ORIENTED_EDGE('',*,*,#15075,.F.);
#19522=ORIENTED_EDGE('',*,*,#15072,.F.);
#19523=ORIENTED_EDGE('',*,*,#15076,.T.);
#19524=ORIENTED_EDGE('',*,*,#15077,.T.);
#19525=ORIENTED_EDGE('',*,*,#15078,.T.);
#19526=ORIENTED_EDGE('',*,*,#15077,.F.);
#19527=ORIENTED_EDGE('',*,*,#15076,.F.);
#19528=ORIENTED_EDGE('',*,*,#15079,.T.);
#19529=ORIENTED_EDGE('',*,*,#15080,.F.);
#19530=ORIENTED_EDGE('',*,*,#15079,.F.);
#19531=ORIENTED_EDGE('',*,*,#15081,.F.);
#19532=ORIENTED_EDGE('',*,*,#15078,.F.);
#19533=ORIENTED_EDGE('',*,*,#15082,.T.);
#19534=ORIENTED_EDGE('',*,*,#15083,.T.);
#19535=ORIENTED_EDGE('',*,*,#15084,.T.);
#19536=ORIENTED_EDGE('',*,*,#15083,.F.);
#19537=ORIENTED_EDGE('',*,*,#15082,.F.);
#19538=ORIENTED_EDGE('',*,*,#15085,.T.);
#19539=ORIENTED_EDGE('',*,*,#15086,.F.);
#19540=ORIENTED_EDGE('',*,*,#15085,.F.);
#19541=ORIENTED_EDGE('',*,*,#15087,.F.);
#19542=ORIENTED_EDGE('',*,*,#15084,.F.);
#19543=ORIENTED_EDGE('',*,*,#14872,.F.);
#19544=ORIENTED_EDGE('',*,*,#14867,.F.);
#19545=ORIENTED_EDGE('',*,*,#15088,.T.);
#19546=ORIENTED_EDGE('',*,*,#15089,.T.);
#19547=ORIENTED_EDGE('',*,*,#15046,.F.);
#19548=ORIENTED_EDGE('',*,*,#14883,.T.);
#19549=ORIENTED_EDGE('',*,*,#15043,.F.);
#19550=ORIENTED_EDGE('',*,*,#15089,.F.);
#19551=ORIENTED_EDGE('',*,*,#15090,.T.);
#19552=ORIENTED_EDGE('',*,*,#15091,.T.);
#19553=ORIENTED_EDGE('',*,*,#15092,.T.);
#19554=ORIENTED_EDGE('',*,*,#14870,.F.);
#19555=ORIENTED_EDGE('',*,*,#15093,.F.);
#19556=ORIENTED_EDGE('',*,*,#15094,.F.);
#19557=ORIENTED_EDGE('',*,*,#15095,.F.);
#19558=ORIENTED_EDGE('',*,*,#15096,.F.);
#19559=ORIENTED_EDGE('',*,*,#15097,.F.);
#19560=ORIENTED_EDGE('',*,*,#15098,.F.);
#19561=ORIENTED_EDGE('',*,*,#15099,.F.);
#19562=ORIENTED_EDGE('',*,*,#15100,.F.);
#19563=ORIENTED_EDGE('',*,*,#15101,.F.);
#19564=ORIENTED_EDGE('',*,*,#15102,.F.);
#19565=ORIENTED_EDGE('',*,*,#15103,.F.);
#19566=ORIENTED_EDGE('',*,*,#15102,.T.);
#19567=ORIENTED_EDGE('',*,*,#15104,.T.);
#19568=ORIENTED_EDGE('',*,*,#15100,.T.);
#19569=ORIENTED_EDGE('',*,*,#15105,.T.);
#19570=ORIENTED_EDGE('',*,*,#15055,.T.);
#19571=ORIENTED_EDGE('',*,*,#15103,.T.);
#19572=ORIENTED_EDGE('',*,*,#15106,.T.);
#19573=ORIENTED_EDGE('',*,*,#15048,.F.);
#19574=ORIENTED_EDGE('',*,*,#15096,.T.);
#19575=ORIENTED_EDGE('',*,*,#15107,.T.);
#19576=ORIENTED_EDGE('',*,*,#15101,.T.);
#19577=ORIENTED_EDGE('',*,*,#15054,.T.);
#19578=ORIENTED_EDGE('',*,*,#14859,.F.);
#19579=ORIENTED_EDGE('',*,*,#14878,.F.);
#19580=ORIENTED_EDGE('',*,*,#15108,.T.);
#19581=ORIENTED_EDGE('',*,*,#15099,.T.);
#19582=ORIENTED_EDGE('',*,*,#15109,.T.);
#19583=ORIENTED_EDGE('',*,*,#15093,.T.);
#19584=ORIENTED_EDGE('',*,*,#15110,.T.);
#19585=ORIENTED_EDGE('',*,*,#15098,.T.);
#19586=ORIENTED_EDGE('',*,*,#15111,.T.);
#19587=ORIENTED_EDGE('',*,*,#15112,.T.);
#19588=ORIENTED_EDGE('',*,*,#15097,.T.);
#19589=ORIENTED_EDGE('',*,*,#15053,.T.);
#19590=ORIENTED_EDGE('',*,*,#15091,.F.);
#19591=ORIENTED_EDGE('',*,*,#15095,.T.);
#19592=ORIENTED_EDGE('',*,*,#15113,.T.);
#19593=ORIENTED_EDGE('',*,*,#15094,.T.);
#19594=ORIENTED_EDGE('',*,*,#15114,.T.);
#19595=ORIENTED_EDGE('',*,*,#15044,.F.);
#19596=ORIENTED_EDGE('',*,*,#15092,.F.);
#19597=ORIENTED_EDGE('',*,*,#15056,.F.);
#19598=ORIENTED_EDGE('',*,*,#15047,.F.);
#19599=ORIENTED_EDGE('',*,*,#15088,.F.);
#19600=ORIENTED_EDGE('',*,*,#14866,.F.);
#19601=ORIENTED_EDGE('',*,*,#14871,.F.);
#19602=ORIENTED_EDGE('',*,*,#15113,.F.);
#19603=ORIENTED_EDGE('',*,*,#15112,.F.);
#19604=ORIENTED_EDGE('',*,*,#15090,.F.);
#19605=ORIENTED_EDGE('',*,*,#15115,.F.);
#19606=ORIENTED_EDGE('',*,*,#15116,.F.);
#19607=ORIENTED_EDGE('',*,*,#15117,.F.);
#19608=ORIENTED_EDGE('',*,*,#15118,.F.);
#19609=ORIENTED_EDGE('',*,*,#15119,.F.);
#19610=ORIENTED_EDGE('',*,*,#15120,.F.);
#19611=ORIENTED_EDGE('',*,*,#15121,.F.);
#19612=ORIENTED_EDGE('',*,*,#15122,.F.);
#19613=ORIENTED_EDGE('',*,*,#15123,.T.);
#19614=ORIENTED_EDGE('',*,*,#15124,.F.);
#19615=ORIENTED_EDGE('',*,*,#15125,.F.);
#19616=ORIENTED_EDGE('',*,*,#15126,.F.);
#19617=ORIENTED_EDGE('',*,*,#15127,.F.);
#19618=ORIENTED_EDGE('',*,*,#15128,.F.);
#19619=ORIENTED_EDGE('',*,*,#15129,.F.);
#19620=ORIENTED_EDGE('',*,*,#15130,.F.);
#19621=ORIENTED_EDGE('',*,*,#15131,.F.);
#19622=ORIENTED_EDGE('',*,*,#15104,.F.);
#19623=ORIENTED_EDGE('',*,*,#15107,.F.);
#19624=ORIENTED_EDGE('',*,*,#15114,.F.);
#19625=ORIENTED_EDGE('',*,*,#15111,.F.);
#19626=ORIENTED_EDGE('',*,*,#15049,.F.);
#19627=ORIENTED_EDGE('',*,*,#15106,.F.);
#19628=ORIENTED_EDGE('',*,*,#15105,.F.);
#19629=ORIENTED_EDGE('',*,*,#15108,.F.);
#19630=ORIENTED_EDGE('',*,*,#14877,.F.);
#19631=ORIENTED_EDGE('',*,*,#14882,.F.);
#19632=ORIENTED_EDGE('',*,*,#15132,.F.);
#19633=ORIENTED_EDGE('',*,*,#15133,.F.);
#19634=ORIENTED_EDGE('',*,*,#15134,.F.);
#19635=ORIENTED_EDGE('',*,*,#15135,.F.);
#19636=ORIENTED_EDGE('',*,*,#15136,.F.);
#19637=ORIENTED_EDGE('',*,*,#14885,.F.);
#19638=ORIENTED_EDGE('',*,*,#15137,.T.);
#19639=ORIENTED_EDGE('',*,*,#15138,.T.);
#19640=ORIENTED_EDGE('',*,*,#15139,.F.);
#19641=ORIENTED_EDGE('',*,*,#14896,.F.);
#19642=ORIENTED_EDGE('',*,*,#15140,.T.);
#19643=ORIENTED_EDGE('',*,*,#15141,.T.);
#19644=ORIENTED_EDGE('',*,*,#15137,.F.);
#19645=ORIENTED_EDGE('',*,*,#14895,.F.);
#19646=ORIENTED_EDGE('',*,*,#15142,.T.);
#19647=ORIENTED_EDGE('',*,*,#15143,.T.);
#19648=ORIENTED_EDGE('',*,*,#15140,.F.);
#19649=ORIENTED_EDGE('',*,*,#14894,.F.);
#19650=ORIENTED_EDGE('',*,*,#15144,.T.);
#19651=ORIENTED_EDGE('',*,*,#15145,.T.);
#19652=ORIENTED_EDGE('',*,*,#15142,.F.);
#19653=ORIENTED_EDGE('',*,*,#14893,.F.);
#19654=ORIENTED_EDGE('',*,*,#15146,.T.);
#19655=ORIENTED_EDGE('',*,*,#15147,.T.);
#19656=ORIENTED_EDGE('',*,*,#15144,.F.);
#19657=ORIENTED_EDGE('',*,*,#14892,.F.);
#19658=ORIENTED_EDGE('',*,*,#15148,.T.);
#19659=ORIENTED_EDGE('',*,*,#15149,.T.);
#19660=ORIENTED_EDGE('',*,*,#15146,.F.);
#19661=ORIENTED_EDGE('',*,*,#14891,.F.);
#19662=ORIENTED_EDGE('',*,*,#15150,.T.);
#19663=ORIENTED_EDGE('',*,*,#15151,.T.);
#19664=ORIENTED_EDGE('',*,*,#15148,.F.);
#19665=ORIENTED_EDGE('',*,*,#14890,.F.);
#19666=ORIENTED_EDGE('',*,*,#15152,.T.);
#19667=ORIENTED_EDGE('',*,*,#15153,.T.);
#19668=ORIENTED_EDGE('',*,*,#15150,.F.);
#19669=ORIENTED_EDGE('',*,*,#14889,.F.);
#19670=ORIENTED_EDGE('',*,*,#15154,.T.);
#19671=ORIENTED_EDGE('',*,*,#15155,.T.);
#19672=ORIENTED_EDGE('',*,*,#15152,.F.);
#19673=ORIENTED_EDGE('',*,*,#14888,.F.);
#19674=ORIENTED_EDGE('',*,*,#15156,.T.);
#19675=ORIENTED_EDGE('',*,*,#15157,.T.);
#19676=ORIENTED_EDGE('',*,*,#15154,.F.);
#19677=ORIENTED_EDGE('',*,*,#14887,.F.);
#19678=ORIENTED_EDGE('',*,*,#15158,.T.);
#19679=ORIENTED_EDGE('',*,*,#15159,.T.);
#19680=ORIENTED_EDGE('',*,*,#15156,.F.);
#19681=ORIENTED_EDGE('',*,*,#14886,.F.);
#19682=ORIENTED_EDGE('',*,*,#15139,.T.);
#19683=ORIENTED_EDGE('',*,*,#15160,.T.);
#19684=ORIENTED_EDGE('',*,*,#15158,.F.);
#19685=ORIENTED_EDGE('',*,*,#15160,.F.);
#19686=ORIENTED_EDGE('',*,*,#15138,.F.);
#19687=ORIENTED_EDGE('',*,*,#15141,.F.);
#19688=ORIENTED_EDGE('',*,*,#15143,.F.);
#19689=ORIENTED_EDGE('',*,*,#15145,.F.);
#19690=ORIENTED_EDGE('',*,*,#15147,.F.);
#19691=ORIENTED_EDGE('',*,*,#15149,.F.);
#19692=ORIENTED_EDGE('',*,*,#15151,.F.);
#19693=ORIENTED_EDGE('',*,*,#15153,.F.);
#19694=ORIENTED_EDGE('',*,*,#15155,.F.);
#19695=ORIENTED_EDGE('',*,*,#15157,.F.);
#19696=ORIENTED_EDGE('',*,*,#15159,.F.);
#19697=ORIENTED_EDGE('',*,*,#14897,.F.);
#19698=ORIENTED_EDGE('',*,*,#15161,.T.);
#19699=ORIENTED_EDGE('',*,*,#15162,.T.);
#19700=ORIENTED_EDGE('',*,*,#15163,.F.);
#19701=ORIENTED_EDGE('',*,*,#14915,.F.);
#19702=ORIENTED_EDGE('',*,*,#15164,.T.);
#19703=ORIENTED_EDGE('',*,*,#15165,.T.);
#19704=ORIENTED_EDGE('',*,*,#15161,.F.);
#19705=ORIENTED_EDGE('',*,*,#14914,.F.);
#19706=ORIENTED_EDGE('',*,*,#15166,.T.);
#19707=ORIENTED_EDGE('',*,*,#15167,.T.);
#19708=ORIENTED_EDGE('',*,*,#15164,.F.);
#19709=ORIENTED_EDGE('',*,*,#14913,.F.);
#19710=ORIENTED_EDGE('',*,*,#15168,.T.);
#19711=ORIENTED_EDGE('',*,*,#15169,.T.);
#19712=ORIENTED_EDGE('',*,*,#15166,.F.);
#19713=ORIENTED_EDGE('',*,*,#14912,.F.);
#19714=ORIENTED_EDGE('',*,*,#15170,.T.);
#19715=ORIENTED_EDGE('',*,*,#15171,.T.);
#19716=ORIENTED_EDGE('',*,*,#15168,.F.);
#19717=ORIENTED_EDGE('',*,*,#14911,.F.);
#19718=ORIENTED_EDGE('',*,*,#15172,.T.);
#19719=ORIENTED_EDGE('',*,*,#15173,.T.);
#19720=ORIENTED_EDGE('',*,*,#15170,.F.);
#19721=ORIENTED_EDGE('',*,*,#14910,.F.);
#19722=ORIENTED_EDGE('',*,*,#15174,.T.);
#19723=ORIENTED_EDGE('',*,*,#15175,.T.);
#19724=ORIENTED_EDGE('',*,*,#15172,.F.);
#19725=ORIENTED_EDGE('',*,*,#14909,.F.);
#19726=ORIENTED_EDGE('',*,*,#15176,.T.);
#19727=ORIENTED_EDGE('',*,*,#15177,.T.);
#19728=ORIENTED_EDGE('',*,*,#15174,.F.);
#19729=ORIENTED_EDGE('',*,*,#14908,.F.);
#19730=ORIENTED_EDGE('',*,*,#15178,.T.);
#19731=ORIENTED_EDGE('',*,*,#15179,.T.);
#19732=ORIENTED_EDGE('',*,*,#15176,.F.);
#19733=ORIENTED_EDGE('',*,*,#14907,.F.);
#19734=ORIENTED_EDGE('',*,*,#15180,.T.);
#19735=ORIENTED_EDGE('',*,*,#15181,.T.);
#19736=ORIENTED_EDGE('',*,*,#15178,.F.);
#19737=ORIENTED_EDGE('',*,*,#14906,.F.);
#19738=ORIENTED_EDGE('',*,*,#15182,.T.);
#19739=ORIENTED_EDGE('',*,*,#15183,.T.);
#19740=ORIENTED_EDGE('',*,*,#15180,.F.);
#19741=ORIENTED_EDGE('',*,*,#14905,.F.);
#19742=ORIENTED_EDGE('',*,*,#15184,.T.);
#19743=ORIENTED_EDGE('',*,*,#15185,.T.);
#19744=ORIENTED_EDGE('',*,*,#15182,.F.);
#19745=ORIENTED_EDGE('',*,*,#14904,.F.);
#19746=ORIENTED_EDGE('',*,*,#15186,.T.);
#19747=ORIENTED_EDGE('',*,*,#15187,.T.);
#19748=ORIENTED_EDGE('',*,*,#15184,.F.);
#19749=ORIENTED_EDGE('',*,*,#14903,.F.);
#19750=ORIENTED_EDGE('',*,*,#15188,.T.);
#19751=ORIENTED_EDGE('',*,*,#15189,.T.);
#19752=ORIENTED_EDGE('',*,*,#15186,.F.);
#19753=ORIENTED_EDGE('',*,*,#14902,.F.);
#19754=ORIENTED_EDGE('',*,*,#15190,.T.);
#19755=ORIENTED_EDGE('',*,*,#15191,.T.);
#19756=ORIENTED_EDGE('',*,*,#15188,.F.);
#19757=ORIENTED_EDGE('',*,*,#14901,.F.);
#19758=ORIENTED_EDGE('',*,*,#15192,.T.);
#19759=ORIENTED_EDGE('',*,*,#15193,.T.);
#19760=ORIENTED_EDGE('',*,*,#15190,.F.);
#19761=ORIENTED_EDGE('',*,*,#14900,.F.);
#19762=ORIENTED_EDGE('',*,*,#15194,.T.);
#19763=ORIENTED_EDGE('',*,*,#15195,.T.);
#19764=ORIENTED_EDGE('',*,*,#15192,.F.);
#19765=ORIENTED_EDGE('',*,*,#14899,.F.);
#19766=ORIENTED_EDGE('',*,*,#15196,.T.);
#19767=ORIENTED_EDGE('',*,*,#15197,.T.);
#19768=ORIENTED_EDGE('',*,*,#15194,.F.);
#19769=ORIENTED_EDGE('',*,*,#14898,.F.);
#19770=ORIENTED_EDGE('',*,*,#15163,.T.);
#19771=ORIENTED_EDGE('',*,*,#15198,.T.);
#19772=ORIENTED_EDGE('',*,*,#15196,.F.);
#19773=ORIENTED_EDGE('',*,*,#15198,.F.);
#19774=ORIENTED_EDGE('',*,*,#15162,.F.);
#19775=ORIENTED_EDGE('',*,*,#15165,.F.);
#19776=ORIENTED_EDGE('',*,*,#15167,.F.);
#19777=ORIENTED_EDGE('',*,*,#15169,.F.);
#19778=ORIENTED_EDGE('',*,*,#15171,.F.);
#19779=ORIENTED_EDGE('',*,*,#15173,.F.);
#19780=ORIENTED_EDGE('',*,*,#15175,.F.);
#19781=ORIENTED_EDGE('',*,*,#15177,.F.);
#19782=ORIENTED_EDGE('',*,*,#15179,.F.);
#19783=ORIENTED_EDGE('',*,*,#15181,.F.);
#19784=ORIENTED_EDGE('',*,*,#15183,.F.);
#19785=ORIENTED_EDGE('',*,*,#15185,.F.);
#19786=ORIENTED_EDGE('',*,*,#15187,.F.);
#19787=ORIENTED_EDGE('',*,*,#15189,.F.);
#19788=ORIENTED_EDGE('',*,*,#15191,.F.);
#19789=ORIENTED_EDGE('',*,*,#15193,.F.);
#19790=ORIENTED_EDGE('',*,*,#15195,.F.);
#19791=ORIENTED_EDGE('',*,*,#15197,.F.);
#19792=ORIENTED_EDGE('',*,*,#14916,.F.);
#19793=ORIENTED_EDGE('',*,*,#15199,.T.);
#19794=ORIENTED_EDGE('',*,*,#15200,.T.);
#19795=ORIENTED_EDGE('',*,*,#15201,.F.);
#19796=ORIENTED_EDGE('',*,*,#14927,.F.);
#19797=ORIENTED_EDGE('',*,*,#15202,.T.);
#19798=ORIENTED_EDGE('',*,*,#15203,.T.);
#19799=ORIENTED_EDGE('',*,*,#15199,.F.);
#19800=ORIENTED_EDGE('',*,*,#14926,.F.);
#19801=ORIENTED_EDGE('',*,*,#15204,.T.);
#19802=ORIENTED_EDGE('',*,*,#15205,.T.);
#19803=ORIENTED_EDGE('',*,*,#15202,.F.);
#19804=ORIENTED_EDGE('',*,*,#14925,.F.);
#19805=ORIENTED_EDGE('',*,*,#15206,.T.);
#19806=ORIENTED_EDGE('',*,*,#15207,.T.);
#19807=ORIENTED_EDGE('',*,*,#15204,.F.);
#19808=ORIENTED_EDGE('',*,*,#14924,.F.);
#19809=ORIENTED_EDGE('',*,*,#15208,.T.);
#19810=ORIENTED_EDGE('',*,*,#15209,.T.);
#19811=ORIENTED_EDGE('',*,*,#15206,.F.);
#19812=ORIENTED_EDGE('',*,*,#14923,.F.);
#19813=ORIENTED_EDGE('',*,*,#15210,.T.);
#19814=ORIENTED_EDGE('',*,*,#15211,.T.);
#19815=ORIENTED_EDGE('',*,*,#15208,.F.);
#19816=ORIENTED_EDGE('',*,*,#14922,.F.);
#19817=ORIENTED_EDGE('',*,*,#15212,.T.);
#19818=ORIENTED_EDGE('',*,*,#15213,.T.);
#19819=ORIENTED_EDGE('',*,*,#15210,.F.);
#19820=ORIENTED_EDGE('',*,*,#14921,.F.);
#19821=ORIENTED_EDGE('',*,*,#15214,.T.);
#19822=ORIENTED_EDGE('',*,*,#15215,.T.);
#19823=ORIENTED_EDGE('',*,*,#15212,.F.);
#19824=ORIENTED_EDGE('',*,*,#14920,.F.);
#19825=ORIENTED_EDGE('',*,*,#15216,.T.);
#19826=ORIENTED_EDGE('',*,*,#15217,.T.);
#19827=ORIENTED_EDGE('',*,*,#15214,.F.);
#19828=ORIENTED_EDGE('',*,*,#14919,.F.);
#19829=ORIENTED_EDGE('',*,*,#15218,.T.);
#19830=ORIENTED_EDGE('',*,*,#15219,.T.);
#19831=ORIENTED_EDGE('',*,*,#15216,.F.);
#19832=ORIENTED_EDGE('',*,*,#14918,.F.);
#19833=ORIENTED_EDGE('',*,*,#15220,.T.);
#19834=ORIENTED_EDGE('',*,*,#15221,.T.);
#19835=ORIENTED_EDGE('',*,*,#15218,.F.);
#19836=ORIENTED_EDGE('',*,*,#14917,.F.);
#19837=ORIENTED_EDGE('',*,*,#15201,.T.);
#19838=ORIENTED_EDGE('',*,*,#15222,.T.);
#19839=ORIENTED_EDGE('',*,*,#15220,.F.);
#19840=ORIENTED_EDGE('',*,*,#15222,.F.);
#19841=ORIENTED_EDGE('',*,*,#15200,.F.);
#19842=ORIENTED_EDGE('',*,*,#15203,.F.);
#19843=ORIENTED_EDGE('',*,*,#15205,.F.);
#19844=ORIENTED_EDGE('',*,*,#15207,.F.);
#19845=ORIENTED_EDGE('',*,*,#15209,.F.);
#19846=ORIENTED_EDGE('',*,*,#15211,.F.);
#19847=ORIENTED_EDGE('',*,*,#15213,.F.);
#19848=ORIENTED_EDGE('',*,*,#15215,.F.);
#19849=ORIENTED_EDGE('',*,*,#15217,.F.);
#19850=ORIENTED_EDGE('',*,*,#15219,.F.);
#19851=ORIENTED_EDGE('',*,*,#15221,.F.);
#19852=ORIENTED_EDGE('',*,*,#14928,.F.);
#19853=ORIENTED_EDGE('',*,*,#15223,.T.);
#19854=ORIENTED_EDGE('',*,*,#15224,.T.);
#19855=ORIENTED_EDGE('',*,*,#15225,.F.);
#19856=ORIENTED_EDGE('',*,*,#14938,.F.);
#19857=ORIENTED_EDGE('',*,*,#15226,.T.);
#19858=ORIENTED_EDGE('',*,*,#15227,.T.);
#19859=ORIENTED_EDGE('',*,*,#15223,.F.);
#19860=ORIENTED_EDGE('',*,*,#14937,.F.);
#19861=ORIENTED_EDGE('',*,*,#15228,.T.);
#19862=ORIENTED_EDGE('',*,*,#15229,.T.);
#19863=ORIENTED_EDGE('',*,*,#15226,.F.);
#19864=ORIENTED_EDGE('',*,*,#14936,.F.);
#19865=ORIENTED_EDGE('',*,*,#15230,.T.);
#19866=ORIENTED_EDGE('',*,*,#15231,.T.);
#19867=ORIENTED_EDGE('',*,*,#15228,.F.);
#19868=ORIENTED_EDGE('',*,*,#14935,.F.);
#19869=ORIENTED_EDGE('',*,*,#15232,.T.);
#19870=ORIENTED_EDGE('',*,*,#15233,.T.);
#19871=ORIENTED_EDGE('',*,*,#15230,.F.);
#19872=ORIENTED_EDGE('',*,*,#14934,.F.);
#19873=ORIENTED_EDGE('',*,*,#15234,.T.);
#19874=ORIENTED_EDGE('',*,*,#15235,.T.);
#19875=ORIENTED_EDGE('',*,*,#15232,.F.);
#19876=ORIENTED_EDGE('',*,*,#14933,.F.);
#19877=ORIENTED_EDGE('',*,*,#15236,.T.);
#19878=ORIENTED_EDGE('',*,*,#15237,.T.);
#19879=ORIENTED_EDGE('',*,*,#15234,.F.);
#19880=ORIENTED_EDGE('',*,*,#14932,.F.);
#19881=ORIENTED_EDGE('',*,*,#15238,.T.);
#19882=ORIENTED_EDGE('',*,*,#15239,.T.);
#19883=ORIENTED_EDGE('',*,*,#15236,.F.);
#19884=ORIENTED_EDGE('',*,*,#14931,.F.);
#19885=ORIENTED_EDGE('',*,*,#15240,.T.);
#19886=ORIENTED_EDGE('',*,*,#15241,.T.);
#19887=ORIENTED_EDGE('',*,*,#15238,.F.);
#19888=ORIENTED_EDGE('',*,*,#14930,.F.);
#19889=ORIENTED_EDGE('',*,*,#15242,.T.);
#19890=ORIENTED_EDGE('',*,*,#15243,.T.);
#19891=ORIENTED_EDGE('',*,*,#15240,.F.);
#19892=ORIENTED_EDGE('',*,*,#14929,.F.);
#19893=ORIENTED_EDGE('',*,*,#15225,.T.);
#19894=ORIENTED_EDGE('',*,*,#15244,.T.);
#19895=ORIENTED_EDGE('',*,*,#15242,.F.);
#19896=ORIENTED_EDGE('',*,*,#15244,.F.);
#19897=ORIENTED_EDGE('',*,*,#15224,.F.);
#19898=ORIENTED_EDGE('',*,*,#15227,.F.);
#19899=ORIENTED_EDGE('',*,*,#15229,.F.);
#19900=ORIENTED_EDGE('',*,*,#15231,.F.);
#19901=ORIENTED_EDGE('',*,*,#15233,.F.);
#19902=ORIENTED_EDGE('',*,*,#15235,.F.);
#19903=ORIENTED_EDGE('',*,*,#15237,.F.);
#19904=ORIENTED_EDGE('',*,*,#15239,.F.);
#19905=ORIENTED_EDGE('',*,*,#15241,.F.);
#19906=ORIENTED_EDGE('',*,*,#15243,.F.);
#19907=ORIENTED_EDGE('',*,*,#14939,.F.);
#19908=ORIENTED_EDGE('',*,*,#15245,.T.);
#19909=ORIENTED_EDGE('',*,*,#15246,.T.);
#19910=ORIENTED_EDGE('',*,*,#15247,.F.);
#19911=ORIENTED_EDGE('',*,*,#14973,.F.);
#19912=ORIENTED_EDGE('',*,*,#15248,.T.);
#19913=ORIENTED_EDGE('',*,*,#15249,.T.);
#19914=ORIENTED_EDGE('',*,*,#15245,.F.);
#19915=ORIENTED_EDGE('',*,*,#14972,.F.);
#19916=ORIENTED_EDGE('',*,*,#15250,.T.);
#19917=ORIENTED_EDGE('',*,*,#15251,.T.);
#19918=ORIENTED_EDGE('',*,*,#15248,.F.);
#19919=ORIENTED_EDGE('',*,*,#14971,.F.);
#19920=ORIENTED_EDGE('',*,*,#15252,.T.);
#19921=ORIENTED_EDGE('',*,*,#15253,.T.);
#19922=ORIENTED_EDGE('',*,*,#15250,.F.);
#19923=ORIENTED_EDGE('',*,*,#14970,.F.);
#19924=ORIENTED_EDGE('',*,*,#15254,.T.);
#19925=ORIENTED_EDGE('',*,*,#15255,.T.);
#19926=ORIENTED_EDGE('',*,*,#15252,.F.);
#19927=ORIENTED_EDGE('',*,*,#14969,.F.);
#19928=ORIENTED_EDGE('',*,*,#15256,.T.);
#19929=ORIENTED_EDGE('',*,*,#15257,.T.);
#19930=ORIENTED_EDGE('',*,*,#15254,.F.);
#19931=ORIENTED_EDGE('',*,*,#14968,.F.);
#19932=ORIENTED_EDGE('',*,*,#15258,.T.);
#19933=ORIENTED_EDGE('',*,*,#15259,.T.);
#19934=ORIENTED_EDGE('',*,*,#15256,.F.);
#19935=ORIENTED_EDGE('',*,*,#14967,.F.);
#19936=ORIENTED_EDGE('',*,*,#15260,.T.);
#19937=ORIENTED_EDGE('',*,*,#15261,.T.);
#19938=ORIENTED_EDGE('',*,*,#15258,.F.);
#19939=ORIENTED_EDGE('',*,*,#14966,.F.);
#19940=ORIENTED_EDGE('',*,*,#15262,.T.);
#19941=ORIENTED_EDGE('',*,*,#15263,.T.);
#19942=ORIENTED_EDGE('',*,*,#15260,.F.);
#19943=ORIENTED_EDGE('',*,*,#14965,.F.);
#19944=ORIENTED_EDGE('',*,*,#15264,.T.);
#19945=ORIENTED_EDGE('',*,*,#15265,.T.);
#19946=ORIENTED_EDGE('',*,*,#15262,.F.);
#19947=ORIENTED_EDGE('',*,*,#14964,.F.);
#19948=ORIENTED_EDGE('',*,*,#15266,.T.);
#19949=ORIENTED_EDGE('',*,*,#15267,.T.);
#19950=ORIENTED_EDGE('',*,*,#15264,.F.);
#19951=ORIENTED_EDGE('',*,*,#14963,.F.);
#19952=ORIENTED_EDGE('',*,*,#15268,.T.);
#19953=ORIENTED_EDGE('',*,*,#15269,.T.);
#19954=ORIENTED_EDGE('',*,*,#15266,.F.);
#19955=ORIENTED_EDGE('',*,*,#14962,.F.);
#19956=ORIENTED_EDGE('',*,*,#15270,.T.);
#19957=ORIENTED_EDGE('',*,*,#15271,.T.);
#19958=ORIENTED_EDGE('',*,*,#15268,.F.);
#19959=ORIENTED_EDGE('',*,*,#14961,.F.);
#19960=ORIENTED_EDGE('',*,*,#15272,.T.);
#19961=ORIENTED_EDGE('',*,*,#15273,.T.);
#19962=ORIENTED_EDGE('',*,*,#15270,.F.);
#19963=ORIENTED_EDGE('',*,*,#14960,.F.);
#19964=ORIENTED_EDGE('',*,*,#15274,.T.);
#19965=ORIENTED_EDGE('',*,*,#15275,.T.);
#19966=ORIENTED_EDGE('',*,*,#15272,.F.);
#19967=ORIENTED_EDGE('',*,*,#14959,.F.);
#19968=ORIENTED_EDGE('',*,*,#15276,.T.);
#19969=ORIENTED_EDGE('',*,*,#15277,.T.);
#19970=ORIENTED_EDGE('',*,*,#15274,.F.);
#19971=ORIENTED_EDGE('',*,*,#14958,.F.);
#19972=ORIENTED_EDGE('',*,*,#15278,.T.);
#19973=ORIENTED_EDGE('',*,*,#15279,.T.);
#19974=ORIENTED_EDGE('',*,*,#15276,.F.);
#19975=ORIENTED_EDGE('',*,*,#14957,.F.);
#19976=ORIENTED_EDGE('',*,*,#15280,.T.);
#19977=ORIENTED_EDGE('',*,*,#15281,.T.);
#19978=ORIENTED_EDGE('',*,*,#15278,.F.);
#19979=ORIENTED_EDGE('',*,*,#14956,.F.);
#19980=ORIENTED_EDGE('',*,*,#15282,.T.);
#19981=ORIENTED_EDGE('',*,*,#15283,.T.);
#19982=ORIENTED_EDGE('',*,*,#15280,.F.);
#19983=ORIENTED_EDGE('',*,*,#14955,.F.);
#19984=ORIENTED_EDGE('',*,*,#15284,.T.);
#19985=ORIENTED_EDGE('',*,*,#15285,.T.);
#19986=ORIENTED_EDGE('',*,*,#15282,.F.);
#19987=ORIENTED_EDGE('',*,*,#14954,.F.);
#19988=ORIENTED_EDGE('',*,*,#15286,.T.);
#19989=ORIENTED_EDGE('',*,*,#15287,.T.);
#19990=ORIENTED_EDGE('',*,*,#15284,.F.);
#19991=ORIENTED_EDGE('',*,*,#14953,.F.);
#19992=ORIENTED_EDGE('',*,*,#15288,.T.);
#19993=ORIENTED_EDGE('',*,*,#15289,.T.);
#19994=ORIENTED_EDGE('',*,*,#15286,.F.);
#19995=ORIENTED_EDGE('',*,*,#14952,.F.);
#19996=ORIENTED_EDGE('',*,*,#15290,.T.);
#19997=ORIENTED_EDGE('',*,*,#15291,.T.);
#19998=ORIENTED_EDGE('',*,*,#15288,.F.);
#19999=ORIENTED_EDGE('',*,*,#14951,.F.);
#20000=ORIENTED_EDGE('',*,*,#15292,.T.);
#20001=ORIENTED_EDGE('',*,*,#15293,.T.);
#20002=ORIENTED_EDGE('',*,*,#15290,.F.);
#20003=ORIENTED_EDGE('',*,*,#14950,.F.);
#20004=ORIENTED_EDGE('',*,*,#15294,.T.);
#20005=ORIENTED_EDGE('',*,*,#15295,.T.);
#20006=ORIENTED_EDGE('',*,*,#15292,.F.);
#20007=ORIENTED_EDGE('',*,*,#14949,.F.);
#20008=ORIENTED_EDGE('',*,*,#15296,.T.);
#20009=ORIENTED_EDGE('',*,*,#15297,.T.);
#20010=ORIENTED_EDGE('',*,*,#15294,.F.);
#20011=ORIENTED_EDGE('',*,*,#14948,.F.);
#20012=ORIENTED_EDGE('',*,*,#15298,.T.);
#20013=ORIENTED_EDGE('',*,*,#15299,.T.);
#20014=ORIENTED_EDGE('',*,*,#15296,.F.);
#20015=ORIENTED_EDGE('',*,*,#14947,.F.);
#20016=ORIENTED_EDGE('',*,*,#15300,.T.);
#20017=ORIENTED_EDGE('',*,*,#15301,.T.);
#20018=ORIENTED_EDGE('',*,*,#15298,.F.);
#20019=ORIENTED_EDGE('',*,*,#14946,.F.);
#20020=ORIENTED_EDGE('',*,*,#15302,.T.);
#20021=ORIENTED_EDGE('',*,*,#15303,.T.);
#20022=ORIENTED_EDGE('',*,*,#15300,.F.);
#20023=ORIENTED_EDGE('',*,*,#14945,.F.);
#20024=ORIENTED_EDGE('',*,*,#15304,.T.);
#20025=ORIENTED_EDGE('',*,*,#15305,.T.);
#20026=ORIENTED_EDGE('',*,*,#15302,.F.);
#20027=ORIENTED_EDGE('',*,*,#14944,.F.);
#20028=ORIENTED_EDGE('',*,*,#15306,.T.);
#20029=ORIENTED_EDGE('',*,*,#15307,.T.);
#20030=ORIENTED_EDGE('',*,*,#15304,.F.);
#20031=ORIENTED_EDGE('',*,*,#14943,.F.);
#20032=ORIENTED_EDGE('',*,*,#15308,.T.);
#20033=ORIENTED_EDGE('',*,*,#15309,.T.);
#20034=ORIENTED_EDGE('',*,*,#15306,.F.);
#20035=ORIENTED_EDGE('',*,*,#14942,.F.);
#20036=ORIENTED_EDGE('',*,*,#15310,.T.);
#20037=ORIENTED_EDGE('',*,*,#15311,.T.);
#20038=ORIENTED_EDGE('',*,*,#15308,.F.);
#20039=ORIENTED_EDGE('',*,*,#14941,.F.);
#20040=ORIENTED_EDGE('',*,*,#15312,.T.);
#20041=ORIENTED_EDGE('',*,*,#15313,.T.);
#20042=ORIENTED_EDGE('',*,*,#15310,.F.);
#20043=ORIENTED_EDGE('',*,*,#14940,.F.);
#20044=ORIENTED_EDGE('',*,*,#15247,.T.);
#20045=ORIENTED_EDGE('',*,*,#15314,.T.);
#20046=ORIENTED_EDGE('',*,*,#15312,.F.);
#20047=ORIENTED_EDGE('',*,*,#15314,.F.);
#20048=ORIENTED_EDGE('',*,*,#15246,.F.);
#20049=ORIENTED_EDGE('',*,*,#15249,.F.);
#20050=ORIENTED_EDGE('',*,*,#15251,.F.);
#20051=ORIENTED_EDGE('',*,*,#15253,.F.);
#20052=ORIENTED_EDGE('',*,*,#15255,.F.);
#20053=ORIENTED_EDGE('',*,*,#15257,.F.);
#20054=ORIENTED_EDGE('',*,*,#15259,.F.);
#20055=ORIENTED_EDGE('',*,*,#15261,.F.);
#20056=ORIENTED_EDGE('',*,*,#15263,.F.);
#20057=ORIENTED_EDGE('',*,*,#15265,.F.);
#20058=ORIENTED_EDGE('',*,*,#15267,.F.);
#20059=ORIENTED_EDGE('',*,*,#15269,.F.);
#20060=ORIENTED_EDGE('',*,*,#15271,.F.);
#20061=ORIENTED_EDGE('',*,*,#15273,.F.);
#20062=ORIENTED_EDGE('',*,*,#15275,.F.);
#20063=ORIENTED_EDGE('',*,*,#15277,.F.);
#20064=ORIENTED_EDGE('',*,*,#15279,.F.);
#20065=ORIENTED_EDGE('',*,*,#15281,.F.);
#20066=ORIENTED_EDGE('',*,*,#15283,.F.);
#20067=ORIENTED_EDGE('',*,*,#15285,.F.);
#20068=ORIENTED_EDGE('',*,*,#15287,.F.);
#20069=ORIENTED_EDGE('',*,*,#15289,.F.);
#20070=ORIENTED_EDGE('',*,*,#15291,.F.);
#20071=ORIENTED_EDGE('',*,*,#15293,.F.);
#20072=ORIENTED_EDGE('',*,*,#15295,.F.);
#20073=ORIENTED_EDGE('',*,*,#15297,.F.);
#20074=ORIENTED_EDGE('',*,*,#15299,.F.);
#20075=ORIENTED_EDGE('',*,*,#15301,.F.);
#20076=ORIENTED_EDGE('',*,*,#15303,.F.);
#20077=ORIENTED_EDGE('',*,*,#15305,.F.);
#20078=ORIENTED_EDGE('',*,*,#15307,.F.);
#20079=ORIENTED_EDGE('',*,*,#15309,.F.);
#20080=ORIENTED_EDGE('',*,*,#15311,.F.);
#20081=ORIENTED_EDGE('',*,*,#15313,.F.);
#20082=ORIENTED_EDGE('',*,*,#14974,.F.);
#20083=ORIENTED_EDGE('',*,*,#15315,.T.);
#20084=ORIENTED_EDGE('',*,*,#15316,.T.);
#20085=ORIENTED_EDGE('',*,*,#15317,.F.);
#20086=ORIENTED_EDGE('',*,*,#15003,.F.);
#20087=ORIENTED_EDGE('',*,*,#15318,.T.);
#20088=ORIENTED_EDGE('',*,*,#15319,.T.);
#20089=ORIENTED_EDGE('',*,*,#15315,.F.);
#20090=ORIENTED_EDGE('',*,*,#15002,.F.);
#20091=ORIENTED_EDGE('',*,*,#15320,.T.);
#20092=ORIENTED_EDGE('',*,*,#15321,.T.);
#20093=ORIENTED_EDGE('',*,*,#15318,.F.);
#20094=ORIENTED_EDGE('',*,*,#15001,.F.);
#20095=ORIENTED_EDGE('',*,*,#15322,.T.);
#20096=ORIENTED_EDGE('',*,*,#15323,.T.);
#20097=ORIENTED_EDGE('',*,*,#15320,.F.);
#20098=ORIENTED_EDGE('',*,*,#15000,.F.);
#20099=ORIENTED_EDGE('',*,*,#15324,.T.);
#20100=ORIENTED_EDGE('',*,*,#15325,.T.);
#20101=ORIENTED_EDGE('',*,*,#15322,.F.);
#20102=ORIENTED_EDGE('',*,*,#14999,.F.);
#20103=ORIENTED_EDGE('',*,*,#15326,.T.);
#20104=ORIENTED_EDGE('',*,*,#15327,.T.);
#20105=ORIENTED_EDGE('',*,*,#15324,.F.);
#20106=ORIENTED_EDGE('',*,*,#14998,.F.);
#20107=ORIENTED_EDGE('',*,*,#15328,.T.);
#20108=ORIENTED_EDGE('',*,*,#15329,.T.);
#20109=ORIENTED_EDGE('',*,*,#15326,.F.);
#20110=ORIENTED_EDGE('',*,*,#14997,.F.);
#20111=ORIENTED_EDGE('',*,*,#15330,.T.);
#20112=ORIENTED_EDGE('',*,*,#15331,.T.);
#20113=ORIENTED_EDGE('',*,*,#15328,.F.);
#20114=ORIENTED_EDGE('',*,*,#14996,.F.);
#20115=ORIENTED_EDGE('',*,*,#15332,.T.);
#20116=ORIENTED_EDGE('',*,*,#15333,.T.);
#20117=ORIENTED_EDGE('',*,*,#15330,.F.);
#20118=ORIENTED_EDGE('',*,*,#14995,.F.);
#20119=ORIENTED_EDGE('',*,*,#15334,.T.);
#20120=ORIENTED_EDGE('',*,*,#15335,.T.);
#20121=ORIENTED_EDGE('',*,*,#15332,.F.);
#20122=ORIENTED_EDGE('',*,*,#14994,.F.);
#20123=ORIENTED_EDGE('',*,*,#15336,.T.);
#20124=ORIENTED_EDGE('',*,*,#15337,.T.);
#20125=ORIENTED_EDGE('',*,*,#15334,.F.);
#20126=ORIENTED_EDGE('',*,*,#14993,.F.);
#20127=ORIENTED_EDGE('',*,*,#15338,.T.);
#20128=ORIENTED_EDGE('',*,*,#15339,.T.);
#20129=ORIENTED_EDGE('',*,*,#15336,.F.);
#20130=ORIENTED_EDGE('',*,*,#14992,.F.);
#20131=ORIENTED_EDGE('',*,*,#15340,.T.);
#20132=ORIENTED_EDGE('',*,*,#15341,.T.);
#20133=ORIENTED_EDGE('',*,*,#15338,.F.);
#20134=ORIENTED_EDGE('',*,*,#14991,.F.);
#20135=ORIENTED_EDGE('',*,*,#15342,.T.);
#20136=ORIENTED_EDGE('',*,*,#15343,.T.);
#20137=ORIENTED_EDGE('',*,*,#15340,.F.);
#20138=ORIENTED_EDGE('',*,*,#14990,.F.);
#20139=ORIENTED_EDGE('',*,*,#15344,.T.);
#20140=ORIENTED_EDGE('',*,*,#15345,.T.);
#20141=ORIENTED_EDGE('',*,*,#15342,.F.);
#20142=ORIENTED_EDGE('',*,*,#14989,.F.);
#20143=ORIENTED_EDGE('',*,*,#15346,.T.);
#20144=ORIENTED_EDGE('',*,*,#15347,.T.);
#20145=ORIENTED_EDGE('',*,*,#15344,.F.);
#20146=ORIENTED_EDGE('',*,*,#14988,.F.);
#20147=ORIENTED_EDGE('',*,*,#15348,.T.);
#20148=ORIENTED_EDGE('',*,*,#15349,.T.);
#20149=ORIENTED_EDGE('',*,*,#15346,.F.);
#20150=ORIENTED_EDGE('',*,*,#14987,.F.);
#20151=ORIENTED_EDGE('',*,*,#15350,.T.);
#20152=ORIENTED_EDGE('',*,*,#15351,.T.);
#20153=ORIENTED_EDGE('',*,*,#15348,.F.);
#20154=ORIENTED_EDGE('',*,*,#14986,.F.);
#20155=ORIENTED_EDGE('',*,*,#15352,.T.);
#20156=ORIENTED_EDGE('',*,*,#15353,.T.);
#20157=ORIENTED_EDGE('',*,*,#15350,.F.);
#20158=ORIENTED_EDGE('',*,*,#14985,.F.);
#20159=ORIENTED_EDGE('',*,*,#15354,.T.);
#20160=ORIENTED_EDGE('',*,*,#15355,.T.);
#20161=ORIENTED_EDGE('',*,*,#15352,.F.);
#20162=ORIENTED_EDGE('',*,*,#14984,.F.);
#20163=ORIENTED_EDGE('',*,*,#15356,.T.);
#20164=ORIENTED_EDGE('',*,*,#15357,.T.);
#20165=ORIENTED_EDGE('',*,*,#15354,.F.);
#20166=ORIENTED_EDGE('',*,*,#14983,.F.);
#20167=ORIENTED_EDGE('',*,*,#15358,.T.);
#20168=ORIENTED_EDGE('',*,*,#15359,.T.);
#20169=ORIENTED_EDGE('',*,*,#15356,.F.);
#20170=ORIENTED_EDGE('',*,*,#14982,.F.);
#20171=ORIENTED_EDGE('',*,*,#15360,.T.);
#20172=ORIENTED_EDGE('',*,*,#15361,.T.);
#20173=ORIENTED_EDGE('',*,*,#15358,.F.);
#20174=ORIENTED_EDGE('',*,*,#14981,.F.);
#20175=ORIENTED_EDGE('',*,*,#15362,.T.);
#20176=ORIENTED_EDGE('',*,*,#15363,.T.);
#20177=ORIENTED_EDGE('',*,*,#15360,.F.);
#20178=ORIENTED_EDGE('',*,*,#14980,.F.);
#20179=ORIENTED_EDGE('',*,*,#15364,.T.);
#20180=ORIENTED_EDGE('',*,*,#15365,.T.);
#20181=ORIENTED_EDGE('',*,*,#15362,.F.);
#20182=ORIENTED_EDGE('',*,*,#14979,.F.);
#20183=ORIENTED_EDGE('',*,*,#15366,.T.);
#20184=ORIENTED_EDGE('',*,*,#15367,.T.);
#20185=ORIENTED_EDGE('',*,*,#15364,.F.);
#20186=ORIENTED_EDGE('',*,*,#14978,.F.);
#20187=ORIENTED_EDGE('',*,*,#15368,.T.);
#20188=ORIENTED_EDGE('',*,*,#15369,.T.);
#20189=ORIENTED_EDGE('',*,*,#15366,.F.);
#20190=ORIENTED_EDGE('',*,*,#14977,.F.);
#20191=ORIENTED_EDGE('',*,*,#15370,.T.);
#20192=ORIENTED_EDGE('',*,*,#15371,.T.);
#20193=ORIENTED_EDGE('',*,*,#15368,.F.);
#20194=ORIENTED_EDGE('',*,*,#14976,.F.);
#20195=ORIENTED_EDGE('',*,*,#15372,.T.);
#20196=ORIENTED_EDGE('',*,*,#15373,.T.);
#20197=ORIENTED_EDGE('',*,*,#15370,.F.);
#20198=ORIENTED_EDGE('',*,*,#14975,.F.);
#20199=ORIENTED_EDGE('',*,*,#15317,.T.);
#20200=ORIENTED_EDGE('',*,*,#15374,.T.);
#20201=ORIENTED_EDGE('',*,*,#15372,.F.);
#20202=ORIENTED_EDGE('',*,*,#15374,.F.);
#20203=ORIENTED_EDGE('',*,*,#15316,.F.);
#20204=ORIENTED_EDGE('',*,*,#15319,.F.);
#20205=ORIENTED_EDGE('',*,*,#15321,.F.);
#20206=ORIENTED_EDGE('',*,*,#15323,.F.);
#20207=ORIENTED_EDGE('',*,*,#15325,.F.);
#20208=ORIENTED_EDGE('',*,*,#15327,.F.);
#20209=ORIENTED_EDGE('',*,*,#15329,.F.);
#20210=ORIENTED_EDGE('',*,*,#15331,.F.);
#20211=ORIENTED_EDGE('',*,*,#15333,.F.);
#20212=ORIENTED_EDGE('',*,*,#15335,.F.);
#20213=ORIENTED_EDGE('',*,*,#15337,.F.);
#20214=ORIENTED_EDGE('',*,*,#15339,.F.);
#20215=ORIENTED_EDGE('',*,*,#15341,.F.);
#20216=ORIENTED_EDGE('',*,*,#15343,.F.);
#20217=ORIENTED_EDGE('',*,*,#15345,.F.);
#20218=ORIENTED_EDGE('',*,*,#15347,.F.);
#20219=ORIENTED_EDGE('',*,*,#15349,.F.);
#20220=ORIENTED_EDGE('',*,*,#15351,.F.);
#20221=ORIENTED_EDGE('',*,*,#15353,.F.);
#20222=ORIENTED_EDGE('',*,*,#15355,.F.);
#20223=ORIENTED_EDGE('',*,*,#15357,.F.);
#20224=ORIENTED_EDGE('',*,*,#15359,.F.);
#20225=ORIENTED_EDGE('',*,*,#15361,.F.);
#20226=ORIENTED_EDGE('',*,*,#15363,.F.);
#20227=ORIENTED_EDGE('',*,*,#15365,.F.);
#20228=ORIENTED_EDGE('',*,*,#15367,.F.);
#20229=ORIENTED_EDGE('',*,*,#15369,.F.);
#20230=ORIENTED_EDGE('',*,*,#15371,.F.);
#20231=ORIENTED_EDGE('',*,*,#15373,.F.);
#20232=ORIENTED_EDGE('',*,*,#15004,.F.);
#20233=ORIENTED_EDGE('',*,*,#15375,.T.);
#20234=ORIENTED_EDGE('',*,*,#15376,.T.);
#20235=ORIENTED_EDGE('',*,*,#15377,.F.);
#20236=ORIENTED_EDGE('',*,*,#15007,.F.);
#20237=ORIENTED_EDGE('',*,*,#15378,.T.);
#20238=ORIENTED_EDGE('',*,*,#15379,.T.);
#20239=ORIENTED_EDGE('',*,*,#15375,.F.);
#20240=ORIENTED_EDGE('',*,*,#15006,.F.);
#20241=ORIENTED_EDGE('',*,*,#15380,.T.);
#20242=ORIENTED_EDGE('',*,*,#15381,.T.);
#20243=ORIENTED_EDGE('',*,*,#15378,.F.);
#20244=ORIENTED_EDGE('',*,*,#15005,.F.);
#20245=ORIENTED_EDGE('',*,*,#15377,.T.);
#20246=ORIENTED_EDGE('',*,*,#15382,.T.);
#20247=ORIENTED_EDGE('',*,*,#15380,.F.);
#20248=ORIENTED_EDGE('',*,*,#15382,.F.);
#20249=ORIENTED_EDGE('',*,*,#15376,.F.);
#20250=ORIENTED_EDGE('',*,*,#15379,.F.);
#20251=ORIENTED_EDGE('',*,*,#15381,.F.);
#20252=ORIENTED_EDGE('',*,*,#15008,.F.);
#20253=ORIENTED_EDGE('',*,*,#15383,.T.);
#20254=ORIENTED_EDGE('',*,*,#15384,.T.);
#20255=ORIENTED_EDGE('',*,*,#15385,.F.);
#20256=ORIENTED_EDGE('',*,*,#15042,.F.);
#20257=ORIENTED_EDGE('',*,*,#15386,.T.);
#20258=ORIENTED_EDGE('',*,*,#15387,.T.);
#20259=ORIENTED_EDGE('',*,*,#15383,.F.);
#20260=ORIENTED_EDGE('',*,*,#15041,.F.);
#20261=ORIENTED_EDGE('',*,*,#15388,.T.);
#20262=ORIENTED_EDGE('',*,*,#15389,.T.);
#20263=ORIENTED_EDGE('',*,*,#15386,.F.);
#20264=ORIENTED_EDGE('',*,*,#15040,.F.);
#20265=ORIENTED_EDGE('',*,*,#15390,.T.);
#20266=ORIENTED_EDGE('',*,*,#15391,.T.);
#20267=ORIENTED_EDGE('',*,*,#15388,.F.);
#20268=ORIENTED_EDGE('',*,*,#15039,.F.);
#20269=ORIENTED_EDGE('',*,*,#15392,.T.);
#20270=ORIENTED_EDGE('',*,*,#15393,.T.);
#20271=ORIENTED_EDGE('',*,*,#15390,.F.);
#20272=ORIENTED_EDGE('',*,*,#15038,.F.);
#20273=ORIENTED_EDGE('',*,*,#15394,.T.);
#20274=ORIENTED_EDGE('',*,*,#15395,.T.);
#20275=ORIENTED_EDGE('',*,*,#15392,.F.);
#20276=ORIENTED_EDGE('',*,*,#15037,.F.);
#20277=ORIENTED_EDGE('',*,*,#15396,.T.);
#20278=ORIENTED_EDGE('',*,*,#15397,.T.);
#20279=ORIENTED_EDGE('',*,*,#15394,.F.);
#20280=ORIENTED_EDGE('',*,*,#15036,.F.);
#20281=ORIENTED_EDGE('',*,*,#15398,.T.);
#20282=ORIENTED_EDGE('',*,*,#15399,.T.);
#20283=ORIENTED_EDGE('',*,*,#15396,.F.);
#20284=ORIENTED_EDGE('',*,*,#15035,.F.);
#20285=ORIENTED_EDGE('',*,*,#15400,.T.);
#20286=ORIENTED_EDGE('',*,*,#15401,.T.);
#20287=ORIENTED_EDGE('',*,*,#15398,.F.);
#20288=ORIENTED_EDGE('',*,*,#15034,.F.);
#20289=ORIENTED_EDGE('',*,*,#15402,.T.);
#20290=ORIENTED_EDGE('',*,*,#15403,.T.);
#20291=ORIENTED_EDGE('',*,*,#15400,.F.);
#20292=ORIENTED_EDGE('',*,*,#15033,.F.);
#20293=ORIENTED_EDGE('',*,*,#15404,.T.);
#20294=ORIENTED_EDGE('',*,*,#15405,.T.);
#20295=ORIENTED_EDGE('',*,*,#15402,.F.);
#20296=ORIENTED_EDGE('',*,*,#15032,.F.);
#20297=ORIENTED_EDGE('',*,*,#15406,.T.);
#20298=ORIENTED_EDGE('',*,*,#15407,.T.);
#20299=ORIENTED_EDGE('',*,*,#15404,.F.);
#20300=ORIENTED_EDGE('',*,*,#15031,.F.);
#20301=ORIENTED_EDGE('',*,*,#15408,.T.);
#20302=ORIENTED_EDGE('',*,*,#15409,.T.);
#20303=ORIENTED_EDGE('',*,*,#15406,.F.);
#20304=ORIENTED_EDGE('',*,*,#15030,.F.);
#20305=ORIENTED_EDGE('',*,*,#15410,.T.);
#20306=ORIENTED_EDGE('',*,*,#15411,.T.);
#20307=ORIENTED_EDGE('',*,*,#15408,.F.);
#20308=ORIENTED_EDGE('',*,*,#15029,.F.);
#20309=ORIENTED_EDGE('',*,*,#15412,.T.);
#20310=ORIENTED_EDGE('',*,*,#15413,.T.);
#20311=ORIENTED_EDGE('',*,*,#15410,.F.);
#20312=ORIENTED_EDGE('',*,*,#15028,.F.);
#20313=ORIENTED_EDGE('',*,*,#15414,.T.);
#20314=ORIENTED_EDGE('',*,*,#15415,.T.);
#20315=ORIENTED_EDGE('',*,*,#15412,.F.);
#20316=ORIENTED_EDGE('',*,*,#15027,.F.);
#20317=ORIENTED_EDGE('',*,*,#15416,.T.);
#20318=ORIENTED_EDGE('',*,*,#15417,.T.);
#20319=ORIENTED_EDGE('',*,*,#15414,.F.);
#20320=ORIENTED_EDGE('',*,*,#15026,.F.);
#20321=ORIENTED_EDGE('',*,*,#15418,.T.);
#20322=ORIENTED_EDGE('',*,*,#15419,.T.);
#20323=ORIENTED_EDGE('',*,*,#15416,.F.);
#20324=ORIENTED_EDGE('',*,*,#15025,.F.);
#20325=ORIENTED_EDGE('',*,*,#15420,.T.);
#20326=ORIENTED_EDGE('',*,*,#15421,.T.);
#20327=ORIENTED_EDGE('',*,*,#15418,.F.);
#20328=ORIENTED_EDGE('',*,*,#15024,.F.);
#20329=ORIENTED_EDGE('',*,*,#15422,.T.);
#20330=ORIENTED_EDGE('',*,*,#15423,.T.);
#20331=ORIENTED_EDGE('',*,*,#15420,.F.);
#20332=ORIENTED_EDGE('',*,*,#15023,.F.);
#20333=ORIENTED_EDGE('',*,*,#15424,.T.);
#20334=ORIENTED_EDGE('',*,*,#15425,.T.);
#20335=ORIENTED_EDGE('',*,*,#15422,.F.);
#20336=ORIENTED_EDGE('',*,*,#15022,.F.);
#20337=ORIENTED_EDGE('',*,*,#15426,.T.);
#20338=ORIENTED_EDGE('',*,*,#15427,.T.);
#20339=ORIENTED_EDGE('',*,*,#15424,.F.);
#20340=ORIENTED_EDGE('',*,*,#15021,.F.);
#20341=ORIENTED_EDGE('',*,*,#15428,.T.);
#20342=ORIENTED_EDGE('',*,*,#15429,.T.);
#20343=ORIENTED_EDGE('',*,*,#15426,.F.);
#20344=ORIENTED_EDGE('',*,*,#15020,.F.);
#20345=ORIENTED_EDGE('',*,*,#15430,.T.);
#20346=ORIENTED_EDGE('',*,*,#15431,.T.);
#20347=ORIENTED_EDGE('',*,*,#15428,.F.);
#20348=ORIENTED_EDGE('',*,*,#15019,.F.);
#20349=ORIENTED_EDGE('',*,*,#15432,.T.);
#20350=ORIENTED_EDGE('',*,*,#15433,.T.);
#20351=ORIENTED_EDGE('',*,*,#15430,.F.);
#20352=ORIENTED_EDGE('',*,*,#15018,.F.);
#20353=ORIENTED_EDGE('',*,*,#15434,.T.);
#20354=ORIENTED_EDGE('',*,*,#15435,.T.);
#20355=ORIENTED_EDGE('',*,*,#15432,.F.);
#20356=ORIENTED_EDGE('',*,*,#15017,.F.);
#20357=ORIENTED_EDGE('',*,*,#15436,.T.);
#20358=ORIENTED_EDGE('',*,*,#15437,.T.);
#20359=ORIENTED_EDGE('',*,*,#15434,.F.);
#20360=ORIENTED_EDGE('',*,*,#15016,.F.);
#20361=ORIENTED_EDGE('',*,*,#15438,.T.);
#20362=ORIENTED_EDGE('',*,*,#15439,.T.);
#20363=ORIENTED_EDGE('',*,*,#15436,.F.);
#20364=ORIENTED_EDGE('',*,*,#15015,.F.);
#20365=ORIENTED_EDGE('',*,*,#15440,.T.);
#20366=ORIENTED_EDGE('',*,*,#15441,.T.);
#20367=ORIENTED_EDGE('',*,*,#15438,.F.);
#20368=ORIENTED_EDGE('',*,*,#15014,.F.);
#20369=ORIENTED_EDGE('',*,*,#15442,.T.);
#20370=ORIENTED_EDGE('',*,*,#15443,.T.);
#20371=ORIENTED_EDGE('',*,*,#15440,.F.);
#20372=ORIENTED_EDGE('',*,*,#15013,.F.);
#20373=ORIENTED_EDGE('',*,*,#15444,.T.);
#20374=ORIENTED_EDGE('',*,*,#15445,.T.);
#20375=ORIENTED_EDGE('',*,*,#15442,.F.);
#20376=ORIENTED_EDGE('',*,*,#15012,.F.);
#20377=ORIENTED_EDGE('',*,*,#15446,.T.);
#20378=ORIENTED_EDGE('',*,*,#15447,.T.);
#20379=ORIENTED_EDGE('',*,*,#15444,.F.);
#20380=ORIENTED_EDGE('',*,*,#15011,.F.);
#20381=ORIENTED_EDGE('',*,*,#15448,.T.);
#20382=ORIENTED_EDGE('',*,*,#15449,.T.);
#20383=ORIENTED_EDGE('',*,*,#15446,.F.);
#20384=ORIENTED_EDGE('',*,*,#15010,.F.);
#20385=ORIENTED_EDGE('',*,*,#15450,.T.);
#20386=ORIENTED_EDGE('',*,*,#15451,.T.);
#20387=ORIENTED_EDGE('',*,*,#15448,.F.);
#20388=ORIENTED_EDGE('',*,*,#15009,.F.);
#20389=ORIENTED_EDGE('',*,*,#15385,.T.);
#20390=ORIENTED_EDGE('',*,*,#15452,.T.);
#20391=ORIENTED_EDGE('',*,*,#15450,.F.);
#20392=ORIENTED_EDGE('',*,*,#15452,.F.);
#20393=ORIENTED_EDGE('',*,*,#15384,.F.);
#20394=ORIENTED_EDGE('',*,*,#15387,.F.);
#20395=ORIENTED_EDGE('',*,*,#15389,.F.);
#20396=ORIENTED_EDGE('',*,*,#15391,.F.);
#20397=ORIENTED_EDGE('',*,*,#15393,.F.);
#20398=ORIENTED_EDGE('',*,*,#15395,.F.);
#20399=ORIENTED_EDGE('',*,*,#15397,.F.);
#20400=ORIENTED_EDGE('',*,*,#15399,.F.);
#20401=ORIENTED_EDGE('',*,*,#15401,.F.);
#20402=ORIENTED_EDGE('',*,*,#15403,.F.);
#20403=ORIENTED_EDGE('',*,*,#15405,.F.);
#20404=ORIENTED_EDGE('',*,*,#15407,.F.);
#20405=ORIENTED_EDGE('',*,*,#15409,.F.);
#20406=ORIENTED_EDGE('',*,*,#15411,.F.);
#20407=ORIENTED_EDGE('',*,*,#15413,.F.);
#20408=ORIENTED_EDGE('',*,*,#15415,.F.);
#20409=ORIENTED_EDGE('',*,*,#15417,.F.);
#20410=ORIENTED_EDGE('',*,*,#15419,.F.);
#20411=ORIENTED_EDGE('',*,*,#15421,.F.);
#20412=ORIENTED_EDGE('',*,*,#15423,.F.);
#20413=ORIENTED_EDGE('',*,*,#15425,.F.);
#20414=ORIENTED_EDGE('',*,*,#15427,.F.);
#20415=ORIENTED_EDGE('',*,*,#15429,.F.);
#20416=ORIENTED_EDGE('',*,*,#15431,.F.);
#20417=ORIENTED_EDGE('',*,*,#15433,.F.);
#20418=ORIENTED_EDGE('',*,*,#15435,.F.);
#20419=ORIENTED_EDGE('',*,*,#15437,.F.);
#20420=ORIENTED_EDGE('',*,*,#15439,.F.);
#20421=ORIENTED_EDGE('',*,*,#15441,.F.);
#20422=ORIENTED_EDGE('',*,*,#15443,.F.);
#20423=ORIENTED_EDGE('',*,*,#15445,.F.);
#20424=ORIENTED_EDGE('',*,*,#15447,.F.);
#20425=ORIENTED_EDGE('',*,*,#15449,.F.);
#20426=ORIENTED_EDGE('',*,*,#15451,.F.);
#20427=ORIENTED_EDGE('',*,*,#15132,.T.);
#20428=ORIENTED_EDGE('',*,*,#15453,.T.);
#20429=ORIENTED_EDGE('',*,*,#15454,.T.);
#20430=ORIENTED_EDGE('',*,*,#15453,.F.);
#20431=ORIENTED_EDGE('',*,*,#15455,.T.);
#20432=ORIENTED_EDGE('',*,*,#15456,.T.);
#20433=ORIENTED_EDGE('',*,*,#15454,.F.);
#20434=ORIENTED_EDGE('',*,*,#15456,.F.);
#20435=ORIENTED_EDGE('',*,*,#15115,.T.);
#20436=ORIENTED_EDGE('',*,*,#15457,.T.);
#20437=ORIENTED_EDGE('',*,*,#15458,.T.);
#20438=ORIENTED_EDGE('',*,*,#15457,.F.);
#20439=ORIENTED_EDGE('',*,*,#15458,.F.);
#20440=ORIENTED_EDGE('',*,*,#15459,.T.);
#20441=ORIENTED_EDGE('',*,*,#15460,.T.);
#20442=ORIENTED_EDGE('',*,*,#15459,.F.);
#20443=ORIENTED_EDGE('',*,*,#15131,.T.);
#20444=ORIENTED_EDGE('',*,*,#15461,.T.);
#20445=ORIENTED_EDGE('',*,*,#15462,.T.);
#20446=ORIENTED_EDGE('',*,*,#15461,.F.);
#20447=ORIENTED_EDGE('',*,*,#15462,.F.);
#20448=ORIENTED_EDGE('',*,*,#15463,.T.);
#20449=ORIENTED_EDGE('',*,*,#15464,.T.);
#20450=ORIENTED_EDGE('',*,*,#15463,.F.);
#20451=ORIENTED_EDGE('',*,*,#15116,.T.);
#20452=ORIENTED_EDGE('',*,*,#15465,.T.);
#20453=ORIENTED_EDGE('',*,*,#15466,.T.);
#20454=ORIENTED_EDGE('',*,*,#15465,.F.);
#20455=ORIENTED_EDGE('',*,*,#15466,.F.);
#20456=ORIENTED_EDGE('',*,*,#15467,.T.);
#20457=ORIENTED_EDGE('',*,*,#15468,.T.);
#20458=ORIENTED_EDGE('',*,*,#15467,.F.);
#20459=ORIENTED_EDGE('',*,*,#15130,.T.);
#20460=ORIENTED_EDGE('',*,*,#15469,.T.);
#20461=ORIENTED_EDGE('',*,*,#15470,.T.);
#20462=ORIENTED_EDGE('',*,*,#15469,.F.);
#20463=ORIENTED_EDGE('',*,*,#15470,.F.);
#20464=ORIENTED_EDGE('',*,*,#15471,.T.);
#20465=ORIENTED_EDGE('',*,*,#15472,.T.);
#20466=ORIENTED_EDGE('',*,*,#15471,.F.);
#20467=ORIENTED_EDGE('',*,*,#15117,.T.);
#20468=ORIENTED_EDGE('',*,*,#15473,.T.);
#20469=ORIENTED_EDGE('',*,*,#15474,.T.);
#20470=ORIENTED_EDGE('',*,*,#15473,.F.);
#20471=ORIENTED_EDGE('',*,*,#15474,.F.);
#20472=ORIENTED_EDGE('',*,*,#15475,.T.);
#20473=ORIENTED_EDGE('',*,*,#15476,.T.);
#20474=ORIENTED_EDGE('',*,*,#15475,.F.);
#20475=ORIENTED_EDGE('',*,*,#15129,.T.);
#20476=ORIENTED_EDGE('',*,*,#15477,.T.);
#20477=ORIENTED_EDGE('',*,*,#15478,.T.);
#20478=ORIENTED_EDGE('',*,*,#15477,.F.);
#20479=ORIENTED_EDGE('',*,*,#15478,.F.);
#20480=ORIENTED_EDGE('',*,*,#15479,.T.);
#20481=ORIENTED_EDGE('',*,*,#15480,.T.);
#20482=ORIENTED_EDGE('',*,*,#15479,.F.);
#20483=ORIENTED_EDGE('',*,*,#15118,.T.);
#20484=ORIENTED_EDGE('',*,*,#15481,.T.);
#20485=ORIENTED_EDGE('',*,*,#15482,.T.);
#20486=ORIENTED_EDGE('',*,*,#15481,.F.);
#20487=ORIENTED_EDGE('',*,*,#15482,.F.);
#20488=ORIENTED_EDGE('',*,*,#15483,.T.);
#20489=ORIENTED_EDGE('',*,*,#15484,.T.);
#20490=ORIENTED_EDGE('',*,*,#15483,.F.);
#20491=ORIENTED_EDGE('',*,*,#15128,.T.);
#20492=ORIENTED_EDGE('',*,*,#15485,.T.);
#20493=ORIENTED_EDGE('',*,*,#15486,.T.);
#20494=ORIENTED_EDGE('',*,*,#15485,.F.);
#20495=ORIENTED_EDGE('',*,*,#15486,.F.);
#20496=ORIENTED_EDGE('',*,*,#15487,.T.);
#20497=ORIENTED_EDGE('',*,*,#15488,.T.);
#20498=ORIENTED_EDGE('',*,*,#15487,.F.);
#20499=ORIENTED_EDGE('',*,*,#15119,.T.);
#20500=ORIENTED_EDGE('',*,*,#15489,.T.);
#20501=ORIENTED_EDGE('',*,*,#15490,.T.);
#20502=ORIENTED_EDGE('',*,*,#15489,.F.);
#20503=ORIENTED_EDGE('',*,*,#15490,.F.);
#20504=ORIENTED_EDGE('',*,*,#15491,.T.);
#20505=ORIENTED_EDGE('',*,*,#15492,.T.);
#20506=ORIENTED_EDGE('',*,*,#15491,.F.);
#20507=ORIENTED_EDGE('',*,*,#15127,.T.);
#20508=ORIENTED_EDGE('',*,*,#15493,.T.);
#20509=ORIENTED_EDGE('',*,*,#15494,.T.);
#20510=ORIENTED_EDGE('',*,*,#15493,.F.);
#20511=ORIENTED_EDGE('',*,*,#15494,.F.);
#20512=ORIENTED_EDGE('',*,*,#15495,.T.);
#20513=ORIENTED_EDGE('',*,*,#15496,.T.);
#20514=ORIENTED_EDGE('',*,*,#15495,.F.);
#20515=ORIENTED_EDGE('',*,*,#15120,.T.);
#20516=ORIENTED_EDGE('',*,*,#15497,.T.);
#20517=ORIENTED_EDGE('',*,*,#15498,.T.);
#20518=ORIENTED_EDGE('',*,*,#15497,.F.);
#20519=ORIENTED_EDGE('',*,*,#15498,.F.);
#20520=ORIENTED_EDGE('',*,*,#15499,.T.);
#20521=ORIENTED_EDGE('',*,*,#15500,.T.);
#20522=ORIENTED_EDGE('',*,*,#15499,.F.);
#20523=ORIENTED_EDGE('',*,*,#15126,.T.);
#20524=ORIENTED_EDGE('',*,*,#15501,.T.);
#20525=ORIENTED_EDGE('',*,*,#15502,.T.);
#20526=ORIENTED_EDGE('',*,*,#15501,.F.);
#20527=ORIENTED_EDGE('',*,*,#15502,.F.);
#20528=ORIENTED_EDGE('',*,*,#15503,.T.);
#20529=ORIENTED_EDGE('',*,*,#15504,.T.);
#20530=ORIENTED_EDGE('',*,*,#15503,.F.);
#20531=ORIENTED_EDGE('',*,*,#15121,.T.);
#20532=ORIENTED_EDGE('',*,*,#15505,.T.);
#20533=ORIENTED_EDGE('',*,*,#15506,.T.);
#20534=ORIENTED_EDGE('',*,*,#15505,.F.);
#20535=ORIENTED_EDGE('',*,*,#15506,.F.);
#20536=ORIENTED_EDGE('',*,*,#15507,.T.);
#20537=ORIENTED_EDGE('',*,*,#15087,.T.);
#20538=ORIENTED_EDGE('',*,*,#15507,.F.);
#20539=ORIENTED_EDGE('',*,*,#15125,.T.);
#20540=ORIENTED_EDGE('',*,*,#15508,.T.);
#20541=ORIENTED_EDGE('',*,*,#15509,.T.);
#20542=ORIENTED_EDGE('',*,*,#15508,.F.);
#20543=ORIENTED_EDGE('',*,*,#15509,.F.);
#20544=ORIENTED_EDGE('',*,*,#15510,.T.);
#20545=ORIENTED_EDGE('',*,*,#15081,.T.);
#20546=ORIENTED_EDGE('',*,*,#15510,.F.);
#20547=ORIENTED_EDGE('',*,*,#15122,.T.);
#20548=ORIENTED_EDGE('',*,*,#15511,.T.);
#20549=ORIENTED_EDGE('',*,*,#15512,.T.);
#20550=ORIENTED_EDGE('',*,*,#15511,.F.);
#20551=ORIENTED_EDGE('',*,*,#15512,.F.);
#20552=ORIENTED_EDGE('',*,*,#15513,.T.);
#20553=ORIENTED_EDGE('',*,*,#15075,.T.);
#20554=ORIENTED_EDGE('',*,*,#15513,.F.);
#20555=ORIENTED_EDGE('',*,*,#15124,.T.);
#20556=ORIENTED_EDGE('',*,*,#15514,.T.);
#20557=ORIENTED_EDGE('',*,*,#15515,.T.);
#20558=ORIENTED_EDGE('',*,*,#15514,.F.);
#20559=ORIENTED_EDGE('',*,*,#15515,.F.);
#20560=ORIENTED_EDGE('',*,*,#15516,.T.);
#20561=ORIENTED_EDGE('',*,*,#15069,.T.);
#20562=ORIENTED_EDGE('',*,*,#15516,.F.);
#20563=ORIENTED_EDGE('',*,*,#15136,.T.);
#20564=ORIENTED_EDGE('',*,*,#15517,.T.);
#20565=ORIENTED_EDGE('',*,*,#15086,.T.);
#20566=ORIENTED_EDGE('',*,*,#15517,.F.);
#20567=ORIENTED_EDGE('',*,*,#15133,.T.);
#20568=ORIENTED_EDGE('',*,*,#15518,.T.);
#20569=ORIENTED_EDGE('',*,*,#15080,.T.);
#20570=ORIENTED_EDGE('',*,*,#15518,.F.);
#20571=ORIENTED_EDGE('',*,*,#15135,.T.);
#20572=ORIENTED_EDGE('',*,*,#15519,.T.);
#20573=ORIENTED_EDGE('',*,*,#15074,.T.);
#20574=ORIENTED_EDGE('',*,*,#15519,.F.);
#20575=ORIENTED_EDGE('',*,*,#15134,.T.);
#20576=ORIENTED_EDGE('',*,*,#15520,.T.);
#20577=ORIENTED_EDGE('',*,*,#15068,.T.);
#20578=ORIENTED_EDGE('',*,*,#15520,.F.);
#20579=ORIENTED_EDGE('',*,*,#15063,.F.);
#20580=ORIENTED_EDGE('',*,*,#15059,.F.);
#20581=ORIENTED_EDGE('',*,*,#15504,.F.);
#20582=ORIENTED_EDGE('',*,*,#15500,.F.);
#20583=ORIENTED_EDGE('',*,*,#15496,.F.);
#20584=ORIENTED_EDGE('',*,*,#15492,.F.);
#20585=ORIENTED_EDGE('',*,*,#15488,.F.);
#20586=ORIENTED_EDGE('',*,*,#15484,.F.);
#20587=ORIENTED_EDGE('',*,*,#15480,.F.);
#20588=ORIENTED_EDGE('',*,*,#15476,.F.);
#20589=ORIENTED_EDGE('',*,*,#15472,.F.);
#20590=ORIENTED_EDGE('',*,*,#15468,.F.);
#20591=ORIENTED_EDGE('',*,*,#15464,.F.);
#20592=ORIENTED_EDGE('',*,*,#15460,.F.);
#20593=ORIENTED_EDGE('',*,*,#15123,.F.);
#20594=ORIENTED_EDGE('',*,*,#15521,.T.);
#20595=ORIENTED_EDGE('',*,*,#15522,.T.);
#20596=ORIENTED_EDGE('',*,*,#15521,.F.);
#20597=ORIENTED_EDGE('',*,*,#15522,.F.);
#20598=ORIENTED_EDGE('',*,*,#15455,.F.);
#20599=ORIENTED_EDGE('',*,*,#14860,.F.);
#20600=ORIENTED_EDGE('',*,*,#15109,.F.);
#20601=ORIENTED_EDGE('',*,*,#15110,.F.);
#20602=ORIENTED_EDGE('',*,*,#14869,.F.);
#20603=ORIENTED_EDGE('',*,*,#15523,.T.);
#20604=ORIENTED_EDGE('',*,*,#15524,.T.);
#20605=ORIENTED_EDGE('',*,*,#15525,.T.);
#20606=ORIENTED_EDGE('',*,*,#15524,.F.);
#20607=ORIENTED_EDGE('',*,*,#15526,.F.);
#20608=ORIENTED_EDGE('',*,*,#15527,.F.);
#20609=ORIENTED_EDGE('',*,*,#15528,.F.);
#20610=ORIENTED_EDGE('',*,*,#15529,.F.);
#20611=ORIENTED_EDGE('',*,*,#15530,.F.);
#20612=ORIENTED_EDGE('',*,*,#15531,.F.);
#20613=ORIENTED_EDGE('',*,*,#15532,.F.);
#20614=ORIENTED_EDGE('',*,*,#15533,.F.);
#20615=ORIENTED_EDGE('',*,*,#15534,.F.);
#20616=ORIENTED_EDGE('',*,*,#15535,.F.);
#20617=ORIENTED_EDGE('',*,*,#15536,.F.);
#20618=ORIENTED_EDGE('',*,*,#15537,.F.);
#20619=ORIENTED_EDGE('',*,*,#15538,.F.);
#20620=ORIENTED_EDGE('',*,*,#15539,.F.);
#20621=ORIENTED_EDGE('',*,*,#15540,.F.);
#20622=ORIENTED_EDGE('',*,*,#15541,.F.);
#20623=ORIENTED_EDGE('',*,*,#15542,.F.);
#20624=ORIENTED_EDGE('',*,*,#15543,.F.);
#20625=ORIENTED_EDGE('',*,*,#15544,.F.);
#20626=ORIENTED_EDGE('',*,*,#15545,.F.);
#20627=ORIENTED_EDGE('',*,*,#15546,.F.);
#20628=ORIENTED_EDGE('',*,*,#15547,.F.);
#20629=ORIENTED_EDGE('',*,*,#15548,.F.);
#20630=ORIENTED_EDGE('',*,*,#15549,.F.);
#20631=ORIENTED_EDGE('',*,*,#15550,.F.);
#20632=ORIENTED_EDGE('',*,*,#15551,.F.);
#20633=ORIENTED_EDGE('',*,*,#15552,.F.);
#20634=ORIENTED_EDGE('',*,*,#15553,.F.);
#20635=ORIENTED_EDGE('',*,*,#15554,.T.);
#20636=ORIENTED_EDGE('',*,*,#15555,.T.);
#20637=ORIENTED_EDGE('',*,*,#15556,.T.);
#20638=ORIENTED_EDGE('',*,*,#15557,.T.);
#20639=ORIENTED_EDGE('',*,*,#15558,.F.);
#20640=ORIENTED_EDGE('',*,*,#15559,.F.);
#20641=ORIENTED_EDGE('',*,*,#15523,.F.);
#20642=ORIENTED_EDGE('',*,*,#15525,.F.);
#20643=ORIENTED_EDGE('',*,*,#15560,.T.);
#20644=ORIENTED_EDGE('',*,*,#15561,.T.);
#20645=ORIENTED_EDGE('',*,*,#15560,.F.);
#20646=ORIENTED_EDGE('',*,*,#15551,.T.);
#20647=ORIENTED_EDGE('',*,*,#15562,.T.);
#20648=ORIENTED_EDGE('',*,*,#15563,.T.);
#20649=ORIENTED_EDGE('',*,*,#15562,.F.);
#20650=ORIENTED_EDGE('',*,*,#15563,.F.);
#20651=ORIENTED_EDGE('',*,*,#15564,.T.);
#20652=ORIENTED_EDGE('',*,*,#15565,.T.);
#20653=ORIENTED_EDGE('',*,*,#15564,.F.);
#20654=ORIENTED_EDGE('',*,*,#15566,.T.);
#20655=ORIENTED_EDGE('',*,*,#15567,.T.);
#20656=ORIENTED_EDGE('',*,*,#15568,.T.);
#20657=ORIENTED_EDGE('',*,*,#15527,.T.);
#20658=ORIENTED_EDGE('',*,*,#15568,.F.);
#20659=ORIENTED_EDGE('',*,*,#15569,.T.);
#20660=ORIENTED_EDGE('',*,*,#15570,.T.);
#20661=ORIENTED_EDGE('',*,*,#15528,.T.);
#20662=ORIENTED_EDGE('',*,*,#15571,.T.);
#20663=ORIENTED_EDGE('',*,*,#15529,.T.);
#20664=ORIENTED_EDGE('',*,*,#15570,.F.);
#20665=ORIENTED_EDGE('',*,*,#15572,.T.);
#20666=ORIENTED_EDGE('',*,*,#15571,.F.);
#20667=ORIENTED_EDGE('',*,*,#15573,.T.);
#20668=ORIENTED_EDGE('',*,*,#15574,.T.);
#20669=ORIENTED_EDGE('',*,*,#15530,.T.);
#20670=ORIENTED_EDGE('',*,*,#15575,.T.);
#20671=ORIENTED_EDGE('',*,*,#15531,.T.);
#20672=ORIENTED_EDGE('',*,*,#15574,.F.);
#20673=ORIENTED_EDGE('',*,*,#15576,.T.);
#20674=ORIENTED_EDGE('',*,*,#15577,.T.);
#20675=ORIENTED_EDGE('',*,*,#15575,.F.);
#20676=ORIENTED_EDGE('',*,*,#15578,.F.);
#20677=ORIENTED_EDGE('',*,*,#15579,.T.);
#20678=ORIENTED_EDGE('',*,*,#15580,.F.);
#20679=ORIENTED_EDGE('',*,*,#15581,.F.);
#20680=ORIENTED_EDGE('',*,*,#15532,.T.);
#20681=ORIENTED_EDGE('',*,*,#15577,.F.);
#20682=ORIENTED_EDGE('',*,*,#15582,.T.);
#20683=ORIENTED_EDGE('',*,*,#15583,.T.);
#20684=ORIENTED_EDGE('',*,*,#15584,.T.);
#20685=ORIENTED_EDGE('',*,*,#15578,.T.);
#20686=ORIENTED_EDGE('',*,*,#15585,.F.);
#20687=ORIENTED_EDGE('',*,*,#15583,.F.);
#20688=ORIENTED_EDGE('',*,*,#15586,.F.);
#20689=ORIENTED_EDGE('',*,*,#15587,.T.);
#20690=ORIENTED_EDGE('',*,*,#15588,.T.);
#20691=ORIENTED_EDGE('',*,*,#15589,.T.);
#20692=ORIENTED_EDGE('',*,*,#15590,.T.);
#20693=ORIENTED_EDGE('',*,*,#15591,.T.);
#20694=ORIENTED_EDGE('',*,*,#15592,.T.);
#20695=ORIENTED_EDGE('',*,*,#15589,.F.);
#20696=ORIENTED_EDGE('',*,*,#15593,.T.);
#20697=ORIENTED_EDGE('',*,*,#15594,.T.);
#20698=ORIENTED_EDGE('',*,*,#15595,.T.);
#20699=ORIENTED_EDGE('',*,*,#15591,.F.);
#20700=ORIENTED_EDGE('',*,*,#15596,.T.);
#20701=ORIENTED_EDGE('',*,*,#15597,.T.);
#20702=ORIENTED_EDGE('',*,*,#15598,.T.);
#20703=ORIENTED_EDGE('',*,*,#15594,.F.);
#20704=ORIENTED_EDGE('',*,*,#15599,.T.);
#20705=ORIENTED_EDGE('',*,*,#15597,.F.);
#20706=ORIENTED_EDGE('',*,*,#15600,.T.);
#20707=ORIENTED_EDGE('',*,*,#15586,.T.);
#20708=ORIENTED_EDGE('',*,*,#15601,.T.);
#20709=ORIENTED_EDGE('',*,*,#15602,.T.);
#20710=ORIENTED_EDGE('',*,*,#15603,.T.);
#20711=ORIENTED_EDGE('',*,*,#15585,.T.);
#20712=ORIENTED_EDGE('',*,*,#15604,.T.);
#20713=ORIENTED_EDGE('',*,*,#15605,.T.);
#20714=ORIENTED_EDGE('',*,*,#15572,.F.);
#20715=ORIENTED_EDGE('',*,*,#15606,.F.);
#20716=ORIENTED_EDGE('',*,*,#15595,.F.);
#20717=ORIENTED_EDGE('',*,*,#15607,.F.);
#20718=ORIENTED_EDGE('',*,*,#15573,.F.);
#20719=ORIENTED_EDGE('',*,*,#15607,.T.);
#20720=ORIENTED_EDGE('',*,*,#15598,.F.);
#20721=ORIENTED_EDGE('',*,*,#15608,.T.);
#20722=ORIENTED_EDGE('',*,*,#15576,.F.);
#20723=ORIENTED_EDGE('',*,*,#15608,.F.);
#20724=ORIENTED_EDGE('',*,*,#15601,.F.);
#20725=ORIENTED_EDGE('',*,*,#15582,.F.);
#20726=ORIENTED_EDGE('',*,*,#15584,.F.);
#20727=ORIENTED_EDGE('',*,*,#15603,.F.);
#20728=ORIENTED_EDGE('',*,*,#15609,.F.);
#20729=ORIENTED_EDGE('',*,*,#15579,.F.);
#20730=ORIENTED_EDGE('',*,*,#15602,.F.);
#20731=ORIENTED_EDGE('',*,*,#15610,.F.);
#20732=ORIENTED_EDGE('',*,*,#15611,.T.);
#20733=ORIENTED_EDGE('',*,*,#15612,.T.);
#20734=ORIENTED_EDGE('',*,*,#15580,.T.);
#20735=ORIENTED_EDGE('',*,*,#15609,.T.);
#20736=ORIENTED_EDGE('',*,*,#15605,.F.);
#20737=ORIENTED_EDGE('',*,*,#15613,.T.);
#20738=ORIENTED_EDGE('',*,*,#15614,.T.);
#20739=ORIENTED_EDGE('',*,*,#15615,.T.);
#20740=ORIENTED_EDGE('',*,*,#15610,.T.);
#20741=ORIENTED_EDGE('',*,*,#15616,.T.);
#20742=ORIENTED_EDGE('',*,*,#15617,.T.);
#20743=ORIENTED_EDGE('',*,*,#15618,.T.);
#20744=ORIENTED_EDGE('',*,*,#15617,.F.);
#20745=ORIENTED_EDGE('',*,*,#15588,.F.);
#20746=ORIENTED_EDGE('',*,*,#15619,.T.);
#20747=ORIENTED_EDGE('',*,*,#15620,.F.);
#20748=ORIENTED_EDGE('',*,*,#15621,.T.);
#20749=ORIENTED_EDGE('',*,*,#15622,.F.);
#20750=ORIENTED_EDGE('',*,*,#15623,.F.);
#20751=ORIENTED_EDGE('',*,*,#15624,.F.);
#20752=ORIENTED_EDGE('',*,*,#15625,.F.);
#20753=ORIENTED_EDGE('',*,*,#15626,.F.);
#20754=ORIENTED_EDGE('',*,*,#15627,.F.);
#20755=ORIENTED_EDGE('',*,*,#15628,.F.);
#20756=ORIENTED_EDGE('',*,*,#15629,.F.);
#20757=ORIENTED_EDGE('',*,*,#15630,.F.);
#20758=ORIENTED_EDGE('',*,*,#15631,.F.);
#20759=ORIENTED_EDGE('',*,*,#15632,.F.);
#20760=ORIENTED_EDGE('',*,*,#15613,.F.);
#20761=ORIENTED_EDGE('',*,*,#15604,.F.);
#20762=ORIENTED_EDGE('',*,*,#15600,.F.);
#20763=ORIENTED_EDGE('',*,*,#15599,.F.);
#20764=ORIENTED_EDGE('',*,*,#15596,.F.);
#20765=ORIENTED_EDGE('',*,*,#15593,.F.);
#20766=ORIENTED_EDGE('',*,*,#15633,.F.);
#20767=ORIENTED_EDGE('',*,*,#15634,.T.);
#20768=ORIENTED_EDGE('',*,*,#15635,.F.);
#20769=ORIENTED_EDGE('',*,*,#15616,.F.);
#20770=ORIENTED_EDGE('',*,*,#15636,.F.);
#20771=ORIENTED_EDGE('',*,*,#15637,.T.);
#20772=ORIENTED_EDGE('',*,*,#15618,.F.);
#20773=ORIENTED_EDGE('',*,*,#15637,.F.);
#20774=ORIENTED_EDGE('',*,*,#15633,.T.);
#20775=ORIENTED_EDGE('',*,*,#15638,.T.);
#20776=ORIENTED_EDGE('',*,*,#15639,.T.);
#20777=ORIENTED_EDGE('',*,*,#15638,.F.);
#20778=ORIENTED_EDGE('',*,*,#15640,.F.);
#20779=ORIENTED_EDGE('',*,*,#15641,.T.);
#20780=ORIENTED_EDGE('',*,*,#15639,.F.);
#20781=ORIENTED_EDGE('',*,*,#15641,.F.);
#20782=ORIENTED_EDGE('',*,*,#15635,.T.);
#20783=ORIENTED_EDGE('',*,*,#15642,.T.);
#20784=ORIENTED_EDGE('',*,*,#15643,.T.);
#20785=ORIENTED_EDGE('',*,*,#15642,.F.);
#20786=ORIENTED_EDGE('',*,*,#15644,.F.);
#20787=ORIENTED_EDGE('',*,*,#15645,.T.);
#20788=ORIENTED_EDGE('',*,*,#15643,.F.);
#20789=ORIENTED_EDGE('',*,*,#15645,.F.);
#20790=ORIENTED_EDGE('',*,*,#15646,.T.);
#20791=ORIENTED_EDGE('',*,*,#15647,.T.);
#20792=ORIENTED_EDGE('',*,*,#15614,.F.);
#20793=ORIENTED_EDGE('',*,*,#15632,.T.);
#20794=ORIENTED_EDGE('',*,*,#15648,.T.);
#20795=ORIENTED_EDGE('',*,*,#15649,.T.);
#20796=ORIENTED_EDGE('',*,*,#15646,.F.);
#20797=ORIENTED_EDGE('',*,*,#15631,.T.);
#20798=ORIENTED_EDGE('',*,*,#15650,.T.);
#20799=ORIENTED_EDGE('',*,*,#15651,.T.);
#20800=ORIENTED_EDGE('',*,*,#15648,.F.);
#20801=ORIENTED_EDGE('',*,*,#15630,.T.);
#20802=ORIENTED_EDGE('',*,*,#15652,.T.);
#20803=ORIENTED_EDGE('',*,*,#15653,.T.);
#20804=ORIENTED_EDGE('',*,*,#15650,.F.);
#20805=ORIENTED_EDGE('',*,*,#15629,.T.);
#20806=ORIENTED_EDGE('',*,*,#15654,.T.);
#20807=ORIENTED_EDGE('',*,*,#15655,.T.);
#20808=ORIENTED_EDGE('',*,*,#15652,.F.);
#20809=ORIENTED_EDGE('',*,*,#15628,.T.);
#20810=ORIENTED_EDGE('',*,*,#15656,.T.);
#20811=ORIENTED_EDGE('',*,*,#15657,.T.);
#20812=ORIENTED_EDGE('',*,*,#15654,.F.);
#20813=ORIENTED_EDGE('',*,*,#15627,.T.);
#20814=ORIENTED_EDGE('',*,*,#15658,.T.);
#20815=ORIENTED_EDGE('',*,*,#15659,.T.);
#20816=ORIENTED_EDGE('',*,*,#15656,.F.);
#20817=ORIENTED_EDGE('',*,*,#15626,.T.);
#20818=ORIENTED_EDGE('',*,*,#15660,.T.);
#20819=ORIENTED_EDGE('',*,*,#15661,.T.);
#20820=ORIENTED_EDGE('',*,*,#15658,.F.);
#20821=ORIENTED_EDGE('',*,*,#15625,.T.);
#20822=ORIENTED_EDGE('',*,*,#15662,.T.);
#20823=ORIENTED_EDGE('',*,*,#15663,.T.);
#20824=ORIENTED_EDGE('',*,*,#15660,.F.);
#20825=ORIENTED_EDGE('',*,*,#15624,.T.);
#20826=ORIENTED_EDGE('',*,*,#15664,.T.);
#20827=ORIENTED_EDGE('',*,*,#15665,.T.);
#20828=ORIENTED_EDGE('',*,*,#15662,.F.);
#20829=ORIENTED_EDGE('',*,*,#15623,.T.);
#20830=ORIENTED_EDGE('',*,*,#15666,.T.);
#20831=ORIENTED_EDGE('',*,*,#15667,.T.);
#20832=ORIENTED_EDGE('',*,*,#15664,.F.);
#20833=ORIENTED_EDGE('',*,*,#15622,.T.);
#20834=ORIENTED_EDGE('',*,*,#15612,.F.);
#20835=ORIENTED_EDGE('',*,*,#15668,.T.);
#20836=ORIENTED_EDGE('',*,*,#15669,.T.);
#20837=ORIENTED_EDGE('',*,*,#15533,.T.);
#20838=ORIENTED_EDGE('',*,*,#15581,.T.);
#20839=ORIENTED_EDGE('',*,*,#15670,.T.);
#20840=ORIENTED_EDGE('',*,*,#15671,.T.);
#20841=ORIENTED_EDGE('',*,*,#15672,.T.);
#20842=ORIENTED_EDGE('',*,*,#15673,.T.);
#20843=ORIENTED_EDGE('',*,*,#15674,.T.);
#20844=ORIENTED_EDGE('',*,*,#15675,.T.);
#20845=ORIENTED_EDGE('',*,*,#15670,.F.);
#20846=ORIENTED_EDGE('',*,*,#15676,.T.);
#20847=ORIENTED_EDGE('',*,*,#15677,.T.);
#20848=ORIENTED_EDGE('',*,*,#15678,.T.);
#20849=ORIENTED_EDGE('',*,*,#15674,.F.);
#20850=ORIENTED_EDGE('',*,*,#15679,.T.);
#20851=ORIENTED_EDGE('',*,*,#15680,.T.);
#20852=ORIENTED_EDGE('',*,*,#15681,.T.);
#20853=ORIENTED_EDGE('',*,*,#15677,.F.);
#20854=ORIENTED_EDGE('',*,*,#15682,.T.);
#20855=ORIENTED_EDGE('',*,*,#15683,.T.);
#20856=ORIENTED_EDGE('',*,*,#15684,.T.);
#20857=ORIENTED_EDGE('',*,*,#15680,.F.);
#20858=ORIENTED_EDGE('',*,*,#15685,.T.);
#20859=ORIENTED_EDGE('',*,*,#15686,.T.);
#20860=ORIENTED_EDGE('',*,*,#15687,.T.);
#20861=ORIENTED_EDGE('',*,*,#15683,.F.);
#20862=ORIENTED_EDGE('',*,*,#15688,.T.);
#20863=ORIENTED_EDGE('',*,*,#15689,.T.);
#20864=ORIENTED_EDGE('',*,*,#15690,.T.);
#20865=ORIENTED_EDGE('',*,*,#15686,.F.);
#20866=ORIENTED_EDGE('',*,*,#15691,.T.);
#20867=ORIENTED_EDGE('',*,*,#15672,.F.);
#20868=ORIENTED_EDGE('',*,*,#15692,.T.);
#20869=ORIENTED_EDGE('',*,*,#15689,.F.);
#20870=ORIENTED_EDGE('',*,*,#15693,.T.);
#20871=ORIENTED_EDGE('',*,*,#15687,.F.);
#20872=ORIENTED_EDGE('',*,*,#15694,.T.);
#20873=ORIENTED_EDGE('',*,*,#15695,.F.);
#20874=ORIENTED_EDGE('',*,*,#15696,.T.);
#20875=ORIENTED_EDGE('',*,*,#15690,.F.);
#20876=ORIENTED_EDGE('',*,*,#15697,.F.);
#20877=ORIENTED_EDGE('',*,*,#15698,.F.);
#20878=ORIENTED_EDGE('',*,*,#15694,.F.);
#20879=ORIENTED_EDGE('',*,*,#15692,.F.);
#20880=ORIENTED_EDGE('',*,*,#15699,.T.);
#20881=ORIENTED_EDGE('',*,*,#15700,.T.);
#20882=ORIENTED_EDGE('',*,*,#15701,.T.);
#20883=ORIENTED_EDGE('',*,*,#15702,.F.);
#20884=ORIENTED_EDGE('',*,*,#15697,.T.);
#20885=ORIENTED_EDGE('',*,*,#15671,.F.);
#20886=ORIENTED_EDGE('',*,*,#15703,.F.);
#20887=ORIENTED_EDGE('',*,*,#15619,.F.);
#20888=ORIENTED_EDGE('',*,*,#15587,.F.);
#20889=ORIENTED_EDGE('',*,*,#15704,.T.);
#20890=ORIENTED_EDGE('',*,*,#15705,.F.);
#20891=ORIENTED_EDGE('',*,*,#15701,.F.);
#20892=ORIENTED_EDGE('',*,*,#15706,.T.);
#20893=ORIENTED_EDGE('',*,*,#15707,.T.);
#20894=ORIENTED_EDGE('',*,*,#15699,.F.);
#20895=ORIENTED_EDGE('',*,*,#15708,.T.);
#20896=ORIENTED_EDGE('',*,*,#15673,.F.);
#20897=ORIENTED_EDGE('',*,*,#15693,.F.);
#20898=ORIENTED_EDGE('',*,*,#15691,.F.);
#20899=ORIENTED_EDGE('',*,*,#15688,.F.);
#20900=ORIENTED_EDGE('',*,*,#15685,.F.);
#20901=ORIENTED_EDGE('',*,*,#15682,.F.);
#20902=ORIENTED_EDGE('',*,*,#15679,.F.);
#20903=ORIENTED_EDGE('',*,*,#15676,.F.);
#20904=ORIENTED_EDGE('',*,*,#15669,.F.);
#20905=ORIENTED_EDGE('',*,*,#15709,.T.);
#20906=ORIENTED_EDGE('',*,*,#15710,.T.);
#20907=ORIENTED_EDGE('',*,*,#15534,.T.);
#20908=ORIENTED_EDGE('',*,*,#15711,.T.);
#20909=ORIENTED_EDGE('',*,*,#15535,.T.);
#20910=ORIENTED_EDGE('',*,*,#15710,.F.);
#20911=ORIENTED_EDGE('',*,*,#15712,.T.);
#20912=ORIENTED_EDGE('',*,*,#15711,.F.);
#20913=ORIENTED_EDGE('',*,*,#15713,.T.);
#20914=ORIENTED_EDGE('',*,*,#15714,.T.);
#20915=ORIENTED_EDGE('',*,*,#15536,.T.);
#20916=ORIENTED_EDGE('',*,*,#15715,.T.);
#20917=ORIENTED_EDGE('',*,*,#15537,.T.);
#20918=ORIENTED_EDGE('',*,*,#15714,.F.);
#20919=ORIENTED_EDGE('',*,*,#15716,.T.);
#20920=ORIENTED_EDGE('',*,*,#15715,.F.);
#20921=ORIENTED_EDGE('',*,*,#15717,.T.);
#20922=ORIENTED_EDGE('',*,*,#15718,.T.);
#20923=ORIENTED_EDGE('',*,*,#15538,.T.);
#20924=ORIENTED_EDGE('',*,*,#15719,.T.);
#20925=ORIENTED_EDGE('',*,*,#15539,.T.);
#20926=ORIENTED_EDGE('',*,*,#15718,.F.);
#20927=ORIENTED_EDGE('',*,*,#15720,.T.);
#20928=ORIENTED_EDGE('',*,*,#15719,.F.);
#20929=ORIENTED_EDGE('',*,*,#15721,.T.);
#20930=ORIENTED_EDGE('',*,*,#15722,.T.);
#20931=ORIENTED_EDGE('',*,*,#15540,.T.);
#20932=ORIENTED_EDGE('',*,*,#15723,.T.);
#20933=ORIENTED_EDGE('',*,*,#15541,.T.);
#20934=ORIENTED_EDGE('',*,*,#15722,.F.);
#20935=ORIENTED_EDGE('',*,*,#15724,.T.);
#20936=ORIENTED_EDGE('',*,*,#15723,.F.);
#20937=ORIENTED_EDGE('',*,*,#15725,.T.);
#20938=ORIENTED_EDGE('',*,*,#15726,.T.);
#20939=ORIENTED_EDGE('',*,*,#15542,.T.);
#20940=ORIENTED_EDGE('',*,*,#15727,.T.);
#20941=ORIENTED_EDGE('',*,*,#15543,.T.);
#20942=ORIENTED_EDGE('',*,*,#15726,.F.);
#20943=ORIENTED_EDGE('',*,*,#15728,.T.);
#20944=ORIENTED_EDGE('',*,*,#15727,.F.);
#20945=ORIENTED_EDGE('',*,*,#15729,.T.);
#20946=ORIENTED_EDGE('',*,*,#15730,.T.);
#20947=ORIENTED_EDGE('',*,*,#15544,.T.);
#20948=ORIENTED_EDGE('',*,*,#15731,.T.);
#20949=ORIENTED_EDGE('',*,*,#15545,.T.);
#20950=ORIENTED_EDGE('',*,*,#15730,.F.);
#20951=ORIENTED_EDGE('',*,*,#15732,.T.);
#20952=ORIENTED_EDGE('',*,*,#15731,.F.);
#20953=ORIENTED_EDGE('',*,*,#15733,.T.);
#20954=ORIENTED_EDGE('',*,*,#15734,.T.);
#20955=ORIENTED_EDGE('',*,*,#15546,.T.);
#20956=ORIENTED_EDGE('',*,*,#15735,.T.);
#20957=ORIENTED_EDGE('',*,*,#15547,.T.);
#20958=ORIENTED_EDGE('',*,*,#15734,.F.);
#20959=ORIENTED_EDGE('',*,*,#15736,.T.);
#20960=ORIENTED_EDGE('',*,*,#15735,.F.);
#20961=ORIENTED_EDGE('',*,*,#15695,.T.);
#20962=ORIENTED_EDGE('',*,*,#15737,.T.);
#20963=ORIENTED_EDGE('',*,*,#15548,.T.);
#20964=ORIENTED_EDGE('',*,*,#15738,.T.);
#20965=ORIENTED_EDGE('',*,*,#15549,.T.);
#20966=ORIENTED_EDGE('',*,*,#15737,.F.);
#20967=ORIENTED_EDGE('',*,*,#15698,.T.);
#20968=ORIENTED_EDGE('',*,*,#15738,.F.);
#20969=ORIENTED_EDGE('',*,*,#15702,.T.);
#20970=ORIENTED_EDGE('',*,*,#15739,.T.);
#20971=ORIENTED_EDGE('',*,*,#15550,.T.);
#20972=ORIENTED_EDGE('',*,*,#15526,.T.);
#20973=ORIENTED_EDGE('',*,*,#15739,.F.);
#20974=ORIENTED_EDGE('',*,*,#15705,.T.);
#20975=ORIENTED_EDGE('',*,*,#15566,.F.);
#20976=ORIENTED_EDGE('',*,*,#15684,.F.);
#20977=ORIENTED_EDGE('',*,*,#15696,.F.);
#20978=ORIENTED_EDGE('',*,*,#15736,.F.);
#20979=ORIENTED_EDGE('',*,*,#15740,.F.);
#20980=ORIENTED_EDGE('',*,*,#15681,.F.);
#20981=ORIENTED_EDGE('',*,*,#15740,.T.);
#20982=ORIENTED_EDGE('',*,*,#15733,.F.);
#20983=ORIENTED_EDGE('',*,*,#15741,.T.);
#20984=ORIENTED_EDGE('',*,*,#15678,.F.);
#20985=ORIENTED_EDGE('',*,*,#15741,.F.);
#20986=ORIENTED_EDGE('',*,*,#15732,.F.);
#20987=ORIENTED_EDGE('',*,*,#15742,.F.);
#20988=ORIENTED_EDGE('',*,*,#15666,.F.);
#20989=ORIENTED_EDGE('',*,*,#15621,.F.);
#20990=ORIENTED_EDGE('',*,*,#15743,.F.);
#20991=ORIENTED_EDGE('',*,*,#15667,.F.);
#20992=ORIENTED_EDGE('',*,*,#15742,.T.);
#20993=ORIENTED_EDGE('',*,*,#15729,.F.);
#20994=ORIENTED_EDGE('',*,*,#15744,.T.);
#20995=ORIENTED_EDGE('',*,*,#15665,.F.);
#20996=ORIENTED_EDGE('',*,*,#15744,.F.);
#20997=ORIENTED_EDGE('',*,*,#15728,.F.);
#20998=ORIENTED_EDGE('',*,*,#15745,.F.);
#20999=ORIENTED_EDGE('',*,*,#15663,.F.);
#21000=ORIENTED_EDGE('',*,*,#15745,.T.);
#21001=ORIENTED_EDGE('',*,*,#15725,.F.);
#21002=ORIENTED_EDGE('',*,*,#15746,.T.);
#21003=ORIENTED_EDGE('',*,*,#15661,.F.);
#21004=ORIENTED_EDGE('',*,*,#15746,.F.);
#21005=ORIENTED_EDGE('',*,*,#15724,.F.);
#21006=ORIENTED_EDGE('',*,*,#15747,.F.);
#21007=ORIENTED_EDGE('',*,*,#15659,.F.);
#21008=ORIENTED_EDGE('',*,*,#15747,.T.);
#21009=ORIENTED_EDGE('',*,*,#15721,.F.);
#21010=ORIENTED_EDGE('',*,*,#15748,.T.);
#21011=ORIENTED_EDGE('',*,*,#15657,.F.);
#21012=ORIENTED_EDGE('',*,*,#15748,.F.);
#21013=ORIENTED_EDGE('',*,*,#15720,.F.);
#21014=ORIENTED_EDGE('',*,*,#15749,.F.);
#21015=ORIENTED_EDGE('',*,*,#15655,.F.);
#21016=ORIENTED_EDGE('',*,*,#15749,.T.);
#21017=ORIENTED_EDGE('',*,*,#15717,.F.);
#21018=ORIENTED_EDGE('',*,*,#15750,.T.);
#21019=ORIENTED_EDGE('',*,*,#15653,.F.);
#21020=ORIENTED_EDGE('',*,*,#15750,.F.);
#21021=ORIENTED_EDGE('',*,*,#15716,.F.);
#21022=ORIENTED_EDGE('',*,*,#15751,.F.);
#21023=ORIENTED_EDGE('',*,*,#15651,.F.);
#21024=ORIENTED_EDGE('',*,*,#15751,.T.);
#21025=ORIENTED_EDGE('',*,*,#15713,.F.);
#21026=ORIENTED_EDGE('',*,*,#15752,.T.);
#21027=ORIENTED_EDGE('',*,*,#15649,.F.);
#21028=ORIENTED_EDGE('',*,*,#15752,.F.);
#21029=ORIENTED_EDGE('',*,*,#15712,.F.);
#21030=ORIENTED_EDGE('',*,*,#15753,.F.);
#21031=ORIENTED_EDGE('',*,*,#15647,.F.);
#21032=ORIENTED_EDGE('',*,*,#15753,.T.);
#21033=ORIENTED_EDGE('',*,*,#15709,.F.);
#21034=ORIENTED_EDGE('',*,*,#15754,.T.);
#21035=ORIENTED_EDGE('',*,*,#15615,.F.);
#21036=ORIENTED_EDGE('',*,*,#15754,.F.);
#21037=ORIENTED_EDGE('',*,*,#15668,.F.);
#21038=ORIENTED_EDGE('',*,*,#15611,.F.);
#21039=ORIENTED_EDGE('',*,*,#15552,.T.);
#21040=ORIENTED_EDGE('',*,*,#15755,.T.);
#21041=ORIENTED_EDGE('',*,*,#15644,.T.);
#21042=ORIENTED_EDGE('',*,*,#15755,.F.);
#21043=ORIENTED_EDGE('',*,*,#15559,.T.);
#21044=ORIENTED_EDGE('',*,*,#15756,.T.);
#21045=ORIENTED_EDGE('',*,*,#15640,.T.);
#21046=ORIENTED_EDGE('',*,*,#15756,.F.);
#21047=ORIENTED_EDGE('',*,*,#15553,.T.);
#21048=ORIENTED_EDGE('',*,*,#15757,.T.);
#21049=ORIENTED_EDGE('',*,*,#15636,.T.);
#21050=ORIENTED_EDGE('',*,*,#15757,.F.);
#21051=ORIENTED_EDGE('',*,*,#15558,.T.);
#21052=ORIENTED_EDGE('',*,*,#15758,.T.);
#21053=ORIENTED_EDGE('',*,*,#15759,.T.);
#21054=ORIENTED_EDGE('',*,*,#15758,.F.);
#21055=ORIENTED_EDGE('',*,*,#15759,.F.);
#21056=ORIENTED_EDGE('',*,*,#15760,.T.);
#21057=ORIENTED_EDGE('',*,*,#15634,.F.);
#21058=ORIENTED_EDGE('',*,*,#15760,.F.);
#21059=ORIENTED_EDGE('',*,*,#15554,.F.);
#21060=ORIENTED_EDGE('',*,*,#15761,.T.);
#21061=ORIENTED_EDGE('',*,*,#15762,.F.);
#21062=ORIENTED_EDGE('',*,*,#15763,.F.);
#21063=ORIENTED_EDGE('',*,*,#15764,.F.);
#21064=ORIENTED_EDGE('',*,*,#15761,.F.);
#21065=ORIENTED_EDGE('',*,*,#15765,.F.);
#21066=ORIENTED_EDGE('',*,*,#15766,.F.);
#21067=ORIENTED_EDGE('',*,*,#15767,.T.);
#21068=ORIENTED_EDGE('',*,*,#15768,.T.);
#21069=ORIENTED_EDGE('',*,*,#15767,.F.);
#21070=ORIENTED_EDGE('',*,*,#15768,.F.);
#21071=ORIENTED_EDGE('',*,*,#15700,.F.);
#21072=ORIENTED_EDGE('',*,*,#15707,.F.);
#21073=ORIENTED_EDGE('',*,*,#15769,.T.);
#21074=ORIENTED_EDGE('',*,*,#15762,.T.);
#21075=ORIENTED_EDGE('',*,*,#15770,.T.);
#21076=ORIENTED_EDGE('',*,*,#15771,.T.);
#21077=ORIENTED_EDGE('',*,*,#15770,.F.);
#21078=ORIENTED_EDGE('',*,*,#15764,.T.);
#21079=ORIENTED_EDGE('',*,*,#15763,.T.);
#21080=ORIENTED_EDGE('',*,*,#15769,.F.);
#21081=ORIENTED_EDGE('',*,*,#15706,.F.);
#21082=ORIENTED_EDGE('',*,*,#15765,.T.);
#21083=ORIENTED_EDGE('',*,*,#15766,.T.);
#21084=ORIENTED_EDGE('',*,*,#15771,.F.);
#21085=ORIENTED_EDGE('',*,*,#15708,.F.);
#21086=ORIENTED_EDGE('',*,*,#15772,.T.);
#21087=ORIENTED_EDGE('',*,*,#15773,.T.);
#21088=ORIENTED_EDGE('',*,*,#15772,.F.);
#21089=ORIENTED_EDGE('',*,*,#15773,.F.);
#21090=ORIENTED_EDGE('',*,*,#15565,.F.);
#21091=ORIENTED_EDGE('',*,*,#15561,.F.);
#21092=ORIENTED_EDGE('',*,*,#15557,.F.);
#21093=ORIENTED_EDGE('',*,*,#15774,.T.);
#21094=ORIENTED_EDGE('',*,*,#15775,.T.);
#21095=ORIENTED_EDGE('',*,*,#15774,.F.);
#21096=ORIENTED_EDGE('',*,*,#15775,.F.);
#21097=ORIENTED_EDGE('',*,*,#15556,.F.);
#21098=ORIENTED_EDGE('',*,*,#15776,.T.);
#21099=ORIENTED_EDGE('',*,*,#15777,.T.);
#21100=ORIENTED_EDGE('',*,*,#15776,.F.);
#21101=ORIENTED_EDGE('',*,*,#15777,.F.);
#21102=ORIENTED_EDGE('',*,*,#15555,.F.);
#21103=ORIENTED_EDGE('',*,*,#15778,.T.);
#21104=ORIENTED_EDGE('',*,*,#15779,.T.);
#21105=ORIENTED_EDGE('',*,*,#15778,.F.);
#21106=ORIENTED_EDGE('',*,*,#15779,.F.);
#21107=ORIENTED_EDGE('',*,*,#15569,.F.);
#21108=ORIENTED_EDGE('',*,*,#15780,.T.);
#21109=ORIENTED_EDGE('',*,*,#15592,.F.);
#21110=ORIENTED_EDGE('',*,*,#15606,.T.);
#21111=ORIENTED_EDGE('',*,*,#15567,.F.);
#21112=ORIENTED_EDGE('',*,*,#15704,.F.);
#21113=ORIENTED_EDGE('',*,*,#15590,.F.);
#21114=ORIENTED_EDGE('',*,*,#15780,.F.);
#21115=ORIENTED_EDGE('',*,*,#15675,.F.);
#21116=ORIENTED_EDGE('',*,*,#15743,.T.);
#21117=ORIENTED_EDGE('',*,*,#15620,.T.);
#21118=ORIENTED_EDGE('',*,*,#15703,.T.);
#21119=ORIENTED_EDGE('',*,*,#15781,.T.);
#21120=ORIENTED_EDGE('',*,*,#15782,.T.);
#21121=ORIENTED_EDGE('',*,*,#15783,.T.);
#21122=ORIENTED_EDGE('',*,*,#15782,.F.);
#21123=ORIENTED_EDGE('',*,*,#15781,.F.);
#21124=ORIENTED_EDGE('',*,*,#15784,.T.);
#21125=ORIENTED_EDGE('',*,*,#15785,.F.);
#21126=ORIENTED_EDGE('',*,*,#15784,.F.);
#21127=ORIENTED_EDGE('',*,*,#15786,.F.);
#21128=ORIENTED_EDGE('',*,*,#15783,.F.);
#21129=ORIENTED_EDGE('',*,*,#15787,.T.);
#21130=ORIENTED_EDGE('',*,*,#15788,.T.);
#21131=ORIENTED_EDGE('',*,*,#15789,.T.);
#21132=ORIENTED_EDGE('',*,*,#15788,.F.);
#21133=ORIENTED_EDGE('',*,*,#15787,.F.);
#21134=ORIENTED_EDGE('',*,*,#15790,.T.);
#21135=ORIENTED_EDGE('',*,*,#15791,.F.);
#21136=ORIENTED_EDGE('',*,*,#15790,.F.);
#21137=ORIENTED_EDGE('',*,*,#15792,.F.);
#21138=ORIENTED_EDGE('',*,*,#15789,.F.);
#21139=ORIENTED_EDGE('',*,*,#15793,.T.);
#21140=ORIENTED_EDGE('',*,*,#15794,.T.);
#21141=ORIENTED_EDGE('',*,*,#15795,.T.);
#21142=ORIENTED_EDGE('',*,*,#15794,.F.);
#21143=ORIENTED_EDGE('',*,*,#15793,.F.);
#21144=ORIENTED_EDGE('',*,*,#15796,.T.);
#21145=ORIENTED_EDGE('',*,*,#15797,.F.);
#21146=ORIENTED_EDGE('',*,*,#15796,.F.);
#21147=ORIENTED_EDGE('',*,*,#15798,.F.);
#21148=ORIENTED_EDGE('',*,*,#15795,.F.);
#21149=ORIENTED_EDGE('',*,*,#15799,.T.);
#21150=ORIENTED_EDGE('',*,*,#15800,.T.);
#21151=ORIENTED_EDGE('',*,*,#15801,.T.);
#21152=ORIENTED_EDGE('',*,*,#15800,.F.);
#21153=ORIENTED_EDGE('',*,*,#15799,.F.);
#21154=ORIENTED_EDGE('',*,*,#15802,.T.);
#21155=ORIENTED_EDGE('',*,*,#15803,.F.);
#21156=ORIENTED_EDGE('',*,*,#15802,.F.);
#21157=ORIENTED_EDGE('',*,*,#15804,.F.);
#21158=ORIENTED_EDGE('',*,*,#15801,.F.);
#21159=ORIENTED_EDGE('',*,*,#15805,.T.);
#21160=ORIENTED_EDGE('',*,*,#15806,.T.);
#21161=ORIENTED_EDGE('',*,*,#15807,.T.);
#21162=ORIENTED_EDGE('',*,*,#15806,.F.);
#21163=ORIENTED_EDGE('',*,*,#15805,.F.);
#21164=ORIENTED_EDGE('',*,*,#15808,.T.);
#21165=ORIENTED_EDGE('',*,*,#15809,.F.);
#21166=ORIENTED_EDGE('',*,*,#15808,.F.);
#21167=ORIENTED_EDGE('',*,*,#15810,.F.);
#21168=ORIENTED_EDGE('',*,*,#15807,.F.);
#21169=ORIENTED_EDGE('',*,*,#15811,.T.);
#21170=ORIENTED_EDGE('',*,*,#15812,.T.);
#21171=ORIENTED_EDGE('',*,*,#15813,.T.);
#21172=ORIENTED_EDGE('',*,*,#15812,.F.);
#21173=ORIENTED_EDGE('',*,*,#15811,.F.);
#21174=ORIENTED_EDGE('',*,*,#15814,.T.);
#21175=ORIENTED_EDGE('',*,*,#15815,.F.);
#21176=ORIENTED_EDGE('',*,*,#15814,.F.);
#21177=ORIENTED_EDGE('',*,*,#15816,.F.);
#21178=ORIENTED_EDGE('',*,*,#15813,.F.);
#21179=ORIENTED_EDGE('',*,*,#15817,.T.);
#21180=ORIENTED_EDGE('',*,*,#15818,.T.);
#21181=ORIENTED_EDGE('',*,*,#15819,.T.);
#21182=ORIENTED_EDGE('',*,*,#15818,.F.);
#21183=ORIENTED_EDGE('',*,*,#15817,.F.);
#21184=ORIENTED_EDGE('',*,*,#15820,.T.);
#21185=ORIENTED_EDGE('',*,*,#15821,.F.);
#21186=ORIENTED_EDGE('',*,*,#15820,.F.);
#21187=ORIENTED_EDGE('',*,*,#15822,.F.);
#21188=ORIENTED_EDGE('',*,*,#15819,.F.);
#21189=ORIENTED_EDGE('',*,*,#15823,.T.);
#21190=ORIENTED_EDGE('',*,*,#15824,.T.);
#21191=ORIENTED_EDGE('',*,*,#15825,.T.);
#21192=ORIENTED_EDGE('',*,*,#15824,.F.);
#21193=ORIENTED_EDGE('',*,*,#15823,.F.);
#21194=ORIENTED_EDGE('',*,*,#15826,.T.);
#21195=ORIENTED_EDGE('',*,*,#15827,.F.);
#21196=ORIENTED_EDGE('',*,*,#15826,.F.);
#21197=ORIENTED_EDGE('',*,*,#15828,.F.);
#21198=ORIENTED_EDGE('',*,*,#15825,.F.);
#21199=ORIENTED_EDGE('',*,*,#15829,.T.);
#21200=ORIENTED_EDGE('',*,*,#15830,.T.);
#21201=ORIENTED_EDGE('',*,*,#15831,.T.);
#21202=ORIENTED_EDGE('',*,*,#15830,.F.);
#21203=ORIENTED_EDGE('',*,*,#15832,.F.);
#21204=ORIENTED_EDGE('',*,*,#15833,.T.);
#21205=ORIENTED_EDGE('',*,*,#15829,.F.);
#21206=ORIENTED_EDGE('',*,*,#15833,.F.);
#21207=ORIENTED_EDGE('',*,*,#15834,.F.);
#21208=ORIENTED_EDGE('',*,*,#15831,.F.);
#21209=ORIENTED_EDGE('',*,*,#15835,.T.);
#21210=ORIENTED_EDGE('',*,*,#15836,.T.);
#21211=ORIENTED_EDGE('',*,*,#15837,.T.);
#21212=ORIENTED_EDGE('',*,*,#15838,.T.);
#21213=ORIENTED_EDGE('',*,*,#15839,.T.);
#21214=ORIENTED_EDGE('',*,*,#15840,.T.);
#21215=ORIENTED_EDGE('',*,*,#15840,.F.);
#21216=ORIENTED_EDGE('',*,*,#15841,.T.);
#21217=ORIENTED_EDGE('',*,*,#15842,.F.);
#21218=ORIENTED_EDGE('',*,*,#15843,.F.);
#21219=ORIENTED_EDGE('',*,*,#15844,.T.);
#21220=ORIENTED_EDGE('',*,*,#15845,.T.);
#21221=ORIENTED_EDGE('',*,*,#15839,.F.);
#21222=ORIENTED_EDGE('',*,*,#15846,.F.);
#21223=ORIENTED_EDGE('',*,*,#15847,.F.);
#21224=ORIENTED_EDGE('',*,*,#15841,.F.);
#21225=ORIENTED_EDGE('',*,*,#15838,.F.);
#21226=ORIENTED_EDGE('',*,*,#15848,.F.);
#21227=ORIENTED_EDGE('',*,*,#15849,.T.);
#21228=ORIENTED_EDGE('',*,*,#15850,.T.);
#21229=ORIENTED_EDGE('',*,*,#15851,.F.);
#21230=ORIENTED_EDGE('',*,*,#15846,.T.);
#21231=ORIENTED_EDGE('',*,*,#15852,.T.);
#21232=ORIENTED_EDGE('',*,*,#15853,.T.);
#21233=ORIENTED_EDGE('',*,*,#15854,.T.);
#21234=ORIENTED_EDGE('',*,*,#15853,.F.);
#21235=ORIENTED_EDGE('',*,*,#15852,.F.);
#21236=ORIENTED_EDGE('',*,*,#15855,.T.);
#21237=ORIENTED_EDGE('',*,*,#15856,.F.);
#21238=ORIENTED_EDGE('',*,*,#15855,.F.);
#21239=ORIENTED_EDGE('',*,*,#15857,.F.);
#21240=ORIENTED_EDGE('',*,*,#15854,.F.);
#21241=ORIENTED_EDGE('',*,*,#15858,.T.);
#21242=ORIENTED_EDGE('',*,*,#15859,.T.);
#21243=ORIENTED_EDGE('',*,*,#15860,.T.);
#21244=ORIENTED_EDGE('',*,*,#15859,.F.);
#21245=ORIENTED_EDGE('',*,*,#15858,.F.);
#21246=ORIENTED_EDGE('',*,*,#15861,.T.);
#21247=ORIENTED_EDGE('',*,*,#15862,.F.);
#21248=ORIENTED_EDGE('',*,*,#15861,.F.);
#21249=ORIENTED_EDGE('',*,*,#15863,.F.);
#21250=ORIENTED_EDGE('',*,*,#15860,.F.);
#21251=ORIENTED_EDGE('',*,*,#15864,.T.);
#21252=ORIENTED_EDGE('',*,*,#15865,.T.);
#21253=ORIENTED_EDGE('',*,*,#15866,.T.);
#21254=ORIENTED_EDGE('',*,*,#15867,.T.);
#21255=ORIENTED_EDGE('',*,*,#15868,.T.);
#21256=ORIENTED_EDGE('',*,*,#15869,.T.);
#21257=ORIENTED_EDGE('',*,*,#15866,.F.);
#21258=ORIENTED_EDGE('',*,*,#15870,.T.);
#21259=ORIENTED_EDGE('',*,*,#15871,.F.);
#21260=ORIENTED_EDGE('',*,*,#15872,.T.);
#21261=ORIENTED_EDGE('',*,*,#15873,.T.);
#21262=ORIENTED_EDGE('',*,*,#15874,.T.);
#21263=ORIENTED_EDGE('',*,*,#15865,.F.);
#21264=ORIENTED_EDGE('',*,*,#15875,.F.);
#21265=ORIENTED_EDGE('',*,*,#15876,.F.);
#21266=ORIENTED_EDGE('',*,*,#15870,.F.);
#21267=ORIENTED_EDGE('',*,*,#15864,.F.);
#21268=ORIENTED_EDGE('',*,*,#15877,.F.);
#21269=ORIENTED_EDGE('',*,*,#15878,.T.);
#21270=ORIENTED_EDGE('',*,*,#15879,.T.);
#21271=ORIENTED_EDGE('',*,*,#15880,.F.);
#21272=ORIENTED_EDGE('',*,*,#15875,.T.);
#21273=ORIENTED_EDGE('',*,*,#15842,.T.);
#21274=ORIENTED_EDGE('',*,*,#15847,.T.);
#21275=ORIENTED_EDGE('',*,*,#15851,.T.);
#21276=ORIENTED_EDGE('',*,*,#15881,.T.);
#21277=ORIENTED_EDGE('',*,*,#15882,.T.);
#21278=ORIENTED_EDGE('',*,*,#15883,.T.);
#21279=ORIENTED_EDGE('',*,*,#15884,.T.);
#21280=ORIENTED_EDGE('',*,*,#15885,.T.);
#21281=ORIENTED_EDGE('',*,*,#15886,.T.);
#21282=ORIENTED_EDGE('',*,*,#15871,.T.);
#21283=ORIENTED_EDGE('',*,*,#15876,.T.);
#21284=ORIENTED_EDGE('',*,*,#15880,.T.);
#21285=ORIENTED_EDGE('',*,*,#15887,.T.);
#21286=ORIENTED_EDGE('',*,*,#15888,.T.);
#21287=ORIENTED_EDGE('',*,*,#15889,.T.);
#21288=ORIENTED_EDGE('',*,*,#15888,.F.);
#21289=ORIENTED_EDGE('',*,*,#15887,.F.);
#21290=ORIENTED_EDGE('',*,*,#15890,.T.);
#21291=ORIENTED_EDGE('',*,*,#15891,.F.);
#21292=ORIENTED_EDGE('',*,*,#15890,.F.);
#21293=ORIENTED_EDGE('',*,*,#15892,.F.);
#21294=ORIENTED_EDGE('',*,*,#15889,.F.);
#21295=ORIENTED_EDGE('',*,*,#15893,.T.);
#21296=ORIENTED_EDGE('',*,*,#15894,.T.);
#21297=ORIENTED_EDGE('',*,*,#15895,.T.);
#21298=ORIENTED_EDGE('',*,*,#15894,.F.);
#21299=ORIENTED_EDGE('',*,*,#15893,.F.);
#21300=ORIENTED_EDGE('',*,*,#15896,.T.);
#21301=ORIENTED_EDGE('',*,*,#15897,.F.);
#21302=ORIENTED_EDGE('',*,*,#15896,.F.);
#21303=ORIENTED_EDGE('',*,*,#15898,.F.);
#21304=ORIENTED_EDGE('',*,*,#15895,.F.);
#21305=ORIENTED_EDGE('',*,*,#15899,.T.);
#21306=ORIENTED_EDGE('',*,*,#15900,.T.);
#21307=ORIENTED_EDGE('',*,*,#15821,.T.);
#21308=ORIENTED_EDGE('',*,*,#15900,.F.);
#21309=ORIENTED_EDGE('',*,*,#15873,.F.);
#21310=ORIENTED_EDGE('',*,*,#15901,.F.);
#21311=ORIENTED_EDGE('',*,*,#15849,.F.);
#21312=ORIENTED_EDGE('',*,*,#15902,.F.);
#21313=ORIENTED_EDGE('',*,*,#15903,.F.);
#21314=ORIENTED_EDGE('',*,*,#15904,.F.);
#21315=ORIENTED_EDGE('',*,*,#15905,.F.);
#21316=ORIENTED_EDGE('',*,*,#15906,.F.);
#21317=ORIENTED_EDGE('',*,*,#15907,.F.);
#21318=ORIENTED_EDGE('',*,*,#15908,.F.);
#21319=ORIENTED_EDGE('',*,*,#15909,.F.);
#21320=ORIENTED_EDGE('',*,*,#15910,.F.);
#21321=ORIENTED_EDGE('',*,*,#15911,.F.);
#21322=ORIENTED_EDGE('',*,*,#15912,.F.);
#21323=ORIENTED_EDGE('',*,*,#15913,.F.);
#21324=ORIENTED_EDGE('',*,*,#15914,.F.);
#21325=ORIENTED_EDGE('',*,*,#15915,.F.);
#21326=ORIENTED_EDGE('',*,*,#15916,.F.);
#21327=ORIENTED_EDGE('',*,*,#15917,.F.);
#21328=ORIENTED_EDGE('',*,*,#15918,.F.);
#21329=ORIENTED_EDGE('',*,*,#15919,.F.);
#21330=ORIENTED_EDGE('',*,*,#15920,.F.);
#21331=ORIENTED_EDGE('',*,*,#15921,.F.);
#21332=ORIENTED_EDGE('',*,*,#15922,.F.);
#21333=ORIENTED_EDGE('',*,*,#15923,.F.);
#21334=ORIENTED_EDGE('',*,*,#15924,.T.);
#21335=ORIENTED_EDGE('',*,*,#15925,.F.);
#21336=ORIENTED_EDGE('',*,*,#15926,.F.);
#21337=ORIENTED_EDGE('',*,*,#15927,.F.);
#21338=ORIENTED_EDGE('',*,*,#15928,.F.);
#21339=ORIENTED_EDGE('',*,*,#15929,.F.);
#21340=ORIENTED_EDGE('',*,*,#15930,.F.);
#21341=ORIENTED_EDGE('',*,*,#15931,.F.);
#21342=ORIENTED_EDGE('',*,*,#15932,.F.);
#21343=ORIENTED_EDGE('',*,*,#15933,.F.);
#21344=ORIENTED_EDGE('',*,*,#15934,.F.);
#21345=ORIENTED_EDGE('',*,*,#15935,.F.);
#21346=ORIENTED_EDGE('',*,*,#15936,.F.);
#21347=ORIENTED_EDGE('',*,*,#15937,.F.);
#21348=ORIENTED_EDGE('',*,*,#15938,.F.);
#21349=ORIENTED_EDGE('',*,*,#15939,.F.);
#21350=ORIENTED_EDGE('',*,*,#15940,.F.);
#21351=ORIENTED_EDGE('',*,*,#15941,.F.);
#21352=ORIENTED_EDGE('',*,*,#15942,.F.);
#21353=ORIENTED_EDGE('',*,*,#15943,.F.);
#21354=ORIENTED_EDGE('',*,*,#15899,.F.);
#21355=ORIENTED_EDGE('',*,*,#15903,.T.);
#21356=ORIENTED_EDGE('',*,*,#15944,.T.);
#21357=ORIENTED_EDGE('',*,*,#15815,.T.);
#21358=ORIENTED_EDGE('',*,*,#15944,.F.);
#21359=ORIENTED_EDGE('',*,*,#15943,.T.);
#21360=ORIENTED_EDGE('',*,*,#15945,.T.);
#21361=ORIENTED_EDGE('',*,*,#15809,.T.);
#21362=ORIENTED_EDGE('',*,*,#15945,.F.);
#21363=ORIENTED_EDGE('',*,*,#15904,.T.);
#21364=ORIENTED_EDGE('',*,*,#15946,.T.);
#21365=ORIENTED_EDGE('',*,*,#15803,.T.);
#21366=ORIENTED_EDGE('',*,*,#15946,.F.);
#21367=ORIENTED_EDGE('',*,*,#15942,.T.);
#21368=ORIENTED_EDGE('',*,*,#15947,.T.);
#21369=ORIENTED_EDGE('',*,*,#15797,.T.);
#21370=ORIENTED_EDGE('',*,*,#15947,.F.);
#21371=ORIENTED_EDGE('',*,*,#15905,.T.);
#21372=ORIENTED_EDGE('',*,*,#15948,.T.);
#21373=ORIENTED_EDGE('',*,*,#15791,.T.);
#21374=ORIENTED_EDGE('',*,*,#15948,.F.);
#21375=ORIENTED_EDGE('',*,*,#15941,.T.);
#21376=ORIENTED_EDGE('',*,*,#15949,.T.);
#21377=ORIENTED_EDGE('',*,*,#15785,.T.);
#21378=ORIENTED_EDGE('',*,*,#15949,.F.);
#21379=ORIENTED_EDGE('',*,*,#15906,.T.);
#21380=ORIENTED_EDGE('',*,*,#15950,.T.);
#21381=ORIENTED_EDGE('',*,*,#15827,.T.);
#21382=ORIENTED_EDGE('',*,*,#15950,.F.);
#21383=ORIENTED_EDGE('',*,*,#15940,.T.);
#21384=ORIENTED_EDGE('',*,*,#15951,.T.);
#21385=ORIENTED_EDGE('',*,*,#15952,.T.);
#21386=ORIENTED_EDGE('',*,*,#15951,.F.);
#21387=ORIENTED_EDGE('',*,*,#15953,.F.);
#21388=ORIENTED_EDGE('',*,*,#15954,.T.);
#21389=ORIENTED_EDGE('',*,*,#15952,.F.);
#21390=ORIENTED_EDGE('',*,*,#15954,.F.);
#21391=ORIENTED_EDGE('',*,*,#15907,.T.);
#21392=ORIENTED_EDGE('',*,*,#15955,.T.);
#21393=ORIENTED_EDGE('',*,*,#15956,.T.);
#21394=ORIENTED_EDGE('',*,*,#15955,.F.);
#21395=ORIENTED_EDGE('',*,*,#15957,.F.);
#21396=ORIENTED_EDGE('',*,*,#15958,.T.);
#21397=ORIENTED_EDGE('',*,*,#15956,.F.);
#21398=ORIENTED_EDGE('',*,*,#15958,.F.);
#21399=ORIENTED_EDGE('',*,*,#15939,.T.);
#21400=ORIENTED_EDGE('',*,*,#15959,.T.);
#21401=ORIENTED_EDGE('',*,*,#15897,.T.);
#21402=ORIENTED_EDGE('',*,*,#15959,.F.);
#21403=ORIENTED_EDGE('',*,*,#15908,.T.);
#21404=ORIENTED_EDGE('',*,*,#15960,.T.);
#21405=ORIENTED_EDGE('',*,*,#15891,.T.);
#21406=ORIENTED_EDGE('',*,*,#15960,.F.);
#21407=ORIENTED_EDGE('',*,*,#15881,.F.);
#21408=ORIENTED_EDGE('',*,*,#15850,.F.);
#21409=ORIENTED_EDGE('',*,*,#15901,.T.);
#21410=ORIENTED_EDGE('',*,*,#15872,.F.);
#21411=ORIENTED_EDGE('',*,*,#15886,.F.);
#21412=ORIENTED_EDGE('',*,*,#15961,.T.);
#21413=ORIENTED_EDGE('',*,*,#15837,.F.);
#21414=ORIENTED_EDGE('',*,*,#15962,.T.);
#21415=ORIENTED_EDGE('',*,*,#15867,.F.);
#21416=ORIENTED_EDGE('',*,*,#15874,.F.);
#21417=ORIENTED_EDGE('',*,*,#15902,.T.);
#21418=ORIENTED_EDGE('',*,*,#15848,.T.);
#21419=ORIENTED_EDGE('',*,*,#15882,.F.);
#21420=ORIENTED_EDGE('',*,*,#15961,.F.);
#21421=ORIENTED_EDGE('',*,*,#15885,.F.);
#21422=ORIENTED_EDGE('',*,*,#15963,.F.);
#21423=ORIENTED_EDGE('',*,*,#15909,.T.);
#21424=ORIENTED_EDGE('',*,*,#15964,.T.);
#21425=ORIENTED_EDGE('',*,*,#15965,.T.);
#21426=ORIENTED_EDGE('',*,*,#15964,.F.);
#21427=ORIENTED_EDGE('',*,*,#15966,.F.);
#21428=ORIENTED_EDGE('',*,*,#15967,.T.);
#21429=ORIENTED_EDGE('',*,*,#15965,.F.);
#21430=ORIENTED_EDGE('',*,*,#15967,.F.);
#21431=ORIENTED_EDGE('',*,*,#15938,.T.);
#21432=ORIENTED_EDGE('',*,*,#15968,.T.);
#21433=ORIENTED_EDGE('',*,*,#15969,.T.);
#21434=ORIENTED_EDGE('',*,*,#15968,.F.);
#21435=ORIENTED_EDGE('',*,*,#15970,.F.);
#21436=ORIENTED_EDGE('',*,*,#15971,.T.);
#21437=ORIENTED_EDGE('',*,*,#15969,.F.);
#21438=ORIENTED_EDGE('',*,*,#15971,.F.);
#21439=ORIENTED_EDGE('',*,*,#15910,.T.);
#21440=ORIENTED_EDGE('',*,*,#15972,.T.);
#21441=ORIENTED_EDGE('',*,*,#15973,.T.);
#21442=ORIENTED_EDGE('',*,*,#15972,.F.);
#21443=ORIENTED_EDGE('',*,*,#15974,.F.);
#21444=ORIENTED_EDGE('',*,*,#15975,.T.);
#21445=ORIENTED_EDGE('',*,*,#15973,.F.);
#21446=ORIENTED_EDGE('',*,*,#15975,.F.);
#21447=ORIENTED_EDGE('',*,*,#15937,.T.);
#21448=ORIENTED_EDGE('',*,*,#15976,.T.);
#21449=ORIENTED_EDGE('',*,*,#15977,.T.);
#21450=ORIENTED_EDGE('',*,*,#15976,.F.);
#21451=ORIENTED_EDGE('',*,*,#15978,.F.);
#21452=ORIENTED_EDGE('',*,*,#15979,.T.);
#21453=ORIENTED_EDGE('',*,*,#15977,.F.);
#21454=ORIENTED_EDGE('',*,*,#15979,.F.);
#21455=ORIENTED_EDGE('',*,*,#15911,.T.);
#21456=ORIENTED_EDGE('',*,*,#15980,.T.);
#21457=ORIENTED_EDGE('',*,*,#15981,.T.);
#21458=ORIENTED_EDGE('',*,*,#15980,.F.);
#21459=ORIENTED_EDGE('',*,*,#15982,.F.);
#21460=ORIENTED_EDGE('',*,*,#15983,.T.);
#21461=ORIENTED_EDGE('',*,*,#15981,.F.);
#21462=ORIENTED_EDGE('',*,*,#15983,.F.);
#21463=ORIENTED_EDGE('',*,*,#15936,.T.);
#21464=ORIENTED_EDGE('',*,*,#15984,.T.);
#21465=ORIENTED_EDGE('',*,*,#15985,.T.);
#21466=ORIENTED_EDGE('',*,*,#15984,.F.);
#21467=ORIENTED_EDGE('',*,*,#15986,.F.);
#21468=ORIENTED_EDGE('',*,*,#15987,.T.);
#21469=ORIENTED_EDGE('',*,*,#15985,.F.);
#21470=ORIENTED_EDGE('',*,*,#15987,.F.);
#21471=ORIENTED_EDGE('',*,*,#15912,.T.);
#21472=ORIENTED_EDGE('',*,*,#15988,.T.);
#21473=ORIENTED_EDGE('',*,*,#15989,.T.);
#21474=ORIENTED_EDGE('',*,*,#15988,.F.);
#21475=ORIENTED_EDGE('',*,*,#15990,.F.);
#21476=ORIENTED_EDGE('',*,*,#15991,.T.);
#21477=ORIENTED_EDGE('',*,*,#15989,.F.);
#21478=ORIENTED_EDGE('',*,*,#15991,.F.);
#21479=ORIENTED_EDGE('',*,*,#15935,.T.);
#21480=ORIENTED_EDGE('',*,*,#15992,.T.);
#21481=ORIENTED_EDGE('',*,*,#15993,.T.);
#21482=ORIENTED_EDGE('',*,*,#15992,.F.);
#21483=ORIENTED_EDGE('',*,*,#15994,.F.);
#21484=ORIENTED_EDGE('',*,*,#15995,.T.);
#21485=ORIENTED_EDGE('',*,*,#15993,.F.);
#21486=ORIENTED_EDGE('',*,*,#15995,.F.);
#21487=ORIENTED_EDGE('',*,*,#15913,.T.);
#21488=ORIENTED_EDGE('',*,*,#15996,.T.);
#21489=ORIENTED_EDGE('',*,*,#15997,.T.);
#21490=ORIENTED_EDGE('',*,*,#15996,.F.);
#21491=ORIENTED_EDGE('',*,*,#15998,.F.);
#21492=ORIENTED_EDGE('',*,*,#15999,.T.);
#21493=ORIENTED_EDGE('',*,*,#15997,.F.);
#21494=ORIENTED_EDGE('',*,*,#15999,.F.);
#21495=ORIENTED_EDGE('',*,*,#15934,.T.);
#21496=ORIENTED_EDGE('',*,*,#16000,.T.);
#21497=ORIENTED_EDGE('',*,*,#16001,.T.);
#21498=ORIENTED_EDGE('',*,*,#16000,.F.);
#21499=ORIENTED_EDGE('',*,*,#16002,.F.);
#21500=ORIENTED_EDGE('',*,*,#16003,.T.);
#21501=ORIENTED_EDGE('',*,*,#16001,.F.);
#21502=ORIENTED_EDGE('',*,*,#16003,.F.);
#21503=ORIENTED_EDGE('',*,*,#15914,.T.);
#21504=ORIENTED_EDGE('',*,*,#16004,.T.);
#21505=ORIENTED_EDGE('',*,*,#16005,.T.);
#21506=ORIENTED_EDGE('',*,*,#16004,.F.);
#21507=ORIENTED_EDGE('',*,*,#16006,.F.);
#21508=ORIENTED_EDGE('',*,*,#16007,.T.);
#21509=ORIENTED_EDGE('',*,*,#16005,.F.);
#21510=ORIENTED_EDGE('',*,*,#16007,.F.);
#21511=ORIENTED_EDGE('',*,*,#15933,.T.);
#21512=ORIENTED_EDGE('',*,*,#16008,.T.);
#21513=ORIENTED_EDGE('',*,*,#16009,.T.);
#21514=ORIENTED_EDGE('',*,*,#16008,.F.);
#21515=ORIENTED_EDGE('',*,*,#16010,.F.);
#21516=ORIENTED_EDGE('',*,*,#16011,.T.);
#21517=ORIENTED_EDGE('',*,*,#16009,.F.);
#21518=ORIENTED_EDGE('',*,*,#16011,.F.);
#21519=ORIENTED_EDGE('',*,*,#15915,.T.);
#21520=ORIENTED_EDGE('',*,*,#16012,.T.);
#21521=ORIENTED_EDGE('',*,*,#15862,.T.);
#21522=ORIENTED_EDGE('',*,*,#16012,.F.);
#21523=ORIENTED_EDGE('',*,*,#15932,.T.);
#21524=ORIENTED_EDGE('',*,*,#16013,.T.);
#21525=ORIENTED_EDGE('',*,*,#15856,.T.);
#21526=ORIENTED_EDGE('',*,*,#16013,.F.);
#21527=ORIENTED_EDGE('',*,*,#15916,.T.);
#21528=ORIENTED_EDGE('',*,*,#16014,.T.);
#21529=ORIENTED_EDGE('',*,*,#16015,.T.);
#21530=ORIENTED_EDGE('',*,*,#16014,.F.);
#21531=ORIENTED_EDGE('',*,*,#16016,.F.);
#21532=ORIENTED_EDGE('',*,*,#16017,.T.);
#21533=ORIENTED_EDGE('',*,*,#16015,.F.);
#21534=ORIENTED_EDGE('',*,*,#16017,.F.);
#21535=ORIENTED_EDGE('',*,*,#15931,.T.);
#21536=ORIENTED_EDGE('',*,*,#16018,.T.);
#21537=ORIENTED_EDGE('',*,*,#16019,.T.);
#21538=ORIENTED_EDGE('',*,*,#16018,.F.);
#21539=ORIENTED_EDGE('',*,*,#16020,.F.);
#21540=ORIENTED_EDGE('',*,*,#16021,.T.);
#21541=ORIENTED_EDGE('',*,*,#16019,.F.);
#21542=ORIENTED_EDGE('',*,*,#16021,.F.);
#21543=ORIENTED_EDGE('',*,*,#15917,.T.);
#21544=ORIENTED_EDGE('',*,*,#16022,.T.);
#21545=ORIENTED_EDGE('',*,*,#16023,.T.);
#21546=ORIENTED_EDGE('',*,*,#16022,.F.);
#21547=ORIENTED_EDGE('',*,*,#16024,.F.);
#21548=ORIENTED_EDGE('',*,*,#16025,.T.);
#21549=ORIENTED_EDGE('',*,*,#16023,.F.);
#21550=ORIENTED_EDGE('',*,*,#16025,.F.);
#21551=ORIENTED_EDGE('',*,*,#15930,.T.);
#21552=ORIENTED_EDGE('',*,*,#16026,.T.);
#21553=ORIENTED_EDGE('',*,*,#16027,.T.);
#21554=ORIENTED_EDGE('',*,*,#16026,.F.);
#21555=ORIENTED_EDGE('',*,*,#16028,.F.);
#21556=ORIENTED_EDGE('',*,*,#16029,.T.);
#21557=ORIENTED_EDGE('',*,*,#16027,.F.);
#21558=ORIENTED_EDGE('',*,*,#16029,.F.);
#21559=ORIENTED_EDGE('',*,*,#15918,.T.);
#21560=ORIENTED_EDGE('',*,*,#16030,.T.);
#21561=ORIENTED_EDGE('',*,*,#16031,.T.);
#21562=ORIENTED_EDGE('',*,*,#16030,.F.);
#21563=ORIENTED_EDGE('',*,*,#16032,.F.);
#21564=ORIENTED_EDGE('',*,*,#16033,.T.);
#21565=ORIENTED_EDGE('',*,*,#16031,.F.);
#21566=ORIENTED_EDGE('',*,*,#16033,.F.);
#21567=ORIENTED_EDGE('',*,*,#15929,.T.);
#21568=ORIENTED_EDGE('',*,*,#16034,.T.);
#21569=ORIENTED_EDGE('',*,*,#16035,.T.);
#21570=ORIENTED_EDGE('',*,*,#16034,.F.);
#21571=ORIENTED_EDGE('',*,*,#16036,.F.);
#21572=ORIENTED_EDGE('',*,*,#16037,.T.);
#21573=ORIENTED_EDGE('',*,*,#16035,.F.);
#21574=ORIENTED_EDGE('',*,*,#16037,.F.);
#21575=ORIENTED_EDGE('',*,*,#15919,.T.);
#21576=ORIENTED_EDGE('',*,*,#16038,.T.);
#21577=ORIENTED_EDGE('',*,*,#16039,.T.);
#21578=ORIENTED_EDGE('',*,*,#16038,.F.);
#21579=ORIENTED_EDGE('',*,*,#16040,.F.);
#21580=ORIENTED_EDGE('',*,*,#16041,.T.);
#21581=ORIENTED_EDGE('',*,*,#16039,.F.);
#21582=ORIENTED_EDGE('',*,*,#16041,.F.);
#21583=ORIENTED_EDGE('',*,*,#15928,.T.);
#21584=ORIENTED_EDGE('',*,*,#16042,.T.);
#21585=ORIENTED_EDGE('',*,*,#16043,.T.);
#21586=ORIENTED_EDGE('',*,*,#16042,.F.);
#21587=ORIENTED_EDGE('',*,*,#16044,.F.);
#21588=ORIENTED_EDGE('',*,*,#16045,.T.);
#21589=ORIENTED_EDGE('',*,*,#16043,.F.);
#21590=ORIENTED_EDGE('',*,*,#16045,.F.);
#21591=ORIENTED_EDGE('',*,*,#15920,.T.);
#21592=ORIENTED_EDGE('',*,*,#16046,.T.);
#21593=ORIENTED_EDGE('',*,*,#16047,.T.);
#21594=ORIENTED_EDGE('',*,*,#16046,.F.);
#21595=ORIENTED_EDGE('',*,*,#16048,.F.);
#21596=ORIENTED_EDGE('',*,*,#16049,.T.);
#21597=ORIENTED_EDGE('',*,*,#16047,.F.);
#21598=ORIENTED_EDGE('',*,*,#16049,.F.);
#21599=ORIENTED_EDGE('',*,*,#15927,.T.);
#21600=ORIENTED_EDGE('',*,*,#16050,.T.);
#21601=ORIENTED_EDGE('',*,*,#16051,.T.);
#21602=ORIENTED_EDGE('',*,*,#16050,.F.);
#21603=ORIENTED_EDGE('',*,*,#16052,.F.);
#21604=ORIENTED_EDGE('',*,*,#16053,.T.);
#21605=ORIENTED_EDGE('',*,*,#16051,.F.);
#21606=ORIENTED_EDGE('',*,*,#16053,.F.);
#21607=ORIENTED_EDGE('',*,*,#15921,.T.);
#21608=ORIENTED_EDGE('',*,*,#16054,.T.);
#21609=ORIENTED_EDGE('',*,*,#16055,.T.);
#21610=ORIENTED_EDGE('',*,*,#16054,.F.);
#21611=ORIENTED_EDGE('',*,*,#16056,.F.);
#21612=ORIENTED_EDGE('',*,*,#16057,.T.);
#21613=ORIENTED_EDGE('',*,*,#16055,.F.);
#21614=ORIENTED_EDGE('',*,*,#16057,.F.);
#21615=ORIENTED_EDGE('',*,*,#15926,.T.);
#21616=ORIENTED_EDGE('',*,*,#16058,.T.);
#21617=ORIENTED_EDGE('',*,*,#16059,.T.);
#21618=ORIENTED_EDGE('',*,*,#16058,.F.);
#21619=ORIENTED_EDGE('',*,*,#16060,.F.);
#21620=ORIENTED_EDGE('',*,*,#16061,.T.);
#21621=ORIENTED_EDGE('',*,*,#16059,.F.);
#21622=ORIENTED_EDGE('',*,*,#16061,.F.);
#21623=ORIENTED_EDGE('',*,*,#15922,.T.);
#21624=ORIENTED_EDGE('',*,*,#16062,.T.);
#21625=ORIENTED_EDGE('',*,*,#16063,.T.);
#21626=ORIENTED_EDGE('',*,*,#16062,.F.);
#21627=ORIENTED_EDGE('',*,*,#16064,.F.);
#21628=ORIENTED_EDGE('',*,*,#16065,.T.);
#21629=ORIENTED_EDGE('',*,*,#16063,.F.);
#21630=ORIENTED_EDGE('',*,*,#16065,.F.);
#21631=ORIENTED_EDGE('',*,*,#15925,.T.);
#21632=ORIENTED_EDGE('',*,*,#16066,.T.);
#21633=ORIENTED_EDGE('',*,*,#16067,.T.);
#21634=ORIENTED_EDGE('',*,*,#16066,.F.);
#21635=ORIENTED_EDGE('',*,*,#16068,.F.);
#21636=ORIENTED_EDGE('',*,*,#16069,.T.);
#21637=ORIENTED_EDGE('',*,*,#16067,.F.);
#21638=ORIENTED_EDGE('',*,*,#16069,.F.);
#21639=ORIENTED_EDGE('',*,*,#15923,.T.);
#21640=ORIENTED_EDGE('',*,*,#16070,.T.);
#21641=ORIENTED_EDGE('',*,*,#16071,.T.);
#21642=ORIENTED_EDGE('',*,*,#16070,.F.);
#21643=ORIENTED_EDGE('',*,*,#16072,.F.);
#21644=ORIENTED_EDGE('',*,*,#16073,.T.);
#21645=ORIENTED_EDGE('',*,*,#16071,.F.);
#21646=ORIENTED_EDGE('',*,*,#16073,.F.);
#21647=ORIENTED_EDGE('',*,*,#15835,.F.);
#21648=ORIENTED_EDGE('',*,*,#15845,.F.);
#21649=ORIENTED_EDGE('',*,*,#16074,.T.);
#21650=ORIENTED_EDGE('',*,*,#15877,.T.);
#21651=ORIENTED_EDGE('',*,*,#15869,.F.);
#21652=ORIENTED_EDGE('',*,*,#16075,.T.);
#21653=ORIENTED_EDGE('',*,*,#15883,.F.);
#21654=ORIENTED_EDGE('',*,*,#15963,.T.);
#21655=ORIENTED_EDGE('',*,*,#15884,.F.);
#21656=ORIENTED_EDGE('',*,*,#15879,.F.);
#21657=ORIENTED_EDGE('',*,*,#16076,.T.);
#21658=ORIENTED_EDGE('',*,*,#15843,.T.);
#21659=ORIENTED_EDGE('',*,*,#15844,.F.);
#21660=ORIENTED_EDGE('',*,*,#16076,.F.);
#21661=ORIENTED_EDGE('',*,*,#15878,.F.);
#21662=ORIENTED_EDGE('',*,*,#16074,.F.);
#21663=ORIENTED_EDGE('',*,*,#16077,.F.);
#21664=ORIENTED_EDGE('',*,*,#16078,.F.);
#21665=ORIENTED_EDGE('',*,*,#16079,.F.);
#21666=ORIENTED_EDGE('',*,*,#16080,.F.);
#21667=ORIENTED_EDGE('',*,*,#16081,.F.);
#21668=ORIENTED_EDGE('',*,*,#16082,.F.);
#21669=ORIENTED_EDGE('',*,*,#16083,.F.);
#21670=ORIENTED_EDGE('',*,*,#16084,.F.);
#21671=ORIENTED_EDGE('',*,*,#16085,.F.);
#21672=ORIENTED_EDGE('',*,*,#16086,.F.);
#21673=ORIENTED_EDGE('',*,*,#16087,.F.);
#21674=ORIENTED_EDGE('',*,*,#16088,.F.);
#21675=ORIENTED_EDGE('',*,*,#16089,.F.);
#21676=ORIENTED_EDGE('',*,*,#16090,.F.);
#21677=ORIENTED_EDGE('',*,*,#16091,.F.);
#21678=ORIENTED_EDGE('',*,*,#16092,.F.);
#21679=ORIENTED_EDGE('',*,*,#16093,.F.);
#21680=ORIENTED_EDGE('',*,*,#16094,.F.);
#21681=ORIENTED_EDGE('',*,*,#16095,.F.);
#21682=ORIENTED_EDGE('',*,*,#16096,.F.);
#21683=ORIENTED_EDGE('',*,*,#16097,.F.);
#21684=ORIENTED_EDGE('',*,*,#16098,.F.);
#21685=ORIENTED_EDGE('',*,*,#16099,.F.);
#21686=ORIENTED_EDGE('',*,*,#16100,.F.);
#21687=ORIENTED_EDGE('',*,*,#16101,.F.);
#21688=ORIENTED_EDGE('',*,*,#16102,.F.);
#21689=ORIENTED_EDGE('',*,*,#16103,.F.);
#21690=ORIENTED_EDGE('',*,*,#16104,.F.);
#21691=ORIENTED_EDGE('',*,*,#16105,.F.);
#21692=ORIENTED_EDGE('',*,*,#16106,.F.);
#21693=ORIENTED_EDGE('',*,*,#16107,.F.);
#21694=ORIENTED_EDGE('',*,*,#16108,.F.);
#21695=ORIENTED_EDGE('',*,*,#16109,.F.);
#21696=ORIENTED_EDGE('',*,*,#16110,.F.);
#21697=ORIENTED_EDGE('',*,*,#16111,.F.);
#21698=ORIENTED_EDGE('',*,*,#16112,.F.);
#21699=ORIENTED_EDGE('',*,*,#16113,.F.);
#21700=ORIENTED_EDGE('',*,*,#16114,.F.);
#21701=ORIENTED_EDGE('',*,*,#16115,.F.);
#21702=ORIENTED_EDGE('',*,*,#16116,.F.);
#21703=ORIENTED_EDGE('',*,*,#16117,.F.);
#21704=ORIENTED_EDGE('',*,*,#16118,.F.);
#21705=ORIENTED_EDGE('',*,*,#16077,.T.);
#21706=ORIENTED_EDGE('',*,*,#16119,.T.);
#21707=ORIENTED_EDGE('',*,*,#15832,.T.);
#21708=ORIENTED_EDGE('',*,*,#16119,.F.);
#21709=ORIENTED_EDGE('',*,*,#16118,.T.);
#21710=ORIENTED_EDGE('',*,*,#16120,.T.);
#21711=ORIENTED_EDGE('',*,*,#16072,.T.);
#21712=ORIENTED_EDGE('',*,*,#16120,.F.);
#21713=ORIENTED_EDGE('',*,*,#16078,.T.);
#21714=ORIENTED_EDGE('',*,*,#16121,.T.);
#21715=ORIENTED_EDGE('',*,*,#16068,.T.);
#21716=ORIENTED_EDGE('',*,*,#16121,.F.);
#21717=ORIENTED_EDGE('',*,*,#16117,.T.);
#21718=ORIENTED_EDGE('',*,*,#16122,.T.);
#21719=ORIENTED_EDGE('',*,*,#16064,.T.);
#21720=ORIENTED_EDGE('',*,*,#16122,.F.);
#21721=ORIENTED_EDGE('',*,*,#16079,.T.);
#21722=ORIENTED_EDGE('',*,*,#16123,.T.);
#21723=ORIENTED_EDGE('',*,*,#16060,.T.);
#21724=ORIENTED_EDGE('',*,*,#16123,.F.);
#21725=ORIENTED_EDGE('',*,*,#16116,.T.);
#21726=ORIENTED_EDGE('',*,*,#16124,.T.);
#21727=ORIENTED_EDGE('',*,*,#16056,.T.);
#21728=ORIENTED_EDGE('',*,*,#16124,.F.);
#21729=ORIENTED_EDGE('',*,*,#16080,.T.);
#21730=ORIENTED_EDGE('',*,*,#16125,.T.);
#21731=ORIENTED_EDGE('',*,*,#16052,.T.);
#21732=ORIENTED_EDGE('',*,*,#16125,.F.);
#21733=ORIENTED_EDGE('',*,*,#16115,.T.);
#21734=ORIENTED_EDGE('',*,*,#16126,.T.);
#21735=ORIENTED_EDGE('',*,*,#16048,.T.);
#21736=ORIENTED_EDGE('',*,*,#16126,.F.);
#21737=ORIENTED_EDGE('',*,*,#16081,.T.);
#21738=ORIENTED_EDGE('',*,*,#16127,.T.);
#21739=ORIENTED_EDGE('',*,*,#16128,.T.);
#21740=ORIENTED_EDGE('',*,*,#16127,.F.);
#21741=ORIENTED_EDGE('',*,*,#16128,.F.);
#21742=ORIENTED_EDGE('',*,*,#16129,.T.);
#21743=ORIENTED_EDGE('',*,*,#15892,.T.);
#21744=ORIENTED_EDGE('',*,*,#16129,.F.);
#21745=ORIENTED_EDGE('',*,*,#16114,.T.);
#21746=ORIENTED_EDGE('',*,*,#16130,.T.);
#21747=ORIENTED_EDGE('',*,*,#16131,.T.);
#21748=ORIENTED_EDGE('',*,*,#16130,.F.);
#21749=ORIENTED_EDGE('',*,*,#16131,.F.);
#21750=ORIENTED_EDGE('',*,*,#16132,.T.);
#21751=ORIENTED_EDGE('',*,*,#15898,.T.);
#21752=ORIENTED_EDGE('',*,*,#16132,.F.);
#21753=ORIENTED_EDGE('',*,*,#16082,.T.);
#21754=ORIENTED_EDGE('',*,*,#16133,.T.);
#21755=ORIENTED_EDGE('',*,*,#16134,.T.);
#21756=ORIENTED_EDGE('',*,*,#16133,.F.);
#21757=ORIENTED_EDGE('',*,*,#16134,.F.);
#21758=ORIENTED_EDGE('',*,*,#16135,.T.);
#21759=ORIENTED_EDGE('',*,*,#15822,.T.);
#21760=ORIENTED_EDGE('',*,*,#16135,.F.);
#21761=ORIENTED_EDGE('',*,*,#16113,.T.);
#21762=ORIENTED_EDGE('',*,*,#16136,.T.);
#21763=ORIENTED_EDGE('',*,*,#16137,.T.);
#21764=ORIENTED_EDGE('',*,*,#16136,.F.);
#21765=ORIENTED_EDGE('',*,*,#16137,.F.);
#21766=ORIENTED_EDGE('',*,*,#16138,.T.);
#21767=ORIENTED_EDGE('',*,*,#15816,.T.);
#21768=ORIENTED_EDGE('',*,*,#16138,.F.);
#21769=ORIENTED_EDGE('',*,*,#16083,.T.);
#21770=ORIENTED_EDGE('',*,*,#16139,.T.);
#21771=ORIENTED_EDGE('',*,*,#16140,.T.);
#21772=ORIENTED_EDGE('',*,*,#16139,.F.);
#21773=ORIENTED_EDGE('',*,*,#16140,.F.);
#21774=ORIENTED_EDGE('',*,*,#16141,.T.);
#21775=ORIENTED_EDGE('',*,*,#15810,.T.);
#21776=ORIENTED_EDGE('',*,*,#16141,.F.);
#21777=ORIENTED_EDGE('',*,*,#16112,.T.);
#21778=ORIENTED_EDGE('',*,*,#16142,.T.);
#21779=ORIENTED_EDGE('',*,*,#16143,.T.);
#21780=ORIENTED_EDGE('',*,*,#16142,.F.);
#21781=ORIENTED_EDGE('',*,*,#16143,.F.);
#21782=ORIENTED_EDGE('',*,*,#16144,.T.);
#21783=ORIENTED_EDGE('',*,*,#15804,.T.);
#21784=ORIENTED_EDGE('',*,*,#16144,.F.);
#21785=ORIENTED_EDGE('',*,*,#16084,.T.);
#21786=ORIENTED_EDGE('',*,*,#16145,.T.);
#21787=ORIENTED_EDGE('',*,*,#16146,.T.);
#21788=ORIENTED_EDGE('',*,*,#16145,.F.);
#21789=ORIENTED_EDGE('',*,*,#16146,.F.);
#21790=ORIENTED_EDGE('',*,*,#16147,.T.);
#21791=ORIENTED_EDGE('',*,*,#15798,.T.);
#21792=ORIENTED_EDGE('',*,*,#16147,.F.);
#21793=ORIENTED_EDGE('',*,*,#16111,.T.);
#21794=ORIENTED_EDGE('',*,*,#16148,.T.);
#21795=ORIENTED_EDGE('',*,*,#16149,.T.);
#21796=ORIENTED_EDGE('',*,*,#16148,.F.);
#21797=ORIENTED_EDGE('',*,*,#16149,.F.);
#21798=ORIENTED_EDGE('',*,*,#16150,.T.);
#21799=ORIENTED_EDGE('',*,*,#15792,.T.);
#21800=ORIENTED_EDGE('',*,*,#16150,.F.);
#21801=ORIENTED_EDGE('',*,*,#16085,.T.);
#21802=ORIENTED_EDGE('',*,*,#16151,.T.);
#21803=ORIENTED_EDGE('',*,*,#16152,.T.);
#21804=ORIENTED_EDGE('',*,*,#16151,.F.);
#21805=ORIENTED_EDGE('',*,*,#16152,.F.);
#21806=ORIENTED_EDGE('',*,*,#16153,.T.);
#21807=ORIENTED_EDGE('',*,*,#15786,.T.);
#21808=ORIENTED_EDGE('',*,*,#16153,.F.);
#21809=ORIENTED_EDGE('',*,*,#16110,.T.);
#21810=ORIENTED_EDGE('',*,*,#16154,.T.);
#21811=ORIENTED_EDGE('',*,*,#16155,.T.);
#21812=ORIENTED_EDGE('',*,*,#16154,.F.);
#21813=ORIENTED_EDGE('',*,*,#16155,.F.);
#21814=ORIENTED_EDGE('',*,*,#16156,.T.);
#21815=ORIENTED_EDGE('',*,*,#15828,.T.);
#21816=ORIENTED_EDGE('',*,*,#16156,.F.);
#21817=ORIENTED_EDGE('',*,*,#16086,.T.);
#21818=ORIENTED_EDGE('',*,*,#16157,.T.);
#21819=ORIENTED_EDGE('',*,*,#16044,.T.);
#21820=ORIENTED_EDGE('',*,*,#16157,.F.);
#21821=ORIENTED_EDGE('',*,*,#16109,.T.);
#21822=ORIENTED_EDGE('',*,*,#16158,.T.);
#21823=ORIENTED_EDGE('',*,*,#16040,.T.);
#21824=ORIENTED_EDGE('',*,*,#16158,.F.);
#21825=ORIENTED_EDGE('',*,*,#16087,.T.);
#21826=ORIENTED_EDGE('',*,*,#16159,.T.);
#21827=ORIENTED_EDGE('',*,*,#16036,.T.);
#21828=ORIENTED_EDGE('',*,*,#16159,.F.);
#21829=ORIENTED_EDGE('',*,*,#16108,.T.);
#21830=ORIENTED_EDGE('',*,*,#16160,.T.);
#21831=ORIENTED_EDGE('',*,*,#16032,.T.);
#21832=ORIENTED_EDGE('',*,*,#16160,.F.);
#21833=ORIENTED_EDGE('',*,*,#16088,.T.);
#21834=ORIENTED_EDGE('',*,*,#16161,.T.);
#21835=ORIENTED_EDGE('',*,*,#16028,.T.);
#21836=ORIENTED_EDGE('',*,*,#16161,.F.);
#21837=ORIENTED_EDGE('',*,*,#16107,.T.);
#21838=ORIENTED_EDGE('',*,*,#16162,.T.);
#21839=ORIENTED_EDGE('',*,*,#16024,.T.);
#21840=ORIENTED_EDGE('',*,*,#16162,.F.);
#21841=ORIENTED_EDGE('',*,*,#16089,.T.);
#21842=ORIENTED_EDGE('',*,*,#16163,.T.);
#21843=ORIENTED_EDGE('',*,*,#16020,.T.);
#21844=ORIENTED_EDGE('',*,*,#16163,.F.);
#21845=ORIENTED_EDGE('',*,*,#16106,.T.);
#21846=ORIENTED_EDGE('',*,*,#16164,.T.);
#21847=ORIENTED_EDGE('',*,*,#16016,.T.);
#21848=ORIENTED_EDGE('',*,*,#16164,.F.);
#21849=ORIENTED_EDGE('',*,*,#16090,.T.);
#21850=ORIENTED_EDGE('',*,*,#16165,.T.);
#21851=ORIENTED_EDGE('',*,*,#15966,.T.);
#21852=ORIENTED_EDGE('',*,*,#16165,.F.);
#21853=ORIENTED_EDGE('',*,*,#16105,.T.);
#21854=ORIENTED_EDGE('',*,*,#16166,.T.);
#21855=ORIENTED_EDGE('',*,*,#15970,.T.);
#21856=ORIENTED_EDGE('',*,*,#16166,.F.);
#21857=ORIENTED_EDGE('',*,*,#16091,.T.);
#21858=ORIENTED_EDGE('',*,*,#16167,.T.);
#21859=ORIENTED_EDGE('',*,*,#15974,.T.);
#21860=ORIENTED_EDGE('',*,*,#16167,.F.);
#21861=ORIENTED_EDGE('',*,*,#16104,.T.);
#21862=ORIENTED_EDGE('',*,*,#16168,.T.);
#21863=ORIENTED_EDGE('',*,*,#15978,.T.);
#21864=ORIENTED_EDGE('',*,*,#16168,.F.);
#21865=ORIENTED_EDGE('',*,*,#16092,.T.);
#21866=ORIENTED_EDGE('',*,*,#16169,.T.);
#21867=ORIENTED_EDGE('',*,*,#15982,.T.);
#21868=ORIENTED_EDGE('',*,*,#16169,.F.);
#21869=ORIENTED_EDGE('',*,*,#16103,.T.);
#21870=ORIENTED_EDGE('',*,*,#16170,.T.);
#21871=ORIENTED_EDGE('',*,*,#15986,.T.);
#21872=ORIENTED_EDGE('',*,*,#16170,.F.);
#21873=ORIENTED_EDGE('',*,*,#16093,.T.);
#21874=ORIENTED_EDGE('',*,*,#16171,.T.);
#21875=ORIENTED_EDGE('',*,*,#15990,.T.);
#21876=ORIENTED_EDGE('',*,*,#16171,.F.);
#21877=ORIENTED_EDGE('',*,*,#16102,.T.);
#21878=ORIENTED_EDGE('',*,*,#16172,.T.);
#21879=ORIENTED_EDGE('',*,*,#15994,.T.);
#21880=ORIENTED_EDGE('',*,*,#16172,.F.);
#21881=ORIENTED_EDGE('',*,*,#16094,.T.);
#21882=ORIENTED_EDGE('',*,*,#16173,.T.);
#21883=ORIENTED_EDGE('',*,*,#15998,.T.);
#21884=ORIENTED_EDGE('',*,*,#16173,.F.);
#21885=ORIENTED_EDGE('',*,*,#16101,.T.);
#21886=ORIENTED_EDGE('',*,*,#16174,.T.);
#21887=ORIENTED_EDGE('',*,*,#16002,.T.);
#21888=ORIENTED_EDGE('',*,*,#16174,.F.);
#21889=ORIENTED_EDGE('',*,*,#16095,.T.);
#21890=ORIENTED_EDGE('',*,*,#16175,.T.);
#21891=ORIENTED_EDGE('',*,*,#16006,.T.);
#21892=ORIENTED_EDGE('',*,*,#16175,.F.);
#21893=ORIENTED_EDGE('',*,*,#16100,.T.);
#21894=ORIENTED_EDGE('',*,*,#16176,.T.);
#21895=ORIENTED_EDGE('',*,*,#16010,.T.);
#21896=ORIENTED_EDGE('',*,*,#16176,.F.);
#21897=ORIENTED_EDGE('',*,*,#16096,.T.);
#21898=ORIENTED_EDGE('',*,*,#16177,.T.);
#21899=ORIENTED_EDGE('',*,*,#15953,.T.);
#21900=ORIENTED_EDGE('',*,*,#16177,.F.);
#21901=ORIENTED_EDGE('',*,*,#16099,.T.);
#21902=ORIENTED_EDGE('',*,*,#16178,.T.);
#21903=ORIENTED_EDGE('',*,*,#15957,.T.);
#21904=ORIENTED_EDGE('',*,*,#16178,.F.);
#21905=ORIENTED_EDGE('',*,*,#16097,.T.);
#21906=ORIENTED_EDGE('',*,*,#16179,.T.);
#21907=ORIENTED_EDGE('',*,*,#16180,.T.);
#21908=ORIENTED_EDGE('',*,*,#16179,.F.);
#21909=ORIENTED_EDGE('',*,*,#16180,.F.);
#21910=ORIENTED_EDGE('',*,*,#16181,.T.);
#21911=ORIENTED_EDGE('',*,*,#15863,.T.);
#21912=ORIENTED_EDGE('',*,*,#16181,.F.);
#21913=ORIENTED_EDGE('',*,*,#16098,.T.);
#21914=ORIENTED_EDGE('',*,*,#16182,.T.);
#21915=ORIENTED_EDGE('',*,*,#16183,.T.);
#21916=ORIENTED_EDGE('',*,*,#16182,.F.);
#21917=ORIENTED_EDGE('',*,*,#16183,.F.);
#21918=ORIENTED_EDGE('',*,*,#16184,.T.);
#21919=ORIENTED_EDGE('',*,*,#15857,.T.);
#21920=ORIENTED_EDGE('',*,*,#16184,.F.);
#21921=ORIENTED_EDGE('',*,*,#15924,.F.);
#21922=ORIENTED_EDGE('',*,*,#16185,.T.);
#21923=ORIENTED_EDGE('',*,*,#15834,.T.);
#21924=ORIENTED_EDGE('',*,*,#16185,.F.);
#21925=ORIENTED_EDGE('',*,*,#15836,.F.);
#21926=ORIENTED_EDGE('',*,*,#16075,.F.);
#21927=ORIENTED_EDGE('',*,*,#15868,.F.);
#21928=ORIENTED_EDGE('',*,*,#15962,.F.);
#21929=ORIENTED_EDGE('',*,*,#16186,.T.);
#21930=ORIENTED_EDGE('',*,*,#16187,.T.);
#21931=ORIENTED_EDGE('',*,*,#16188,.T.);
#21932=ORIENTED_EDGE('',*,*,#16189,.T.);
#21933=ORIENTED_EDGE('',*,*,#16188,.F.);
#21934=ORIENTED_EDGE('',*,*,#16190,.T.);
#21935=ORIENTED_EDGE('',*,*,#16186,.F.);
#21936=ORIENTED_EDGE('',*,*,#16191,.T.);
#21937=ORIENTED_EDGE('',*,*,#16192,.T.);
#21938=ORIENTED_EDGE('',*,*,#16193,.T.);
#21939=ORIENTED_EDGE('',*,*,#16192,.F.);
#21940=ORIENTED_EDGE('',*,*,#16194,.T.);
#21941=ORIENTED_EDGE('',*,*,#16195,.T.);
#21942=ORIENTED_EDGE('',*,*,#16196,.T.);
#21943=ORIENTED_EDGE('',*,*,#16189,.F.);
#21944=ORIENTED_EDGE('',*,*,#16197,.T.);
#21945=ORIENTED_EDGE('',*,*,#16198,.T.);
#21946=ORIENTED_EDGE('',*,*,#16197,.F.);
#21947=ORIENTED_EDGE('',*,*,#16195,.F.);
#21948=ORIENTED_EDGE('',*,*,#16199,.T.);
#21949=ORIENTED_EDGE('',*,*,#16200,.T.);
#21950=ORIENTED_EDGE('',*,*,#16201,.T.);
#21951=ORIENTED_EDGE('',*,*,#16202,.F.);
#21952=ORIENTED_EDGE('',*,*,#16203,.T.);
#21953=ORIENTED_EDGE('',*,*,#16204,.T.);
#21954=ORIENTED_EDGE('',*,*,#16193,.F.);
#21955=ORIENTED_EDGE('',*,*,#16205,.T.);
#21956=ORIENTED_EDGE('',*,*,#16206,.T.);
#21957=ORIENTED_EDGE('',*,*,#16205,.F.);
#21958=ORIENTED_EDGE('',*,*,#16207,.F.);
#21959=ORIENTED_EDGE('',*,*,#16208,.F.);
#21960=ORIENTED_EDGE('',*,*,#16200,.F.);
#21961=ORIENTED_EDGE('',*,*,#16209,.F.);
#21962=ORIENTED_EDGE('',*,*,#16210,.F.);
#21963=ORIENTED_EDGE('',*,*,#16211,.F.);
#21964=ORIENTED_EDGE('',*,*,#16208,.T.);
#21965=ORIENTED_EDGE('',*,*,#16212,.T.);
#21966=ORIENTED_EDGE('',*,*,#16210,.T.);
#21967=ORIENTED_EDGE('',*,*,#16213,.T.);
#21968=ORIENTED_EDGE('',*,*,#16214,.T.);
#21969=ORIENTED_EDGE('',*,*,#16215,.T.);
#21970=ORIENTED_EDGE('',*,*,#16211,.T.);
#21971=ORIENTED_EDGE('',*,*,#16216,.T.);
#21972=ORIENTED_EDGE('',*,*,#16217,.T.);
#21973=ORIENTED_EDGE('',*,*,#16218,.F.);
#21974=ORIENTED_EDGE('',*,*,#16219,.F.);
#21975=ORIENTED_EDGE('',*,*,#16220,.F.);
#21976=ORIENTED_EDGE('',*,*,#16202,.T.);
#21977=ORIENTED_EDGE('',*,*,#16221,.T.);
#21978=ORIENTED_EDGE('',*,*,#16219,.T.);
#21979=ORIENTED_EDGE('',*,*,#16222,.T.);
#21980=ORIENTED_EDGE('',*,*,#16223,.T.);
#21981=ORIENTED_EDGE('',*,*,#16209,.T.);
#21982=ORIENTED_EDGE('',*,*,#16224,.T.);
#21983=ORIENTED_EDGE('',*,*,#16220,.T.);
#21984=ORIENTED_EDGE('',*,*,#16225,.T.);
#21985=ORIENTED_EDGE('',*,*,#16226,.T.);
#21986=ORIENTED_EDGE('',*,*,#16227,.T.);
#21987=ORIENTED_EDGE('',*,*,#16218,.T.);
#21988=ORIENTED_EDGE('',*,*,#16228,.T.);
#21989=ORIENTED_EDGE('',*,*,#16229,.T.);
#21990=ORIENTED_EDGE('',*,*,#16230,.T.);
#21991=ORIENTED_EDGE('',*,*,#16231,.T.);
#21992=ORIENTED_EDGE('',*,*,#16207,.T.);
#21993=ORIENTED_EDGE('',*,*,#16232,.T.);
#21994=ORIENTED_EDGE('',*,*,#16233,.T.);
#21995=ORIENTED_EDGE('',*,*,#16228,.F.);
#21996=ORIENTED_EDGE('',*,*,#16224,.F.);
#21997=ORIENTED_EDGE('',*,*,#16215,.F.);
#21998=ORIENTED_EDGE('',*,*,#16234,.F.);
#21999=ORIENTED_EDGE('',*,*,#16235,.T.);
#22000=ORIENTED_EDGE('',*,*,#16236,.T.);
#22001=ORIENTED_EDGE('',*,*,#16216,.F.);
#22002=ORIENTED_EDGE('',*,*,#16212,.F.);
#22003=ORIENTED_EDGE('',*,*,#16231,.F.);
#22004=ORIENTED_EDGE('',*,*,#16237,.F.);
#22005=ORIENTED_EDGE('',*,*,#16238,.T.);
#22006=ORIENTED_EDGE('',*,*,#16239,.T.);
#22007=ORIENTED_EDGE('',*,*,#16217,.F.);
#22008=ORIENTED_EDGE('',*,*,#16237,.T.);
#22009=ORIENTED_EDGE('',*,*,#16230,.F.);
#22010=ORIENTED_EDGE('',*,*,#16240,.F.);
#22011=ORIENTED_EDGE('',*,*,#16241,.T.);
#22012=ORIENTED_EDGE('',*,*,#16242,.T.);
#22013=ORIENTED_EDGE('',*,*,#16233,.F.);
#22014=ORIENTED_EDGE('',*,*,#16243,.T.);
#22015=ORIENTED_EDGE('',*,*,#16244,.T.);
#22016=ORIENTED_EDGE('',*,*,#16245,.T.);
#22017=ORIENTED_EDGE('',*,*,#16240,.T.);
#22018=ORIENTED_EDGE('',*,*,#16201,.F.);
#22019=ORIENTED_EDGE('',*,*,#16213,.F.);
#22020=ORIENTED_EDGE('',*,*,#16225,.F.);
#22021=ORIENTED_EDGE('',*,*,#16221,.F.);
#22022=ORIENTED_EDGE('',*,*,#16244,.F.);
#22023=ORIENTED_EDGE('',*,*,#16246,.F.);
#22024=ORIENTED_EDGE('',*,*,#16247,.F.);
#22025=ORIENTED_EDGE('',*,*,#16223,.F.);
#22026=ORIENTED_EDGE('',*,*,#16248,.T.);
#22027=ORIENTED_EDGE('',*,*,#16246,.T.);
#22028=ORIENTED_EDGE('',*,*,#16249,.T.);
#22029=ORIENTED_EDGE('',*,*,#16203,.F.);
#22030=ORIENTED_EDGE('',*,*,#16229,.F.);
#22031=ORIENTED_EDGE('',*,*,#16234,.T.);
#22032=ORIENTED_EDGE('',*,*,#16214,.F.);
#22033=ORIENTED_EDGE('',*,*,#16242,.F.);
#22034=ORIENTED_EDGE('',*,*,#16250,.T.);
#22035=ORIENTED_EDGE('',*,*,#16251,.T.);
#22036=ORIENTED_EDGE('',*,*,#16226,.F.);
#22037=ORIENTED_EDGE('',*,*,#16251,.F.);
#22038=ORIENTED_EDGE('',*,*,#16252,.T.);
#22039=ORIENTED_EDGE('',*,*,#16247,.T.);
#22040=ORIENTED_EDGE('',*,*,#16253,.T.);
#22041=ORIENTED_EDGE('',*,*,#16227,.F.);
#22042=ORIENTED_EDGE('',*,*,#16253,.F.);
#22043=ORIENTED_EDGE('',*,*,#16248,.F.);
#22044=ORIENTED_EDGE('',*,*,#16222,.F.);
#22045=ORIENTED_EDGE('',*,*,#16254,.T.);
#22046=ORIENTED_EDGE('',*,*,#16245,.F.);
#22047=ORIENTED_EDGE('',*,*,#16252,.F.);
#22048=ORIENTED_EDGE('',*,*,#16250,.F.);
#22049=ORIENTED_EDGE('',*,*,#16241,.F.);
#22050=ORIENTED_EDGE('',*,*,#16255,.T.);
#22051=ORIENTED_EDGE('',*,*,#16206,.F.);
#22052=ORIENTED_EDGE('',*,*,#16256,.F.);
#22053=ORIENTED_EDGE('',*,*,#16198,.F.);
#22054=ORIENTED_EDGE('',*,*,#16257,.F.);
#22055=ORIENTED_EDGE('',*,*,#16256,.T.);
#22056=ORIENTED_EDGE('',*,*,#16258,.T.);
#22057=ORIENTED_EDGE('',*,*,#16236,.F.);
#22058=ORIENTED_EDGE('',*,*,#16258,.F.);
#22059=ORIENTED_EDGE('',*,*,#16257,.T.);
#22060=ORIENTED_EDGE('',*,*,#16259,.T.);
#22061=ORIENTED_EDGE('',*,*,#16235,.F.);
#22062=ORIENTED_EDGE('',*,*,#16259,.F.);
#22063=ORIENTED_EDGE('',*,*,#16255,.F.);
#22064=ORIENTED_EDGE('',*,*,#16260,.T.);
#22065=ORIENTED_EDGE('',*,*,#16261,.F.);
#22066=ORIENTED_EDGE('',*,*,#16262,.F.);
#22067=ORIENTED_EDGE('',*,*,#16263,.F.);
#22068=ORIENTED_EDGE('',*,*,#16260,.F.);
#22069=ORIENTED_EDGE('',*,*,#16264,.F.);
#22070=ORIENTED_EDGE('',*,*,#16265,.F.);
#22071=ORIENTED_EDGE('',*,*,#16266,.T.);
#22072=ORIENTED_EDGE('',*,*,#16267,.T.);
#22073=ORIENTED_EDGE('',*,*,#16266,.F.);
#22074=ORIENTED_EDGE('',*,*,#16267,.F.);
#22075=ORIENTED_EDGE('',*,*,#16239,.F.);
#22076=ORIENTED_EDGE('',*,*,#16268,.T.);
#22077=ORIENTED_EDGE('',*,*,#16263,.T.);
#22078=ORIENTED_EDGE('',*,*,#16269,.T.);
#22079=ORIENTED_EDGE('',*,*,#16270,.T.);
#22080=ORIENTED_EDGE('',*,*,#16269,.F.);
#22081=ORIENTED_EDGE('',*,*,#16262,.T.);
#22082=ORIENTED_EDGE('',*,*,#16261,.T.);
#22083=ORIENTED_EDGE('',*,*,#16268,.F.);
#22084=ORIENTED_EDGE('',*,*,#16264,.T.);
#22085=ORIENTED_EDGE('',*,*,#16265,.T.);
#22086=ORIENTED_EDGE('',*,*,#16270,.F.);
#22087=ORIENTED_EDGE('',*,*,#16254,.F.);
#22088=ORIENTED_EDGE('',*,*,#16271,.T.);
#22089=ORIENTED_EDGE('',*,*,#16238,.F.);
#22090=ORIENTED_EDGE('',*,*,#16271,.F.);
#22091=ORIENTED_EDGE('',*,*,#16187,.F.);
#22092=ORIENTED_EDGE('',*,*,#16196,.F.);
#22093=ORIENTED_EDGE('',*,*,#16204,.F.);
#22094=ORIENTED_EDGE('',*,*,#16249,.F.);
#22095=ORIENTED_EDGE('',*,*,#16243,.F.);
#22096=ORIENTED_EDGE('',*,*,#16232,.F.);
#22097=ORIENTED_EDGE('',*,*,#16199,.F.);
#22098=ORIENTED_EDGE('',*,*,#16194,.F.);
#22099=ORIENTED_EDGE('',*,*,#16191,.F.);
#22100=ORIENTED_EDGE('',*,*,#16190,.F.);
#22101=ORIENTED_EDGE('',*,*,#16272,.F.);
#22102=ORIENTED_EDGE('',*,*,#16273,.F.);
#22103=ORIENTED_EDGE('',*,*,#16274,.F.);
#22104=ORIENTED_EDGE('',*,*,#16275,.T.);
#22105=ORIENTED_EDGE('',*,*,#16276,.F.);
#22106=ORIENTED_EDGE('',*,*,#16277,.F.);
#22107=ORIENTED_EDGE('',*,*,#16275,.F.);
#22108=ORIENTED_EDGE('',*,*,#16278,.F.);
#22109=ORIENTED_EDGE('',*,*,#16279,.F.);
#22110=ORIENTED_EDGE('',*,*,#16278,.T.);
#22111=ORIENTED_EDGE('',*,*,#16274,.T.);
#22112=ORIENTED_EDGE('',*,*,#16280,.F.);
#22113=ORIENTED_EDGE('',*,*,#16281,.T.);
#22114=ORIENTED_EDGE('',*,*,#16280,.T.);
#22115=ORIENTED_EDGE('',*,*,#16281,.F.);
#22116=ORIENTED_EDGE('',*,*,#16276,.T.);
#22117=ORIENTED_EDGE('',*,*,#16277,.T.);
#22118=ORIENTED_EDGE('',*,*,#16279,.T.);
#22119=ORIENTED_EDGE('',*,*,#16282,.T.);
#22120=ORIENTED_EDGE('',*,*,#16283,.F.);
#22121=ORIENTED_EDGE('',*,*,#16284,.F.);
#22122=ORIENTED_EDGE('',*,*,#16285,.F.);
#22123=ORIENTED_EDGE('',*,*,#16286,.F.);
#22124=ORIENTED_EDGE('',*,*,#16287,.T.);
#22125=ORIENTED_EDGE('',*,*,#16288,.F.);
#22126=ORIENTED_EDGE('',*,*,#16289,.F.);
#22127=ORIENTED_EDGE('',*,*,#16287,.F.);
#22128=ORIENTED_EDGE('',*,*,#16290,.F.);
#22129=ORIENTED_EDGE('',*,*,#16285,.T.);
#22130=ORIENTED_EDGE('',*,*,#16291,.F.);
#22131=ORIENTED_EDGE('',*,*,#16292,.T.);
#22132=ORIENTED_EDGE('',*,*,#16291,.T.);
#22133=ORIENTED_EDGE('',*,*,#16292,.F.);
#22134=ORIENTED_EDGE('',*,*,#16288,.T.);
#22135=ORIENTED_EDGE('',*,*,#16289,.T.);
#22136=ORIENTED_EDGE('',*,*,#16290,.T.);
#22137=ORIENTED_EDGE('',*,*,#16293,.F.);
#22138=ORIENTED_EDGE('',*,*,#16272,.T.);
#22139=ORIENTED_EDGE('',*,*,#16282,.F.);
#22140=ORIENTED_EDGE('',*,*,#16273,.T.);
#22141=ORIENTED_EDGE('',*,*,#16294,.F.);
#22142=ORIENTED_EDGE('',*,*,#16283,.T.);
#22143=ORIENTED_EDGE('',*,*,#16286,.T.);
#22144=ORIENTED_EDGE('',*,*,#16293,.T.);
#22145=ORIENTED_EDGE('',*,*,#16284,.T.);
#22146=ORIENTED_EDGE('',*,*,#16294,.T.);
#22147=ORIENTED_EDGE('',*,*,#16295,.F.);
#22148=ORIENTED_EDGE('',*,*,#16296,.T.);
#22149=ORIENTED_EDGE('',*,*,#16297,.T.);
#22150=ORIENTED_EDGE('',*,*,#16298,.T.);
#22151=ORIENTED_EDGE('',*,*,#16299,.F.);
#22152=ORIENTED_EDGE('',*,*,#16300,.T.);
#22153=ORIENTED_EDGE('',*,*,#16295,.T.);
#22154=ORIENTED_EDGE('',*,*,#16301,.T.);
#22155=ORIENTED_EDGE('',*,*,#16302,.F.);
#22156=ORIENTED_EDGE('',*,*,#16303,.T.);
#22157=ORIENTED_EDGE('',*,*,#16299,.T.);
#22158=ORIENTED_EDGE('',*,*,#16304,.T.);
#22159=ORIENTED_EDGE('',*,*,#16305,.F.);
#22160=ORIENTED_EDGE('',*,*,#16306,.T.);
#22161=ORIENTED_EDGE('',*,*,#16302,.T.);
#22162=ORIENTED_EDGE('',*,*,#16307,.T.);
#22163=ORIENTED_EDGE('',*,*,#16308,.F.);
#22164=ORIENTED_EDGE('',*,*,#16309,.T.);
#22165=ORIENTED_EDGE('',*,*,#16305,.T.);
#22166=ORIENTED_EDGE('',*,*,#16310,.T.);
#22167=ORIENTED_EDGE('',*,*,#16311,.F.);
#22168=ORIENTED_EDGE('',*,*,#16312,.T.);
#22169=ORIENTED_EDGE('',*,*,#16308,.T.);
#22170=ORIENTED_EDGE('',*,*,#16313,.T.);
#22171=ORIENTED_EDGE('',*,*,#16314,.F.);
#22172=ORIENTED_EDGE('',*,*,#16315,.T.);
#22173=ORIENTED_EDGE('',*,*,#16311,.T.);
#22174=ORIENTED_EDGE('',*,*,#16316,.T.);
#22175=ORIENTED_EDGE('',*,*,#16317,.F.);
#22176=ORIENTED_EDGE('',*,*,#16318,.T.);
#22177=ORIENTED_EDGE('',*,*,#16314,.T.);
#22178=ORIENTED_EDGE('',*,*,#16319,.T.);
#22179=ORIENTED_EDGE('',*,*,#16320,.F.);
#22180=ORIENTED_EDGE('',*,*,#16321,.T.);
#22181=ORIENTED_EDGE('',*,*,#16317,.T.);
#22182=ORIENTED_EDGE('',*,*,#16322,.T.);
#22183=ORIENTED_EDGE('',*,*,#16323,.F.);
#22184=ORIENTED_EDGE('',*,*,#16324,.T.);
#22185=ORIENTED_EDGE('',*,*,#16320,.T.);
#22186=ORIENTED_EDGE('',*,*,#16325,.T.);
#22187=ORIENTED_EDGE('',*,*,#16326,.F.);
#22188=ORIENTED_EDGE('',*,*,#16327,.T.);
#22189=ORIENTED_EDGE('',*,*,#16328,.F.);
#22190=ORIENTED_EDGE('',*,*,#16329,.F.);
#22191=ORIENTED_EDGE('',*,*,#16330,.F.);
#22192=ORIENTED_EDGE('',*,*,#16331,.T.);
#22193=ORIENTED_EDGE('',*,*,#16326,.T.);
#22194=ORIENTED_EDGE('',*,*,#16332,.F.);
#22195=ORIENTED_EDGE('',*,*,#16333,.F.);
#22196=ORIENTED_EDGE('',*,*,#16334,.T.);
#22197=ORIENTED_EDGE('',*,*,#16330,.T.);
#22198=ORIENTED_EDGE('',*,*,#16335,.F.);
#22199=ORIENTED_EDGE('',*,*,#16336,.F.);
#22200=ORIENTED_EDGE('',*,*,#16337,.T.);
#22201=ORIENTED_EDGE('',*,*,#16333,.T.);
#22202=ORIENTED_EDGE('',*,*,#16338,.F.);
#22203=ORIENTED_EDGE('',*,*,#16339,.F.);
#22204=ORIENTED_EDGE('',*,*,#16340,.T.);
#22205=ORIENTED_EDGE('',*,*,#16336,.T.);
#22206=ORIENTED_EDGE('',*,*,#16341,.F.);
#22207=ORIENTED_EDGE('',*,*,#16342,.F.);
#22208=ORIENTED_EDGE('',*,*,#16343,.T.);
#22209=ORIENTED_EDGE('',*,*,#16339,.T.);
#22210=ORIENTED_EDGE('',*,*,#16344,.F.);
#22211=ORIENTED_EDGE('',*,*,#16345,.F.);
#22212=ORIENTED_EDGE('',*,*,#16346,.T.);
#22213=ORIENTED_EDGE('',*,*,#16342,.T.);
#22214=ORIENTED_EDGE('',*,*,#16347,.F.);
#22215=ORIENTED_EDGE('',*,*,#16348,.F.);
#22216=ORIENTED_EDGE('',*,*,#16349,.T.);
#22217=ORIENTED_EDGE('',*,*,#16345,.T.);
#22218=ORIENTED_EDGE('',*,*,#16350,.F.);
#22219=ORIENTED_EDGE('',*,*,#16351,.F.);
#22220=ORIENTED_EDGE('',*,*,#16352,.T.);
#22221=ORIENTED_EDGE('',*,*,#16348,.T.);
#22222=ORIENTED_EDGE('',*,*,#16353,.F.);
#22223=ORIENTED_EDGE('',*,*,#16354,.F.);
#22224=ORIENTED_EDGE('',*,*,#16355,.T.);
#22225=ORIENTED_EDGE('',*,*,#16351,.T.);
#22226=ORIENTED_EDGE('',*,*,#16356,.F.);
#22227=ORIENTED_EDGE('',*,*,#16328,.T.);
#22228=ORIENTED_EDGE('',*,*,#16357,.T.);
#22229=ORIENTED_EDGE('',*,*,#16358,.F.);
#22230=ORIENTED_EDGE('',*,*,#16359,.F.);
#22231=ORIENTED_EDGE('',*,*,#16360,.T.);
#22232=ORIENTED_EDGE('',*,*,#16360,.F.);
#22233=ORIENTED_EDGE('',*,*,#16361,.F.);
#22234=ORIENTED_EDGE('',*,*,#16325,.F.);
#22235=ORIENTED_EDGE('',*,*,#16322,.F.);
#22236=ORIENTED_EDGE('',*,*,#16319,.F.);
#22237=ORIENTED_EDGE('',*,*,#16316,.F.);
#22238=ORIENTED_EDGE('',*,*,#16313,.F.);
#22239=ORIENTED_EDGE('',*,*,#16310,.F.);
#22240=ORIENTED_EDGE('',*,*,#16307,.F.);
#22241=ORIENTED_EDGE('',*,*,#16304,.F.);
#22242=ORIENTED_EDGE('',*,*,#16301,.F.);
#22243=ORIENTED_EDGE('',*,*,#16298,.F.);
#22244=ORIENTED_EDGE('',*,*,#16362,.F.);
#22245=ORIENTED_EDGE('',*,*,#16363,.T.);
#22246=ORIENTED_EDGE('',*,*,#16356,.T.);
#22247=ORIENTED_EDGE('',*,*,#16353,.T.);
#22248=ORIENTED_EDGE('',*,*,#16350,.T.);
#22249=ORIENTED_EDGE('',*,*,#16347,.T.);
#22250=ORIENTED_EDGE('',*,*,#16344,.T.);
#22251=ORIENTED_EDGE('',*,*,#16341,.T.);
#22252=ORIENTED_EDGE('',*,*,#16338,.T.);
#22253=ORIENTED_EDGE('',*,*,#16335,.T.);
#22254=ORIENTED_EDGE('',*,*,#16332,.T.);
#22255=ORIENTED_EDGE('',*,*,#16329,.T.);
#22256=ORIENTED_EDGE('',*,*,#16364,.T.);
#22257=ORIENTED_EDGE('',*,*,#16365,.T.);
#22258=ORIENTED_EDGE('',*,*,#16366,.T.);
#22259=ORIENTED_EDGE('',*,*,#16367,.T.);
#22260=ORIENTED_EDGE('',*,*,#16362,.T.);
#22261=ORIENTED_EDGE('',*,*,#16354,.T.);
#22262=ORIENTED_EDGE('',*,*,#16363,.F.);
#22263=ORIENTED_EDGE('',*,*,#16367,.F.);
#22264=ORIENTED_EDGE('',*,*,#16368,.T.);
#22265=ORIENTED_EDGE('',*,*,#16357,.F.);
#22266=ORIENTED_EDGE('',*,*,#16327,.F.);
#22267=ORIENTED_EDGE('',*,*,#16331,.F.);
#22268=ORIENTED_EDGE('',*,*,#16334,.F.);
#22269=ORIENTED_EDGE('',*,*,#16337,.F.);
#22270=ORIENTED_EDGE('',*,*,#16340,.F.);
#22271=ORIENTED_EDGE('',*,*,#16343,.F.);
#22272=ORIENTED_EDGE('',*,*,#16346,.F.);
#22273=ORIENTED_EDGE('',*,*,#16349,.F.);
#22274=ORIENTED_EDGE('',*,*,#16352,.F.);
#22275=ORIENTED_EDGE('',*,*,#16355,.F.);
#22276=ORIENTED_EDGE('',*,*,#16368,.F.);
#22277=ORIENTED_EDGE('',*,*,#16366,.F.);
#22278=ORIENTED_EDGE('',*,*,#16296,.F.);
#22279=ORIENTED_EDGE('',*,*,#16300,.F.);
#22280=ORIENTED_EDGE('',*,*,#16303,.F.);
#22281=ORIENTED_EDGE('',*,*,#16306,.F.);
#22282=ORIENTED_EDGE('',*,*,#16309,.F.);
#22283=ORIENTED_EDGE('',*,*,#16312,.F.);
#22284=ORIENTED_EDGE('',*,*,#16315,.F.);
#22285=ORIENTED_EDGE('',*,*,#16318,.F.);
#22286=ORIENTED_EDGE('',*,*,#16321,.F.);
#22287=ORIENTED_EDGE('',*,*,#16324,.F.);
#22288=ORIENTED_EDGE('',*,*,#16369,.F.);
#22289=ORIENTED_EDGE('',*,*,#16370,.F.);
#22290=ORIENTED_EDGE('',*,*,#16371,.T.);
#22291=ORIENTED_EDGE('',*,*,#16372,.F.);
#22292=ORIENTED_EDGE('',*,*,#16373,.F.);
#22293=ORIENTED_EDGE('',*,*,#16374,.F.);
#22294=ORIENTED_EDGE('',*,*,#16373,.T.);
#22295=ORIENTED_EDGE('',*,*,#16375,.T.);
#22296=ORIENTED_EDGE('',*,*,#16376,.F.);
#22297=ORIENTED_EDGE('',*,*,#16375,.F.);
#22298=ORIENTED_EDGE('',*,*,#16372,.T.);
#22299=ORIENTED_EDGE('',*,*,#16377,.T.);
#22300=ORIENTED_EDGE('',*,*,#16378,.F.);
#22301=ORIENTED_EDGE('',*,*,#16377,.F.);
#22302=ORIENTED_EDGE('',*,*,#16371,.F.);
#22303=ORIENTED_EDGE('',*,*,#16379,.F.);
#22304=ORIENTED_EDGE('',*,*,#16380,.T.);
#22305=ORIENTED_EDGE('',*,*,#16381,.F.);
#22306=ORIENTED_EDGE('',*,*,#16382,.F.);
#22307=ORIENTED_EDGE('',*,*,#16383,.F.);
#22308=ORIENTED_EDGE('',*,*,#16382,.T.);
#22309=ORIENTED_EDGE('',*,*,#16384,.T.);
#22310=ORIENTED_EDGE('',*,*,#16385,.F.);
#22311=ORIENTED_EDGE('',*,*,#16384,.F.);
#22312=ORIENTED_EDGE('',*,*,#16381,.T.);
#22313=ORIENTED_EDGE('',*,*,#16386,.T.);
#22314=ORIENTED_EDGE('',*,*,#16387,.F.);
#22315=ORIENTED_EDGE('',*,*,#16386,.F.);
#22316=ORIENTED_EDGE('',*,*,#16380,.F.);
#22317=ORIENTED_EDGE('',*,*,#16388,.F.);
#22318=ORIENTED_EDGE('',*,*,#16389,.T.);
#22319=ORIENTED_EDGE('',*,*,#16390,.F.);
#22320=ORIENTED_EDGE('',*,*,#16391,.F.);
#22321=ORIENTED_EDGE('',*,*,#16392,.F.);
#22322=ORIENTED_EDGE('',*,*,#16391,.T.);
#22323=ORIENTED_EDGE('',*,*,#16393,.T.);
#22324=ORIENTED_EDGE('',*,*,#16394,.F.);
#22325=ORIENTED_EDGE('',*,*,#16393,.F.);
#22326=ORIENTED_EDGE('',*,*,#16390,.T.);
#22327=ORIENTED_EDGE('',*,*,#16395,.T.);
#22328=ORIENTED_EDGE('',*,*,#16396,.F.);
#22329=ORIENTED_EDGE('',*,*,#16395,.F.);
#22330=ORIENTED_EDGE('',*,*,#16389,.F.);
#22331=ORIENTED_EDGE('',*,*,#16397,.F.);
#22332=ORIENTED_EDGE('',*,*,#16398,.T.);
#22333=ORIENTED_EDGE('',*,*,#16399,.F.);
#22334=ORIENTED_EDGE('',*,*,#16400,.F.);
#22335=ORIENTED_EDGE('',*,*,#16401,.F.);
#22336=ORIENTED_EDGE('',*,*,#16400,.T.);
#22337=ORIENTED_EDGE('',*,*,#16402,.T.);
#22338=ORIENTED_EDGE('',*,*,#16403,.F.);
#22339=ORIENTED_EDGE('',*,*,#16402,.F.);
#22340=ORIENTED_EDGE('',*,*,#16399,.T.);
#22341=ORIENTED_EDGE('',*,*,#16404,.T.);
#22342=ORIENTED_EDGE('',*,*,#16405,.F.);
#22343=ORIENTED_EDGE('',*,*,#16404,.F.);
#22344=ORIENTED_EDGE('',*,*,#16398,.F.);
#22345=ORIENTED_EDGE('',*,*,#16406,.F.);
#22346=ORIENTED_EDGE('',*,*,#16407,.T.);
#22347=ORIENTED_EDGE('',*,*,#16408,.F.);
#22348=ORIENTED_EDGE('',*,*,#16409,.F.);
#22349=ORIENTED_EDGE('',*,*,#16410,.F.);
#22350=ORIENTED_EDGE('',*,*,#16409,.T.);
#22351=ORIENTED_EDGE('',*,*,#16411,.T.);
#22352=ORIENTED_EDGE('',*,*,#16412,.F.);
#22353=ORIENTED_EDGE('',*,*,#16411,.F.);
#22354=ORIENTED_EDGE('',*,*,#16408,.T.);
#22355=ORIENTED_EDGE('',*,*,#16413,.T.);
#22356=ORIENTED_EDGE('',*,*,#16414,.F.);
#22357=ORIENTED_EDGE('',*,*,#16413,.F.);
#22358=ORIENTED_EDGE('',*,*,#16407,.F.);
#22359=ORIENTED_EDGE('',*,*,#16415,.F.);
#22360=ORIENTED_EDGE('',*,*,#16416,.T.);
#22361=ORIENTED_EDGE('',*,*,#16417,.F.);
#22362=ORIENTED_EDGE('',*,*,#16418,.F.);
#22363=ORIENTED_EDGE('',*,*,#16419,.F.);
#22364=ORIENTED_EDGE('',*,*,#16418,.T.);
#22365=ORIENTED_EDGE('',*,*,#16420,.T.);
#22366=ORIENTED_EDGE('',*,*,#16421,.F.);
#22367=ORIENTED_EDGE('',*,*,#16420,.F.);
#22368=ORIENTED_EDGE('',*,*,#16417,.T.);
#22369=ORIENTED_EDGE('',*,*,#16422,.T.);
#22370=ORIENTED_EDGE('',*,*,#16423,.F.);
#22371=ORIENTED_EDGE('',*,*,#16422,.F.);
#22372=ORIENTED_EDGE('',*,*,#16416,.F.);
#22373=ORIENTED_EDGE('',*,*,#16424,.F.);
#22374=ORIENTED_EDGE('',*,*,#16425,.T.);
#22375=ORIENTED_EDGE('',*,*,#16426,.F.);
#22376=ORIENTED_EDGE('',*,*,#16427,.F.);
#22377=ORIENTED_EDGE('',*,*,#16428,.F.);
#22378=ORIENTED_EDGE('',*,*,#16427,.T.);
#22379=ORIENTED_EDGE('',*,*,#16429,.T.);
#22380=ORIENTED_EDGE('',*,*,#16430,.F.);
#22381=ORIENTED_EDGE('',*,*,#16429,.F.);
#22382=ORIENTED_EDGE('',*,*,#16426,.T.);
#22383=ORIENTED_EDGE('',*,*,#16431,.T.);
#22384=ORIENTED_EDGE('',*,*,#16432,.F.);
#22385=ORIENTED_EDGE('',*,*,#16431,.F.);
#22386=ORIENTED_EDGE('',*,*,#16425,.F.);
#22387=ORIENTED_EDGE('',*,*,#16433,.F.);
#22388=ORIENTED_EDGE('',*,*,#16434,.T.);
#22389=ORIENTED_EDGE('',*,*,#16435,.F.);
#22390=ORIENTED_EDGE('',*,*,#16436,.F.);
#22391=ORIENTED_EDGE('',*,*,#16437,.F.);
#22392=ORIENTED_EDGE('',*,*,#16436,.T.);
#22393=ORIENTED_EDGE('',*,*,#16438,.T.);
#22394=ORIENTED_EDGE('',*,*,#16439,.F.);
#22395=ORIENTED_EDGE('',*,*,#16438,.F.);
#22396=ORIENTED_EDGE('',*,*,#16435,.T.);
#22397=ORIENTED_EDGE('',*,*,#16440,.T.);
#22398=ORIENTED_EDGE('',*,*,#16441,.F.);
#22399=ORIENTED_EDGE('',*,*,#16440,.F.);
#22400=ORIENTED_EDGE('',*,*,#16434,.F.);
#22401=ORIENTED_EDGE('',*,*,#16442,.F.);
#22402=ORIENTED_EDGE('',*,*,#16443,.T.);
#22403=ORIENTED_EDGE('',*,*,#16444,.F.);
#22404=ORIENTED_EDGE('',*,*,#16445,.F.);
#22405=ORIENTED_EDGE('',*,*,#16446,.F.);
#22406=ORIENTED_EDGE('',*,*,#16445,.T.);
#22407=ORIENTED_EDGE('',*,*,#16447,.T.);
#22408=ORIENTED_EDGE('',*,*,#16448,.F.);
#22409=ORIENTED_EDGE('',*,*,#16447,.F.);
#22410=ORIENTED_EDGE('',*,*,#16444,.T.);
#22411=ORIENTED_EDGE('',*,*,#16449,.T.);
#22412=ORIENTED_EDGE('',*,*,#16450,.F.);
#22413=ORIENTED_EDGE('',*,*,#16449,.F.);
#22414=ORIENTED_EDGE('',*,*,#16443,.F.);
#22415=ORIENTED_EDGE('',*,*,#16451,.F.);
#22416=ORIENTED_EDGE('',*,*,#16452,.T.);
#22417=ORIENTED_EDGE('',*,*,#16453,.F.);
#22418=ORIENTED_EDGE('',*,*,#16454,.F.);
#22419=ORIENTED_EDGE('',*,*,#16455,.F.);
#22420=ORIENTED_EDGE('',*,*,#16454,.T.);
#22421=ORIENTED_EDGE('',*,*,#16456,.T.);
#22422=ORIENTED_EDGE('',*,*,#16457,.F.);
#22423=ORIENTED_EDGE('',*,*,#16456,.F.);
#22424=ORIENTED_EDGE('',*,*,#16453,.T.);
#22425=ORIENTED_EDGE('',*,*,#16458,.T.);
#22426=ORIENTED_EDGE('',*,*,#16459,.F.);
#22427=ORIENTED_EDGE('',*,*,#16458,.F.);
#22428=ORIENTED_EDGE('',*,*,#16452,.F.);
#22429=ORIENTED_EDGE('',*,*,#16460,.F.);
#22430=ORIENTED_EDGE('',*,*,#16461,.T.);
#22431=ORIENTED_EDGE('',*,*,#16462,.F.);
#22432=ORIENTED_EDGE('',*,*,#16463,.F.);
#22433=ORIENTED_EDGE('',*,*,#16464,.F.);
#22434=ORIENTED_EDGE('',*,*,#16463,.T.);
#22435=ORIENTED_EDGE('',*,*,#16465,.T.);
#22436=ORIENTED_EDGE('',*,*,#16466,.F.);
#22437=ORIENTED_EDGE('',*,*,#16465,.F.);
#22438=ORIENTED_EDGE('',*,*,#16462,.T.);
#22439=ORIENTED_EDGE('',*,*,#16467,.T.);
#22440=ORIENTED_EDGE('',*,*,#16468,.F.);
#22441=ORIENTED_EDGE('',*,*,#16467,.F.);
#22442=ORIENTED_EDGE('',*,*,#16461,.F.);
#22443=ORIENTED_EDGE('',*,*,#16469,.F.);
#22444=ORIENTED_EDGE('',*,*,#16470,.T.);
#22445=ORIENTED_EDGE('',*,*,#16471,.F.);
#22446=ORIENTED_EDGE('',*,*,#16472,.F.);
#22447=ORIENTED_EDGE('',*,*,#16473,.F.);
#22448=ORIENTED_EDGE('',*,*,#16472,.T.);
#22449=ORIENTED_EDGE('',*,*,#16474,.T.);
#22450=ORIENTED_EDGE('',*,*,#16475,.F.);
#22451=ORIENTED_EDGE('',*,*,#16474,.F.);
#22452=ORIENTED_EDGE('',*,*,#16471,.T.);
#22453=ORIENTED_EDGE('',*,*,#16476,.T.);
#22454=ORIENTED_EDGE('',*,*,#16477,.F.);
#22455=ORIENTED_EDGE('',*,*,#16476,.F.);
#22456=ORIENTED_EDGE('',*,*,#16470,.F.);
#22457=ORIENTED_EDGE('',*,*,#16478,.F.);
#22458=ORIENTED_EDGE('',*,*,#16479,.T.);
#22459=ORIENTED_EDGE('',*,*,#16480,.F.);
#22460=ORIENTED_EDGE('',*,*,#16481,.F.);
#22461=ORIENTED_EDGE('',*,*,#16482,.F.);
#22462=ORIENTED_EDGE('',*,*,#16481,.T.);
#22463=ORIENTED_EDGE('',*,*,#16483,.T.);
#22464=ORIENTED_EDGE('',*,*,#16484,.F.);
#22465=ORIENTED_EDGE('',*,*,#16483,.F.);
#22466=ORIENTED_EDGE('',*,*,#16480,.T.);
#22467=ORIENTED_EDGE('',*,*,#16485,.T.);
#22468=ORIENTED_EDGE('',*,*,#16486,.F.);
#22469=ORIENTED_EDGE('',*,*,#16485,.F.);
#22470=ORIENTED_EDGE('',*,*,#16479,.F.);
#22471=ORIENTED_EDGE('',*,*,#16487,.F.);
#22472=ORIENTED_EDGE('',*,*,#16488,.T.);
#22473=ORIENTED_EDGE('',*,*,#16489,.F.);
#22474=ORIENTED_EDGE('',*,*,#16490,.F.);
#22475=ORIENTED_EDGE('',*,*,#16491,.F.);
#22476=ORIENTED_EDGE('',*,*,#16490,.T.);
#22477=ORIENTED_EDGE('',*,*,#16492,.T.);
#22478=ORIENTED_EDGE('',*,*,#16493,.F.);
#22479=ORIENTED_EDGE('',*,*,#16492,.F.);
#22480=ORIENTED_EDGE('',*,*,#16489,.T.);
#22481=ORIENTED_EDGE('',*,*,#16494,.T.);
#22482=ORIENTED_EDGE('',*,*,#16495,.F.);
#22483=ORIENTED_EDGE('',*,*,#16494,.F.);
#22484=ORIENTED_EDGE('',*,*,#16488,.F.);
#22485=ORIENTED_EDGE('',*,*,#16496,.F.);
#22486=ORIENTED_EDGE('',*,*,#16497,.T.);
#22487=ORIENTED_EDGE('',*,*,#16498,.F.);
#22488=ORIENTED_EDGE('',*,*,#16499,.F.);
#22489=ORIENTED_EDGE('',*,*,#16500,.F.);
#22490=ORIENTED_EDGE('',*,*,#16499,.T.);
#22491=ORIENTED_EDGE('',*,*,#16501,.T.);
#22492=ORIENTED_EDGE('',*,*,#16502,.F.);
#22493=ORIENTED_EDGE('',*,*,#16501,.F.);
#22494=ORIENTED_EDGE('',*,*,#16498,.T.);
#22495=ORIENTED_EDGE('',*,*,#16503,.T.);
#22496=ORIENTED_EDGE('',*,*,#16504,.F.);
#22497=ORIENTED_EDGE('',*,*,#16503,.F.);
#22498=ORIENTED_EDGE('',*,*,#16497,.F.);
#22499=ORIENTED_EDGE('',*,*,#16505,.F.);
#22500=ORIENTED_EDGE('',*,*,#16506,.T.);
#22501=ORIENTED_EDGE('',*,*,#16507,.F.);
#22502=ORIENTED_EDGE('',*,*,#16508,.F.);
#22503=ORIENTED_EDGE('',*,*,#16509,.F.);
#22504=ORIENTED_EDGE('',*,*,#16508,.T.);
#22505=ORIENTED_EDGE('',*,*,#16510,.T.);
#22506=ORIENTED_EDGE('',*,*,#16511,.F.);
#22507=ORIENTED_EDGE('',*,*,#16510,.F.);
#22508=ORIENTED_EDGE('',*,*,#16507,.T.);
#22509=ORIENTED_EDGE('',*,*,#16512,.T.);
#22510=ORIENTED_EDGE('',*,*,#16513,.F.);
#22511=ORIENTED_EDGE('',*,*,#16512,.F.);
#22512=ORIENTED_EDGE('',*,*,#16506,.F.);
#22513=ORIENTED_EDGE('',*,*,#16514,.F.);
#22514=ORIENTED_EDGE('',*,*,#16515,.T.);
#22515=ORIENTED_EDGE('',*,*,#16516,.F.);
#22516=ORIENTED_EDGE('',*,*,#16517,.F.);
#22517=ORIENTED_EDGE('',*,*,#16518,.F.);
#22518=ORIENTED_EDGE('',*,*,#16517,.T.);
#22519=ORIENTED_EDGE('',*,*,#16519,.T.);
#22520=ORIENTED_EDGE('',*,*,#16520,.F.);
#22521=ORIENTED_EDGE('',*,*,#16519,.F.);
#22522=ORIENTED_EDGE('',*,*,#16516,.T.);
#22523=ORIENTED_EDGE('',*,*,#16521,.T.);
#22524=ORIENTED_EDGE('',*,*,#16522,.F.);
#22525=ORIENTED_EDGE('',*,*,#16521,.F.);
#22526=ORIENTED_EDGE('',*,*,#16515,.F.);
#22527=ORIENTED_EDGE('',*,*,#16523,.F.);
#22528=ORIENTED_EDGE('',*,*,#16524,.T.);
#22529=ORIENTED_EDGE('',*,*,#16525,.F.);
#22530=ORIENTED_EDGE('',*,*,#16526,.F.);
#22531=ORIENTED_EDGE('',*,*,#16527,.F.);
#22532=ORIENTED_EDGE('',*,*,#16526,.T.);
#22533=ORIENTED_EDGE('',*,*,#16528,.T.);
#22534=ORIENTED_EDGE('',*,*,#16529,.F.);
#22535=ORIENTED_EDGE('',*,*,#16530,.F.);
#22536=ORIENTED_EDGE('',*,*,#16528,.F.);
#22537=ORIENTED_EDGE('',*,*,#16525,.T.);
#22538=ORIENTED_EDGE('',*,*,#16531,.T.);
#22539=ORIENTED_EDGE('',*,*,#16532,.F.);
#22540=ORIENTED_EDGE('',*,*,#16531,.F.);
#22541=ORIENTED_EDGE('',*,*,#16524,.F.);
#22542=ORIENTED_EDGE('',*,*,#16533,.F.);
#22543=ORIENTED_EDGE('',*,*,#16534,.F.);
#22544=ORIENTED_EDGE('',*,*,#16535,.T.);
#22545=ORIENTED_EDGE('',*,*,#16536,.F.);
#22546=ORIENTED_EDGE('',*,*,#16537,.F.);
#22547=ORIENTED_EDGE('',*,*,#16538,.F.);
#22548=ORIENTED_EDGE('',*,*,#16537,.T.);
#22549=ORIENTED_EDGE('',*,*,#16539,.T.);
#22550=ORIENTED_EDGE('',*,*,#16540,.F.);
#22551=ORIENTED_EDGE('',*,*,#16539,.F.);
#22552=ORIENTED_EDGE('',*,*,#16536,.T.);
#22553=ORIENTED_EDGE('',*,*,#16541,.T.);
#22554=ORIENTED_EDGE('',*,*,#16542,.F.);
#22555=ORIENTED_EDGE('',*,*,#16541,.F.);
#22556=ORIENTED_EDGE('',*,*,#16535,.F.);
#22557=ORIENTED_EDGE('',*,*,#16543,.F.);
#22558=ORIENTED_EDGE('',*,*,#16544,.T.);
#22559=ORIENTED_EDGE('',*,*,#16545,.F.);
#22560=ORIENTED_EDGE('',*,*,#16546,.F.);
#22561=ORIENTED_EDGE('',*,*,#16547,.F.);
#22562=ORIENTED_EDGE('',*,*,#16546,.T.);
#22563=ORIENTED_EDGE('',*,*,#16548,.T.);
#22564=ORIENTED_EDGE('',*,*,#16549,.F.);
#22565=ORIENTED_EDGE('',*,*,#16548,.F.);
#22566=ORIENTED_EDGE('',*,*,#16545,.T.);
#22567=ORIENTED_EDGE('',*,*,#16550,.T.);
#22568=ORIENTED_EDGE('',*,*,#16551,.F.);
#22569=ORIENTED_EDGE('',*,*,#16550,.F.);
#22570=ORIENTED_EDGE('',*,*,#16544,.F.);
#22571=ORIENTED_EDGE('',*,*,#16552,.F.);
#22572=ORIENTED_EDGE('',*,*,#16553,.T.);
#22573=ORIENTED_EDGE('',*,*,#16554,.F.);
#22574=ORIENTED_EDGE('',*,*,#16555,.F.);
#22575=ORIENTED_EDGE('',*,*,#16556,.F.);
#22576=ORIENTED_EDGE('',*,*,#16555,.T.);
#22577=ORIENTED_EDGE('',*,*,#16557,.T.);
#22578=ORIENTED_EDGE('',*,*,#16558,.F.);
#22579=ORIENTED_EDGE('',*,*,#16557,.F.);
#22580=ORIENTED_EDGE('',*,*,#16554,.T.);
#22581=ORIENTED_EDGE('',*,*,#16559,.T.);
#22582=ORIENTED_EDGE('',*,*,#16560,.F.);
#22583=ORIENTED_EDGE('',*,*,#16559,.F.);
#22584=ORIENTED_EDGE('',*,*,#16553,.F.);
#22585=ORIENTED_EDGE('',*,*,#16561,.F.);
#22586=ORIENTED_EDGE('',*,*,#16562,.T.);
#22587=ORIENTED_EDGE('',*,*,#16563,.F.);
#22588=ORIENTED_EDGE('',*,*,#16564,.F.);
#22589=ORIENTED_EDGE('',*,*,#16565,.F.);
#22590=ORIENTED_EDGE('',*,*,#16564,.T.);
#22591=ORIENTED_EDGE('',*,*,#16566,.T.);
#22592=ORIENTED_EDGE('',*,*,#16567,.F.);
#22593=ORIENTED_EDGE('',*,*,#16566,.F.);
#22594=ORIENTED_EDGE('',*,*,#16563,.T.);
#22595=ORIENTED_EDGE('',*,*,#16568,.T.);
#22596=ORIENTED_EDGE('',*,*,#16569,.F.);
#22597=ORIENTED_EDGE('',*,*,#16568,.F.);
#22598=ORIENTED_EDGE('',*,*,#16562,.F.);
#22599=ORIENTED_EDGE('',*,*,#16570,.F.);
#22600=ORIENTED_EDGE('',*,*,#16571,.T.);
#22601=ORIENTED_EDGE('',*,*,#16572,.F.);
#22602=ORIENTED_EDGE('',*,*,#16573,.F.);
#22603=ORIENTED_EDGE('',*,*,#16574,.F.);
#22604=ORIENTED_EDGE('',*,*,#16573,.T.);
#22605=ORIENTED_EDGE('',*,*,#16575,.T.);
#22606=ORIENTED_EDGE('',*,*,#16576,.F.);
#22607=ORIENTED_EDGE('',*,*,#16575,.F.);
#22608=ORIENTED_EDGE('',*,*,#16572,.T.);
#22609=ORIENTED_EDGE('',*,*,#16577,.T.);
#22610=ORIENTED_EDGE('',*,*,#16578,.F.);
#22611=ORIENTED_EDGE('',*,*,#16577,.F.);
#22612=ORIENTED_EDGE('',*,*,#16571,.F.);
#22613=ORIENTED_EDGE('',*,*,#16579,.F.);
#22614=ORIENTED_EDGE('',*,*,#16580,.T.);
#22615=ORIENTED_EDGE('',*,*,#16581,.F.);
#22616=ORIENTED_EDGE('',*,*,#16582,.F.);
#22617=ORIENTED_EDGE('',*,*,#16583,.F.);
#22618=ORIENTED_EDGE('',*,*,#16582,.T.);
#22619=ORIENTED_EDGE('',*,*,#16584,.T.);
#22620=ORIENTED_EDGE('',*,*,#16585,.F.);
#22621=ORIENTED_EDGE('',*,*,#16584,.F.);
#22622=ORIENTED_EDGE('',*,*,#16581,.T.);
#22623=ORIENTED_EDGE('',*,*,#16586,.T.);
#22624=ORIENTED_EDGE('',*,*,#16587,.F.);
#22625=ORIENTED_EDGE('',*,*,#16586,.F.);
#22626=ORIENTED_EDGE('',*,*,#16580,.F.);
#22627=ORIENTED_EDGE('',*,*,#16588,.F.);
#22628=ORIENTED_EDGE('',*,*,#16589,.T.);
#22629=ORIENTED_EDGE('',*,*,#16590,.F.);
#22630=ORIENTED_EDGE('',*,*,#16591,.F.);
#22631=ORIENTED_EDGE('',*,*,#16592,.F.);
#22632=ORIENTED_EDGE('',*,*,#16591,.T.);
#22633=ORIENTED_EDGE('',*,*,#16593,.T.);
#22634=ORIENTED_EDGE('',*,*,#16594,.F.);
#22635=ORIENTED_EDGE('',*,*,#16593,.F.);
#22636=ORIENTED_EDGE('',*,*,#16590,.T.);
#22637=ORIENTED_EDGE('',*,*,#16595,.T.);
#22638=ORIENTED_EDGE('',*,*,#16596,.F.);
#22639=ORIENTED_EDGE('',*,*,#16595,.F.);
#22640=ORIENTED_EDGE('',*,*,#16589,.F.);
#22641=ORIENTED_EDGE('',*,*,#16597,.F.);
#22642=ORIENTED_EDGE('',*,*,#16598,.T.);
#22643=ORIENTED_EDGE('',*,*,#16599,.F.);
#22644=ORIENTED_EDGE('',*,*,#16600,.F.);
#22645=ORIENTED_EDGE('',*,*,#16601,.F.);
#22646=ORIENTED_EDGE('',*,*,#16600,.T.);
#22647=ORIENTED_EDGE('',*,*,#16602,.T.);
#22648=ORIENTED_EDGE('',*,*,#16603,.F.);
#22649=ORIENTED_EDGE('',*,*,#16602,.F.);
#22650=ORIENTED_EDGE('',*,*,#16599,.T.);
#22651=ORIENTED_EDGE('',*,*,#16604,.T.);
#22652=ORIENTED_EDGE('',*,*,#16605,.F.);
#22653=ORIENTED_EDGE('',*,*,#16604,.F.);
#22654=ORIENTED_EDGE('',*,*,#16598,.F.);
#22655=ORIENTED_EDGE('',*,*,#16606,.F.);
#22656=ORIENTED_EDGE('',*,*,#16607,.T.);
#22657=ORIENTED_EDGE('',*,*,#16608,.F.);
#22658=ORIENTED_EDGE('',*,*,#16609,.F.);
#22659=ORIENTED_EDGE('',*,*,#16610,.F.);
#22660=ORIENTED_EDGE('',*,*,#16609,.T.);
#22661=ORIENTED_EDGE('',*,*,#16611,.T.);
#22662=ORIENTED_EDGE('',*,*,#16612,.F.);
#22663=ORIENTED_EDGE('',*,*,#16611,.F.);
#22664=ORIENTED_EDGE('',*,*,#16608,.T.);
#22665=ORIENTED_EDGE('',*,*,#16613,.T.);
#22666=ORIENTED_EDGE('',*,*,#16614,.F.);
#22667=ORIENTED_EDGE('',*,*,#16613,.F.);
#22668=ORIENTED_EDGE('',*,*,#16607,.F.);
#22669=ORIENTED_EDGE('',*,*,#16615,.F.);
#22670=ORIENTED_EDGE('',*,*,#16616,.T.);
#22671=ORIENTED_EDGE('',*,*,#16617,.F.);
#22672=ORIENTED_EDGE('',*,*,#16618,.F.);
#22673=ORIENTED_EDGE('',*,*,#16619,.F.);
#22674=ORIENTED_EDGE('',*,*,#16618,.T.);
#22675=ORIENTED_EDGE('',*,*,#16620,.T.);
#22676=ORIENTED_EDGE('',*,*,#16621,.F.);
#22677=ORIENTED_EDGE('',*,*,#16620,.F.);
#22678=ORIENTED_EDGE('',*,*,#16617,.T.);
#22679=ORIENTED_EDGE('',*,*,#16622,.T.);
#22680=ORIENTED_EDGE('',*,*,#16623,.F.);
#22681=ORIENTED_EDGE('',*,*,#16622,.F.);
#22682=ORIENTED_EDGE('',*,*,#16616,.F.);
#22683=ORIENTED_EDGE('',*,*,#16624,.F.);
#22684=ORIENTED_EDGE('',*,*,#16625,.T.);
#22685=ORIENTED_EDGE('',*,*,#16626,.F.);
#22686=ORIENTED_EDGE('',*,*,#16627,.F.);
#22687=ORIENTED_EDGE('',*,*,#16628,.F.);
#22688=ORIENTED_EDGE('',*,*,#16627,.T.);
#22689=ORIENTED_EDGE('',*,*,#16629,.T.);
#22690=ORIENTED_EDGE('',*,*,#16630,.F.);
#22691=ORIENTED_EDGE('',*,*,#16629,.F.);
#22692=ORIENTED_EDGE('',*,*,#16626,.T.);
#22693=ORIENTED_EDGE('',*,*,#16631,.T.);
#22694=ORIENTED_EDGE('',*,*,#16632,.F.);
#22695=ORIENTED_EDGE('',*,*,#16631,.F.);
#22696=ORIENTED_EDGE('',*,*,#16625,.F.);
#22697=ORIENTED_EDGE('',*,*,#16633,.F.);
#22698=ORIENTED_EDGE('',*,*,#16634,.T.);
#22699=ORIENTED_EDGE('',*,*,#16635,.F.);
#22700=ORIENTED_EDGE('',*,*,#16636,.F.);
#22701=ORIENTED_EDGE('',*,*,#16637,.F.);
#22702=ORIENTED_EDGE('',*,*,#16636,.T.);
#22703=ORIENTED_EDGE('',*,*,#16638,.T.);
#22704=ORIENTED_EDGE('',*,*,#16639,.F.);
#22705=ORIENTED_EDGE('',*,*,#16638,.F.);
#22706=ORIENTED_EDGE('',*,*,#16635,.T.);
#22707=ORIENTED_EDGE('',*,*,#16640,.T.);
#22708=ORIENTED_EDGE('',*,*,#16641,.F.);
#22709=ORIENTED_EDGE('',*,*,#16640,.F.);
#22710=ORIENTED_EDGE('',*,*,#16634,.F.);
#22711=ORIENTED_EDGE('',*,*,#16642,.F.);
#22712=ORIENTED_EDGE('',*,*,#16643,.T.);
#22713=ORIENTED_EDGE('',*,*,#16644,.F.);
#22714=ORIENTED_EDGE('',*,*,#16645,.F.);
#22715=ORIENTED_EDGE('',*,*,#16646,.F.);
#22716=ORIENTED_EDGE('',*,*,#16645,.T.);
#22717=ORIENTED_EDGE('',*,*,#16647,.T.);
#22718=ORIENTED_EDGE('',*,*,#16648,.F.);
#22719=ORIENTED_EDGE('',*,*,#16647,.F.);
#22720=ORIENTED_EDGE('',*,*,#16644,.T.);
#22721=ORIENTED_EDGE('',*,*,#16649,.T.);
#22722=ORIENTED_EDGE('',*,*,#16650,.F.);
#22723=ORIENTED_EDGE('',*,*,#16649,.F.);
#22724=ORIENTED_EDGE('',*,*,#16643,.F.);
#22725=ORIENTED_EDGE('',*,*,#16651,.F.);
#22726=ORIENTED_EDGE('',*,*,#16652,.T.);
#22727=ORIENTED_EDGE('',*,*,#16653,.F.);
#22728=ORIENTED_EDGE('',*,*,#16654,.F.);
#22729=ORIENTED_EDGE('',*,*,#16655,.F.);
#22730=ORIENTED_EDGE('',*,*,#16654,.T.);
#22731=ORIENTED_EDGE('',*,*,#16656,.T.);
#22732=ORIENTED_EDGE('',*,*,#16657,.F.);
#22733=ORIENTED_EDGE('',*,*,#16656,.F.);
#22734=ORIENTED_EDGE('',*,*,#16653,.T.);
#22735=ORIENTED_EDGE('',*,*,#16658,.T.);
#22736=ORIENTED_EDGE('',*,*,#16659,.F.);
#22737=ORIENTED_EDGE('',*,*,#16658,.F.);
#22738=ORIENTED_EDGE('',*,*,#16652,.F.);
#22739=ORIENTED_EDGE('',*,*,#16660,.F.);
#22740=ORIENTED_EDGE('',*,*,#16661,.T.);
#22741=ORIENTED_EDGE('',*,*,#16662,.F.);
#22742=ORIENTED_EDGE('',*,*,#16663,.F.);
#22743=ORIENTED_EDGE('',*,*,#16664,.F.);
#22744=ORIENTED_EDGE('',*,*,#16663,.T.);
#22745=ORIENTED_EDGE('',*,*,#16665,.T.);
#22746=ORIENTED_EDGE('',*,*,#16666,.F.);
#22747=ORIENTED_EDGE('',*,*,#16665,.F.);
#22748=ORIENTED_EDGE('',*,*,#16662,.T.);
#22749=ORIENTED_EDGE('',*,*,#16667,.T.);
#22750=ORIENTED_EDGE('',*,*,#16668,.F.);
#22751=ORIENTED_EDGE('',*,*,#16667,.F.);
#22752=ORIENTED_EDGE('',*,*,#16661,.F.);
#22753=ORIENTED_EDGE('',*,*,#16669,.F.);
#22754=ORIENTED_EDGE('',*,*,#16670,.T.);
#22755=ORIENTED_EDGE('',*,*,#16671,.F.);
#22756=ORIENTED_EDGE('',*,*,#16672,.F.);
#22757=ORIENTED_EDGE('',*,*,#16673,.F.);
#22758=ORIENTED_EDGE('',*,*,#16672,.T.);
#22759=ORIENTED_EDGE('',*,*,#16674,.T.);
#22760=ORIENTED_EDGE('',*,*,#16675,.F.);
#22761=ORIENTED_EDGE('',*,*,#16674,.F.);
#22762=ORIENTED_EDGE('',*,*,#16671,.T.);
#22763=ORIENTED_EDGE('',*,*,#16676,.T.);
#22764=ORIENTED_EDGE('',*,*,#16677,.F.);
#22765=ORIENTED_EDGE('',*,*,#16676,.F.);
#22766=ORIENTED_EDGE('',*,*,#16670,.F.);
#22767=ORIENTED_EDGE('',*,*,#16678,.F.);
#22768=ORIENTED_EDGE('',*,*,#16679,.T.);
#22769=ORIENTED_EDGE('',*,*,#16680,.F.);
#22770=ORIENTED_EDGE('',*,*,#16681,.F.);
#22771=ORIENTED_EDGE('',*,*,#16682,.F.);
#22772=ORIENTED_EDGE('',*,*,#16681,.T.);
#22773=ORIENTED_EDGE('',*,*,#16683,.T.);
#22774=ORIENTED_EDGE('',*,*,#16684,.F.);
#22775=ORIENTED_EDGE('',*,*,#16683,.F.);
#22776=ORIENTED_EDGE('',*,*,#16680,.T.);
#22777=ORIENTED_EDGE('',*,*,#16685,.T.);
#22778=ORIENTED_EDGE('',*,*,#16686,.F.);
#22779=ORIENTED_EDGE('',*,*,#16685,.F.);
#22780=ORIENTED_EDGE('',*,*,#16679,.F.);
#22781=ORIENTED_EDGE('',*,*,#16687,.F.);
#22782=ORIENTED_EDGE('',*,*,#16688,.T.);
#22783=ORIENTED_EDGE('',*,*,#16689,.F.);
#22784=ORIENTED_EDGE('',*,*,#16690,.F.);
#22785=ORIENTED_EDGE('',*,*,#16691,.F.);
#22786=ORIENTED_EDGE('',*,*,#16690,.T.);
#22787=ORIENTED_EDGE('',*,*,#16692,.T.);
#22788=ORIENTED_EDGE('',*,*,#16693,.F.);
#22789=ORIENTED_EDGE('',*,*,#16692,.F.);
#22790=ORIENTED_EDGE('',*,*,#16689,.T.);
#22791=ORIENTED_EDGE('',*,*,#16694,.T.);
#22792=ORIENTED_EDGE('',*,*,#16695,.F.);
#22793=ORIENTED_EDGE('',*,*,#16694,.F.);
#22794=ORIENTED_EDGE('',*,*,#16688,.F.);
#22795=ORIENTED_EDGE('',*,*,#16696,.T.);
#22796=ORIENTED_EDGE('',*,*,#16697,.F.);
#22797=ORIENTED_EDGE('',*,*,#16696,.F.);
#22798=ORIENTED_EDGE('',*,*,#16698,.F.);
#22799=ORIENTED_EDGE('',*,*,#16699,.T.);
#22800=ORIENTED_EDGE('',*,*,#16700,.T.);
#22801=ORIENTED_EDGE('',*,*,#16701,.F.);
#22802=ORIENTED_EDGE('',*,*,#16702,.F.);
#22803=ORIENTED_EDGE('',*,*,#16703,.T.);
#22804=ORIENTED_EDGE('',*,*,#16704,.T.);
#22805=ORIENTED_EDGE('',*,*,#16699,.F.);
#22806=ORIENTED_EDGE('',*,*,#16705,.F.);
#22807=ORIENTED_EDGE('',*,*,#16706,.T.);
#22808=ORIENTED_EDGE('',*,*,#16707,.T.);
#22809=ORIENTED_EDGE('',*,*,#16703,.F.);
#22810=ORIENTED_EDGE('',*,*,#16708,.F.);
#22811=ORIENTED_EDGE('',*,*,#16709,.T.);
#22812=ORIENTED_EDGE('',*,*,#16710,.T.);
#22813=ORIENTED_EDGE('',*,*,#16706,.F.);
#22814=ORIENTED_EDGE('',*,*,#16711,.F.);
#22815=ORIENTED_EDGE('',*,*,#16712,.T.);
#22816=ORIENTED_EDGE('',*,*,#16713,.T.);
#22817=ORIENTED_EDGE('',*,*,#16709,.F.);
#22818=ORIENTED_EDGE('',*,*,#16714,.F.);
#22819=ORIENTED_EDGE('',*,*,#16701,.T.);
#22820=ORIENTED_EDGE('',*,*,#16715,.T.);
#22821=ORIENTED_EDGE('',*,*,#16712,.F.);
#22822=ORIENTED_EDGE('',*,*,#16715,.F.);
#22823=ORIENTED_EDGE('',*,*,#16700,.F.);
#22824=ORIENTED_EDGE('',*,*,#16704,.F.);
#22825=ORIENTED_EDGE('',*,*,#16707,.F.);
#22826=ORIENTED_EDGE('',*,*,#16710,.F.);
#22827=ORIENTED_EDGE('',*,*,#16713,.F.);
#22828=ORIENTED_EDGE('',*,*,#16697,.T.);
#22829=ORIENTED_EDGE('',*,*,#16716,.T.);
#22830=ORIENTED_EDGE('',*,*,#16717,.T.);
#22831=ORIENTED_EDGE('',*,*,#16718,.T.);
#22832=ORIENTED_EDGE('',*,*,#16717,.F.);
#22833=ORIENTED_EDGE('',*,*,#16719,.T.);
#22834=ORIENTED_EDGE('',*,*,#16716,.F.);
#22835=ORIENTED_EDGE('',*,*,#16720,.T.);
#22836=ORIENTED_EDGE('',*,*,#16721,.T.);
#22837=ORIENTED_EDGE('',*,*,#16720,.F.);
#22838=ORIENTED_EDGE('',*,*,#16719,.F.);
#22839=ORIENTED_EDGE('',*,*,#16722,.F.);
#22840=ORIENTED_EDGE('',*,*,#16718,.F.);
#22841=ORIENTED_EDGE('',*,*,#16723,.F.);
#22842=ORIENTED_EDGE('',*,*,#16364,.F.);
#22843=ORIENTED_EDGE('',*,*,#16297,.F.);
#22844=ORIENTED_EDGE('',*,*,#16365,.F.);
#22845=ORIENTED_EDGE('',*,*,#16724,.T.);
#22846=ORIENTED_EDGE('',*,*,#16723,.T.);
#22847=ORIENTED_EDGE('',*,*,#16724,.F.);
#22848=ORIENTED_EDGE('',*,*,#16323,.T.);
#22849=ORIENTED_EDGE('',*,*,#16361,.T.);
#22850=ORIENTED_EDGE('',*,*,#16725,.F.);
#22851=ORIENTED_EDGE('',*,*,#16369,.T.);
#22852=ORIENTED_EDGE('',*,*,#16726,.F.);
#22853=ORIENTED_EDGE('',*,*,#16727,.T.);
#22854=ORIENTED_EDGE('',*,*,#16358,.T.);
#22855=ORIENTED_EDGE('',*,*,#16725,.T.);
#22856=ORIENTED_EDGE('',*,*,#16359,.T.);
#22857=ORIENTED_EDGE('',*,*,#16727,.F.);
#22858=ORIENTED_EDGE('',*,*,#16728,.F.);
#22859=ORIENTED_EDGE('',*,*,#16729,.T.);
#22860=ORIENTED_EDGE('',*,*,#16726,.T.);
#22861=ORIENTED_EDGE('',*,*,#16729,.F.);
#22862=ORIENTED_EDGE('',*,*,#16721,.F.);
#22863=ORIENTED_EDGE('',*,*,#16728,.T.);
#22864=ORIENTED_EDGE('',*,*,#16730,.F.);
#22865=ORIENTED_EDGE('',*,*,#16731,.T.);
#22866=ORIENTED_EDGE('',*,*,#16533,.T.);
#22867=ORIENTED_EDGE('',*,*,#16523,.T.);
#22868=ORIENTED_EDGE('',*,*,#16527,.T.);
#22869=ORIENTED_EDGE('',*,*,#16732,.T.);
#22870=ORIENTED_EDGE('',*,*,#16722,.T.);
#22871=ORIENTED_EDGE('',*,*,#16732,.F.);
#22872=ORIENTED_EDGE('',*,*,#16529,.T.);
#22873=ORIENTED_EDGE('',*,*,#16530,.T.);
#22874=ORIENTED_EDGE('',*,*,#16532,.T.);
#22875=ORIENTED_EDGE('',*,*,#16731,.F.);
#22876=ORIENTED_EDGE('',*,*,#16376,.T.);
#22877=ORIENTED_EDGE('',*,*,#16378,.T.);
#22878=ORIENTED_EDGE('',*,*,#16370,.T.);
#22879=ORIENTED_EDGE('',*,*,#16374,.T.);
#22880=ORIENTED_EDGE('',*,*,#16385,.T.);
#22881=ORIENTED_EDGE('',*,*,#16387,.T.);
#22882=ORIENTED_EDGE('',*,*,#16379,.T.);
#22883=ORIENTED_EDGE('',*,*,#16383,.T.);
#22884=ORIENTED_EDGE('',*,*,#16394,.T.);
#22885=ORIENTED_EDGE('',*,*,#16396,.T.);
#22886=ORIENTED_EDGE('',*,*,#16388,.T.);
#22887=ORIENTED_EDGE('',*,*,#16392,.T.);
#22888=ORIENTED_EDGE('',*,*,#16403,.T.);
#22889=ORIENTED_EDGE('',*,*,#16405,.T.);
#22890=ORIENTED_EDGE('',*,*,#16397,.T.);
#22891=ORIENTED_EDGE('',*,*,#16401,.T.);
#22892=ORIENTED_EDGE('',*,*,#16412,.T.);
#22893=ORIENTED_EDGE('',*,*,#16414,.T.);
#22894=ORIENTED_EDGE('',*,*,#16406,.T.);
#22895=ORIENTED_EDGE('',*,*,#16410,.T.);
#22896=ORIENTED_EDGE('',*,*,#16421,.T.);
#22897=ORIENTED_EDGE('',*,*,#16423,.T.);
#22898=ORIENTED_EDGE('',*,*,#16415,.T.);
#22899=ORIENTED_EDGE('',*,*,#16419,.T.);
#22900=ORIENTED_EDGE('',*,*,#16430,.T.);
#22901=ORIENTED_EDGE('',*,*,#16432,.T.);
#22902=ORIENTED_EDGE('',*,*,#16424,.T.);
#22903=ORIENTED_EDGE('',*,*,#16428,.T.);
#22904=ORIENTED_EDGE('',*,*,#16439,.T.);
#22905=ORIENTED_EDGE('',*,*,#16441,.T.);
#22906=ORIENTED_EDGE('',*,*,#16433,.T.);
#22907=ORIENTED_EDGE('',*,*,#16437,.T.);
#22908=ORIENTED_EDGE('',*,*,#16448,.T.);
#22909=ORIENTED_EDGE('',*,*,#16450,.T.);
#22910=ORIENTED_EDGE('',*,*,#16442,.T.);
#22911=ORIENTED_EDGE('',*,*,#16446,.T.);
#22912=ORIENTED_EDGE('',*,*,#16457,.T.);
#22913=ORIENTED_EDGE('',*,*,#16459,.T.);
#22914=ORIENTED_EDGE('',*,*,#16451,.T.);
#22915=ORIENTED_EDGE('',*,*,#16455,.T.);
#22916=ORIENTED_EDGE('',*,*,#16466,.T.);
#22917=ORIENTED_EDGE('',*,*,#16468,.T.);
#22918=ORIENTED_EDGE('',*,*,#16460,.T.);
#22919=ORIENTED_EDGE('',*,*,#16464,.T.);
#22920=ORIENTED_EDGE('',*,*,#16475,.T.);
#22921=ORIENTED_EDGE('',*,*,#16477,.T.);
#22922=ORIENTED_EDGE('',*,*,#16469,.T.);
#22923=ORIENTED_EDGE('',*,*,#16473,.T.);
#22924=ORIENTED_EDGE('',*,*,#16484,.T.);
#22925=ORIENTED_EDGE('',*,*,#16486,.T.);
#22926=ORIENTED_EDGE('',*,*,#16478,.T.);
#22927=ORIENTED_EDGE('',*,*,#16482,.T.);
#22928=ORIENTED_EDGE('',*,*,#16493,.T.);
#22929=ORIENTED_EDGE('',*,*,#16495,.T.);
#22930=ORIENTED_EDGE('',*,*,#16487,.T.);
#22931=ORIENTED_EDGE('',*,*,#16491,.T.);
#22932=ORIENTED_EDGE('',*,*,#16502,.T.);
#22933=ORIENTED_EDGE('',*,*,#16504,.T.);
#22934=ORIENTED_EDGE('',*,*,#16496,.T.);
#22935=ORIENTED_EDGE('',*,*,#16500,.T.);
#22936=ORIENTED_EDGE('',*,*,#16511,.T.);
#22937=ORIENTED_EDGE('',*,*,#16513,.T.);
#22938=ORIENTED_EDGE('',*,*,#16505,.T.);
#22939=ORIENTED_EDGE('',*,*,#16509,.T.);
#22940=ORIENTED_EDGE('',*,*,#16520,.T.);
#22941=ORIENTED_EDGE('',*,*,#16522,.T.);
#22942=ORIENTED_EDGE('',*,*,#16514,.T.);
#22943=ORIENTED_EDGE('',*,*,#16518,.T.);
#22944=ORIENTED_EDGE('',*,*,#16540,.T.);
#22945=ORIENTED_EDGE('',*,*,#16542,.T.);
#22946=ORIENTED_EDGE('',*,*,#16534,.T.);
#22947=ORIENTED_EDGE('',*,*,#16538,.T.);
#22948=ORIENTED_EDGE('',*,*,#16549,.T.);
#22949=ORIENTED_EDGE('',*,*,#16551,.T.);
#22950=ORIENTED_EDGE('',*,*,#16543,.T.);
#22951=ORIENTED_EDGE('',*,*,#16547,.T.);
#22952=ORIENTED_EDGE('',*,*,#16558,.T.);
#22953=ORIENTED_EDGE('',*,*,#16560,.T.);
#22954=ORIENTED_EDGE('',*,*,#16552,.T.);
#22955=ORIENTED_EDGE('',*,*,#16556,.T.);
#22956=ORIENTED_EDGE('',*,*,#16567,.T.);
#22957=ORIENTED_EDGE('',*,*,#16569,.T.);
#22958=ORIENTED_EDGE('',*,*,#16561,.T.);
#22959=ORIENTED_EDGE('',*,*,#16565,.T.);
#22960=ORIENTED_EDGE('',*,*,#16576,.T.);
#22961=ORIENTED_EDGE('',*,*,#16578,.T.);
#22962=ORIENTED_EDGE('',*,*,#16570,.T.);
#22963=ORIENTED_EDGE('',*,*,#16574,.T.);
#22964=ORIENTED_EDGE('',*,*,#16585,.T.);
#22965=ORIENTED_EDGE('',*,*,#16587,.T.);
#22966=ORIENTED_EDGE('',*,*,#16579,.T.);
#22967=ORIENTED_EDGE('',*,*,#16583,.T.);
#22968=ORIENTED_EDGE('',*,*,#16594,.T.);
#22969=ORIENTED_EDGE('',*,*,#16596,.T.);
#22970=ORIENTED_EDGE('',*,*,#16588,.T.);
#22971=ORIENTED_EDGE('',*,*,#16592,.T.);
#22972=ORIENTED_EDGE('',*,*,#16603,.T.);
#22973=ORIENTED_EDGE('',*,*,#16605,.T.);
#22974=ORIENTED_EDGE('',*,*,#16597,.T.);
#22975=ORIENTED_EDGE('',*,*,#16601,.T.);
#22976=ORIENTED_EDGE('',*,*,#16612,.T.);
#22977=ORIENTED_EDGE('',*,*,#16614,.T.);
#22978=ORIENTED_EDGE('',*,*,#16606,.T.);
#22979=ORIENTED_EDGE('',*,*,#16610,.T.);
#22980=ORIENTED_EDGE('',*,*,#16621,.T.);
#22981=ORIENTED_EDGE('',*,*,#16623,.T.);
#22982=ORIENTED_EDGE('',*,*,#16615,.T.);
#22983=ORIENTED_EDGE('',*,*,#16619,.T.);
#22984=ORIENTED_EDGE('',*,*,#16630,.T.);
#22985=ORIENTED_EDGE('',*,*,#16632,.T.);
#22986=ORIENTED_EDGE('',*,*,#16624,.T.);
#22987=ORIENTED_EDGE('',*,*,#16628,.T.);
#22988=ORIENTED_EDGE('',*,*,#16639,.T.);
#22989=ORIENTED_EDGE('',*,*,#16641,.T.);
#22990=ORIENTED_EDGE('',*,*,#16633,.T.);
#22991=ORIENTED_EDGE('',*,*,#16637,.T.);
#22992=ORIENTED_EDGE('',*,*,#16648,.T.);
#22993=ORIENTED_EDGE('',*,*,#16650,.T.);
#22994=ORIENTED_EDGE('',*,*,#16642,.T.);
#22995=ORIENTED_EDGE('',*,*,#16646,.T.);
#22996=ORIENTED_EDGE('',*,*,#16657,.T.);
#22997=ORIENTED_EDGE('',*,*,#16659,.T.);
#22998=ORIENTED_EDGE('',*,*,#16651,.T.);
#22999=ORIENTED_EDGE('',*,*,#16655,.T.);
#23000=ORIENTED_EDGE('',*,*,#16666,.T.);
#23001=ORIENTED_EDGE('',*,*,#16668,.T.);
#23002=ORIENTED_EDGE('',*,*,#16660,.T.);
#23003=ORIENTED_EDGE('',*,*,#16664,.T.);
#23004=ORIENTED_EDGE('',*,*,#16675,.T.);
#23005=ORIENTED_EDGE('',*,*,#16677,.T.);
#23006=ORIENTED_EDGE('',*,*,#16669,.T.);
#23007=ORIENTED_EDGE('',*,*,#16673,.T.);
#23008=ORIENTED_EDGE('',*,*,#16684,.T.);
#23009=ORIENTED_EDGE('',*,*,#16686,.T.);
#23010=ORIENTED_EDGE('',*,*,#16678,.T.);
#23011=ORIENTED_EDGE('',*,*,#16682,.T.);
#23012=ORIENTED_EDGE('',*,*,#16693,.T.);
#23013=ORIENTED_EDGE('',*,*,#16695,.T.);
#23014=ORIENTED_EDGE('',*,*,#16687,.T.);
#23015=ORIENTED_EDGE('',*,*,#16691,.T.);
#23016=ORIENTED_EDGE('',*,*,#16733,.F.);
#23017=ORIENTED_EDGE('',*,*,#16734,.T.);
#23018=ORIENTED_EDGE('',*,*,#16730,.T.);
#23019=ORIENTED_EDGE('',*,*,#16734,.F.);
#23020=ORIENTED_EDGE('',*,*,#16733,.T.);
#23021=ORIENTED_EDGE('',*,*,#16698,.T.);
#23022=ORIENTED_EDGE('',*,*,#16714,.T.);
#23023=ORIENTED_EDGE('',*,*,#16711,.T.);
#23024=ORIENTED_EDGE('',*,*,#16708,.T.);
#23025=ORIENTED_EDGE('',*,*,#16705,.T.);
#23026=ORIENTED_EDGE('',*,*,#16702,.T.);
#23027=ORIENTED_EDGE('',*,*,#16735,.T.);
#23028=ORIENTED_EDGE('',*,*,#16736,.T.);
#23029=ORIENTED_EDGE('',*,*,#16737,.F.);
#23030=ORIENTED_EDGE('',*,*,#16736,.F.);
#23031=ORIENTED_EDGE('',*,*,#16738,.F.);
#23032=ORIENTED_EDGE('',*,*,#16737,.T.);
#23033=ORIENTED_EDGE('',*,*,#16739,.F.);
#23034=ORIENTED_EDGE('',*,*,#16740,.T.);
#23035=ORIENTED_EDGE('',*,*,#16738,.T.);
#23036=ORIENTED_EDGE('',*,*,#16740,.F.);
#23037=ORIENTED_EDGE('',*,*,#16739,.T.);
#23038=ORIENTED_EDGE('',*,*,#16735,.F.);
#23039=ORIENTED_EDGE('',*,*,#16741,.T.);
#23040=ORIENTED_EDGE('',*,*,#16741,.F.);
#23041=ORIENTED_EDGE('',*,*,#16742,.F.);
#23042=ORIENTED_EDGE('',*,*,#16743,.F.);
#23043=ORIENTED_EDGE('',*,*,#16744,.T.);
#23044=ORIENTED_EDGE('',*,*,#16742,.T.);
#23045=ORIENTED_EDGE('',*,*,#16744,.F.);
#23046=ORIENTED_EDGE('',*,*,#16745,.F.);
#23047=ORIENTED_EDGE('',*,*,#16746,.T.);
#23048=ORIENTED_EDGE('',*,*,#16743,.T.);
#23049=ORIENTED_EDGE('',*,*,#16746,.F.);
#23050=ORIENTED_EDGE('',*,*,#16747,.F.);
#23051=ORIENTED_EDGE('',*,*,#16748,.T.);
#23052=ORIENTED_EDGE('',*,*,#16745,.T.);
#23053=ORIENTED_EDGE('',*,*,#16748,.F.);
#23054=ORIENTED_EDGE('',*,*,#16747,.T.);
#23055=ORIENTED_EDGE('',*,*,#16749,.T.);
#23056=ORIENTED_EDGE('',*,*,#16750,.T.);
#23057=ORIENTED_EDGE('',*,*,#16751,.F.);
#23058=ORIENTED_EDGE('',*,*,#16750,.F.);
#23059=ORIENTED_EDGE('',*,*,#16751,.T.);
#23060=ORIENTED_EDGE('',*,*,#16749,.F.);
#23061=ORIENTED_EDGE('',*,*,#16752,.T.);
#23062=ORIENTED_EDGE('',*,*,#16753,.T.);
#23063=ORIENTED_EDGE('',*,*,#16754,.T.);
#23064=ORIENTED_EDGE('',*,*,#16755,.T.);
#23065=ORIENTED_EDGE('',*,*,#16753,.F.);
#23066=ORIENTED_EDGE('',*,*,#16754,.F.);
#23067=ORIENTED_EDGE('',*,*,#16755,.F.);
#23068=ORIENTED_EDGE('',*,*,#16756,.T.);
#23069=ORIENTED_EDGE('',*,*,#16757,.T.);
#23070=ORIENTED_EDGE('',*,*,#16756,.F.);
#23071=ORIENTED_EDGE('',*,*,#16752,.F.);
#23072=ORIENTED_EDGE('',*,*,#16758,.F.);
#23073=ORIENTED_EDGE('',*,*,#16758,.T.);
#23074=ORIENTED_EDGE('',*,*,#16759,.T.);
#23075=ORIENTED_EDGE('',*,*,#16760,.F.);
#23076=ORIENTED_EDGE('',*,*,#16759,.F.);
#23077=ORIENTED_EDGE('',*,*,#16761,.F.);
#23078=ORIENTED_EDGE('',*,*,#16760,.T.);
#23079=ORIENTED_EDGE('',*,*,#16757,.F.);
#23080=ORIENTED_EDGE('',*,*,#16762,.T.);
#23081=ORIENTED_EDGE('',*,*,#16761,.T.);
#23082=ORIENTED_EDGE('',*,*,#16762,.F.);
#23083=ORIENTED_EDGE('',*,*,#16763,.F.);
#23084=ORIENTED_EDGE('',*,*,#16764,.T.);
#23085=ORIENTED_EDGE('',*,*,#16765,.T.);
#23086=ORIENTED_EDGE('',*,*,#16766,.T.);
#23087=ORIENTED_EDGE('',*,*,#16767,.F.);
#23088=ORIENTED_EDGE('',*,*,#16768,.T.);
#23089=ORIENTED_EDGE('',*,*,#16763,.T.);
#23090=ORIENTED_EDGE('',*,*,#16769,.T.);
#23091=ORIENTED_EDGE('',*,*,#16770,.F.);
#23092=ORIENTED_EDGE('',*,*,#16771,.T.);
#23093=ORIENTED_EDGE('',*,*,#16767,.T.);
#23094=ORIENTED_EDGE('',*,*,#16772,.T.);
#23095=ORIENTED_EDGE('',*,*,#16773,.F.);
#23096=ORIENTED_EDGE('',*,*,#16774,.T.);
#23097=ORIENTED_EDGE('',*,*,#16770,.T.);
#23098=ORIENTED_EDGE('',*,*,#16775,.T.);
#23099=ORIENTED_EDGE('',*,*,#16776,.F.);
#23100=ORIENTED_EDGE('',*,*,#16777,.T.);
#23101=ORIENTED_EDGE('',*,*,#16773,.T.);
#23102=ORIENTED_EDGE('',*,*,#16778,.T.);
#23103=ORIENTED_EDGE('',*,*,#16779,.F.);
#23104=ORIENTED_EDGE('',*,*,#16780,.T.);
#23105=ORIENTED_EDGE('',*,*,#16776,.T.);
#23106=ORIENTED_EDGE('',*,*,#16781,.T.);
#23107=ORIENTED_EDGE('',*,*,#16782,.F.);
#23108=ORIENTED_EDGE('',*,*,#16783,.T.);
#23109=ORIENTED_EDGE('',*,*,#16779,.T.);
#23110=ORIENTED_EDGE('',*,*,#16784,.T.);
#23111=ORIENTED_EDGE('',*,*,#16785,.F.);
#23112=ORIENTED_EDGE('',*,*,#16786,.T.);
#23113=ORIENTED_EDGE('',*,*,#16782,.T.);
#23114=ORIENTED_EDGE('',*,*,#16787,.T.);
#23115=ORIENTED_EDGE('',*,*,#16788,.F.);
#23116=ORIENTED_EDGE('',*,*,#16789,.T.);
#23117=ORIENTED_EDGE('',*,*,#16785,.T.);
#23118=ORIENTED_EDGE('',*,*,#16790,.T.);
#23119=ORIENTED_EDGE('',*,*,#16791,.F.);
#23120=ORIENTED_EDGE('',*,*,#16792,.T.);
#23121=ORIENTED_EDGE('',*,*,#16788,.T.);
#23122=ORIENTED_EDGE('',*,*,#16793,.T.);
#23123=ORIENTED_EDGE('',*,*,#16794,.F.);
#23124=ORIENTED_EDGE('',*,*,#16795,.T.);
#23125=ORIENTED_EDGE('',*,*,#16791,.T.);
#23126=ORIENTED_EDGE('',*,*,#16796,.T.);
#23127=ORIENTED_EDGE('',*,*,#16797,.F.);
#23128=ORIENTED_EDGE('',*,*,#16798,.T.);
#23129=ORIENTED_EDGE('',*,*,#16794,.T.);
#23130=ORIENTED_EDGE('',*,*,#16799,.T.);
#23131=ORIENTED_EDGE('',*,*,#16800,.F.);
#23132=ORIENTED_EDGE('',*,*,#16801,.T.);
#23133=ORIENTED_EDGE('',*,*,#16797,.T.);
#23134=ORIENTED_EDGE('',*,*,#16802,.T.);
#23135=ORIENTED_EDGE('',*,*,#16803,.F.);
#23136=ORIENTED_EDGE('',*,*,#16804,.T.);
#23137=ORIENTED_EDGE('',*,*,#16800,.T.);
#23138=ORIENTED_EDGE('',*,*,#16805,.T.);
#23139=ORIENTED_EDGE('',*,*,#16806,.F.);
#23140=ORIENTED_EDGE('',*,*,#16807,.T.);
#23141=ORIENTED_EDGE('',*,*,#16803,.T.);
#23142=ORIENTED_EDGE('',*,*,#16808,.T.);
#23143=ORIENTED_EDGE('',*,*,#16809,.F.);
#23144=ORIENTED_EDGE('',*,*,#16810,.T.);
#23145=ORIENTED_EDGE('',*,*,#16806,.T.);
#23146=ORIENTED_EDGE('',*,*,#16811,.T.);
#23147=ORIENTED_EDGE('',*,*,#16812,.F.);
#23148=ORIENTED_EDGE('',*,*,#16813,.T.);
#23149=ORIENTED_EDGE('',*,*,#16809,.T.);
#23150=ORIENTED_EDGE('',*,*,#16814,.T.);
#23151=ORIENTED_EDGE('',*,*,#16815,.F.);
#23152=ORIENTED_EDGE('',*,*,#16816,.T.);
#23153=ORIENTED_EDGE('',*,*,#16812,.T.);
#23154=ORIENTED_EDGE('',*,*,#16817,.T.);
#23155=ORIENTED_EDGE('',*,*,#16818,.F.);
#23156=ORIENTED_EDGE('',*,*,#16819,.T.);
#23157=ORIENTED_EDGE('',*,*,#16815,.T.);
#23158=ORIENTED_EDGE('',*,*,#16820,.T.);
#23159=ORIENTED_EDGE('',*,*,#16821,.F.);
#23160=ORIENTED_EDGE('',*,*,#16822,.T.);
#23161=ORIENTED_EDGE('',*,*,#16818,.T.);
#23162=ORIENTED_EDGE('',*,*,#16823,.T.);
#23163=ORIENTED_EDGE('',*,*,#16824,.F.);
#23164=ORIENTED_EDGE('',*,*,#16825,.T.);
#23165=ORIENTED_EDGE('',*,*,#16821,.T.);
#23166=ORIENTED_EDGE('',*,*,#16826,.T.);
#23167=ORIENTED_EDGE('',*,*,#16827,.F.);
#23168=ORIENTED_EDGE('',*,*,#16828,.T.);
#23169=ORIENTED_EDGE('',*,*,#16824,.T.);
#23170=ORIENTED_EDGE('',*,*,#16829,.T.);
#23171=ORIENTED_EDGE('',*,*,#16830,.F.);
#23172=ORIENTED_EDGE('',*,*,#16831,.T.);
#23173=ORIENTED_EDGE('',*,*,#16827,.T.);
#23174=ORIENTED_EDGE('',*,*,#16832,.T.);
#23175=ORIENTED_EDGE('',*,*,#16833,.F.);
#23176=ORIENTED_EDGE('',*,*,#16834,.T.);
#23177=ORIENTED_EDGE('',*,*,#16830,.T.);
#23178=ORIENTED_EDGE('',*,*,#16835,.T.);
#23179=ORIENTED_EDGE('',*,*,#16836,.F.);
#23180=ORIENTED_EDGE('',*,*,#16837,.T.);
#23181=ORIENTED_EDGE('',*,*,#16833,.T.);
#23182=ORIENTED_EDGE('',*,*,#16838,.T.);
#23183=ORIENTED_EDGE('',*,*,#16839,.F.);
#23184=ORIENTED_EDGE('',*,*,#16840,.T.);
#23185=ORIENTED_EDGE('',*,*,#16836,.T.);
#23186=ORIENTED_EDGE('',*,*,#16841,.T.);
#23187=ORIENTED_EDGE('',*,*,#16842,.F.);
#23188=ORIENTED_EDGE('',*,*,#16843,.T.);
#23189=ORIENTED_EDGE('',*,*,#16839,.T.);
#23190=ORIENTED_EDGE('',*,*,#16844,.T.);
#23191=ORIENTED_EDGE('',*,*,#16845,.F.);
#23192=ORIENTED_EDGE('',*,*,#16846,.T.);
#23193=ORIENTED_EDGE('',*,*,#16842,.T.);
#23194=ORIENTED_EDGE('',*,*,#16847,.T.);
#23195=ORIENTED_EDGE('',*,*,#16848,.F.);
#23196=ORIENTED_EDGE('',*,*,#16849,.T.);
#23197=ORIENTED_EDGE('',*,*,#16845,.T.);
#23198=ORIENTED_EDGE('',*,*,#16850,.T.);
#23199=ORIENTED_EDGE('',*,*,#16851,.F.);
#23200=ORIENTED_EDGE('',*,*,#16852,.T.);
#23201=ORIENTED_EDGE('',*,*,#16848,.T.);
#23202=ORIENTED_EDGE('',*,*,#16853,.T.);
#23203=ORIENTED_EDGE('',*,*,#16854,.F.);
#23204=ORIENTED_EDGE('',*,*,#16855,.T.);
#23205=ORIENTED_EDGE('',*,*,#16851,.T.);
#23206=ORIENTED_EDGE('',*,*,#16856,.T.);
#23207=ORIENTED_EDGE('',*,*,#16857,.F.);
#23208=ORIENTED_EDGE('',*,*,#16858,.T.);
#23209=ORIENTED_EDGE('',*,*,#16854,.T.);
#23210=ORIENTED_EDGE('',*,*,#16859,.T.);
#23211=ORIENTED_EDGE('',*,*,#16860,.F.);
#23212=ORIENTED_EDGE('',*,*,#16861,.T.);
#23213=ORIENTED_EDGE('',*,*,#16857,.T.);
#23214=ORIENTED_EDGE('',*,*,#16862,.T.);
#23215=ORIENTED_EDGE('',*,*,#16863,.F.);
#23216=ORIENTED_EDGE('',*,*,#16864,.T.);
#23217=ORIENTED_EDGE('',*,*,#16860,.T.);
#23218=ORIENTED_EDGE('',*,*,#16865,.T.);
#23219=ORIENTED_EDGE('',*,*,#16866,.F.);
#23220=ORIENTED_EDGE('',*,*,#16867,.T.);
#23221=ORIENTED_EDGE('',*,*,#16863,.T.);
#23222=ORIENTED_EDGE('',*,*,#16868,.T.);
#23223=ORIENTED_EDGE('',*,*,#16869,.F.);
#23224=ORIENTED_EDGE('',*,*,#16870,.T.);
#23225=ORIENTED_EDGE('',*,*,#16866,.T.);
#23226=ORIENTED_EDGE('',*,*,#16871,.T.);
#23227=ORIENTED_EDGE('',*,*,#16872,.F.);
#23228=ORIENTED_EDGE('',*,*,#16873,.T.);
#23229=ORIENTED_EDGE('',*,*,#16869,.T.);
#23230=ORIENTED_EDGE('',*,*,#16874,.T.);
#23231=ORIENTED_EDGE('',*,*,#16875,.F.);
#23232=ORIENTED_EDGE('',*,*,#16876,.T.);
#23233=ORIENTED_EDGE('',*,*,#16872,.T.);
#23234=ORIENTED_EDGE('',*,*,#16877,.T.);
#23235=ORIENTED_EDGE('',*,*,#16878,.F.);
#23236=ORIENTED_EDGE('',*,*,#16879,.T.);
#23237=ORIENTED_EDGE('',*,*,#16875,.T.);
#23238=ORIENTED_EDGE('',*,*,#16880,.T.);
#23239=ORIENTED_EDGE('',*,*,#16881,.F.);
#23240=ORIENTED_EDGE('',*,*,#16882,.T.);
#23241=ORIENTED_EDGE('',*,*,#16878,.T.);
#23242=ORIENTED_EDGE('',*,*,#16883,.T.);
#23243=ORIENTED_EDGE('',*,*,#16884,.F.);
#23244=ORIENTED_EDGE('',*,*,#16885,.T.);
#23245=ORIENTED_EDGE('',*,*,#16881,.T.);
#23246=ORIENTED_EDGE('',*,*,#16886,.T.);
#23247=ORIENTED_EDGE('',*,*,#16887,.F.);
#23248=ORIENTED_EDGE('',*,*,#16888,.T.);
#23249=ORIENTED_EDGE('',*,*,#16884,.T.);
#23250=ORIENTED_EDGE('',*,*,#16889,.T.);
#23251=ORIENTED_EDGE('',*,*,#16890,.F.);
#23252=ORIENTED_EDGE('',*,*,#16891,.T.);
#23253=ORIENTED_EDGE('',*,*,#16892,.F.);
#23254=ORIENTED_EDGE('',*,*,#16893,.F.);
#23255=ORIENTED_EDGE('',*,*,#16894,.F.);
#23256=ORIENTED_EDGE('',*,*,#16895,.T.);
#23257=ORIENTED_EDGE('',*,*,#16890,.T.);
#23258=ORIENTED_EDGE('',*,*,#16896,.F.);
#23259=ORIENTED_EDGE('',*,*,#16897,.F.);
#23260=ORIENTED_EDGE('',*,*,#16898,.T.);
#23261=ORIENTED_EDGE('',*,*,#16894,.T.);
#23262=ORIENTED_EDGE('',*,*,#16899,.F.);
#23263=ORIENTED_EDGE('',*,*,#16900,.F.);
#23264=ORIENTED_EDGE('',*,*,#16901,.T.);
#23265=ORIENTED_EDGE('',*,*,#16897,.T.);
#23266=ORIENTED_EDGE('',*,*,#16902,.F.);
#23267=ORIENTED_EDGE('',*,*,#16903,.F.);
#23268=ORIENTED_EDGE('',*,*,#16904,.T.);
#23269=ORIENTED_EDGE('',*,*,#16900,.T.);
#23270=ORIENTED_EDGE('',*,*,#16905,.F.);
#23271=ORIENTED_EDGE('',*,*,#16906,.F.);
#23272=ORIENTED_EDGE('',*,*,#16907,.T.);
#23273=ORIENTED_EDGE('',*,*,#16903,.T.);
#23274=ORIENTED_EDGE('',*,*,#16908,.F.);
#23275=ORIENTED_EDGE('',*,*,#16909,.F.);
#23276=ORIENTED_EDGE('',*,*,#16910,.T.);
#23277=ORIENTED_EDGE('',*,*,#16906,.T.);
#23278=ORIENTED_EDGE('',*,*,#16911,.F.);
#23279=ORIENTED_EDGE('',*,*,#16912,.F.);
#23280=ORIENTED_EDGE('',*,*,#16913,.T.);
#23281=ORIENTED_EDGE('',*,*,#16909,.T.);
#23282=ORIENTED_EDGE('',*,*,#16914,.F.);
#23283=ORIENTED_EDGE('',*,*,#16915,.F.);
#23284=ORIENTED_EDGE('',*,*,#16916,.T.);
#23285=ORIENTED_EDGE('',*,*,#16912,.T.);
#23286=ORIENTED_EDGE('',*,*,#16917,.F.);
#23287=ORIENTED_EDGE('',*,*,#16918,.F.);
#23288=ORIENTED_EDGE('',*,*,#16919,.T.);
#23289=ORIENTED_EDGE('',*,*,#16915,.T.);
#23290=ORIENTED_EDGE('',*,*,#16920,.F.);
#23291=ORIENTED_EDGE('',*,*,#16921,.F.);
#23292=ORIENTED_EDGE('',*,*,#16922,.T.);
#23293=ORIENTED_EDGE('',*,*,#16918,.T.);
#23294=ORIENTED_EDGE('',*,*,#16923,.F.);
#23295=ORIENTED_EDGE('',*,*,#16924,.F.);
#23296=ORIENTED_EDGE('',*,*,#16925,.T.);
#23297=ORIENTED_EDGE('',*,*,#16921,.T.);
#23298=ORIENTED_EDGE('',*,*,#16926,.F.);
#23299=ORIENTED_EDGE('',*,*,#16927,.F.);
#23300=ORIENTED_EDGE('',*,*,#16928,.T.);
#23301=ORIENTED_EDGE('',*,*,#16924,.T.);
#23302=ORIENTED_EDGE('',*,*,#16929,.F.);
#23303=ORIENTED_EDGE('',*,*,#16930,.F.);
#23304=ORIENTED_EDGE('',*,*,#16931,.T.);
#23305=ORIENTED_EDGE('',*,*,#16927,.T.);
#23306=ORIENTED_EDGE('',*,*,#16932,.F.);
#23307=ORIENTED_EDGE('',*,*,#16933,.F.);
#23308=ORIENTED_EDGE('',*,*,#16934,.T.);
#23309=ORIENTED_EDGE('',*,*,#16930,.T.);
#23310=ORIENTED_EDGE('',*,*,#16935,.F.);
#23311=ORIENTED_EDGE('',*,*,#16936,.F.);
#23312=ORIENTED_EDGE('',*,*,#16937,.T.);
#23313=ORIENTED_EDGE('',*,*,#16933,.T.);
#23314=ORIENTED_EDGE('',*,*,#16938,.F.);
#23315=ORIENTED_EDGE('',*,*,#16939,.F.);
#23316=ORIENTED_EDGE('',*,*,#16940,.T.);
#23317=ORIENTED_EDGE('',*,*,#16936,.T.);
#23318=ORIENTED_EDGE('',*,*,#16941,.F.);
#23319=ORIENTED_EDGE('',*,*,#16942,.F.);
#23320=ORIENTED_EDGE('',*,*,#16943,.T.);
#23321=ORIENTED_EDGE('',*,*,#16939,.T.);
#23322=ORIENTED_EDGE('',*,*,#16944,.F.);
#23323=ORIENTED_EDGE('',*,*,#16945,.F.);
#23324=ORIENTED_EDGE('',*,*,#16946,.T.);
#23325=ORIENTED_EDGE('',*,*,#16942,.T.);
#23326=ORIENTED_EDGE('',*,*,#16947,.F.);
#23327=ORIENTED_EDGE('',*,*,#16948,.F.);
#23328=ORIENTED_EDGE('',*,*,#16949,.T.);
#23329=ORIENTED_EDGE('',*,*,#16945,.T.);
#23330=ORIENTED_EDGE('',*,*,#16950,.F.);
#23331=ORIENTED_EDGE('',*,*,#16951,.F.);
#23332=ORIENTED_EDGE('',*,*,#16952,.T.);
#23333=ORIENTED_EDGE('',*,*,#16948,.T.);
#23334=ORIENTED_EDGE('',*,*,#16953,.F.);
#23335=ORIENTED_EDGE('',*,*,#16954,.F.);
#23336=ORIENTED_EDGE('',*,*,#16955,.T.);
#23337=ORIENTED_EDGE('',*,*,#16951,.T.);
#23338=ORIENTED_EDGE('',*,*,#16956,.F.);
#23339=ORIENTED_EDGE('',*,*,#16957,.F.);
#23340=ORIENTED_EDGE('',*,*,#16958,.T.);
#23341=ORIENTED_EDGE('',*,*,#16954,.T.);
#23342=ORIENTED_EDGE('',*,*,#16959,.F.);
#23343=ORIENTED_EDGE('',*,*,#16960,.F.);
#23344=ORIENTED_EDGE('',*,*,#16961,.T.);
#23345=ORIENTED_EDGE('',*,*,#16957,.T.);
#23346=ORIENTED_EDGE('',*,*,#16962,.F.);
#23347=ORIENTED_EDGE('',*,*,#16963,.F.);
#23348=ORIENTED_EDGE('',*,*,#16964,.T.);
#23349=ORIENTED_EDGE('',*,*,#16960,.T.);
#23350=ORIENTED_EDGE('',*,*,#16965,.F.);
#23351=ORIENTED_EDGE('',*,*,#16966,.F.);
#23352=ORIENTED_EDGE('',*,*,#16967,.T.);
#23353=ORIENTED_EDGE('',*,*,#16963,.T.);
#23354=ORIENTED_EDGE('',*,*,#16968,.F.);
#23355=ORIENTED_EDGE('',*,*,#16969,.F.);
#23356=ORIENTED_EDGE('',*,*,#16970,.T.);
#23357=ORIENTED_EDGE('',*,*,#16966,.T.);
#23358=ORIENTED_EDGE('',*,*,#16971,.F.);
#23359=ORIENTED_EDGE('',*,*,#16972,.F.);
#23360=ORIENTED_EDGE('',*,*,#16973,.T.);
#23361=ORIENTED_EDGE('',*,*,#16969,.T.);
#23362=ORIENTED_EDGE('',*,*,#16974,.F.);
#23363=ORIENTED_EDGE('',*,*,#16975,.F.);
#23364=ORIENTED_EDGE('',*,*,#16976,.T.);
#23365=ORIENTED_EDGE('',*,*,#16972,.T.);
#23366=ORIENTED_EDGE('',*,*,#16977,.F.);
#23367=ORIENTED_EDGE('',*,*,#16978,.F.);
#23368=ORIENTED_EDGE('',*,*,#16979,.T.);
#23369=ORIENTED_EDGE('',*,*,#16975,.T.);
#23370=ORIENTED_EDGE('',*,*,#16980,.F.);
#23371=ORIENTED_EDGE('',*,*,#16981,.F.);
#23372=ORIENTED_EDGE('',*,*,#16982,.T.);
#23373=ORIENTED_EDGE('',*,*,#16978,.T.);
#23374=ORIENTED_EDGE('',*,*,#16983,.F.);
#23375=ORIENTED_EDGE('',*,*,#16984,.F.);
#23376=ORIENTED_EDGE('',*,*,#16985,.T.);
#23377=ORIENTED_EDGE('',*,*,#16981,.T.);
#23378=ORIENTED_EDGE('',*,*,#16986,.F.);
#23379=ORIENTED_EDGE('',*,*,#16987,.F.);
#23380=ORIENTED_EDGE('',*,*,#16988,.T.);
#23381=ORIENTED_EDGE('',*,*,#16984,.T.);
#23382=ORIENTED_EDGE('',*,*,#16989,.F.);
#23383=ORIENTED_EDGE('',*,*,#16990,.F.);
#23384=ORIENTED_EDGE('',*,*,#16991,.T.);
#23385=ORIENTED_EDGE('',*,*,#16987,.T.);
#23386=ORIENTED_EDGE('',*,*,#16992,.F.);
#23387=ORIENTED_EDGE('',*,*,#16993,.F.);
#23388=ORIENTED_EDGE('',*,*,#16994,.T.);
#23389=ORIENTED_EDGE('',*,*,#16990,.T.);
#23390=ORIENTED_EDGE('',*,*,#16995,.F.);
#23391=ORIENTED_EDGE('',*,*,#16996,.F.);
#23392=ORIENTED_EDGE('',*,*,#16997,.T.);
#23393=ORIENTED_EDGE('',*,*,#16993,.T.);
#23394=ORIENTED_EDGE('',*,*,#16998,.F.);
#23395=ORIENTED_EDGE('',*,*,#16999,.F.);
#23396=ORIENTED_EDGE('',*,*,#17000,.T.);
#23397=ORIENTED_EDGE('',*,*,#16996,.T.);
#23398=ORIENTED_EDGE('',*,*,#17001,.F.);
#23399=ORIENTED_EDGE('',*,*,#17002,.F.);
#23400=ORIENTED_EDGE('',*,*,#17003,.T.);
#23401=ORIENTED_EDGE('',*,*,#16999,.T.);
#23402=ORIENTED_EDGE('',*,*,#17004,.F.);
#23403=ORIENTED_EDGE('',*,*,#17005,.F.);
#23404=ORIENTED_EDGE('',*,*,#17006,.T.);
#23405=ORIENTED_EDGE('',*,*,#17002,.T.);
#23406=ORIENTED_EDGE('',*,*,#17007,.F.);
#23407=ORIENTED_EDGE('',*,*,#17008,.F.);
#23408=ORIENTED_EDGE('',*,*,#17009,.T.);
#23409=ORIENTED_EDGE('',*,*,#17005,.T.);
#23410=ORIENTED_EDGE('',*,*,#17010,.F.);
#23411=ORIENTED_EDGE('',*,*,#17011,.F.);
#23412=ORIENTED_EDGE('',*,*,#17012,.T.);
#23413=ORIENTED_EDGE('',*,*,#17008,.T.);
#23414=ORIENTED_EDGE('',*,*,#17013,.F.);
#23415=ORIENTED_EDGE('',*,*,#17014,.F.);
#23416=ORIENTED_EDGE('',*,*,#17015,.T.);
#23417=ORIENTED_EDGE('',*,*,#17011,.T.);
#23418=ORIENTED_EDGE('',*,*,#17016,.F.);
#23419=ORIENTED_EDGE('',*,*,#16892,.T.);
#23420=ORIENTED_EDGE('',*,*,#17017,.T.);
#23421=ORIENTED_EDGE('',*,*,#17018,.F.);
#23422=ORIENTED_EDGE('',*,*,#17019,.T.);
#23423=ORIENTED_EDGE('',*,*,#17019,.F.);
#23424=ORIENTED_EDGE('',*,*,#17020,.F.);
#23425=ORIENTED_EDGE('',*,*,#16889,.F.);
#23426=ORIENTED_EDGE('',*,*,#16886,.F.);
#23427=ORIENTED_EDGE('',*,*,#16883,.F.);
#23428=ORIENTED_EDGE('',*,*,#16880,.F.);
#23429=ORIENTED_EDGE('',*,*,#16877,.F.);
#23430=ORIENTED_EDGE('',*,*,#16874,.F.);
#23431=ORIENTED_EDGE('',*,*,#16871,.F.);
#23432=ORIENTED_EDGE('',*,*,#16868,.F.);
#23433=ORIENTED_EDGE('',*,*,#16865,.F.);
#23434=ORIENTED_EDGE('',*,*,#16862,.F.);
#23435=ORIENTED_EDGE('',*,*,#16859,.F.);
#23436=ORIENTED_EDGE('',*,*,#16856,.F.);
#23437=ORIENTED_EDGE('',*,*,#16853,.F.);
#23438=ORIENTED_EDGE('',*,*,#16850,.F.);
#23439=ORIENTED_EDGE('',*,*,#16847,.F.);
#23440=ORIENTED_EDGE('',*,*,#16844,.F.);
#23441=ORIENTED_EDGE('',*,*,#16841,.F.);
#23442=ORIENTED_EDGE('',*,*,#16838,.F.);
#23443=ORIENTED_EDGE('',*,*,#16835,.F.);
#23444=ORIENTED_EDGE('',*,*,#16832,.F.);
#23445=ORIENTED_EDGE('',*,*,#16829,.F.);
#23446=ORIENTED_EDGE('',*,*,#16826,.F.);
#23447=ORIENTED_EDGE('',*,*,#16823,.F.);
#23448=ORIENTED_EDGE('',*,*,#16820,.F.);
#23449=ORIENTED_EDGE('',*,*,#16817,.F.);
#23450=ORIENTED_EDGE('',*,*,#16814,.F.);
#23451=ORIENTED_EDGE('',*,*,#16811,.F.);
#23452=ORIENTED_EDGE('',*,*,#16808,.F.);
#23453=ORIENTED_EDGE('',*,*,#16805,.F.);
#23454=ORIENTED_EDGE('',*,*,#16802,.F.);
#23455=ORIENTED_EDGE('',*,*,#16799,.F.);
#23456=ORIENTED_EDGE('',*,*,#16796,.F.);
#23457=ORIENTED_EDGE('',*,*,#16793,.F.);
#23458=ORIENTED_EDGE('',*,*,#16790,.F.);
#23459=ORIENTED_EDGE('',*,*,#16787,.F.);
#23460=ORIENTED_EDGE('',*,*,#16784,.F.);
#23461=ORIENTED_EDGE('',*,*,#16781,.F.);
#23462=ORIENTED_EDGE('',*,*,#16778,.F.);
#23463=ORIENTED_EDGE('',*,*,#16775,.F.);
#23464=ORIENTED_EDGE('',*,*,#16772,.F.);
#23465=ORIENTED_EDGE('',*,*,#16769,.F.);
#23466=ORIENTED_EDGE('',*,*,#16766,.F.);
#23467=ORIENTED_EDGE('',*,*,#17021,.F.);
#23468=ORIENTED_EDGE('',*,*,#17022,.T.);
#23469=ORIENTED_EDGE('',*,*,#17016,.T.);
#23470=ORIENTED_EDGE('',*,*,#17013,.T.);
#23471=ORIENTED_EDGE('',*,*,#17010,.T.);
#23472=ORIENTED_EDGE('',*,*,#17007,.T.);
#23473=ORIENTED_EDGE('',*,*,#17004,.T.);
#23474=ORIENTED_EDGE('',*,*,#17001,.T.);
#23475=ORIENTED_EDGE('',*,*,#16998,.T.);
#23476=ORIENTED_EDGE('',*,*,#16995,.T.);
#23477=ORIENTED_EDGE('',*,*,#16992,.T.);
#23478=ORIENTED_EDGE('',*,*,#16989,.T.);
#23479=ORIENTED_EDGE('',*,*,#16986,.T.);
#23480=ORIENTED_EDGE('',*,*,#16983,.T.);
#23481=ORIENTED_EDGE('',*,*,#16980,.T.);
#23482=ORIENTED_EDGE('',*,*,#16977,.T.);
#23483=ORIENTED_EDGE('',*,*,#16974,.T.);
#23484=ORIENTED_EDGE('',*,*,#16971,.T.);
#23485=ORIENTED_EDGE('',*,*,#16968,.T.);
#23486=ORIENTED_EDGE('',*,*,#16965,.T.);
#23487=ORIENTED_EDGE('',*,*,#16962,.T.);
#23488=ORIENTED_EDGE('',*,*,#16959,.T.);
#23489=ORIENTED_EDGE('',*,*,#16956,.T.);
#23490=ORIENTED_EDGE('',*,*,#16953,.T.);
#23491=ORIENTED_EDGE('',*,*,#16950,.T.);
#23492=ORIENTED_EDGE('',*,*,#16947,.T.);
#23493=ORIENTED_EDGE('',*,*,#16944,.T.);
#23494=ORIENTED_EDGE('',*,*,#16941,.T.);
#23495=ORIENTED_EDGE('',*,*,#16938,.T.);
#23496=ORIENTED_EDGE('',*,*,#16935,.T.);
#23497=ORIENTED_EDGE('',*,*,#16932,.T.);
#23498=ORIENTED_EDGE('',*,*,#16929,.T.);
#23499=ORIENTED_EDGE('',*,*,#16926,.T.);
#23500=ORIENTED_EDGE('',*,*,#16923,.T.);
#23501=ORIENTED_EDGE('',*,*,#16920,.T.);
#23502=ORIENTED_EDGE('',*,*,#16917,.T.);
#23503=ORIENTED_EDGE('',*,*,#16914,.T.);
#23504=ORIENTED_EDGE('',*,*,#16911,.T.);
#23505=ORIENTED_EDGE('',*,*,#16908,.T.);
#23506=ORIENTED_EDGE('',*,*,#16905,.T.);
#23507=ORIENTED_EDGE('',*,*,#16902,.T.);
#23508=ORIENTED_EDGE('',*,*,#16899,.T.);
#23509=ORIENTED_EDGE('',*,*,#16896,.T.);
#23510=ORIENTED_EDGE('',*,*,#16893,.T.);
#23511=ORIENTED_EDGE('',*,*,#17023,.T.);
#23512=ORIENTED_EDGE('',*,*,#17024,.T.);
#23513=ORIENTED_EDGE('',*,*,#17025,.T.);
#23514=ORIENTED_EDGE('',*,*,#17026,.T.);
#23515=ORIENTED_EDGE('',*,*,#17021,.T.);
#23516=ORIENTED_EDGE('',*,*,#17014,.T.);
#23517=ORIENTED_EDGE('',*,*,#17022,.F.);
#23518=ORIENTED_EDGE('',*,*,#17026,.F.);
#23519=ORIENTED_EDGE('',*,*,#17027,.T.);
#23520=ORIENTED_EDGE('',*,*,#17017,.F.);
#23521=ORIENTED_EDGE('',*,*,#16891,.F.);
#23522=ORIENTED_EDGE('',*,*,#16895,.F.);
#23523=ORIENTED_EDGE('',*,*,#16898,.F.);
#23524=ORIENTED_EDGE('',*,*,#16901,.F.);
#23525=ORIENTED_EDGE('',*,*,#16904,.F.);
#23526=ORIENTED_EDGE('',*,*,#16907,.F.);
#23527=ORIENTED_EDGE('',*,*,#16910,.F.);
#23528=ORIENTED_EDGE('',*,*,#16913,.F.);
#23529=ORIENTED_EDGE('',*,*,#16916,.F.);
#23530=ORIENTED_EDGE('',*,*,#16919,.F.);
#23531=ORIENTED_EDGE('',*,*,#16922,.F.);
#23532=ORIENTED_EDGE('',*,*,#16925,.F.);
#23533=ORIENTED_EDGE('',*,*,#16928,.F.);
#23534=ORIENTED_EDGE('',*,*,#16931,.F.);
#23535=ORIENTED_EDGE('',*,*,#16934,.F.);
#23536=ORIENTED_EDGE('',*,*,#16937,.F.);
#23537=ORIENTED_EDGE('',*,*,#16940,.F.);
#23538=ORIENTED_EDGE('',*,*,#16943,.F.);
#23539=ORIENTED_EDGE('',*,*,#16946,.F.);
#23540=ORIENTED_EDGE('',*,*,#16949,.F.);
#23541=ORIENTED_EDGE('',*,*,#16952,.F.);
#23542=ORIENTED_EDGE('',*,*,#16955,.F.);
#23543=ORIENTED_EDGE('',*,*,#16958,.F.);
#23544=ORIENTED_EDGE('',*,*,#16961,.F.);
#23545=ORIENTED_EDGE('',*,*,#16964,.F.);
#23546=ORIENTED_EDGE('',*,*,#16967,.F.);
#23547=ORIENTED_EDGE('',*,*,#16970,.F.);
#23548=ORIENTED_EDGE('',*,*,#16973,.F.);
#23549=ORIENTED_EDGE('',*,*,#16976,.F.);
#23550=ORIENTED_EDGE('',*,*,#16979,.F.);
#23551=ORIENTED_EDGE('',*,*,#16982,.F.);
#23552=ORIENTED_EDGE('',*,*,#16985,.F.);
#23553=ORIENTED_EDGE('',*,*,#16988,.F.);
#23554=ORIENTED_EDGE('',*,*,#16991,.F.);
#23555=ORIENTED_EDGE('',*,*,#16994,.F.);
#23556=ORIENTED_EDGE('',*,*,#16997,.F.);
#23557=ORIENTED_EDGE('',*,*,#17000,.F.);
#23558=ORIENTED_EDGE('',*,*,#17003,.F.);
#23559=ORIENTED_EDGE('',*,*,#17006,.F.);
#23560=ORIENTED_EDGE('',*,*,#17009,.F.);
#23561=ORIENTED_EDGE('',*,*,#17012,.F.);
#23562=ORIENTED_EDGE('',*,*,#17015,.F.);
#23563=ORIENTED_EDGE('',*,*,#17027,.F.);
#23564=ORIENTED_EDGE('',*,*,#17025,.F.);
#23565=ORIENTED_EDGE('',*,*,#16764,.F.);
#23566=ORIENTED_EDGE('',*,*,#16768,.F.);
#23567=ORIENTED_EDGE('',*,*,#16771,.F.);
#23568=ORIENTED_EDGE('',*,*,#16774,.F.);
#23569=ORIENTED_EDGE('',*,*,#16777,.F.);
#23570=ORIENTED_EDGE('',*,*,#16780,.F.);
#23571=ORIENTED_EDGE('',*,*,#16783,.F.);
#23572=ORIENTED_EDGE('',*,*,#16786,.F.);
#23573=ORIENTED_EDGE('',*,*,#16789,.F.);
#23574=ORIENTED_EDGE('',*,*,#16792,.F.);
#23575=ORIENTED_EDGE('',*,*,#16795,.F.);
#23576=ORIENTED_EDGE('',*,*,#16798,.F.);
#23577=ORIENTED_EDGE('',*,*,#16801,.F.);
#23578=ORIENTED_EDGE('',*,*,#16804,.F.);
#23579=ORIENTED_EDGE('',*,*,#16807,.F.);
#23580=ORIENTED_EDGE('',*,*,#16810,.F.);
#23581=ORIENTED_EDGE('',*,*,#16813,.F.);
#23582=ORIENTED_EDGE('',*,*,#16816,.F.);
#23583=ORIENTED_EDGE('',*,*,#16819,.F.);
#23584=ORIENTED_EDGE('',*,*,#16822,.F.);
#23585=ORIENTED_EDGE('',*,*,#16825,.F.);
#23586=ORIENTED_EDGE('',*,*,#16828,.F.);
#23587=ORIENTED_EDGE('',*,*,#16831,.F.);
#23588=ORIENTED_EDGE('',*,*,#16834,.F.);
#23589=ORIENTED_EDGE('',*,*,#16837,.F.);
#23590=ORIENTED_EDGE('',*,*,#16840,.F.);
#23591=ORIENTED_EDGE('',*,*,#16843,.F.);
#23592=ORIENTED_EDGE('',*,*,#16846,.F.);
#23593=ORIENTED_EDGE('',*,*,#16849,.F.);
#23594=ORIENTED_EDGE('',*,*,#16852,.F.);
#23595=ORIENTED_EDGE('',*,*,#16855,.F.);
#23596=ORIENTED_EDGE('',*,*,#16858,.F.);
#23597=ORIENTED_EDGE('',*,*,#16861,.F.);
#23598=ORIENTED_EDGE('',*,*,#16864,.F.);
#23599=ORIENTED_EDGE('',*,*,#16867,.F.);
#23600=ORIENTED_EDGE('',*,*,#16870,.F.);
#23601=ORIENTED_EDGE('',*,*,#16873,.F.);
#23602=ORIENTED_EDGE('',*,*,#16876,.F.);
#23603=ORIENTED_EDGE('',*,*,#16879,.F.);
#23604=ORIENTED_EDGE('',*,*,#16882,.F.);
#23605=ORIENTED_EDGE('',*,*,#16885,.F.);
#23606=ORIENTED_EDGE('',*,*,#16888,.F.);
#23607=ORIENTED_EDGE('',*,*,#17028,.F.);
#23608=ORIENTED_EDGE('',*,*,#17018,.T.);
#23609=ORIENTED_EDGE('',*,*,#17029,.T.);
#23610=ORIENTED_EDGE('',*,*,#17030,.T.);
#23611=ORIENTED_EDGE('',*,*,#17031,.T.);
#23612=ORIENTED_EDGE('',*,*,#17030,.F.);
#23613=ORIENTED_EDGE('',*,*,#17032,.T.);
#23614=ORIENTED_EDGE('',*,*,#16887,.T.);
#23615=ORIENTED_EDGE('',*,*,#17020,.T.);
#23616=ORIENTED_EDGE('',*,*,#17032,.F.);
#23617=ORIENTED_EDGE('',*,*,#17029,.F.);
#23618=ORIENTED_EDGE('',*,*,#17028,.T.);
#23619=ORIENTED_EDGE('',*,*,#17033,.F.);
#23620=ORIENTED_EDGE('',*,*,#17031,.F.);
#23621=ORIENTED_EDGE('',*,*,#17034,.F.);
#23622=ORIENTED_EDGE('',*,*,#17035,.T.);
#23623=ORIENTED_EDGE('',*,*,#17036,.F.);
#23624=ORIENTED_EDGE('',*,*,#17037,.F.);
#23625=ORIENTED_EDGE('',*,*,#17038,.F.);
#23626=ORIENTED_EDGE('',*,*,#17037,.T.);
#23627=ORIENTED_EDGE('',*,*,#17039,.T.);
#23628=ORIENTED_EDGE('',*,*,#17040,.F.);
#23629=ORIENTED_EDGE('',*,*,#17039,.F.);
#23630=ORIENTED_EDGE('',*,*,#17036,.T.);
#23631=ORIENTED_EDGE('',*,*,#17041,.T.);
#23632=ORIENTED_EDGE('',*,*,#17042,.F.);
#23633=ORIENTED_EDGE('',*,*,#17041,.F.);
#23634=ORIENTED_EDGE('',*,*,#17035,.F.);
#23635=ORIENTED_EDGE('',*,*,#17043,.F.);
#23636=ORIENTED_EDGE('',*,*,#17044,.T.);
#23637=ORIENTED_EDGE('',*,*,#17045,.F.);
#23638=ORIENTED_EDGE('',*,*,#17046,.F.);
#23639=ORIENTED_EDGE('',*,*,#17047,.F.);
#23640=ORIENTED_EDGE('',*,*,#17046,.T.);
#23641=ORIENTED_EDGE('',*,*,#17048,.T.);
#23642=ORIENTED_EDGE('',*,*,#17049,.F.);
#23643=ORIENTED_EDGE('',*,*,#17048,.F.);
#23644=ORIENTED_EDGE('',*,*,#17045,.T.);
#23645=ORIENTED_EDGE('',*,*,#17050,.T.);
#23646=ORIENTED_EDGE('',*,*,#17051,.F.);
#23647=ORIENTED_EDGE('',*,*,#17050,.F.);
#23648=ORIENTED_EDGE('',*,*,#17044,.F.);
#23649=ORIENTED_EDGE('',*,*,#17052,.F.);
#23650=ORIENTED_EDGE('',*,*,#17053,.T.);
#23651=ORIENTED_EDGE('',*,*,#17054,.F.);
#23652=ORIENTED_EDGE('',*,*,#17055,.F.);
#23653=ORIENTED_EDGE('',*,*,#17056,.F.);
#23654=ORIENTED_EDGE('',*,*,#17055,.T.);
#23655=ORIENTED_EDGE('',*,*,#17057,.T.);
#23656=ORIENTED_EDGE('',*,*,#17058,.F.);
#23657=ORIENTED_EDGE('',*,*,#17057,.F.);
#23658=ORIENTED_EDGE('',*,*,#17054,.T.);
#23659=ORIENTED_EDGE('',*,*,#17059,.T.);
#23660=ORIENTED_EDGE('',*,*,#17060,.F.);
#23661=ORIENTED_EDGE('',*,*,#17059,.F.);
#23662=ORIENTED_EDGE('',*,*,#17053,.F.);
#23663=ORIENTED_EDGE('',*,*,#17061,.F.);
#23664=ORIENTED_EDGE('',*,*,#17062,.T.);
#23665=ORIENTED_EDGE('',*,*,#17063,.F.);
#23666=ORIENTED_EDGE('',*,*,#17064,.F.);
#23667=ORIENTED_EDGE('',*,*,#17065,.F.);
#23668=ORIENTED_EDGE('',*,*,#17064,.T.);
#23669=ORIENTED_EDGE('',*,*,#17066,.T.);
#23670=ORIENTED_EDGE('',*,*,#17067,.F.);
#23671=ORIENTED_EDGE('',*,*,#17066,.F.);
#23672=ORIENTED_EDGE('',*,*,#17063,.T.);
#23673=ORIENTED_EDGE('',*,*,#17068,.T.);
#23674=ORIENTED_EDGE('',*,*,#17069,.F.);
#23675=ORIENTED_EDGE('',*,*,#17068,.F.);
#23676=ORIENTED_EDGE('',*,*,#17062,.F.);
#23677=ORIENTED_EDGE('',*,*,#17070,.F.);
#23678=ORIENTED_EDGE('',*,*,#17071,.T.);
#23679=ORIENTED_EDGE('',*,*,#17072,.F.);
#23680=ORIENTED_EDGE('',*,*,#17073,.F.);
#23681=ORIENTED_EDGE('',*,*,#17074,.F.);
#23682=ORIENTED_EDGE('',*,*,#17073,.T.);
#23683=ORIENTED_EDGE('',*,*,#17075,.T.);
#23684=ORIENTED_EDGE('',*,*,#17076,.F.);
#23685=ORIENTED_EDGE('',*,*,#17075,.F.);
#23686=ORIENTED_EDGE('',*,*,#17072,.T.);
#23687=ORIENTED_EDGE('',*,*,#17077,.T.);
#23688=ORIENTED_EDGE('',*,*,#17078,.F.);
#23689=ORIENTED_EDGE('',*,*,#17077,.F.);
#23690=ORIENTED_EDGE('',*,*,#17071,.F.);
#23691=ORIENTED_EDGE('',*,*,#17079,.F.);
#23692=ORIENTED_EDGE('',*,*,#17080,.T.);
#23693=ORIENTED_EDGE('',*,*,#17081,.F.);
#23694=ORIENTED_EDGE('',*,*,#17082,.F.);
#23695=ORIENTED_EDGE('',*,*,#17083,.F.);
#23696=ORIENTED_EDGE('',*,*,#17082,.T.);
#23697=ORIENTED_EDGE('',*,*,#17084,.T.);
#23698=ORIENTED_EDGE('',*,*,#17085,.F.);
#23699=ORIENTED_EDGE('',*,*,#17084,.F.);
#23700=ORIENTED_EDGE('',*,*,#17081,.T.);
#23701=ORIENTED_EDGE('',*,*,#17086,.T.);
#23702=ORIENTED_EDGE('',*,*,#17087,.F.);
#23703=ORIENTED_EDGE('',*,*,#17086,.F.);
#23704=ORIENTED_EDGE('',*,*,#17080,.F.);
#23705=ORIENTED_EDGE('',*,*,#17088,.F.);
#23706=ORIENTED_EDGE('',*,*,#17089,.T.);
#23707=ORIENTED_EDGE('',*,*,#17090,.F.);
#23708=ORIENTED_EDGE('',*,*,#17091,.F.);
#23709=ORIENTED_EDGE('',*,*,#17092,.F.);
#23710=ORIENTED_EDGE('',*,*,#17091,.T.);
#23711=ORIENTED_EDGE('',*,*,#17093,.T.);
#23712=ORIENTED_EDGE('',*,*,#17094,.F.);
#23713=ORIENTED_EDGE('',*,*,#17093,.F.);
#23714=ORIENTED_EDGE('',*,*,#17090,.T.);
#23715=ORIENTED_EDGE('',*,*,#17095,.T.);
#23716=ORIENTED_EDGE('',*,*,#17096,.F.);
#23717=ORIENTED_EDGE('',*,*,#17095,.F.);
#23718=ORIENTED_EDGE('',*,*,#17089,.F.);
#23719=ORIENTED_EDGE('',*,*,#17097,.F.);
#23720=ORIENTED_EDGE('',*,*,#17098,.T.);
#23721=ORIENTED_EDGE('',*,*,#17099,.F.);
#23722=ORIENTED_EDGE('',*,*,#17100,.F.);
#23723=ORIENTED_EDGE('',*,*,#17101,.F.);
#23724=ORIENTED_EDGE('',*,*,#17100,.T.);
#23725=ORIENTED_EDGE('',*,*,#17102,.T.);
#23726=ORIENTED_EDGE('',*,*,#17103,.F.);
#23727=ORIENTED_EDGE('',*,*,#17102,.F.);
#23728=ORIENTED_EDGE('',*,*,#17099,.T.);
#23729=ORIENTED_EDGE('',*,*,#17104,.T.);
#23730=ORIENTED_EDGE('',*,*,#17105,.F.);
#23731=ORIENTED_EDGE('',*,*,#17104,.F.);
#23732=ORIENTED_EDGE('',*,*,#17098,.F.);
#23733=ORIENTED_EDGE('',*,*,#17106,.F.);
#23734=ORIENTED_EDGE('',*,*,#17107,.T.);
#23735=ORIENTED_EDGE('',*,*,#17108,.F.);
#23736=ORIENTED_EDGE('',*,*,#17109,.F.);
#23737=ORIENTED_EDGE('',*,*,#17110,.F.);
#23738=ORIENTED_EDGE('',*,*,#17109,.T.);
#23739=ORIENTED_EDGE('',*,*,#17111,.T.);
#23740=ORIENTED_EDGE('',*,*,#17112,.F.);
#23741=ORIENTED_EDGE('',*,*,#17111,.F.);
#23742=ORIENTED_EDGE('',*,*,#17108,.T.);
#23743=ORIENTED_EDGE('',*,*,#17113,.T.);
#23744=ORIENTED_EDGE('',*,*,#17114,.F.);
#23745=ORIENTED_EDGE('',*,*,#17113,.F.);
#23746=ORIENTED_EDGE('',*,*,#17107,.F.);
#23747=ORIENTED_EDGE('',*,*,#17115,.F.);
#23748=ORIENTED_EDGE('',*,*,#17116,.T.);
#23749=ORIENTED_EDGE('',*,*,#17117,.F.);
#23750=ORIENTED_EDGE('',*,*,#17118,.F.);
#23751=ORIENTED_EDGE('',*,*,#17119,.F.);
#23752=ORIENTED_EDGE('',*,*,#17118,.T.);
#23753=ORIENTED_EDGE('',*,*,#17120,.T.);
#23754=ORIENTED_EDGE('',*,*,#17121,.F.);
#23755=ORIENTED_EDGE('',*,*,#17120,.F.);
#23756=ORIENTED_EDGE('',*,*,#17117,.T.);
#23757=ORIENTED_EDGE('',*,*,#17122,.T.);
#23758=ORIENTED_EDGE('',*,*,#17123,.F.);
#23759=ORIENTED_EDGE('',*,*,#17122,.F.);
#23760=ORIENTED_EDGE('',*,*,#17116,.F.);
#23761=ORIENTED_EDGE('',*,*,#17124,.F.);
#23762=ORIENTED_EDGE('',*,*,#17125,.T.);
#23763=ORIENTED_EDGE('',*,*,#17126,.F.);
#23764=ORIENTED_EDGE('',*,*,#17127,.F.);
#23765=ORIENTED_EDGE('',*,*,#17128,.F.);
#23766=ORIENTED_EDGE('',*,*,#17127,.T.);
#23767=ORIENTED_EDGE('',*,*,#17129,.T.);
#23768=ORIENTED_EDGE('',*,*,#17130,.F.);
#23769=ORIENTED_EDGE('',*,*,#17129,.F.);
#23770=ORIENTED_EDGE('',*,*,#17126,.T.);
#23771=ORIENTED_EDGE('',*,*,#17131,.T.);
#23772=ORIENTED_EDGE('',*,*,#17132,.F.);
#23773=ORIENTED_EDGE('',*,*,#17131,.F.);
#23774=ORIENTED_EDGE('',*,*,#17125,.F.);
#23775=ORIENTED_EDGE('',*,*,#17133,.F.);
#23776=ORIENTED_EDGE('',*,*,#17134,.T.);
#23777=ORIENTED_EDGE('',*,*,#17135,.F.);
#23778=ORIENTED_EDGE('',*,*,#17136,.F.);
#23779=ORIENTED_EDGE('',*,*,#17137,.F.);
#23780=ORIENTED_EDGE('',*,*,#17136,.T.);
#23781=ORIENTED_EDGE('',*,*,#17138,.T.);
#23782=ORIENTED_EDGE('',*,*,#17139,.F.);
#23783=ORIENTED_EDGE('',*,*,#17138,.F.);
#23784=ORIENTED_EDGE('',*,*,#17135,.T.);
#23785=ORIENTED_EDGE('',*,*,#17140,.T.);
#23786=ORIENTED_EDGE('',*,*,#17141,.F.);
#23787=ORIENTED_EDGE('',*,*,#17140,.F.);
#23788=ORIENTED_EDGE('',*,*,#17134,.F.);
#23789=ORIENTED_EDGE('',*,*,#17142,.F.);
#23790=ORIENTED_EDGE('',*,*,#17143,.T.);
#23791=ORIENTED_EDGE('',*,*,#17144,.F.);
#23792=ORIENTED_EDGE('',*,*,#17145,.F.);
#23793=ORIENTED_EDGE('',*,*,#17146,.F.);
#23794=ORIENTED_EDGE('',*,*,#17145,.T.);
#23795=ORIENTED_EDGE('',*,*,#17147,.T.);
#23796=ORIENTED_EDGE('',*,*,#17148,.F.);
#23797=ORIENTED_EDGE('',*,*,#17147,.F.);
#23798=ORIENTED_EDGE('',*,*,#17144,.T.);
#23799=ORIENTED_EDGE('',*,*,#17149,.T.);
#23800=ORIENTED_EDGE('',*,*,#17150,.F.);
#23801=ORIENTED_EDGE('',*,*,#17149,.F.);
#23802=ORIENTED_EDGE('',*,*,#17143,.F.);
#23803=ORIENTED_EDGE('',*,*,#17151,.F.);
#23804=ORIENTED_EDGE('',*,*,#17152,.T.);
#23805=ORIENTED_EDGE('',*,*,#17153,.F.);
#23806=ORIENTED_EDGE('',*,*,#17154,.F.);
#23807=ORIENTED_EDGE('',*,*,#17155,.F.);
#23808=ORIENTED_EDGE('',*,*,#17154,.T.);
#23809=ORIENTED_EDGE('',*,*,#17156,.T.);
#23810=ORIENTED_EDGE('',*,*,#17157,.F.);
#23811=ORIENTED_EDGE('',*,*,#17156,.F.);
#23812=ORIENTED_EDGE('',*,*,#17153,.T.);
#23813=ORIENTED_EDGE('',*,*,#17158,.T.);
#23814=ORIENTED_EDGE('',*,*,#17159,.F.);
#23815=ORIENTED_EDGE('',*,*,#17158,.F.);
#23816=ORIENTED_EDGE('',*,*,#17152,.F.);
#23817=ORIENTED_EDGE('',*,*,#17160,.F.);
#23818=ORIENTED_EDGE('',*,*,#17161,.T.);
#23819=ORIENTED_EDGE('',*,*,#17162,.F.);
#23820=ORIENTED_EDGE('',*,*,#17163,.F.);
#23821=ORIENTED_EDGE('',*,*,#17164,.F.);
#23822=ORIENTED_EDGE('',*,*,#17163,.T.);
#23823=ORIENTED_EDGE('',*,*,#17165,.T.);
#23824=ORIENTED_EDGE('',*,*,#17166,.F.);
#23825=ORIENTED_EDGE('',*,*,#17165,.F.);
#23826=ORIENTED_EDGE('',*,*,#17162,.T.);
#23827=ORIENTED_EDGE('',*,*,#17167,.T.);
#23828=ORIENTED_EDGE('',*,*,#17168,.F.);
#23829=ORIENTED_EDGE('',*,*,#17167,.F.);
#23830=ORIENTED_EDGE('',*,*,#17161,.F.);
#23831=ORIENTED_EDGE('',*,*,#17169,.F.);
#23832=ORIENTED_EDGE('',*,*,#17170,.T.);
#23833=ORIENTED_EDGE('',*,*,#17171,.F.);
#23834=ORIENTED_EDGE('',*,*,#17172,.F.);
#23835=ORIENTED_EDGE('',*,*,#17173,.F.);
#23836=ORIENTED_EDGE('',*,*,#17172,.T.);
#23837=ORIENTED_EDGE('',*,*,#17174,.T.);
#23838=ORIENTED_EDGE('',*,*,#17175,.F.);
#23839=ORIENTED_EDGE('',*,*,#17174,.F.);
#23840=ORIENTED_EDGE('',*,*,#17171,.T.);
#23841=ORIENTED_EDGE('',*,*,#17176,.T.);
#23842=ORIENTED_EDGE('',*,*,#17177,.F.);
#23843=ORIENTED_EDGE('',*,*,#17176,.F.);
#23844=ORIENTED_EDGE('',*,*,#17170,.F.);
#23845=ORIENTED_EDGE('',*,*,#17178,.F.);
#23846=ORIENTED_EDGE('',*,*,#17179,.T.);
#23847=ORIENTED_EDGE('',*,*,#17180,.F.);
#23848=ORIENTED_EDGE('',*,*,#17181,.F.);
#23849=ORIENTED_EDGE('',*,*,#17182,.F.);
#23850=ORIENTED_EDGE('',*,*,#17181,.T.);
#23851=ORIENTED_EDGE('',*,*,#17183,.T.);
#23852=ORIENTED_EDGE('',*,*,#17184,.F.);
#23853=ORIENTED_EDGE('',*,*,#17183,.F.);
#23854=ORIENTED_EDGE('',*,*,#17180,.T.);
#23855=ORIENTED_EDGE('',*,*,#17185,.T.);
#23856=ORIENTED_EDGE('',*,*,#17186,.F.);
#23857=ORIENTED_EDGE('',*,*,#17185,.F.);
#23858=ORIENTED_EDGE('',*,*,#17179,.F.);
#23859=ORIENTED_EDGE('',*,*,#17187,.F.);
#23860=ORIENTED_EDGE('',*,*,#17188,.T.);
#23861=ORIENTED_EDGE('',*,*,#17189,.F.);
#23862=ORIENTED_EDGE('',*,*,#17190,.F.);
#23863=ORIENTED_EDGE('',*,*,#17191,.F.);
#23864=ORIENTED_EDGE('',*,*,#17190,.T.);
#23865=ORIENTED_EDGE('',*,*,#17192,.T.);
#23866=ORIENTED_EDGE('',*,*,#17193,.F.);
#23867=ORIENTED_EDGE('',*,*,#17194,.F.);
#23868=ORIENTED_EDGE('',*,*,#17192,.F.);
#23869=ORIENTED_EDGE('',*,*,#17189,.T.);
#23870=ORIENTED_EDGE('',*,*,#17195,.T.);
#23871=ORIENTED_EDGE('',*,*,#17196,.F.);
#23872=ORIENTED_EDGE('',*,*,#17195,.F.);
#23873=ORIENTED_EDGE('',*,*,#17188,.F.);
#23874=ORIENTED_EDGE('',*,*,#17197,.F.);
#23875=ORIENTED_EDGE('',*,*,#17198,.F.);
#23876=ORIENTED_EDGE('',*,*,#17199,.T.);
#23877=ORIENTED_EDGE('',*,*,#17200,.F.);
#23878=ORIENTED_EDGE('',*,*,#17201,.F.);
#23879=ORIENTED_EDGE('',*,*,#17202,.F.);
#23880=ORIENTED_EDGE('',*,*,#17201,.T.);
#23881=ORIENTED_EDGE('',*,*,#17203,.T.);
#23882=ORIENTED_EDGE('',*,*,#17204,.F.);
#23883=ORIENTED_EDGE('',*,*,#17203,.F.);
#23884=ORIENTED_EDGE('',*,*,#17200,.T.);
#23885=ORIENTED_EDGE('',*,*,#17205,.T.);
#23886=ORIENTED_EDGE('',*,*,#17206,.F.);
#23887=ORIENTED_EDGE('',*,*,#17205,.F.);
#23888=ORIENTED_EDGE('',*,*,#17199,.F.);
#23889=ORIENTED_EDGE('',*,*,#17207,.F.);
#23890=ORIENTED_EDGE('',*,*,#17208,.T.);
#23891=ORIENTED_EDGE('',*,*,#17209,.F.);
#23892=ORIENTED_EDGE('',*,*,#17210,.F.);
#23893=ORIENTED_EDGE('',*,*,#17211,.F.);
#23894=ORIENTED_EDGE('',*,*,#17210,.T.);
#23895=ORIENTED_EDGE('',*,*,#17212,.T.);
#23896=ORIENTED_EDGE('',*,*,#17213,.F.);
#23897=ORIENTED_EDGE('',*,*,#17212,.F.);
#23898=ORIENTED_EDGE('',*,*,#17209,.T.);
#23899=ORIENTED_EDGE('',*,*,#17214,.T.);
#23900=ORIENTED_EDGE('',*,*,#17215,.F.);
#23901=ORIENTED_EDGE('',*,*,#17214,.F.);
#23902=ORIENTED_EDGE('',*,*,#17208,.F.);
#23903=ORIENTED_EDGE('',*,*,#17216,.F.);
#23904=ORIENTED_EDGE('',*,*,#17217,.T.);
#23905=ORIENTED_EDGE('',*,*,#17218,.F.);
#23906=ORIENTED_EDGE('',*,*,#17219,.F.);
#23907=ORIENTED_EDGE('',*,*,#17220,.F.);
#23908=ORIENTED_EDGE('',*,*,#17219,.T.);
#23909=ORIENTED_EDGE('',*,*,#17221,.T.);
#23910=ORIENTED_EDGE('',*,*,#17222,.F.);
#23911=ORIENTED_EDGE('',*,*,#17221,.F.);
#23912=ORIENTED_EDGE('',*,*,#17218,.T.);
#23913=ORIENTED_EDGE('',*,*,#17223,.T.);
#23914=ORIENTED_EDGE('',*,*,#17224,.F.);
#23915=ORIENTED_EDGE('',*,*,#17223,.F.);
#23916=ORIENTED_EDGE('',*,*,#17217,.F.);
#23917=ORIENTED_EDGE('',*,*,#17225,.F.);
#23918=ORIENTED_EDGE('',*,*,#17226,.T.);
#23919=ORIENTED_EDGE('',*,*,#17227,.F.);
#23920=ORIENTED_EDGE('',*,*,#17228,.F.);
#23921=ORIENTED_EDGE('',*,*,#17229,.F.);
#23922=ORIENTED_EDGE('',*,*,#17228,.T.);
#23923=ORIENTED_EDGE('',*,*,#17230,.T.);
#23924=ORIENTED_EDGE('',*,*,#17231,.F.);
#23925=ORIENTED_EDGE('',*,*,#17230,.F.);
#23926=ORIENTED_EDGE('',*,*,#17227,.T.);
#23927=ORIENTED_EDGE('',*,*,#17232,.T.);
#23928=ORIENTED_EDGE('',*,*,#17233,.F.);
#23929=ORIENTED_EDGE('',*,*,#17232,.F.);
#23930=ORIENTED_EDGE('',*,*,#17226,.F.);
#23931=ORIENTED_EDGE('',*,*,#17234,.F.);
#23932=ORIENTED_EDGE('',*,*,#17235,.T.);
#23933=ORIENTED_EDGE('',*,*,#17236,.F.);
#23934=ORIENTED_EDGE('',*,*,#17237,.F.);
#23935=ORIENTED_EDGE('',*,*,#17238,.F.);
#23936=ORIENTED_EDGE('',*,*,#17237,.T.);
#23937=ORIENTED_EDGE('',*,*,#17239,.T.);
#23938=ORIENTED_EDGE('',*,*,#17240,.F.);
#23939=ORIENTED_EDGE('',*,*,#17239,.F.);
#23940=ORIENTED_EDGE('',*,*,#17236,.T.);
#23941=ORIENTED_EDGE('',*,*,#17241,.T.);
#23942=ORIENTED_EDGE('',*,*,#17242,.F.);
#23943=ORIENTED_EDGE('',*,*,#17241,.F.);
#23944=ORIENTED_EDGE('',*,*,#17235,.F.);
#23945=ORIENTED_EDGE('',*,*,#17243,.F.);
#23946=ORIENTED_EDGE('',*,*,#17244,.T.);
#23947=ORIENTED_EDGE('',*,*,#17245,.F.);
#23948=ORIENTED_EDGE('',*,*,#17246,.F.);
#23949=ORIENTED_EDGE('',*,*,#17247,.F.);
#23950=ORIENTED_EDGE('',*,*,#17246,.T.);
#23951=ORIENTED_EDGE('',*,*,#17248,.T.);
#23952=ORIENTED_EDGE('',*,*,#17249,.F.);
#23953=ORIENTED_EDGE('',*,*,#17248,.F.);
#23954=ORIENTED_EDGE('',*,*,#17245,.T.);
#23955=ORIENTED_EDGE('',*,*,#17250,.T.);
#23956=ORIENTED_EDGE('',*,*,#17251,.F.);
#23957=ORIENTED_EDGE('',*,*,#17250,.F.);
#23958=ORIENTED_EDGE('',*,*,#17244,.F.);
#23959=ORIENTED_EDGE('',*,*,#17252,.F.);
#23960=ORIENTED_EDGE('',*,*,#17253,.T.);
#23961=ORIENTED_EDGE('',*,*,#17254,.F.);
#23962=ORIENTED_EDGE('',*,*,#17255,.F.);
#23963=ORIENTED_EDGE('',*,*,#17256,.F.);
#23964=ORIENTED_EDGE('',*,*,#17255,.T.);
#23965=ORIENTED_EDGE('',*,*,#17257,.T.);
#23966=ORIENTED_EDGE('',*,*,#17258,.F.);
#23967=ORIENTED_EDGE('',*,*,#17257,.F.);
#23968=ORIENTED_EDGE('',*,*,#17254,.T.);
#23969=ORIENTED_EDGE('',*,*,#17259,.T.);
#23970=ORIENTED_EDGE('',*,*,#17260,.F.);
#23971=ORIENTED_EDGE('',*,*,#17259,.F.);
#23972=ORIENTED_EDGE('',*,*,#17253,.F.);
#23973=ORIENTED_EDGE('',*,*,#17261,.F.);
#23974=ORIENTED_EDGE('',*,*,#17262,.T.);
#23975=ORIENTED_EDGE('',*,*,#17263,.F.);
#23976=ORIENTED_EDGE('',*,*,#17264,.F.);
#23977=ORIENTED_EDGE('',*,*,#17265,.F.);
#23978=ORIENTED_EDGE('',*,*,#17264,.T.);
#23979=ORIENTED_EDGE('',*,*,#17266,.T.);
#23980=ORIENTED_EDGE('',*,*,#17267,.F.);
#23981=ORIENTED_EDGE('',*,*,#17266,.F.);
#23982=ORIENTED_EDGE('',*,*,#17263,.T.);
#23983=ORIENTED_EDGE('',*,*,#17268,.T.);
#23984=ORIENTED_EDGE('',*,*,#17269,.F.);
#23985=ORIENTED_EDGE('',*,*,#17268,.F.);
#23986=ORIENTED_EDGE('',*,*,#17262,.F.);
#23987=ORIENTED_EDGE('',*,*,#17270,.F.);
#23988=ORIENTED_EDGE('',*,*,#17271,.T.);
#23989=ORIENTED_EDGE('',*,*,#17272,.F.);
#23990=ORIENTED_EDGE('',*,*,#17273,.F.);
#23991=ORIENTED_EDGE('',*,*,#17274,.F.);
#23992=ORIENTED_EDGE('',*,*,#17273,.T.);
#23993=ORIENTED_EDGE('',*,*,#17275,.T.);
#23994=ORIENTED_EDGE('',*,*,#17276,.F.);
#23995=ORIENTED_EDGE('',*,*,#17275,.F.);
#23996=ORIENTED_EDGE('',*,*,#17272,.T.);
#23997=ORIENTED_EDGE('',*,*,#17277,.T.);
#23998=ORIENTED_EDGE('',*,*,#17278,.F.);
#23999=ORIENTED_EDGE('',*,*,#17277,.F.);
#24000=ORIENTED_EDGE('',*,*,#17271,.F.);
#24001=ORIENTED_EDGE('',*,*,#17279,.F.);
#24002=ORIENTED_EDGE('',*,*,#17280,.T.);
#24003=ORIENTED_EDGE('',*,*,#17281,.F.);
#24004=ORIENTED_EDGE('',*,*,#17282,.F.);
#24005=ORIENTED_EDGE('',*,*,#17283,.F.);
#24006=ORIENTED_EDGE('',*,*,#17282,.T.);
#24007=ORIENTED_EDGE('',*,*,#17284,.T.);
#24008=ORIENTED_EDGE('',*,*,#17285,.F.);
#24009=ORIENTED_EDGE('',*,*,#17284,.F.);
#24010=ORIENTED_EDGE('',*,*,#17281,.T.);
#24011=ORIENTED_EDGE('',*,*,#17286,.T.);
#24012=ORIENTED_EDGE('',*,*,#17287,.F.);
#24013=ORIENTED_EDGE('',*,*,#17286,.F.);
#24014=ORIENTED_EDGE('',*,*,#17280,.F.);
#24015=ORIENTED_EDGE('',*,*,#17288,.F.);
#24016=ORIENTED_EDGE('',*,*,#17289,.T.);
#24017=ORIENTED_EDGE('',*,*,#17290,.F.);
#24018=ORIENTED_EDGE('',*,*,#17291,.F.);
#24019=ORIENTED_EDGE('',*,*,#17292,.F.);
#24020=ORIENTED_EDGE('',*,*,#17291,.T.);
#24021=ORIENTED_EDGE('',*,*,#17293,.T.);
#24022=ORIENTED_EDGE('',*,*,#17294,.F.);
#24023=ORIENTED_EDGE('',*,*,#17293,.F.);
#24024=ORIENTED_EDGE('',*,*,#17290,.T.);
#24025=ORIENTED_EDGE('',*,*,#17295,.T.);
#24026=ORIENTED_EDGE('',*,*,#17296,.F.);
#24027=ORIENTED_EDGE('',*,*,#17295,.F.);
#24028=ORIENTED_EDGE('',*,*,#17289,.F.);
#24029=ORIENTED_EDGE('',*,*,#17297,.F.);
#24030=ORIENTED_EDGE('',*,*,#17298,.T.);
#24031=ORIENTED_EDGE('',*,*,#17299,.F.);
#24032=ORIENTED_EDGE('',*,*,#17300,.F.);
#24033=ORIENTED_EDGE('',*,*,#17301,.F.);
#24034=ORIENTED_EDGE('',*,*,#17300,.T.);
#24035=ORIENTED_EDGE('',*,*,#17302,.T.);
#24036=ORIENTED_EDGE('',*,*,#17303,.F.);
#24037=ORIENTED_EDGE('',*,*,#17302,.F.);
#24038=ORIENTED_EDGE('',*,*,#17299,.T.);
#24039=ORIENTED_EDGE('',*,*,#17304,.T.);
#24040=ORIENTED_EDGE('',*,*,#17305,.F.);
#24041=ORIENTED_EDGE('',*,*,#17304,.F.);
#24042=ORIENTED_EDGE('',*,*,#17298,.F.);
#24043=ORIENTED_EDGE('',*,*,#17306,.F.);
#24044=ORIENTED_EDGE('',*,*,#17307,.T.);
#24045=ORIENTED_EDGE('',*,*,#17308,.F.);
#24046=ORIENTED_EDGE('',*,*,#17309,.F.);
#24047=ORIENTED_EDGE('',*,*,#17310,.F.);
#24048=ORIENTED_EDGE('',*,*,#17309,.T.);
#24049=ORIENTED_EDGE('',*,*,#17311,.T.);
#24050=ORIENTED_EDGE('',*,*,#17312,.F.);
#24051=ORIENTED_EDGE('',*,*,#17311,.F.);
#24052=ORIENTED_EDGE('',*,*,#17308,.T.);
#24053=ORIENTED_EDGE('',*,*,#17313,.T.);
#24054=ORIENTED_EDGE('',*,*,#17314,.F.);
#24055=ORIENTED_EDGE('',*,*,#17313,.F.);
#24056=ORIENTED_EDGE('',*,*,#17307,.F.);
#24057=ORIENTED_EDGE('',*,*,#17315,.F.);
#24058=ORIENTED_EDGE('',*,*,#17316,.T.);
#24059=ORIENTED_EDGE('',*,*,#17317,.F.);
#24060=ORIENTED_EDGE('',*,*,#17318,.F.);
#24061=ORIENTED_EDGE('',*,*,#17319,.F.);
#24062=ORIENTED_EDGE('',*,*,#17318,.T.);
#24063=ORIENTED_EDGE('',*,*,#17320,.T.);
#24064=ORIENTED_EDGE('',*,*,#17321,.F.);
#24065=ORIENTED_EDGE('',*,*,#17320,.F.);
#24066=ORIENTED_EDGE('',*,*,#17317,.T.);
#24067=ORIENTED_EDGE('',*,*,#17322,.T.);
#24068=ORIENTED_EDGE('',*,*,#17323,.F.);
#24069=ORIENTED_EDGE('',*,*,#17322,.F.);
#24070=ORIENTED_EDGE('',*,*,#17316,.F.);
#24071=ORIENTED_EDGE('',*,*,#17324,.F.);
#24072=ORIENTED_EDGE('',*,*,#17325,.T.);
#24073=ORIENTED_EDGE('',*,*,#17326,.F.);
#24074=ORIENTED_EDGE('',*,*,#17327,.F.);
#24075=ORIENTED_EDGE('',*,*,#17328,.F.);
#24076=ORIENTED_EDGE('',*,*,#17327,.T.);
#24077=ORIENTED_EDGE('',*,*,#17329,.T.);
#24078=ORIENTED_EDGE('',*,*,#17330,.F.);
#24079=ORIENTED_EDGE('',*,*,#17329,.F.);
#24080=ORIENTED_EDGE('',*,*,#17326,.T.);
#24081=ORIENTED_EDGE('',*,*,#17331,.T.);
#24082=ORIENTED_EDGE('',*,*,#17332,.F.);
#24083=ORIENTED_EDGE('',*,*,#17331,.F.);
#24084=ORIENTED_EDGE('',*,*,#17325,.F.);
#24085=ORIENTED_EDGE('',*,*,#17333,.F.);
#24086=ORIENTED_EDGE('',*,*,#17334,.T.);
#24087=ORIENTED_EDGE('',*,*,#17335,.F.);
#24088=ORIENTED_EDGE('',*,*,#17336,.F.);
#24089=ORIENTED_EDGE('',*,*,#17337,.F.);
#24090=ORIENTED_EDGE('',*,*,#17336,.T.);
#24091=ORIENTED_EDGE('',*,*,#17338,.T.);
#24092=ORIENTED_EDGE('',*,*,#17339,.F.);
#24093=ORIENTED_EDGE('',*,*,#17338,.F.);
#24094=ORIENTED_EDGE('',*,*,#17335,.T.);
#24095=ORIENTED_EDGE('',*,*,#17340,.T.);
#24096=ORIENTED_EDGE('',*,*,#17341,.F.);
#24097=ORIENTED_EDGE('',*,*,#17340,.F.);
#24098=ORIENTED_EDGE('',*,*,#17334,.F.);
#24099=ORIENTED_EDGE('',*,*,#17342,.F.);
#24100=ORIENTED_EDGE('',*,*,#17343,.T.);
#24101=ORIENTED_EDGE('',*,*,#17344,.F.);
#24102=ORIENTED_EDGE('',*,*,#17345,.F.);
#24103=ORIENTED_EDGE('',*,*,#17346,.F.);
#24104=ORIENTED_EDGE('',*,*,#17345,.T.);
#24105=ORIENTED_EDGE('',*,*,#17347,.T.);
#24106=ORIENTED_EDGE('',*,*,#17348,.F.);
#24107=ORIENTED_EDGE('',*,*,#17347,.F.);
#24108=ORIENTED_EDGE('',*,*,#17344,.T.);
#24109=ORIENTED_EDGE('',*,*,#17349,.T.);
#24110=ORIENTED_EDGE('',*,*,#17350,.F.);
#24111=ORIENTED_EDGE('',*,*,#17349,.F.);
#24112=ORIENTED_EDGE('',*,*,#17343,.F.);
#24113=ORIENTED_EDGE('',*,*,#17351,.F.);
#24114=ORIENTED_EDGE('',*,*,#17352,.T.);
#24115=ORIENTED_EDGE('',*,*,#17353,.F.);
#24116=ORIENTED_EDGE('',*,*,#17354,.F.);
#24117=ORIENTED_EDGE('',*,*,#17355,.F.);
#24118=ORIENTED_EDGE('',*,*,#17354,.T.);
#24119=ORIENTED_EDGE('',*,*,#17356,.T.);
#24120=ORIENTED_EDGE('',*,*,#17357,.F.);
#24121=ORIENTED_EDGE('',*,*,#17356,.F.);
#24122=ORIENTED_EDGE('',*,*,#17353,.T.);
#24123=ORIENTED_EDGE('',*,*,#17358,.T.);
#24124=ORIENTED_EDGE('',*,*,#17359,.F.);
#24125=ORIENTED_EDGE('',*,*,#17358,.F.);
#24126=ORIENTED_EDGE('',*,*,#17352,.F.);
#24127=ORIENTED_EDGE('',*,*,#17360,.T.);
#24128=ORIENTED_EDGE('',*,*,#17361,.F.);
#24129=ORIENTED_EDGE('',*,*,#17360,.F.);
#24130=ORIENTED_EDGE('',*,*,#17362,.F.);
#24131=ORIENTED_EDGE('',*,*,#17363,.T.);
#24132=ORIENTED_EDGE('',*,*,#17364,.T.);
#24133=ORIENTED_EDGE('',*,*,#17365,.F.);
#24134=ORIENTED_EDGE('',*,*,#17366,.F.);
#24135=ORIENTED_EDGE('',*,*,#17367,.T.);
#24136=ORIENTED_EDGE('',*,*,#17368,.T.);
#24137=ORIENTED_EDGE('',*,*,#17363,.F.);
#24138=ORIENTED_EDGE('',*,*,#17369,.F.);
#24139=ORIENTED_EDGE('',*,*,#17370,.T.);
#24140=ORIENTED_EDGE('',*,*,#17371,.T.);
#24141=ORIENTED_EDGE('',*,*,#17367,.F.);
#24142=ORIENTED_EDGE('',*,*,#17372,.F.);
#24143=ORIENTED_EDGE('',*,*,#17373,.T.);
#24144=ORIENTED_EDGE('',*,*,#17374,.T.);
#24145=ORIENTED_EDGE('',*,*,#17370,.F.);
#24146=ORIENTED_EDGE('',*,*,#17375,.F.);
#24147=ORIENTED_EDGE('',*,*,#17376,.T.);
#24148=ORIENTED_EDGE('',*,*,#17377,.T.);
#24149=ORIENTED_EDGE('',*,*,#17373,.F.);
#24150=ORIENTED_EDGE('',*,*,#17378,.F.);
#24151=ORIENTED_EDGE('',*,*,#17365,.T.);
#24152=ORIENTED_EDGE('',*,*,#17379,.T.);
#24153=ORIENTED_EDGE('',*,*,#17376,.F.);
#24154=ORIENTED_EDGE('',*,*,#17379,.F.);
#24155=ORIENTED_EDGE('',*,*,#17364,.F.);
#24156=ORIENTED_EDGE('',*,*,#17368,.F.);
#24157=ORIENTED_EDGE('',*,*,#17371,.F.);
#24158=ORIENTED_EDGE('',*,*,#17374,.F.);
#24159=ORIENTED_EDGE('',*,*,#17377,.F.);
#24160=ORIENTED_EDGE('',*,*,#17361,.T.);
#24161=ORIENTED_EDGE('',*,*,#17380,.F.);
#24162=ORIENTED_EDGE('',*,*,#17023,.F.);
#24163=ORIENTED_EDGE('',*,*,#16765,.F.);
#24164=ORIENTED_EDGE('',*,*,#17024,.F.);
#24165=ORIENTED_EDGE('',*,*,#17381,.T.);
#24166=ORIENTED_EDGE('',*,*,#17380,.T.);
#24167=ORIENTED_EDGE('',*,*,#17381,.F.);
#24168=ORIENTED_EDGE('',*,*,#17382,.F.);
#24169=ORIENTED_EDGE('',*,*,#17383,.T.);
#24170=ORIENTED_EDGE('',*,*,#17197,.T.);
#24171=ORIENTED_EDGE('',*,*,#17187,.T.);
#24172=ORIENTED_EDGE('',*,*,#17191,.T.);
#24173=ORIENTED_EDGE('',*,*,#17384,.T.);
#24174=ORIENTED_EDGE('',*,*,#17033,.T.);
#24175=ORIENTED_EDGE('',*,*,#17384,.F.);
#24176=ORIENTED_EDGE('',*,*,#17193,.T.);
#24177=ORIENTED_EDGE('',*,*,#17194,.T.);
#24178=ORIENTED_EDGE('',*,*,#17196,.T.);
#24179=ORIENTED_EDGE('',*,*,#17383,.F.);
#24180=ORIENTED_EDGE('',*,*,#17040,.T.);
#24181=ORIENTED_EDGE('',*,*,#17042,.T.);
#24182=ORIENTED_EDGE('',*,*,#17034,.T.);
#24183=ORIENTED_EDGE('',*,*,#17038,.T.);
#24184=ORIENTED_EDGE('',*,*,#17049,.T.);
#24185=ORIENTED_EDGE('',*,*,#17051,.T.);
#24186=ORIENTED_EDGE('',*,*,#17043,.T.);
#24187=ORIENTED_EDGE('',*,*,#17047,.T.);
#24188=ORIENTED_EDGE('',*,*,#17058,.T.);
#24189=ORIENTED_EDGE('',*,*,#17060,.T.);
#24190=ORIENTED_EDGE('',*,*,#17052,.T.);
#24191=ORIENTED_EDGE('',*,*,#17056,.T.);
#24192=ORIENTED_EDGE('',*,*,#17067,.T.);
#24193=ORIENTED_EDGE('',*,*,#17069,.T.);
#24194=ORIENTED_EDGE('',*,*,#17061,.T.);
#24195=ORIENTED_EDGE('',*,*,#17065,.T.);
#24196=ORIENTED_EDGE('',*,*,#17076,.T.);
#24197=ORIENTED_EDGE('',*,*,#17078,.T.);
#24198=ORIENTED_EDGE('',*,*,#17070,.T.);
#24199=ORIENTED_EDGE('',*,*,#17074,.T.);
#24200=ORIENTED_EDGE('',*,*,#17085,.T.);
#24201=ORIENTED_EDGE('',*,*,#17087,.T.);
#24202=ORIENTED_EDGE('',*,*,#17079,.T.);
#24203=ORIENTED_EDGE('',*,*,#17083,.T.);
#24204=ORIENTED_EDGE('',*,*,#17094,.T.);
#24205=ORIENTED_EDGE('',*,*,#17096,.T.);
#24206=ORIENTED_EDGE('',*,*,#17088,.T.);
#24207=ORIENTED_EDGE('',*,*,#17092,.T.);
#24208=ORIENTED_EDGE('',*,*,#17103,.T.);
#24209=ORIENTED_EDGE('',*,*,#17105,.T.);
#24210=ORIENTED_EDGE('',*,*,#17097,.T.);
#24211=ORIENTED_EDGE('',*,*,#17101,.T.);
#24212=ORIENTED_EDGE('',*,*,#17112,.T.);
#24213=ORIENTED_EDGE('',*,*,#17114,.T.);
#24214=ORIENTED_EDGE('',*,*,#17106,.T.);
#24215=ORIENTED_EDGE('',*,*,#17110,.T.);
#24216=ORIENTED_EDGE('',*,*,#17121,.T.);
#24217=ORIENTED_EDGE('',*,*,#17123,.T.);
#24218=ORIENTED_EDGE('',*,*,#17115,.T.);
#24219=ORIENTED_EDGE('',*,*,#17119,.T.);
#24220=ORIENTED_EDGE('',*,*,#17130,.T.);
#24221=ORIENTED_EDGE('',*,*,#17132,.T.);
#24222=ORIENTED_EDGE('',*,*,#17124,.T.);
#24223=ORIENTED_EDGE('',*,*,#17128,.T.);
#24224=ORIENTED_EDGE('',*,*,#17139,.T.);
#24225=ORIENTED_EDGE('',*,*,#17141,.T.);
#24226=ORIENTED_EDGE('',*,*,#17133,.T.);
#24227=ORIENTED_EDGE('',*,*,#17137,.T.);
#24228=ORIENTED_EDGE('',*,*,#17148,.T.);
#24229=ORIENTED_EDGE('',*,*,#17150,.T.);
#24230=ORIENTED_EDGE('',*,*,#17142,.T.);
#24231=ORIENTED_EDGE('',*,*,#17146,.T.);
#24232=ORIENTED_EDGE('',*,*,#17157,.T.);
#24233=ORIENTED_EDGE('',*,*,#17159,.T.);
#24234=ORIENTED_EDGE('',*,*,#17151,.T.);
#24235=ORIENTED_EDGE('',*,*,#17155,.T.);
#24236=ORIENTED_EDGE('',*,*,#17166,.T.);
#24237=ORIENTED_EDGE('',*,*,#17168,.T.);
#24238=ORIENTED_EDGE('',*,*,#17160,.T.);
#24239=ORIENTED_EDGE('',*,*,#17164,.T.);
#24240=ORIENTED_EDGE('',*,*,#17175,.T.);
#24241=ORIENTED_EDGE('',*,*,#17177,.T.);
#24242=ORIENTED_EDGE('',*,*,#17169,.T.);
#24243=ORIENTED_EDGE('',*,*,#17173,.T.);
#24244=ORIENTED_EDGE('',*,*,#17184,.T.);
#24245=ORIENTED_EDGE('',*,*,#17186,.T.);
#24246=ORIENTED_EDGE('',*,*,#17178,.T.);
#24247=ORIENTED_EDGE('',*,*,#17182,.T.);
#24248=ORIENTED_EDGE('',*,*,#17204,.T.);
#24249=ORIENTED_EDGE('',*,*,#17206,.T.);
#24250=ORIENTED_EDGE('',*,*,#17198,.T.);
#24251=ORIENTED_EDGE('',*,*,#17202,.T.);
#24252=ORIENTED_EDGE('',*,*,#17213,.T.);
#24253=ORIENTED_EDGE('',*,*,#17215,.T.);
#24254=ORIENTED_EDGE('',*,*,#17207,.T.);
#24255=ORIENTED_EDGE('',*,*,#17211,.T.);
#24256=ORIENTED_EDGE('',*,*,#17222,.T.);
#24257=ORIENTED_EDGE('',*,*,#17224,.T.);
#24258=ORIENTED_EDGE('',*,*,#17216,.T.);
#24259=ORIENTED_EDGE('',*,*,#17220,.T.);
#24260=ORIENTED_EDGE('',*,*,#17231,.T.);
#24261=ORIENTED_EDGE('',*,*,#17233,.T.);
#24262=ORIENTED_EDGE('',*,*,#17225,.T.);
#24263=ORIENTED_EDGE('',*,*,#17229,.T.);
#24264=ORIENTED_EDGE('',*,*,#17240,.T.);
#24265=ORIENTED_EDGE('',*,*,#17242,.T.);
#24266=ORIENTED_EDGE('',*,*,#17234,.T.);
#24267=ORIENTED_EDGE('',*,*,#17238,.T.);
#24268=ORIENTED_EDGE('',*,*,#17249,.T.);
#24269=ORIENTED_EDGE('',*,*,#17251,.T.);
#24270=ORIENTED_EDGE('',*,*,#17243,.T.);
#24271=ORIENTED_EDGE('',*,*,#17247,.T.);
#24272=ORIENTED_EDGE('',*,*,#17258,.T.);
#24273=ORIENTED_EDGE('',*,*,#17260,.T.);
#24274=ORIENTED_EDGE('',*,*,#17252,.T.);
#24275=ORIENTED_EDGE('',*,*,#17256,.T.);
#24276=ORIENTED_EDGE('',*,*,#17267,.T.);
#24277=ORIENTED_EDGE('',*,*,#17269,.T.);
#24278=ORIENTED_EDGE('',*,*,#17261,.T.);
#24279=ORIENTED_EDGE('',*,*,#17265,.T.);
#24280=ORIENTED_EDGE('',*,*,#17276,.T.);
#24281=ORIENTED_EDGE('',*,*,#17278,.T.);
#24282=ORIENTED_EDGE('',*,*,#17270,.T.);
#24283=ORIENTED_EDGE('',*,*,#17274,.T.);
#24284=ORIENTED_EDGE('',*,*,#17285,.T.);
#24285=ORIENTED_EDGE('',*,*,#17287,.T.);
#24286=ORIENTED_EDGE('',*,*,#17279,.T.);
#24287=ORIENTED_EDGE('',*,*,#17283,.T.);
#24288=ORIENTED_EDGE('',*,*,#17294,.T.);
#24289=ORIENTED_EDGE('',*,*,#17296,.T.);
#24290=ORIENTED_EDGE('',*,*,#17288,.T.);
#24291=ORIENTED_EDGE('',*,*,#17292,.T.);
#24292=ORIENTED_EDGE('',*,*,#17303,.T.);
#24293=ORIENTED_EDGE('',*,*,#17305,.T.);
#24294=ORIENTED_EDGE('',*,*,#17297,.T.);
#24295=ORIENTED_EDGE('',*,*,#17301,.T.);
#24296=ORIENTED_EDGE('',*,*,#17312,.T.);
#24297=ORIENTED_EDGE('',*,*,#17314,.T.);
#24298=ORIENTED_EDGE('',*,*,#17306,.T.);
#24299=ORIENTED_EDGE('',*,*,#17310,.T.);
#24300=ORIENTED_EDGE('',*,*,#17321,.T.);
#24301=ORIENTED_EDGE('',*,*,#17323,.T.);
#24302=ORIENTED_EDGE('',*,*,#17315,.T.);
#24303=ORIENTED_EDGE('',*,*,#17319,.T.);
#24304=ORIENTED_EDGE('',*,*,#17330,.T.);
#24305=ORIENTED_EDGE('',*,*,#17332,.T.);
#24306=ORIENTED_EDGE('',*,*,#17324,.T.);
#24307=ORIENTED_EDGE('',*,*,#17328,.T.);
#24308=ORIENTED_EDGE('',*,*,#17339,.T.);
#24309=ORIENTED_EDGE('',*,*,#17341,.T.);
#24310=ORIENTED_EDGE('',*,*,#17333,.T.);
#24311=ORIENTED_EDGE('',*,*,#17337,.T.);
#24312=ORIENTED_EDGE('',*,*,#17348,.T.);
#24313=ORIENTED_EDGE('',*,*,#17350,.T.);
#24314=ORIENTED_EDGE('',*,*,#17342,.T.);
#24315=ORIENTED_EDGE('',*,*,#17346,.T.);
#24316=ORIENTED_EDGE('',*,*,#17357,.T.);
#24317=ORIENTED_EDGE('',*,*,#17359,.T.);
#24318=ORIENTED_EDGE('',*,*,#17351,.T.);
#24319=ORIENTED_EDGE('',*,*,#17355,.T.);
#24320=ORIENTED_EDGE('',*,*,#17385,.F.);
#24321=ORIENTED_EDGE('',*,*,#17386,.T.);
#24322=ORIENTED_EDGE('',*,*,#17382,.T.);
#24323=ORIENTED_EDGE('',*,*,#17386,.F.);
#24324=ORIENTED_EDGE('',*,*,#17385,.T.);
#24325=ORIENTED_EDGE('',*,*,#17362,.T.);
#24326=ORIENTED_EDGE('',*,*,#17378,.T.);
#24327=ORIENTED_EDGE('',*,*,#17375,.T.);
#24328=ORIENTED_EDGE('',*,*,#17372,.T.);
#24329=ORIENTED_EDGE('',*,*,#17369,.T.);
#24330=ORIENTED_EDGE('',*,*,#17366,.T.);
#24331=ORIENTED_EDGE('',*,*,#17387,.F.);
#24332=ORIENTED_EDGE('',*,*,#17388,.F.);
#24333=ORIENTED_EDGE('',*,*,#17389,.T.);
#24334=ORIENTED_EDGE('',*,*,#17387,.T.);
#24335=ORIENTED_EDGE('',*,*,#17389,.F.);
#24336=ORIENTED_EDGE('',*,*,#17390,.F.);
#24337=ORIENTED_EDGE('',*,*,#17391,.T.);
#24338=ORIENTED_EDGE('',*,*,#17388,.T.);
#24339=ORIENTED_EDGE('',*,*,#17391,.F.);
#24340=ORIENTED_EDGE('',*,*,#17392,.F.);
#24341=ORIENTED_EDGE('',*,*,#17393,.T.);
#24342=ORIENTED_EDGE('',*,*,#17390,.T.);
#24343=ORIENTED_EDGE('',*,*,#17393,.F.);
#24344=ORIENTED_EDGE('',*,*,#17392,.T.);
#24345=ORIENTED_EDGE('',*,*,#17394,.F.);
#24346=ORIENTED_EDGE('',*,*,#17395,.T.);
#24347=ORIENTED_EDGE('',*,*,#17396,.T.);
#24348=ORIENTED_EDGE('',*,*,#17397,.T.);
#24349=ORIENTED_EDGE('',*,*,#17398,.F.);
#24350=ORIENTED_EDGE('',*,*,#17399,.T.);
#24351=ORIENTED_EDGE('',*,*,#17394,.T.);
#24352=ORIENTED_EDGE('',*,*,#17400,.T.);
#24353=ORIENTED_EDGE('',*,*,#17401,.F.);
#24354=ORIENTED_EDGE('',*,*,#17402,.T.);
#24355=ORIENTED_EDGE('',*,*,#17398,.T.);
#24356=ORIENTED_EDGE('',*,*,#17403,.T.);
#24357=ORIENTED_EDGE('',*,*,#17404,.F.);
#24358=ORIENTED_EDGE('',*,*,#17405,.T.);
#24359=ORIENTED_EDGE('',*,*,#17401,.T.);
#24360=ORIENTED_EDGE('',*,*,#17406,.T.);
#24361=ORIENTED_EDGE('',*,*,#17407,.F.);
#24362=ORIENTED_EDGE('',*,*,#17408,.T.);
#24363=ORIENTED_EDGE('',*,*,#17404,.T.);
#24364=ORIENTED_EDGE('',*,*,#17409,.T.);
#24365=ORIENTED_EDGE('',*,*,#17410,.F.);
#24366=ORIENTED_EDGE('',*,*,#17411,.T.);
#24367=ORIENTED_EDGE('',*,*,#17407,.T.);
#24368=ORIENTED_EDGE('',*,*,#17412,.T.);
#24369=ORIENTED_EDGE('',*,*,#17413,.F.);
#24370=ORIENTED_EDGE('',*,*,#17414,.T.);
#24371=ORIENTED_EDGE('',*,*,#17410,.T.);
#24372=ORIENTED_EDGE('',*,*,#17415,.T.);
#24373=ORIENTED_EDGE('',*,*,#17416,.F.);
#24374=ORIENTED_EDGE('',*,*,#17417,.T.);
#24375=ORIENTED_EDGE('',*,*,#17413,.T.);
#24376=ORIENTED_EDGE('',*,*,#17418,.T.);
#24377=ORIENTED_EDGE('',*,*,#17419,.F.);
#24378=ORIENTED_EDGE('',*,*,#17420,.T.);
#24379=ORIENTED_EDGE('',*,*,#17416,.T.);
#24380=ORIENTED_EDGE('',*,*,#17421,.T.);
#24381=ORIENTED_EDGE('',*,*,#17422,.F.);
#24382=ORIENTED_EDGE('',*,*,#17423,.T.);
#24383=ORIENTED_EDGE('',*,*,#17419,.T.);
#24384=ORIENTED_EDGE('',*,*,#17424,.T.);
#24385=ORIENTED_EDGE('',*,*,#17425,.F.);
#24386=ORIENTED_EDGE('',*,*,#17426,.T.);
#24387=ORIENTED_EDGE('',*,*,#17422,.T.);
#24388=ORIENTED_EDGE('',*,*,#17427,.T.);
#24389=ORIENTED_EDGE('',*,*,#17428,.F.);
#24390=ORIENTED_EDGE('',*,*,#17429,.T.);
#24391=ORIENTED_EDGE('',*,*,#17425,.T.);
#24392=ORIENTED_EDGE('',*,*,#17430,.T.);
#24393=ORIENTED_EDGE('',*,*,#17431,.F.);
#24394=ORIENTED_EDGE('',*,*,#17432,.T.);
#24395=ORIENTED_EDGE('',*,*,#17428,.T.);
#24396=ORIENTED_EDGE('',*,*,#17433,.T.);
#24397=ORIENTED_EDGE('',*,*,#17434,.F.);
#24398=ORIENTED_EDGE('',*,*,#17435,.T.);
#24399=ORIENTED_EDGE('',*,*,#17431,.T.);
#24400=ORIENTED_EDGE('',*,*,#17436,.T.);
#24401=ORIENTED_EDGE('',*,*,#17437,.F.);
#24402=ORIENTED_EDGE('',*,*,#17438,.T.);
#24403=ORIENTED_EDGE('',*,*,#17434,.T.);
#24404=ORIENTED_EDGE('',*,*,#17439,.T.);
#24405=ORIENTED_EDGE('',*,*,#17440,.F.);
#24406=ORIENTED_EDGE('',*,*,#17441,.T.);
#24407=ORIENTED_EDGE('',*,*,#17437,.T.);
#24408=ORIENTED_EDGE('',*,*,#17442,.T.);
#24409=ORIENTED_EDGE('',*,*,#17443,.F.);
#24410=ORIENTED_EDGE('',*,*,#17444,.T.);
#24411=ORIENTED_EDGE('',*,*,#17440,.T.);
#24412=ORIENTED_EDGE('',*,*,#17445,.T.);
#24413=ORIENTED_EDGE('',*,*,#17446,.F.);
#24414=ORIENTED_EDGE('',*,*,#17447,.T.);
#24415=ORIENTED_EDGE('',*,*,#17443,.T.);
#24416=ORIENTED_EDGE('',*,*,#17448,.T.);
#24417=ORIENTED_EDGE('',*,*,#17449,.F.);
#24418=ORIENTED_EDGE('',*,*,#17450,.T.);
#24419=ORIENTED_EDGE('',*,*,#17446,.T.);
#24420=ORIENTED_EDGE('',*,*,#17451,.T.);
#24421=ORIENTED_EDGE('',*,*,#17452,.F.);
#24422=ORIENTED_EDGE('',*,*,#17453,.T.);
#24423=ORIENTED_EDGE('',*,*,#17449,.T.);
#24424=ORIENTED_EDGE('',*,*,#17454,.T.);
#24425=ORIENTED_EDGE('',*,*,#17455,.F.);
#24426=ORIENTED_EDGE('',*,*,#17456,.T.);
#24427=ORIENTED_EDGE('',*,*,#17452,.T.);
#24428=ORIENTED_EDGE('',*,*,#17457,.T.);
#24429=ORIENTED_EDGE('',*,*,#17458,.F.);
#24430=ORIENTED_EDGE('',*,*,#17459,.T.);
#24431=ORIENTED_EDGE('',*,*,#17455,.T.);
#24432=ORIENTED_EDGE('',*,*,#17460,.T.);
#24433=ORIENTED_EDGE('',*,*,#17461,.F.);
#24434=ORIENTED_EDGE('',*,*,#17462,.T.);
#24435=ORIENTED_EDGE('',*,*,#17458,.T.);
#24436=ORIENTED_EDGE('',*,*,#17463,.T.);
#24437=ORIENTED_EDGE('',*,*,#17464,.F.);
#24438=ORIENTED_EDGE('',*,*,#17465,.T.);
#24439=ORIENTED_EDGE('',*,*,#17461,.T.);
#24440=ORIENTED_EDGE('',*,*,#17466,.T.);
#24441=ORIENTED_EDGE('',*,*,#17467,.F.);
#24442=ORIENTED_EDGE('',*,*,#17468,.T.);
#24443=ORIENTED_EDGE('',*,*,#17464,.T.);
#24444=ORIENTED_EDGE('',*,*,#17469,.T.);
#24445=ORIENTED_EDGE('',*,*,#17470,.F.);
#24446=ORIENTED_EDGE('',*,*,#17471,.T.);
#24447=ORIENTED_EDGE('',*,*,#17467,.T.);
#24448=ORIENTED_EDGE('',*,*,#17472,.T.);
#24449=ORIENTED_EDGE('',*,*,#17473,.F.);
#24450=ORIENTED_EDGE('',*,*,#17474,.T.);
#24451=ORIENTED_EDGE('',*,*,#17470,.T.);
#24452=ORIENTED_EDGE('',*,*,#17475,.T.);
#24453=ORIENTED_EDGE('',*,*,#17476,.F.);
#24454=ORIENTED_EDGE('',*,*,#17477,.T.);
#24455=ORIENTED_EDGE('',*,*,#17473,.T.);
#24456=ORIENTED_EDGE('',*,*,#17478,.T.);
#24457=ORIENTED_EDGE('',*,*,#17479,.F.);
#24458=ORIENTED_EDGE('',*,*,#17480,.T.);
#24459=ORIENTED_EDGE('',*,*,#17476,.T.);
#24460=ORIENTED_EDGE('',*,*,#17481,.T.);
#24461=ORIENTED_EDGE('',*,*,#17482,.F.);
#24462=ORIENTED_EDGE('',*,*,#17483,.T.);
#24463=ORIENTED_EDGE('',*,*,#17479,.T.);
#24464=ORIENTED_EDGE('',*,*,#17484,.T.);
#24465=ORIENTED_EDGE('',*,*,#17485,.F.);
#24466=ORIENTED_EDGE('',*,*,#17486,.T.);
#24467=ORIENTED_EDGE('',*,*,#17482,.T.);
#24468=ORIENTED_EDGE('',*,*,#17487,.T.);
#24469=ORIENTED_EDGE('',*,*,#17488,.F.);
#24470=ORIENTED_EDGE('',*,*,#17489,.T.);
#24471=ORIENTED_EDGE('',*,*,#17485,.T.);
#24472=ORIENTED_EDGE('',*,*,#17490,.T.);
#24473=ORIENTED_EDGE('',*,*,#17491,.F.);
#24474=ORIENTED_EDGE('',*,*,#17492,.T.);
#24475=ORIENTED_EDGE('',*,*,#17488,.T.);
#24476=ORIENTED_EDGE('',*,*,#17493,.T.);
#24477=ORIENTED_EDGE('',*,*,#17494,.F.);
#24478=ORIENTED_EDGE('',*,*,#17495,.T.);
#24479=ORIENTED_EDGE('',*,*,#17491,.T.);
#24480=ORIENTED_EDGE('',*,*,#17496,.T.);
#24481=ORIENTED_EDGE('',*,*,#17497,.F.);
#24482=ORIENTED_EDGE('',*,*,#17498,.T.);
#24483=ORIENTED_EDGE('',*,*,#17494,.T.);
#24484=ORIENTED_EDGE('',*,*,#17499,.T.);
#24485=ORIENTED_EDGE('',*,*,#17500,.F.);
#24486=ORIENTED_EDGE('',*,*,#17501,.T.);
#24487=ORIENTED_EDGE('',*,*,#17497,.T.);
#24488=ORIENTED_EDGE('',*,*,#17502,.T.);
#24489=ORIENTED_EDGE('',*,*,#17503,.F.);
#24490=ORIENTED_EDGE('',*,*,#17504,.T.);
#24491=ORIENTED_EDGE('',*,*,#17500,.T.);
#24492=ORIENTED_EDGE('',*,*,#17505,.T.);
#24493=ORIENTED_EDGE('',*,*,#17506,.F.);
#24494=ORIENTED_EDGE('',*,*,#17507,.T.);
#24495=ORIENTED_EDGE('',*,*,#17503,.T.);
#24496=ORIENTED_EDGE('',*,*,#17508,.T.);
#24497=ORIENTED_EDGE('',*,*,#17509,.F.);
#24498=ORIENTED_EDGE('',*,*,#17510,.T.);
#24499=ORIENTED_EDGE('',*,*,#17506,.T.);
#24500=ORIENTED_EDGE('',*,*,#17511,.T.);
#24501=ORIENTED_EDGE('',*,*,#17512,.F.);
#24502=ORIENTED_EDGE('',*,*,#17513,.T.);
#24503=ORIENTED_EDGE('',*,*,#17509,.T.);
#24504=ORIENTED_EDGE('',*,*,#17514,.T.);
#24505=ORIENTED_EDGE('',*,*,#17515,.F.);
#24506=ORIENTED_EDGE('',*,*,#17516,.T.);
#24507=ORIENTED_EDGE('',*,*,#17512,.T.);
#24508=ORIENTED_EDGE('',*,*,#17517,.T.);
#24509=ORIENTED_EDGE('',*,*,#17518,.F.);
#24510=ORIENTED_EDGE('',*,*,#17519,.T.);
#24511=ORIENTED_EDGE('',*,*,#17515,.T.);
#24512=ORIENTED_EDGE('',*,*,#17520,.T.);
#24513=ORIENTED_EDGE('',*,*,#17521,.F.);
#24514=ORIENTED_EDGE('',*,*,#17522,.T.);
#24515=ORIENTED_EDGE('',*,*,#17518,.T.);
#24516=ORIENTED_EDGE('',*,*,#17523,.T.);
#24517=ORIENTED_EDGE('',*,*,#17524,.F.);
#24518=ORIENTED_EDGE('',*,*,#17525,.T.);
#24519=ORIENTED_EDGE('',*,*,#17521,.T.);
#24520=ORIENTED_EDGE('',*,*,#17526,.T.);
#24521=ORIENTED_EDGE('',*,*,#17527,.F.);
#24522=ORIENTED_EDGE('',*,*,#17528,.T.);
#24523=ORIENTED_EDGE('',*,*,#17524,.T.);
#24524=ORIENTED_EDGE('',*,*,#17529,.T.);
#24525=ORIENTED_EDGE('',*,*,#17530,.F.);
#24526=ORIENTED_EDGE('',*,*,#17531,.T.);
#24527=ORIENTED_EDGE('',*,*,#17527,.T.);
#24528=ORIENTED_EDGE('',*,*,#17532,.T.);
#24529=ORIENTED_EDGE('',*,*,#17533,.F.);
#24530=ORIENTED_EDGE('',*,*,#17534,.T.);
#24531=ORIENTED_EDGE('',*,*,#17530,.T.);
#24532=ORIENTED_EDGE('',*,*,#17535,.T.);
#24533=ORIENTED_EDGE('',*,*,#17536,.F.);
#24534=ORIENTED_EDGE('',*,*,#17537,.T.);
#24535=ORIENTED_EDGE('',*,*,#17533,.T.);
#24536=ORIENTED_EDGE('',*,*,#17538,.T.);
#24537=ORIENTED_EDGE('',*,*,#17539,.F.);
#24538=ORIENTED_EDGE('',*,*,#17540,.T.);
#24539=ORIENTED_EDGE('',*,*,#17536,.T.);
#24540=ORIENTED_EDGE('',*,*,#17541,.T.);
#24541=ORIENTED_EDGE('',*,*,#17542,.F.);
#24542=ORIENTED_EDGE('',*,*,#17543,.T.);
#24543=ORIENTED_EDGE('',*,*,#17539,.T.);
#24544=ORIENTED_EDGE('',*,*,#17544,.T.);
#24545=ORIENTED_EDGE('',*,*,#17545,.F.);
#24546=ORIENTED_EDGE('',*,*,#17546,.T.);
#24547=ORIENTED_EDGE('',*,*,#17542,.T.);
#24548=ORIENTED_EDGE('',*,*,#17547,.T.);
#24549=ORIENTED_EDGE('',*,*,#17548,.F.);
#24550=ORIENTED_EDGE('',*,*,#17549,.T.);
#24551=ORIENTED_EDGE('',*,*,#17545,.T.);
#24552=ORIENTED_EDGE('',*,*,#17550,.T.);
#24553=ORIENTED_EDGE('',*,*,#17551,.F.);
#24554=ORIENTED_EDGE('',*,*,#17552,.T.);
#24555=ORIENTED_EDGE('',*,*,#17548,.T.);
#24556=ORIENTED_EDGE('',*,*,#17553,.T.);
#24557=ORIENTED_EDGE('',*,*,#17554,.F.);
#24558=ORIENTED_EDGE('',*,*,#17555,.T.);
#24559=ORIENTED_EDGE('',*,*,#17551,.T.);
#24560=ORIENTED_EDGE('',*,*,#17556,.T.);
#24561=ORIENTED_EDGE('',*,*,#17557,.F.);
#24562=ORIENTED_EDGE('',*,*,#17558,.T.);
#24563=ORIENTED_EDGE('',*,*,#17554,.T.);
#24564=ORIENTED_EDGE('',*,*,#17559,.T.);
#24565=ORIENTED_EDGE('',*,*,#17560,.F.);
#24566=ORIENTED_EDGE('',*,*,#17561,.T.);
#24567=ORIENTED_EDGE('',*,*,#17557,.T.);
#24568=ORIENTED_EDGE('',*,*,#17562,.T.);
#24569=ORIENTED_EDGE('',*,*,#17563,.F.);
#24570=ORIENTED_EDGE('',*,*,#17564,.T.);
#24571=ORIENTED_EDGE('',*,*,#17560,.T.);
#24572=ORIENTED_EDGE('',*,*,#17565,.T.);
#24573=ORIENTED_EDGE('',*,*,#17566,.F.);
#24574=ORIENTED_EDGE('',*,*,#17567,.T.);
#24575=ORIENTED_EDGE('',*,*,#17563,.T.);
#24576=ORIENTED_EDGE('',*,*,#17568,.T.);
#24577=ORIENTED_EDGE('',*,*,#17569,.F.);
#24578=ORIENTED_EDGE('',*,*,#17570,.T.);
#24579=ORIENTED_EDGE('',*,*,#17566,.T.);
#24580=ORIENTED_EDGE('',*,*,#17571,.T.);
#24581=ORIENTED_EDGE('',*,*,#17572,.F.);
#24582=ORIENTED_EDGE('',*,*,#17573,.T.);
#24583=ORIENTED_EDGE('',*,*,#17569,.T.);
#24584=ORIENTED_EDGE('',*,*,#17574,.T.);
#24585=ORIENTED_EDGE('',*,*,#17575,.F.);
#24586=ORIENTED_EDGE('',*,*,#17576,.T.);
#24587=ORIENTED_EDGE('',*,*,#17572,.T.);
#24588=ORIENTED_EDGE('',*,*,#17577,.T.);
#24589=ORIENTED_EDGE('',*,*,#17578,.F.);
#24590=ORIENTED_EDGE('',*,*,#17579,.T.);
#24591=ORIENTED_EDGE('',*,*,#17575,.T.);
#24592=ORIENTED_EDGE('',*,*,#17580,.T.);
#24593=ORIENTED_EDGE('',*,*,#17581,.F.);
#24594=ORIENTED_EDGE('',*,*,#17582,.T.);
#24595=ORIENTED_EDGE('',*,*,#17578,.T.);
#24596=ORIENTED_EDGE('',*,*,#17583,.T.);
#24597=ORIENTED_EDGE('',*,*,#17584,.F.);
#24598=ORIENTED_EDGE('',*,*,#17585,.T.);
#24599=ORIENTED_EDGE('',*,*,#17581,.T.);
#24600=ORIENTED_EDGE('',*,*,#17586,.T.);
#24601=ORIENTED_EDGE('',*,*,#17587,.F.);
#24602=ORIENTED_EDGE('',*,*,#17588,.T.);
#24603=ORIENTED_EDGE('',*,*,#17584,.T.);
#24604=ORIENTED_EDGE('',*,*,#17589,.T.);
#24605=ORIENTED_EDGE('',*,*,#17590,.F.);
#24606=ORIENTED_EDGE('',*,*,#17591,.T.);
#24607=ORIENTED_EDGE('',*,*,#17587,.T.);
#24608=ORIENTED_EDGE('',*,*,#17592,.T.);
#24609=ORIENTED_EDGE('',*,*,#17593,.F.);
#24610=ORIENTED_EDGE('',*,*,#17594,.T.);
#24611=ORIENTED_EDGE('',*,*,#17590,.T.);
#24612=ORIENTED_EDGE('',*,*,#17595,.T.);
#24613=ORIENTED_EDGE('',*,*,#17596,.F.);
#24614=ORIENTED_EDGE('',*,*,#17597,.T.);
#24615=ORIENTED_EDGE('',*,*,#17593,.T.);
#24616=ORIENTED_EDGE('',*,*,#17598,.T.);
#24617=ORIENTED_EDGE('',*,*,#17599,.F.);
#24618=ORIENTED_EDGE('',*,*,#17600,.T.);
#24619=ORIENTED_EDGE('',*,*,#17596,.T.);
#24620=ORIENTED_EDGE('',*,*,#17601,.T.);
#24621=ORIENTED_EDGE('',*,*,#17602,.F.);
#24622=ORIENTED_EDGE('',*,*,#17603,.T.);
#24623=ORIENTED_EDGE('',*,*,#17604,.F.);
#24624=ORIENTED_EDGE('',*,*,#17605,.F.);
#24625=ORIENTED_EDGE('',*,*,#17606,.F.);
#24626=ORIENTED_EDGE('',*,*,#17607,.T.);
#24627=ORIENTED_EDGE('',*,*,#17602,.T.);
#24628=ORIENTED_EDGE('',*,*,#17608,.F.);
#24629=ORIENTED_EDGE('',*,*,#17609,.F.);
#24630=ORIENTED_EDGE('',*,*,#17610,.T.);
#24631=ORIENTED_EDGE('',*,*,#17606,.T.);
#24632=ORIENTED_EDGE('',*,*,#17611,.F.);
#24633=ORIENTED_EDGE('',*,*,#17612,.F.);
#24634=ORIENTED_EDGE('',*,*,#17613,.T.);
#24635=ORIENTED_EDGE('',*,*,#17609,.T.);
#24636=ORIENTED_EDGE('',*,*,#17614,.F.);
#24637=ORIENTED_EDGE('',*,*,#17615,.F.);
#24638=ORIENTED_EDGE('',*,*,#17616,.T.);
#24639=ORIENTED_EDGE('',*,*,#17612,.T.);
#24640=ORIENTED_EDGE('',*,*,#17617,.F.);
#24641=ORIENTED_EDGE('',*,*,#17618,.F.);
#24642=ORIENTED_EDGE('',*,*,#17619,.T.);
#24643=ORIENTED_EDGE('',*,*,#17615,.T.);
#24644=ORIENTED_EDGE('',*,*,#17620,.F.);
#24645=ORIENTED_EDGE('',*,*,#17621,.F.);
#24646=ORIENTED_EDGE('',*,*,#17622,.T.);
#24647=ORIENTED_EDGE('',*,*,#17618,.T.);
#24648=ORIENTED_EDGE('',*,*,#17623,.F.);
#24649=ORIENTED_EDGE('',*,*,#17624,.F.);
#24650=ORIENTED_EDGE('',*,*,#17625,.T.);
#24651=ORIENTED_EDGE('',*,*,#17621,.T.);
#24652=ORIENTED_EDGE('',*,*,#17626,.F.);
#24653=ORIENTED_EDGE('',*,*,#17627,.F.);
#24654=ORIENTED_EDGE('',*,*,#17628,.T.);
#24655=ORIENTED_EDGE('',*,*,#17624,.T.);
#24656=ORIENTED_EDGE('',*,*,#17629,.F.);
#24657=ORIENTED_EDGE('',*,*,#17630,.F.);
#24658=ORIENTED_EDGE('',*,*,#17631,.T.);
#24659=ORIENTED_EDGE('',*,*,#17627,.T.);
#24660=ORIENTED_EDGE('',*,*,#17632,.F.);
#24661=ORIENTED_EDGE('',*,*,#17633,.F.);
#24662=ORIENTED_EDGE('',*,*,#17634,.T.);
#24663=ORIENTED_EDGE('',*,*,#17630,.T.);
#24664=ORIENTED_EDGE('',*,*,#17635,.F.);
#24665=ORIENTED_EDGE('',*,*,#17636,.F.);
#24666=ORIENTED_EDGE('',*,*,#17637,.T.);
#24667=ORIENTED_EDGE('',*,*,#17633,.T.);
#24668=ORIENTED_EDGE('',*,*,#17638,.F.);
#24669=ORIENTED_EDGE('',*,*,#17639,.F.);
#24670=ORIENTED_EDGE('',*,*,#17640,.T.);
#24671=ORIENTED_EDGE('',*,*,#17636,.T.);
#24672=ORIENTED_EDGE('',*,*,#17641,.F.);
#24673=ORIENTED_EDGE('',*,*,#17642,.F.);
#24674=ORIENTED_EDGE('',*,*,#17643,.T.);
#24675=ORIENTED_EDGE('',*,*,#17639,.T.);
#24676=ORIENTED_EDGE('',*,*,#17644,.F.);
#24677=ORIENTED_EDGE('',*,*,#17645,.F.);
#24678=ORIENTED_EDGE('',*,*,#17646,.T.);
#24679=ORIENTED_EDGE('',*,*,#17642,.T.);
#24680=ORIENTED_EDGE('',*,*,#17647,.F.);
#24681=ORIENTED_EDGE('',*,*,#17648,.F.);
#24682=ORIENTED_EDGE('',*,*,#17649,.T.);
#24683=ORIENTED_EDGE('',*,*,#17645,.T.);
#24684=ORIENTED_EDGE('',*,*,#17650,.F.);
#24685=ORIENTED_EDGE('',*,*,#17651,.F.);
#24686=ORIENTED_EDGE('',*,*,#17652,.T.);
#24687=ORIENTED_EDGE('',*,*,#17648,.T.);
#24688=ORIENTED_EDGE('',*,*,#17653,.F.);
#24689=ORIENTED_EDGE('',*,*,#17654,.F.);
#24690=ORIENTED_EDGE('',*,*,#17655,.T.);
#24691=ORIENTED_EDGE('',*,*,#17651,.T.);
#24692=ORIENTED_EDGE('',*,*,#17656,.F.);
#24693=ORIENTED_EDGE('',*,*,#17657,.F.);
#24694=ORIENTED_EDGE('',*,*,#17658,.T.);
#24695=ORIENTED_EDGE('',*,*,#17654,.T.);
#24696=ORIENTED_EDGE('',*,*,#17659,.F.);
#24697=ORIENTED_EDGE('',*,*,#17660,.F.);
#24698=ORIENTED_EDGE('',*,*,#17661,.T.);
#24699=ORIENTED_EDGE('',*,*,#17657,.T.);
#24700=ORIENTED_EDGE('',*,*,#17662,.F.);
#24701=ORIENTED_EDGE('',*,*,#17663,.F.);
#24702=ORIENTED_EDGE('',*,*,#17664,.T.);
#24703=ORIENTED_EDGE('',*,*,#17660,.T.);
#24704=ORIENTED_EDGE('',*,*,#17665,.F.);
#24705=ORIENTED_EDGE('',*,*,#17666,.F.);
#24706=ORIENTED_EDGE('',*,*,#17667,.T.);
#24707=ORIENTED_EDGE('',*,*,#17663,.T.);
#24708=ORIENTED_EDGE('',*,*,#17668,.F.);
#24709=ORIENTED_EDGE('',*,*,#17669,.F.);
#24710=ORIENTED_EDGE('',*,*,#17670,.T.);
#24711=ORIENTED_EDGE('',*,*,#17666,.T.);
#24712=ORIENTED_EDGE('',*,*,#17671,.F.);
#24713=ORIENTED_EDGE('',*,*,#17672,.F.);
#24714=ORIENTED_EDGE('',*,*,#17673,.T.);
#24715=ORIENTED_EDGE('',*,*,#17669,.T.);
#24716=ORIENTED_EDGE('',*,*,#17674,.F.);
#24717=ORIENTED_EDGE('',*,*,#17675,.F.);
#24718=ORIENTED_EDGE('',*,*,#17676,.T.);
#24719=ORIENTED_EDGE('',*,*,#17672,.T.);
#24720=ORIENTED_EDGE('',*,*,#17677,.F.);
#24721=ORIENTED_EDGE('',*,*,#17678,.F.);
#24722=ORIENTED_EDGE('',*,*,#17679,.T.);
#24723=ORIENTED_EDGE('',*,*,#17675,.T.);
#24724=ORIENTED_EDGE('',*,*,#17680,.F.);
#24725=ORIENTED_EDGE('',*,*,#17681,.F.);
#24726=ORIENTED_EDGE('',*,*,#17682,.T.);
#24727=ORIENTED_EDGE('',*,*,#17678,.T.);
#24728=ORIENTED_EDGE('',*,*,#17683,.F.);
#24729=ORIENTED_EDGE('',*,*,#17684,.F.);
#24730=ORIENTED_EDGE('',*,*,#17685,.T.);
#24731=ORIENTED_EDGE('',*,*,#17681,.T.);
#24732=ORIENTED_EDGE('',*,*,#17686,.F.);
#24733=ORIENTED_EDGE('',*,*,#17687,.F.);
#24734=ORIENTED_EDGE('',*,*,#17688,.T.);
#24735=ORIENTED_EDGE('',*,*,#17684,.T.);
#24736=ORIENTED_EDGE('',*,*,#17689,.F.);
#24737=ORIENTED_EDGE('',*,*,#17690,.F.);
#24738=ORIENTED_EDGE('',*,*,#17691,.T.);
#24739=ORIENTED_EDGE('',*,*,#17687,.T.);
#24740=ORIENTED_EDGE('',*,*,#17692,.F.);
#24741=ORIENTED_EDGE('',*,*,#17693,.F.);
#24742=ORIENTED_EDGE('',*,*,#17694,.T.);
#24743=ORIENTED_EDGE('',*,*,#17690,.T.);
#24744=ORIENTED_EDGE('',*,*,#17695,.F.);
#24745=ORIENTED_EDGE('',*,*,#17696,.F.);
#24746=ORIENTED_EDGE('',*,*,#17697,.T.);
#24747=ORIENTED_EDGE('',*,*,#17693,.T.);
#24748=ORIENTED_EDGE('',*,*,#17698,.F.);
#24749=ORIENTED_EDGE('',*,*,#17699,.F.);
#24750=ORIENTED_EDGE('',*,*,#17700,.T.);
#24751=ORIENTED_EDGE('',*,*,#17696,.T.);
#24752=ORIENTED_EDGE('',*,*,#17701,.F.);
#24753=ORIENTED_EDGE('',*,*,#17702,.F.);
#24754=ORIENTED_EDGE('',*,*,#17703,.T.);
#24755=ORIENTED_EDGE('',*,*,#17699,.T.);
#24756=ORIENTED_EDGE('',*,*,#17704,.F.);
#24757=ORIENTED_EDGE('',*,*,#17705,.F.);
#24758=ORIENTED_EDGE('',*,*,#17706,.T.);
#24759=ORIENTED_EDGE('',*,*,#17702,.T.);
#24760=ORIENTED_EDGE('',*,*,#17707,.F.);
#24761=ORIENTED_EDGE('',*,*,#17708,.F.);
#24762=ORIENTED_EDGE('',*,*,#17709,.T.);
#24763=ORIENTED_EDGE('',*,*,#17705,.T.);
#24764=ORIENTED_EDGE('',*,*,#17710,.F.);
#24765=ORIENTED_EDGE('',*,*,#17711,.F.);
#24766=ORIENTED_EDGE('',*,*,#17712,.T.);
#24767=ORIENTED_EDGE('',*,*,#17708,.T.);
#24768=ORIENTED_EDGE('',*,*,#17713,.F.);
#24769=ORIENTED_EDGE('',*,*,#17714,.F.);
#24770=ORIENTED_EDGE('',*,*,#17715,.T.);
#24771=ORIENTED_EDGE('',*,*,#17711,.T.);
#24772=ORIENTED_EDGE('',*,*,#17716,.F.);
#24773=ORIENTED_EDGE('',*,*,#17717,.F.);
#24774=ORIENTED_EDGE('',*,*,#17718,.T.);
#24775=ORIENTED_EDGE('',*,*,#17714,.T.);
#24776=ORIENTED_EDGE('',*,*,#17719,.F.);
#24777=ORIENTED_EDGE('',*,*,#17720,.F.);
#24778=ORIENTED_EDGE('',*,*,#17721,.T.);
#24779=ORIENTED_EDGE('',*,*,#17717,.T.);
#24780=ORIENTED_EDGE('',*,*,#17722,.F.);
#24781=ORIENTED_EDGE('',*,*,#17723,.F.);
#24782=ORIENTED_EDGE('',*,*,#17724,.T.);
#24783=ORIENTED_EDGE('',*,*,#17720,.T.);
#24784=ORIENTED_EDGE('',*,*,#17725,.F.);
#24785=ORIENTED_EDGE('',*,*,#17726,.F.);
#24786=ORIENTED_EDGE('',*,*,#17727,.T.);
#24787=ORIENTED_EDGE('',*,*,#17723,.T.);
#24788=ORIENTED_EDGE('',*,*,#17728,.F.);
#24789=ORIENTED_EDGE('',*,*,#17729,.F.);
#24790=ORIENTED_EDGE('',*,*,#17730,.T.);
#24791=ORIENTED_EDGE('',*,*,#17726,.T.);
#24792=ORIENTED_EDGE('',*,*,#17731,.F.);
#24793=ORIENTED_EDGE('',*,*,#17732,.F.);
#24794=ORIENTED_EDGE('',*,*,#17733,.T.);
#24795=ORIENTED_EDGE('',*,*,#17729,.T.);
#24796=ORIENTED_EDGE('',*,*,#17734,.F.);
#24797=ORIENTED_EDGE('',*,*,#17735,.F.);
#24798=ORIENTED_EDGE('',*,*,#17736,.T.);
#24799=ORIENTED_EDGE('',*,*,#17732,.T.);
#24800=ORIENTED_EDGE('',*,*,#17737,.F.);
#24801=ORIENTED_EDGE('',*,*,#17738,.F.);
#24802=ORIENTED_EDGE('',*,*,#17739,.T.);
#24803=ORIENTED_EDGE('',*,*,#17735,.T.);
#24804=ORIENTED_EDGE('',*,*,#17740,.F.);
#24805=ORIENTED_EDGE('',*,*,#17741,.F.);
#24806=ORIENTED_EDGE('',*,*,#17742,.T.);
#24807=ORIENTED_EDGE('',*,*,#17738,.T.);
#24808=ORIENTED_EDGE('',*,*,#17743,.F.);
#24809=ORIENTED_EDGE('',*,*,#17744,.F.);
#24810=ORIENTED_EDGE('',*,*,#17745,.T.);
#24811=ORIENTED_EDGE('',*,*,#17741,.T.);
#24812=ORIENTED_EDGE('',*,*,#17746,.F.);
#24813=ORIENTED_EDGE('',*,*,#17747,.F.);
#24814=ORIENTED_EDGE('',*,*,#17748,.T.);
#24815=ORIENTED_EDGE('',*,*,#17744,.T.);
#24816=ORIENTED_EDGE('',*,*,#17749,.F.);
#24817=ORIENTED_EDGE('',*,*,#17750,.F.);
#24818=ORIENTED_EDGE('',*,*,#17751,.T.);
#24819=ORIENTED_EDGE('',*,*,#17747,.T.);
#24820=ORIENTED_EDGE('',*,*,#17752,.F.);
#24821=ORIENTED_EDGE('',*,*,#17753,.F.);
#24822=ORIENTED_EDGE('',*,*,#17754,.T.);
#24823=ORIENTED_EDGE('',*,*,#17750,.T.);
#24824=ORIENTED_EDGE('',*,*,#17755,.F.);
#24825=ORIENTED_EDGE('',*,*,#17756,.F.);
#24826=ORIENTED_EDGE('',*,*,#17757,.T.);
#24827=ORIENTED_EDGE('',*,*,#17753,.T.);
#24828=ORIENTED_EDGE('',*,*,#17758,.F.);
#24829=ORIENTED_EDGE('',*,*,#17759,.F.);
#24830=ORIENTED_EDGE('',*,*,#17760,.T.);
#24831=ORIENTED_EDGE('',*,*,#17756,.T.);
#24832=ORIENTED_EDGE('',*,*,#17761,.F.);
#24833=ORIENTED_EDGE('',*,*,#17762,.F.);
#24834=ORIENTED_EDGE('',*,*,#17763,.T.);
#24835=ORIENTED_EDGE('',*,*,#17759,.T.);
#24836=ORIENTED_EDGE('',*,*,#17764,.F.);
#24837=ORIENTED_EDGE('',*,*,#17765,.F.);
#24838=ORIENTED_EDGE('',*,*,#17766,.T.);
#24839=ORIENTED_EDGE('',*,*,#17762,.T.);
#24840=ORIENTED_EDGE('',*,*,#17767,.F.);
#24841=ORIENTED_EDGE('',*,*,#17768,.F.);
#24842=ORIENTED_EDGE('',*,*,#17769,.T.);
#24843=ORIENTED_EDGE('',*,*,#17765,.T.);
#24844=ORIENTED_EDGE('',*,*,#17770,.F.);
#24845=ORIENTED_EDGE('',*,*,#17771,.F.);
#24846=ORIENTED_EDGE('',*,*,#17772,.T.);
#24847=ORIENTED_EDGE('',*,*,#17768,.T.);
#24848=ORIENTED_EDGE('',*,*,#17773,.F.);
#24849=ORIENTED_EDGE('',*,*,#17774,.F.);
#24850=ORIENTED_EDGE('',*,*,#17775,.T.);
#24851=ORIENTED_EDGE('',*,*,#17771,.T.);
#24852=ORIENTED_EDGE('',*,*,#17776,.F.);
#24853=ORIENTED_EDGE('',*,*,#17777,.F.);
#24854=ORIENTED_EDGE('',*,*,#17778,.T.);
#24855=ORIENTED_EDGE('',*,*,#17774,.T.);
#24856=ORIENTED_EDGE('',*,*,#17779,.F.);
#24857=ORIENTED_EDGE('',*,*,#17780,.F.);
#24858=ORIENTED_EDGE('',*,*,#17781,.T.);
#24859=ORIENTED_EDGE('',*,*,#17777,.T.);
#24860=ORIENTED_EDGE('',*,*,#17782,.F.);
#24861=ORIENTED_EDGE('',*,*,#17783,.F.);
#24862=ORIENTED_EDGE('',*,*,#17784,.T.);
#24863=ORIENTED_EDGE('',*,*,#17780,.T.);
#24864=ORIENTED_EDGE('',*,*,#17785,.F.);
#24865=ORIENTED_EDGE('',*,*,#17786,.F.);
#24866=ORIENTED_EDGE('',*,*,#17787,.T.);
#24867=ORIENTED_EDGE('',*,*,#17783,.T.);
#24868=ORIENTED_EDGE('',*,*,#17788,.F.);
#24869=ORIENTED_EDGE('',*,*,#17789,.F.);
#24870=ORIENTED_EDGE('',*,*,#17790,.T.);
#24871=ORIENTED_EDGE('',*,*,#17786,.T.);
#24872=ORIENTED_EDGE('',*,*,#17791,.F.);
#24873=ORIENTED_EDGE('',*,*,#17792,.F.);
#24874=ORIENTED_EDGE('',*,*,#17793,.T.);
#24875=ORIENTED_EDGE('',*,*,#17789,.T.);
#24876=ORIENTED_EDGE('',*,*,#17794,.F.);
#24877=ORIENTED_EDGE('',*,*,#17795,.F.);
#24878=ORIENTED_EDGE('',*,*,#17796,.T.);
#24879=ORIENTED_EDGE('',*,*,#17792,.T.);
#24880=ORIENTED_EDGE('',*,*,#17797,.F.);
#24881=ORIENTED_EDGE('',*,*,#17798,.F.);
#24882=ORIENTED_EDGE('',*,*,#17799,.T.);
#24883=ORIENTED_EDGE('',*,*,#17795,.T.);
#24884=ORIENTED_EDGE('',*,*,#17800,.F.);
#24885=ORIENTED_EDGE('',*,*,#17801,.F.);
#24886=ORIENTED_EDGE('',*,*,#17802,.T.);
#24887=ORIENTED_EDGE('',*,*,#17798,.T.);
#24888=ORIENTED_EDGE('',*,*,#17803,.F.);
#24889=ORIENTED_EDGE('',*,*,#17804,.F.);
#24890=ORIENTED_EDGE('',*,*,#17805,.T.);
#24891=ORIENTED_EDGE('',*,*,#17801,.T.);
#24892=ORIENTED_EDGE('',*,*,#17806,.F.);
#24893=ORIENTED_EDGE('',*,*,#17807,.F.);
#24894=ORIENTED_EDGE('',*,*,#17808,.T.);
#24895=ORIENTED_EDGE('',*,*,#17804,.T.);
#24896=ORIENTED_EDGE('',*,*,#17809,.F.);
#24897=ORIENTED_EDGE('',*,*,#17604,.T.);
#24898=ORIENTED_EDGE('',*,*,#17810,.T.);
#24899=ORIENTED_EDGE('',*,*,#17811,.F.);
#24900=ORIENTED_EDGE('',*,*,#17812,.F.);
#24901=ORIENTED_EDGE('',*,*,#17813,.T.);
#24902=ORIENTED_EDGE('',*,*,#17813,.F.);
#24903=ORIENTED_EDGE('',*,*,#17814,.F.);
#24904=ORIENTED_EDGE('',*,*,#17601,.F.);
#24905=ORIENTED_EDGE('',*,*,#17598,.F.);
#24906=ORIENTED_EDGE('',*,*,#17595,.F.);
#24907=ORIENTED_EDGE('',*,*,#17592,.F.);
#24908=ORIENTED_EDGE('',*,*,#17589,.F.);
#24909=ORIENTED_EDGE('',*,*,#17586,.F.);
#24910=ORIENTED_EDGE('',*,*,#17583,.F.);
#24911=ORIENTED_EDGE('',*,*,#17580,.F.);
#24912=ORIENTED_EDGE('',*,*,#17577,.F.);
#24913=ORIENTED_EDGE('',*,*,#17574,.F.);
#24914=ORIENTED_EDGE('',*,*,#17571,.F.);
#24915=ORIENTED_EDGE('',*,*,#17568,.F.);
#24916=ORIENTED_EDGE('',*,*,#17565,.F.);
#24917=ORIENTED_EDGE('',*,*,#17562,.F.);
#24918=ORIENTED_EDGE('',*,*,#17559,.F.);
#24919=ORIENTED_EDGE('',*,*,#17556,.F.);
#24920=ORIENTED_EDGE('',*,*,#17553,.F.);
#24921=ORIENTED_EDGE('',*,*,#17550,.F.);
#24922=ORIENTED_EDGE('',*,*,#17547,.F.);
#24923=ORIENTED_EDGE('',*,*,#17544,.F.);
#24924=ORIENTED_EDGE('',*,*,#17541,.F.);
#24925=ORIENTED_EDGE('',*,*,#17538,.F.);
#24926=ORIENTED_EDGE('',*,*,#17535,.F.);
#24927=ORIENTED_EDGE('',*,*,#17532,.F.);
#24928=ORIENTED_EDGE('',*,*,#17529,.F.);
#24929=ORIENTED_EDGE('',*,*,#17526,.F.);
#24930=ORIENTED_EDGE('',*,*,#17523,.F.);
#24931=ORIENTED_EDGE('',*,*,#17520,.F.);
#24932=ORIENTED_EDGE('',*,*,#17517,.F.);
#24933=ORIENTED_EDGE('',*,*,#17514,.F.);
#24934=ORIENTED_EDGE('',*,*,#17511,.F.);
#24935=ORIENTED_EDGE('',*,*,#17508,.F.);
#24936=ORIENTED_EDGE('',*,*,#17505,.F.);
#24937=ORIENTED_EDGE('',*,*,#17502,.F.);
#24938=ORIENTED_EDGE('',*,*,#17499,.F.);
#24939=ORIENTED_EDGE('',*,*,#17496,.F.);
#24940=ORIENTED_EDGE('',*,*,#17493,.F.);
#24941=ORIENTED_EDGE('',*,*,#17490,.F.);
#24942=ORIENTED_EDGE('',*,*,#17487,.F.);
#24943=ORIENTED_EDGE('',*,*,#17484,.F.);
#24944=ORIENTED_EDGE('',*,*,#17481,.F.);
#24945=ORIENTED_EDGE('',*,*,#17478,.F.);
#24946=ORIENTED_EDGE('',*,*,#17475,.F.);
#24947=ORIENTED_EDGE('',*,*,#17472,.F.);
#24948=ORIENTED_EDGE('',*,*,#17469,.F.);
#24949=ORIENTED_EDGE('',*,*,#17466,.F.);
#24950=ORIENTED_EDGE('',*,*,#17463,.F.);
#24951=ORIENTED_EDGE('',*,*,#17460,.F.);
#24952=ORIENTED_EDGE('',*,*,#17457,.F.);
#24953=ORIENTED_EDGE('',*,*,#17454,.F.);
#24954=ORIENTED_EDGE('',*,*,#17451,.F.);
#24955=ORIENTED_EDGE('',*,*,#17448,.F.);
#24956=ORIENTED_EDGE('',*,*,#17445,.F.);
#24957=ORIENTED_EDGE('',*,*,#17442,.F.);
#24958=ORIENTED_EDGE('',*,*,#17439,.F.);
#24959=ORIENTED_EDGE('',*,*,#17436,.F.);
#24960=ORIENTED_EDGE('',*,*,#17433,.F.);
#24961=ORIENTED_EDGE('',*,*,#17430,.F.);
#24962=ORIENTED_EDGE('',*,*,#17427,.F.);
#24963=ORIENTED_EDGE('',*,*,#17424,.F.);
#24964=ORIENTED_EDGE('',*,*,#17421,.F.);
#24965=ORIENTED_EDGE('',*,*,#17418,.F.);
#24966=ORIENTED_EDGE('',*,*,#17415,.F.);
#24967=ORIENTED_EDGE('',*,*,#17412,.F.);
#24968=ORIENTED_EDGE('',*,*,#17409,.F.);
#24969=ORIENTED_EDGE('',*,*,#17406,.F.);
#24970=ORIENTED_EDGE('',*,*,#17403,.F.);
#24971=ORIENTED_EDGE('',*,*,#17400,.F.);
#24972=ORIENTED_EDGE('',*,*,#17397,.F.);
#24973=ORIENTED_EDGE('',*,*,#17815,.F.);
#24974=ORIENTED_EDGE('',*,*,#17816,.T.);
#24975=ORIENTED_EDGE('',*,*,#17809,.T.);
#24976=ORIENTED_EDGE('',*,*,#17806,.T.);
#24977=ORIENTED_EDGE('',*,*,#17803,.T.);
#24978=ORIENTED_EDGE('',*,*,#17800,.T.);
#24979=ORIENTED_EDGE('',*,*,#17797,.T.);
#24980=ORIENTED_EDGE('',*,*,#17794,.T.);
#24981=ORIENTED_EDGE('',*,*,#17791,.T.);
#24982=ORIENTED_EDGE('',*,*,#17788,.T.);
#24983=ORIENTED_EDGE('',*,*,#17785,.T.);
#24984=ORIENTED_EDGE('',*,*,#17782,.T.);
#24985=ORIENTED_EDGE('',*,*,#17779,.T.);
#24986=ORIENTED_EDGE('',*,*,#17776,.T.);
#24987=ORIENTED_EDGE('',*,*,#17773,.T.);
#24988=ORIENTED_EDGE('',*,*,#17770,.T.);
#24989=ORIENTED_EDGE('',*,*,#17767,.T.);
#24990=ORIENTED_EDGE('',*,*,#17764,.T.);
#24991=ORIENTED_EDGE('',*,*,#17761,.T.);
#24992=ORIENTED_EDGE('',*,*,#17758,.T.);
#24993=ORIENTED_EDGE('',*,*,#17755,.T.);
#24994=ORIENTED_EDGE('',*,*,#17752,.T.);
#24995=ORIENTED_EDGE('',*,*,#17749,.T.);
#24996=ORIENTED_EDGE('',*,*,#17746,.T.);
#24997=ORIENTED_EDGE('',*,*,#17743,.T.);
#24998=ORIENTED_EDGE('',*,*,#17740,.T.);
#24999=ORIENTED_EDGE('',*,*,#17737,.T.);
#25000=ORIENTED_EDGE('',*,*,#17734,.T.);
#25001=ORIENTED_EDGE('',*,*,#17731,.T.);
#25002=ORIENTED_EDGE('',*,*,#17728,.T.);
#25003=ORIENTED_EDGE('',*,*,#17725,.T.);
#25004=ORIENTED_EDGE('',*,*,#17722,.T.);
#25005=ORIENTED_EDGE('',*,*,#17719,.T.);
#25006=ORIENTED_EDGE('',*,*,#17716,.T.);
#25007=ORIENTED_EDGE('',*,*,#17713,.T.);
#25008=ORIENTED_EDGE('',*,*,#17710,.T.);
#25009=ORIENTED_EDGE('',*,*,#17707,.T.);
#25010=ORIENTED_EDGE('',*,*,#17704,.T.);
#25011=ORIENTED_EDGE('',*,*,#17701,.T.);
#25012=ORIENTED_EDGE('',*,*,#17698,.T.);
#25013=ORIENTED_EDGE('',*,*,#17695,.T.);
#25014=ORIENTED_EDGE('',*,*,#17692,.T.);
#25015=ORIENTED_EDGE('',*,*,#17689,.T.);
#25016=ORIENTED_EDGE('',*,*,#17686,.T.);
#25017=ORIENTED_EDGE('',*,*,#17683,.T.);
#25018=ORIENTED_EDGE('',*,*,#17680,.T.);
#25019=ORIENTED_EDGE('',*,*,#17677,.T.);
#25020=ORIENTED_EDGE('',*,*,#17674,.T.);
#25021=ORIENTED_EDGE('',*,*,#17671,.T.);
#25022=ORIENTED_EDGE('',*,*,#17668,.T.);
#25023=ORIENTED_EDGE('',*,*,#17665,.T.);
#25024=ORIENTED_EDGE('',*,*,#17662,.T.);
#25025=ORIENTED_EDGE('',*,*,#17659,.T.);
#25026=ORIENTED_EDGE('',*,*,#17656,.T.);
#25027=ORIENTED_EDGE('',*,*,#17653,.T.);
#25028=ORIENTED_EDGE('',*,*,#17650,.T.);
#25029=ORIENTED_EDGE('',*,*,#17647,.T.);
#25030=ORIENTED_EDGE('',*,*,#17644,.T.);
#25031=ORIENTED_EDGE('',*,*,#17641,.T.);
#25032=ORIENTED_EDGE('',*,*,#17638,.T.);
#25033=ORIENTED_EDGE('',*,*,#17635,.T.);
#25034=ORIENTED_EDGE('',*,*,#17632,.T.);
#25035=ORIENTED_EDGE('',*,*,#17629,.T.);
#25036=ORIENTED_EDGE('',*,*,#17626,.T.);
#25037=ORIENTED_EDGE('',*,*,#17623,.T.);
#25038=ORIENTED_EDGE('',*,*,#17620,.T.);
#25039=ORIENTED_EDGE('',*,*,#17617,.T.);
#25040=ORIENTED_EDGE('',*,*,#17614,.T.);
#25041=ORIENTED_EDGE('',*,*,#17611,.T.);
#25042=ORIENTED_EDGE('',*,*,#17608,.T.);
#25043=ORIENTED_EDGE('',*,*,#17605,.T.);
#25044=ORIENTED_EDGE('',*,*,#17817,.T.);
#25045=ORIENTED_EDGE('',*,*,#17818,.T.);
#25046=ORIENTED_EDGE('',*,*,#17819,.T.);
#25047=ORIENTED_EDGE('',*,*,#17820,.T.);
#25048=ORIENTED_EDGE('',*,*,#17815,.T.);
#25049=ORIENTED_EDGE('',*,*,#17807,.T.);
#25050=ORIENTED_EDGE('',*,*,#17816,.F.);
#25051=ORIENTED_EDGE('',*,*,#17820,.F.);
#25052=ORIENTED_EDGE('',*,*,#17821,.T.);
#25053=ORIENTED_EDGE('',*,*,#17810,.F.);
#25054=ORIENTED_EDGE('',*,*,#17603,.F.);
#25055=ORIENTED_EDGE('',*,*,#17607,.F.);
#25056=ORIENTED_EDGE('',*,*,#17610,.F.);
#25057=ORIENTED_EDGE('',*,*,#17613,.F.);
#25058=ORIENTED_EDGE('',*,*,#17616,.F.);
#25059=ORIENTED_EDGE('',*,*,#17619,.F.);
#25060=ORIENTED_EDGE('',*,*,#17622,.F.);
#25061=ORIENTED_EDGE('',*,*,#17625,.F.);
#25062=ORIENTED_EDGE('',*,*,#17628,.F.);
#25063=ORIENTED_EDGE('',*,*,#17631,.F.);
#25064=ORIENTED_EDGE('',*,*,#17634,.F.);
#25065=ORIENTED_EDGE('',*,*,#17637,.F.);
#25066=ORIENTED_EDGE('',*,*,#17640,.F.);
#25067=ORIENTED_EDGE('',*,*,#17643,.F.);
#25068=ORIENTED_EDGE('',*,*,#17646,.F.);
#25069=ORIENTED_EDGE('',*,*,#17649,.F.);
#25070=ORIENTED_EDGE('',*,*,#17652,.F.);
#25071=ORIENTED_EDGE('',*,*,#17655,.F.);
#25072=ORIENTED_EDGE('',*,*,#17658,.F.);
#25073=ORIENTED_EDGE('',*,*,#17661,.F.);
#25074=ORIENTED_EDGE('',*,*,#17664,.F.);
#25075=ORIENTED_EDGE('',*,*,#17667,.F.);
#25076=ORIENTED_EDGE('',*,*,#17670,.F.);
#25077=ORIENTED_EDGE('',*,*,#17673,.F.);
#25078=ORIENTED_EDGE('',*,*,#17676,.F.);
#25079=ORIENTED_EDGE('',*,*,#17679,.F.);
#25080=ORIENTED_EDGE('',*,*,#17682,.F.);
#25081=ORIENTED_EDGE('',*,*,#17685,.F.);
#25082=ORIENTED_EDGE('',*,*,#17688,.F.);
#25083=ORIENTED_EDGE('',*,*,#17691,.F.);
#25084=ORIENTED_EDGE('',*,*,#17694,.F.);
#25085=ORIENTED_EDGE('',*,*,#17697,.F.);
#25086=ORIENTED_EDGE('',*,*,#17700,.F.);
#25087=ORIENTED_EDGE('',*,*,#17703,.F.);
#25088=ORIENTED_EDGE('',*,*,#17706,.F.);
#25089=ORIENTED_EDGE('',*,*,#17709,.F.);
#25090=ORIENTED_EDGE('',*,*,#17712,.F.);
#25091=ORIENTED_EDGE('',*,*,#17715,.F.);
#25092=ORIENTED_EDGE('',*,*,#17718,.F.);
#25093=ORIENTED_EDGE('',*,*,#17721,.F.);
#25094=ORIENTED_EDGE('',*,*,#17724,.F.);
#25095=ORIENTED_EDGE('',*,*,#17727,.F.);
#25096=ORIENTED_EDGE('',*,*,#17730,.F.);
#25097=ORIENTED_EDGE('',*,*,#17733,.F.);
#25098=ORIENTED_EDGE('',*,*,#17736,.F.);
#25099=ORIENTED_EDGE('',*,*,#17739,.F.);
#25100=ORIENTED_EDGE('',*,*,#17742,.F.);
#25101=ORIENTED_EDGE('',*,*,#17745,.F.);
#25102=ORIENTED_EDGE('',*,*,#17748,.F.);
#25103=ORIENTED_EDGE('',*,*,#17751,.F.);
#25104=ORIENTED_EDGE('',*,*,#17754,.F.);
#25105=ORIENTED_EDGE('',*,*,#17757,.F.);
#25106=ORIENTED_EDGE('',*,*,#17760,.F.);
#25107=ORIENTED_EDGE('',*,*,#17763,.F.);
#25108=ORIENTED_EDGE('',*,*,#17766,.F.);
#25109=ORIENTED_EDGE('',*,*,#17769,.F.);
#25110=ORIENTED_EDGE('',*,*,#17772,.F.);
#25111=ORIENTED_EDGE('',*,*,#17775,.F.);
#25112=ORIENTED_EDGE('',*,*,#17778,.F.);
#25113=ORIENTED_EDGE('',*,*,#17781,.F.);
#25114=ORIENTED_EDGE('',*,*,#17784,.F.);
#25115=ORIENTED_EDGE('',*,*,#17787,.F.);
#25116=ORIENTED_EDGE('',*,*,#17790,.F.);
#25117=ORIENTED_EDGE('',*,*,#17793,.F.);
#25118=ORIENTED_EDGE('',*,*,#17796,.F.);
#25119=ORIENTED_EDGE('',*,*,#17799,.F.);
#25120=ORIENTED_EDGE('',*,*,#17802,.F.);
#25121=ORIENTED_EDGE('',*,*,#17805,.F.);
#25122=ORIENTED_EDGE('',*,*,#17808,.F.);
#25123=ORIENTED_EDGE('',*,*,#17821,.F.);
#25124=ORIENTED_EDGE('',*,*,#17819,.F.);
#25125=ORIENTED_EDGE('',*,*,#17395,.F.);
#25126=ORIENTED_EDGE('',*,*,#17399,.F.);
#25127=ORIENTED_EDGE('',*,*,#17402,.F.);
#25128=ORIENTED_EDGE('',*,*,#17405,.F.);
#25129=ORIENTED_EDGE('',*,*,#17408,.F.);
#25130=ORIENTED_EDGE('',*,*,#17411,.F.);
#25131=ORIENTED_EDGE('',*,*,#17414,.F.);
#25132=ORIENTED_EDGE('',*,*,#17417,.F.);
#25133=ORIENTED_EDGE('',*,*,#17420,.F.);
#25134=ORIENTED_EDGE('',*,*,#17423,.F.);
#25135=ORIENTED_EDGE('',*,*,#17426,.F.);
#25136=ORIENTED_EDGE('',*,*,#17429,.F.);
#25137=ORIENTED_EDGE('',*,*,#17432,.F.);
#25138=ORIENTED_EDGE('',*,*,#17435,.F.);
#25139=ORIENTED_EDGE('',*,*,#17438,.F.);
#25140=ORIENTED_EDGE('',*,*,#17441,.F.);
#25141=ORIENTED_EDGE('',*,*,#17444,.F.);
#25142=ORIENTED_EDGE('',*,*,#17447,.F.);
#25143=ORIENTED_EDGE('',*,*,#17450,.F.);
#25144=ORIENTED_EDGE('',*,*,#17453,.F.);
#25145=ORIENTED_EDGE('',*,*,#17456,.F.);
#25146=ORIENTED_EDGE('',*,*,#17459,.F.);
#25147=ORIENTED_EDGE('',*,*,#17462,.F.);
#25148=ORIENTED_EDGE('',*,*,#17465,.F.);
#25149=ORIENTED_EDGE('',*,*,#17468,.F.);
#25150=ORIENTED_EDGE('',*,*,#17471,.F.);
#25151=ORIENTED_EDGE('',*,*,#17474,.F.);
#25152=ORIENTED_EDGE('',*,*,#17477,.F.);
#25153=ORIENTED_EDGE('',*,*,#17480,.F.);
#25154=ORIENTED_EDGE('',*,*,#17483,.F.);
#25155=ORIENTED_EDGE('',*,*,#17486,.F.);
#25156=ORIENTED_EDGE('',*,*,#17489,.F.);
#25157=ORIENTED_EDGE('',*,*,#17492,.F.);
#25158=ORIENTED_EDGE('',*,*,#17495,.F.);
#25159=ORIENTED_EDGE('',*,*,#17498,.F.);
#25160=ORIENTED_EDGE('',*,*,#17501,.F.);
#25161=ORIENTED_EDGE('',*,*,#17504,.F.);
#25162=ORIENTED_EDGE('',*,*,#17507,.F.);
#25163=ORIENTED_EDGE('',*,*,#17510,.F.);
#25164=ORIENTED_EDGE('',*,*,#17513,.F.);
#25165=ORIENTED_EDGE('',*,*,#17516,.F.);
#25166=ORIENTED_EDGE('',*,*,#17519,.F.);
#25167=ORIENTED_EDGE('',*,*,#17522,.F.);
#25168=ORIENTED_EDGE('',*,*,#17525,.F.);
#25169=ORIENTED_EDGE('',*,*,#17528,.F.);
#25170=ORIENTED_EDGE('',*,*,#17531,.F.);
#25171=ORIENTED_EDGE('',*,*,#17534,.F.);
#25172=ORIENTED_EDGE('',*,*,#17537,.F.);
#25173=ORIENTED_EDGE('',*,*,#17540,.F.);
#25174=ORIENTED_EDGE('',*,*,#17543,.F.);
#25175=ORIENTED_EDGE('',*,*,#17546,.F.);
#25176=ORIENTED_EDGE('',*,*,#17549,.F.);
#25177=ORIENTED_EDGE('',*,*,#17552,.F.);
#25178=ORIENTED_EDGE('',*,*,#17555,.F.);
#25179=ORIENTED_EDGE('',*,*,#17558,.F.);
#25180=ORIENTED_EDGE('',*,*,#17561,.F.);
#25181=ORIENTED_EDGE('',*,*,#17564,.F.);
#25182=ORIENTED_EDGE('',*,*,#17567,.F.);
#25183=ORIENTED_EDGE('',*,*,#17570,.F.);
#25184=ORIENTED_EDGE('',*,*,#17573,.F.);
#25185=ORIENTED_EDGE('',*,*,#17576,.F.);
#25186=ORIENTED_EDGE('',*,*,#17579,.F.);
#25187=ORIENTED_EDGE('',*,*,#17582,.F.);
#25188=ORIENTED_EDGE('',*,*,#17585,.F.);
#25189=ORIENTED_EDGE('',*,*,#17588,.F.);
#25190=ORIENTED_EDGE('',*,*,#17591,.F.);
#25191=ORIENTED_EDGE('',*,*,#17594,.F.);
#25192=ORIENTED_EDGE('',*,*,#17597,.F.);
#25193=ORIENTED_EDGE('',*,*,#17600,.F.);
#25194=ORIENTED_EDGE('',*,*,#17822,.F.);
#25195=ORIENTED_EDGE('',*,*,#17812,.T.);
#25196=ORIENTED_EDGE('',*,*,#17823,.T.);
#25197=ORIENTED_EDGE('',*,*,#17824,.T.);
#25198=ORIENTED_EDGE('',*,*,#17823,.F.);
#25199=ORIENTED_EDGE('',*,*,#17811,.T.);
#25200=ORIENTED_EDGE('',*,*,#17825,.T.);
#25201=ORIENTED_EDGE('',*,*,#17599,.T.);
#25202=ORIENTED_EDGE('',*,*,#17814,.T.);
#25203=ORIENTED_EDGE('',*,*,#17825,.F.);
#25204=ORIENTED_EDGE('',*,*,#17822,.T.);
#25205=ORIENTED_EDGE('',*,*,#17826,.F.);
#25206=ORIENTED_EDGE('',*,*,#17824,.F.);
#25207=ORIENTED_EDGE('',*,*,#17827,.F.);
#25208=ORIENTED_EDGE('',*,*,#17828,.T.);
#25209=ORIENTED_EDGE('',*,*,#17829,.F.);
#25210=ORIENTED_EDGE('',*,*,#17830,.F.);
#25211=ORIENTED_EDGE('',*,*,#17831,.F.);
#25212=ORIENTED_EDGE('',*,*,#17830,.T.);
#25213=ORIENTED_EDGE('',*,*,#17832,.T.);
#25214=ORIENTED_EDGE('',*,*,#17833,.F.);
#25215=ORIENTED_EDGE('',*,*,#17832,.F.);
#25216=ORIENTED_EDGE('',*,*,#17829,.T.);
#25217=ORIENTED_EDGE('',*,*,#17834,.T.);
#25218=ORIENTED_EDGE('',*,*,#17835,.F.);
#25219=ORIENTED_EDGE('',*,*,#17834,.F.);
#25220=ORIENTED_EDGE('',*,*,#17828,.F.);
#25221=ORIENTED_EDGE('',*,*,#17836,.F.);
#25222=ORIENTED_EDGE('',*,*,#17837,.T.);
#25223=ORIENTED_EDGE('',*,*,#17838,.F.);
#25224=ORIENTED_EDGE('',*,*,#17839,.F.);
#25225=ORIENTED_EDGE('',*,*,#17840,.F.);
#25226=ORIENTED_EDGE('',*,*,#17839,.T.);
#25227=ORIENTED_EDGE('',*,*,#17841,.T.);
#25228=ORIENTED_EDGE('',*,*,#17842,.F.);
#25229=ORIENTED_EDGE('',*,*,#17841,.F.);
#25230=ORIENTED_EDGE('',*,*,#17838,.T.);
#25231=ORIENTED_EDGE('',*,*,#17843,.T.);
#25232=ORIENTED_EDGE('',*,*,#17844,.F.);
#25233=ORIENTED_EDGE('',*,*,#17843,.F.);
#25234=ORIENTED_EDGE('',*,*,#17837,.F.);
#25235=ORIENTED_EDGE('',*,*,#17845,.F.);
#25236=ORIENTED_EDGE('',*,*,#17846,.T.);
#25237=ORIENTED_EDGE('',*,*,#17847,.F.);
#25238=ORIENTED_EDGE('',*,*,#17848,.F.);
#25239=ORIENTED_EDGE('',*,*,#17849,.F.);
#25240=ORIENTED_EDGE('',*,*,#17848,.T.);
#25241=ORIENTED_EDGE('',*,*,#17850,.T.);
#25242=ORIENTED_EDGE('',*,*,#17851,.F.);
#25243=ORIENTED_EDGE('',*,*,#17850,.F.);
#25244=ORIENTED_EDGE('',*,*,#17847,.T.);
#25245=ORIENTED_EDGE('',*,*,#17852,.T.);
#25246=ORIENTED_EDGE('',*,*,#17853,.F.);
#25247=ORIENTED_EDGE('',*,*,#17852,.F.);
#25248=ORIENTED_EDGE('',*,*,#17846,.F.);
#25249=ORIENTED_EDGE('',*,*,#17854,.F.);
#25250=ORIENTED_EDGE('',*,*,#17855,.T.);
#25251=ORIENTED_EDGE('',*,*,#17856,.F.);
#25252=ORIENTED_EDGE('',*,*,#17857,.F.);
#25253=ORIENTED_EDGE('',*,*,#17858,.F.);
#25254=ORIENTED_EDGE('',*,*,#17857,.T.);
#25255=ORIENTED_EDGE('',*,*,#17859,.T.);
#25256=ORIENTED_EDGE('',*,*,#17860,.F.);
#25257=ORIENTED_EDGE('',*,*,#17859,.F.);
#25258=ORIENTED_EDGE('',*,*,#17856,.T.);
#25259=ORIENTED_EDGE('',*,*,#17861,.T.);
#25260=ORIENTED_EDGE('',*,*,#17862,.F.);
#25261=ORIENTED_EDGE('',*,*,#17861,.F.);
#25262=ORIENTED_EDGE('',*,*,#17855,.F.);
#25263=ORIENTED_EDGE('',*,*,#17863,.F.);
#25264=ORIENTED_EDGE('',*,*,#17864,.T.);
#25265=ORIENTED_EDGE('',*,*,#17865,.F.);
#25266=ORIENTED_EDGE('',*,*,#17866,.F.);
#25267=ORIENTED_EDGE('',*,*,#17867,.F.);
#25268=ORIENTED_EDGE('',*,*,#17866,.T.);
#25269=ORIENTED_EDGE('',*,*,#17868,.T.);
#25270=ORIENTED_EDGE('',*,*,#17869,.F.);
#25271=ORIENTED_EDGE('',*,*,#17868,.F.);
#25272=ORIENTED_EDGE('',*,*,#17865,.T.);
#25273=ORIENTED_EDGE('',*,*,#17870,.T.);
#25274=ORIENTED_EDGE('',*,*,#17871,.F.);
#25275=ORIENTED_EDGE('',*,*,#17870,.F.);
#25276=ORIENTED_EDGE('',*,*,#17864,.F.);
#25277=ORIENTED_EDGE('',*,*,#17872,.F.);
#25278=ORIENTED_EDGE('',*,*,#17873,.T.);
#25279=ORIENTED_EDGE('',*,*,#17874,.F.);
#25280=ORIENTED_EDGE('',*,*,#17875,.F.);
#25281=ORIENTED_EDGE('',*,*,#17876,.F.);
#25282=ORIENTED_EDGE('',*,*,#17875,.T.);
#25283=ORIENTED_EDGE('',*,*,#17877,.T.);
#25284=ORIENTED_EDGE('',*,*,#17878,.F.);
#25285=ORIENTED_EDGE('',*,*,#17877,.F.);
#25286=ORIENTED_EDGE('',*,*,#17874,.T.);
#25287=ORIENTED_EDGE('',*,*,#17879,.T.);
#25288=ORIENTED_EDGE('',*,*,#17880,.F.);
#25289=ORIENTED_EDGE('',*,*,#17879,.F.);
#25290=ORIENTED_EDGE('',*,*,#17873,.F.);
#25291=ORIENTED_EDGE('',*,*,#17881,.F.);
#25292=ORIENTED_EDGE('',*,*,#17882,.T.);
#25293=ORIENTED_EDGE('',*,*,#17883,.F.);
#25294=ORIENTED_EDGE('',*,*,#17884,.F.);
#25295=ORIENTED_EDGE('',*,*,#17885,.F.);
#25296=ORIENTED_EDGE('',*,*,#17884,.T.);
#25297=ORIENTED_EDGE('',*,*,#17886,.T.);
#25298=ORIENTED_EDGE('',*,*,#17887,.F.);
#25299=ORIENTED_EDGE('',*,*,#17886,.F.);
#25300=ORIENTED_EDGE('',*,*,#17883,.T.);
#25301=ORIENTED_EDGE('',*,*,#17888,.T.);
#25302=ORIENTED_EDGE('',*,*,#17889,.F.);
#25303=ORIENTED_EDGE('',*,*,#17888,.F.);
#25304=ORIENTED_EDGE('',*,*,#17882,.F.);
#25305=ORIENTED_EDGE('',*,*,#17890,.F.);
#25306=ORIENTED_EDGE('',*,*,#17891,.T.);
#25307=ORIENTED_EDGE('',*,*,#17892,.F.);
#25308=ORIENTED_EDGE('',*,*,#17893,.F.);
#25309=ORIENTED_EDGE('',*,*,#17894,.F.);
#25310=ORIENTED_EDGE('',*,*,#17893,.T.);
#25311=ORIENTED_EDGE('',*,*,#17895,.T.);
#25312=ORIENTED_EDGE('',*,*,#17896,.F.);
#25313=ORIENTED_EDGE('',*,*,#17895,.F.);
#25314=ORIENTED_EDGE('',*,*,#17892,.T.);
#25315=ORIENTED_EDGE('',*,*,#17897,.T.);
#25316=ORIENTED_EDGE('',*,*,#17898,.F.);
#25317=ORIENTED_EDGE('',*,*,#17897,.F.);
#25318=ORIENTED_EDGE('',*,*,#17891,.F.);
#25319=ORIENTED_EDGE('',*,*,#17899,.F.);
#25320=ORIENTED_EDGE('',*,*,#17900,.T.);
#25321=ORIENTED_EDGE('',*,*,#17901,.F.);
#25322=ORIENTED_EDGE('',*,*,#17902,.F.);
#25323=ORIENTED_EDGE('',*,*,#17903,.F.);
#25324=ORIENTED_EDGE('',*,*,#17902,.T.);
#25325=ORIENTED_EDGE('',*,*,#17904,.T.);
#25326=ORIENTED_EDGE('',*,*,#17905,.F.);
#25327=ORIENTED_EDGE('',*,*,#17904,.F.);
#25328=ORIENTED_EDGE('',*,*,#17901,.T.);
#25329=ORIENTED_EDGE('',*,*,#17906,.T.);
#25330=ORIENTED_EDGE('',*,*,#17907,.F.);
#25331=ORIENTED_EDGE('',*,*,#17906,.F.);
#25332=ORIENTED_EDGE('',*,*,#17900,.F.);
#25333=ORIENTED_EDGE('',*,*,#17908,.F.);
#25334=ORIENTED_EDGE('',*,*,#17909,.T.);
#25335=ORIENTED_EDGE('',*,*,#17910,.F.);
#25336=ORIENTED_EDGE('',*,*,#17911,.F.);
#25337=ORIENTED_EDGE('',*,*,#17912,.F.);
#25338=ORIENTED_EDGE('',*,*,#17911,.T.);
#25339=ORIENTED_EDGE('',*,*,#17913,.T.);
#25340=ORIENTED_EDGE('',*,*,#17914,.F.);
#25341=ORIENTED_EDGE('',*,*,#17913,.F.);
#25342=ORIENTED_EDGE('',*,*,#17910,.T.);
#25343=ORIENTED_EDGE('',*,*,#17915,.T.);
#25344=ORIENTED_EDGE('',*,*,#17916,.F.);
#25345=ORIENTED_EDGE('',*,*,#17915,.F.);
#25346=ORIENTED_EDGE('',*,*,#17909,.F.);
#25347=ORIENTED_EDGE('',*,*,#17917,.F.);
#25348=ORIENTED_EDGE('',*,*,#17918,.T.);
#25349=ORIENTED_EDGE('',*,*,#17919,.F.);
#25350=ORIENTED_EDGE('',*,*,#17920,.F.);
#25351=ORIENTED_EDGE('',*,*,#17921,.F.);
#25352=ORIENTED_EDGE('',*,*,#17920,.T.);
#25353=ORIENTED_EDGE('',*,*,#17922,.T.);
#25354=ORIENTED_EDGE('',*,*,#17923,.F.);
#25355=ORIENTED_EDGE('',*,*,#17922,.F.);
#25356=ORIENTED_EDGE('',*,*,#17919,.T.);
#25357=ORIENTED_EDGE('',*,*,#17924,.T.);
#25358=ORIENTED_EDGE('',*,*,#17925,.F.);
#25359=ORIENTED_EDGE('',*,*,#17924,.F.);
#25360=ORIENTED_EDGE('',*,*,#17918,.F.);
#25361=ORIENTED_EDGE('',*,*,#17926,.F.);
#25362=ORIENTED_EDGE('',*,*,#17927,.T.);
#25363=ORIENTED_EDGE('',*,*,#17928,.F.);
#25364=ORIENTED_EDGE('',*,*,#17929,.F.);
#25365=ORIENTED_EDGE('',*,*,#17930,.F.);
#25366=ORIENTED_EDGE('',*,*,#17929,.T.);
#25367=ORIENTED_EDGE('',*,*,#17931,.T.);
#25368=ORIENTED_EDGE('',*,*,#17932,.F.);
#25369=ORIENTED_EDGE('',*,*,#17931,.F.);
#25370=ORIENTED_EDGE('',*,*,#17928,.T.);
#25371=ORIENTED_EDGE('',*,*,#17933,.T.);
#25372=ORIENTED_EDGE('',*,*,#17934,.F.);
#25373=ORIENTED_EDGE('',*,*,#17933,.F.);
#25374=ORIENTED_EDGE('',*,*,#17927,.F.);
#25375=ORIENTED_EDGE('',*,*,#17935,.F.);
#25376=ORIENTED_EDGE('',*,*,#17936,.T.);
#25377=ORIENTED_EDGE('',*,*,#17937,.F.);
#25378=ORIENTED_EDGE('',*,*,#17938,.F.);
#25379=ORIENTED_EDGE('',*,*,#17939,.F.);
#25380=ORIENTED_EDGE('',*,*,#17938,.T.);
#25381=ORIENTED_EDGE('',*,*,#17940,.T.);
#25382=ORIENTED_EDGE('',*,*,#17941,.F.);
#25383=ORIENTED_EDGE('',*,*,#17940,.F.);
#25384=ORIENTED_EDGE('',*,*,#17937,.T.);
#25385=ORIENTED_EDGE('',*,*,#17942,.T.);
#25386=ORIENTED_EDGE('',*,*,#17943,.F.);
#25387=ORIENTED_EDGE('',*,*,#17942,.F.);
#25388=ORIENTED_EDGE('',*,*,#17936,.F.);
#25389=ORIENTED_EDGE('',*,*,#17944,.F.);
#25390=ORIENTED_EDGE('',*,*,#17945,.T.);
#25391=ORIENTED_EDGE('',*,*,#17946,.F.);
#25392=ORIENTED_EDGE('',*,*,#17947,.F.);
#25393=ORIENTED_EDGE('',*,*,#17948,.F.);
#25394=ORIENTED_EDGE('',*,*,#17947,.T.);
#25395=ORIENTED_EDGE('',*,*,#17949,.T.);
#25396=ORIENTED_EDGE('',*,*,#17950,.F.);
#25397=ORIENTED_EDGE('',*,*,#17949,.F.);
#25398=ORIENTED_EDGE('',*,*,#17946,.T.);
#25399=ORIENTED_EDGE('',*,*,#17951,.T.);
#25400=ORIENTED_EDGE('',*,*,#17952,.F.);
#25401=ORIENTED_EDGE('',*,*,#17951,.F.);
#25402=ORIENTED_EDGE('',*,*,#17945,.F.);
#25403=ORIENTED_EDGE('',*,*,#17953,.F.);
#25404=ORIENTED_EDGE('',*,*,#17954,.T.);
#25405=ORIENTED_EDGE('',*,*,#17955,.F.);
#25406=ORIENTED_EDGE('',*,*,#17956,.F.);
#25407=ORIENTED_EDGE('',*,*,#17957,.F.);
#25408=ORIENTED_EDGE('',*,*,#17956,.T.);
#25409=ORIENTED_EDGE('',*,*,#17958,.T.);
#25410=ORIENTED_EDGE('',*,*,#17959,.F.);
#25411=ORIENTED_EDGE('',*,*,#17958,.F.);
#25412=ORIENTED_EDGE('',*,*,#17955,.T.);
#25413=ORIENTED_EDGE('',*,*,#17960,.T.);
#25414=ORIENTED_EDGE('',*,*,#17961,.F.);
#25415=ORIENTED_EDGE('',*,*,#17960,.F.);
#25416=ORIENTED_EDGE('',*,*,#17954,.F.);
#25417=ORIENTED_EDGE('',*,*,#17962,.F.);
#25418=ORIENTED_EDGE('',*,*,#17963,.T.);
#25419=ORIENTED_EDGE('',*,*,#17964,.F.);
#25420=ORIENTED_EDGE('',*,*,#17965,.F.);
#25421=ORIENTED_EDGE('',*,*,#17966,.F.);
#25422=ORIENTED_EDGE('',*,*,#17965,.T.);
#25423=ORIENTED_EDGE('',*,*,#17967,.T.);
#25424=ORIENTED_EDGE('',*,*,#17968,.F.);
#25425=ORIENTED_EDGE('',*,*,#17967,.F.);
#25426=ORIENTED_EDGE('',*,*,#17964,.T.);
#25427=ORIENTED_EDGE('',*,*,#17969,.T.);
#25428=ORIENTED_EDGE('',*,*,#17970,.F.);
#25429=ORIENTED_EDGE('',*,*,#17969,.F.);
#25430=ORIENTED_EDGE('',*,*,#17963,.F.);
#25431=ORIENTED_EDGE('',*,*,#17971,.F.);
#25432=ORIENTED_EDGE('',*,*,#17972,.T.);
#25433=ORIENTED_EDGE('',*,*,#17973,.F.);
#25434=ORIENTED_EDGE('',*,*,#17974,.F.);
#25435=ORIENTED_EDGE('',*,*,#17975,.F.);
#25436=ORIENTED_EDGE('',*,*,#17974,.T.);
#25437=ORIENTED_EDGE('',*,*,#17976,.T.);
#25438=ORIENTED_EDGE('',*,*,#17977,.F.);
#25439=ORIENTED_EDGE('',*,*,#17976,.F.);
#25440=ORIENTED_EDGE('',*,*,#17973,.T.);
#25441=ORIENTED_EDGE('',*,*,#17978,.T.);
#25442=ORIENTED_EDGE('',*,*,#17979,.F.);
#25443=ORIENTED_EDGE('',*,*,#17978,.F.);
#25444=ORIENTED_EDGE('',*,*,#17972,.F.);
#25445=ORIENTED_EDGE('',*,*,#17980,.F.);
#25446=ORIENTED_EDGE('',*,*,#17981,.T.);
#25447=ORIENTED_EDGE('',*,*,#17982,.F.);
#25448=ORIENTED_EDGE('',*,*,#17983,.F.);
#25449=ORIENTED_EDGE('',*,*,#17984,.F.);
#25450=ORIENTED_EDGE('',*,*,#17983,.T.);
#25451=ORIENTED_EDGE('',*,*,#17985,.T.);
#25452=ORIENTED_EDGE('',*,*,#17986,.F.);
#25453=ORIENTED_EDGE('',*,*,#17987,.F.);
#25454=ORIENTED_EDGE('',*,*,#17985,.F.);
#25455=ORIENTED_EDGE('',*,*,#17982,.T.);
#25456=ORIENTED_EDGE('',*,*,#17988,.T.);
#25457=ORIENTED_EDGE('',*,*,#17989,.F.);
#25458=ORIENTED_EDGE('',*,*,#17988,.F.);
#25459=ORIENTED_EDGE('',*,*,#17981,.F.);
#25460=ORIENTED_EDGE('',*,*,#17990,.F.);
#25461=ORIENTED_EDGE('',*,*,#17991,.F.);
#25462=ORIENTED_EDGE('',*,*,#17992,.T.);
#25463=ORIENTED_EDGE('',*,*,#17993,.F.);
#25464=ORIENTED_EDGE('',*,*,#17994,.F.);
#25465=ORIENTED_EDGE('',*,*,#17995,.F.);
#25466=ORIENTED_EDGE('',*,*,#17994,.T.);
#25467=ORIENTED_EDGE('',*,*,#17996,.T.);
#25468=ORIENTED_EDGE('',*,*,#17997,.F.);
#25469=ORIENTED_EDGE('',*,*,#17996,.F.);
#25470=ORIENTED_EDGE('',*,*,#17993,.T.);
#25471=ORIENTED_EDGE('',*,*,#17998,.T.);
#25472=ORIENTED_EDGE('',*,*,#17999,.F.);
#25473=ORIENTED_EDGE('',*,*,#17998,.F.);
#25474=ORIENTED_EDGE('',*,*,#17992,.F.);
#25475=ORIENTED_EDGE('',*,*,#18000,.F.);
#25476=ORIENTED_EDGE('',*,*,#18001,.T.);
#25477=ORIENTED_EDGE('',*,*,#18002,.F.);
#25478=ORIENTED_EDGE('',*,*,#18003,.F.);
#25479=ORIENTED_EDGE('',*,*,#18004,.F.);
#25480=ORIENTED_EDGE('',*,*,#18003,.T.);
#25481=ORIENTED_EDGE('',*,*,#18005,.T.);
#25482=ORIENTED_EDGE('',*,*,#18006,.F.);
#25483=ORIENTED_EDGE('',*,*,#18005,.F.);
#25484=ORIENTED_EDGE('',*,*,#18002,.T.);
#25485=ORIENTED_EDGE('',*,*,#18007,.T.);
#25486=ORIENTED_EDGE('',*,*,#18008,.F.);
#25487=ORIENTED_EDGE('',*,*,#18007,.F.);
#25488=ORIENTED_EDGE('',*,*,#18001,.F.);
#25489=ORIENTED_EDGE('',*,*,#18009,.F.);
#25490=ORIENTED_EDGE('',*,*,#18010,.T.);
#25491=ORIENTED_EDGE('',*,*,#18011,.F.);
#25492=ORIENTED_EDGE('',*,*,#18012,.F.);
#25493=ORIENTED_EDGE('',*,*,#18013,.F.);
#25494=ORIENTED_EDGE('',*,*,#18012,.T.);
#25495=ORIENTED_EDGE('',*,*,#18014,.T.);
#25496=ORIENTED_EDGE('',*,*,#18015,.F.);
#25497=ORIENTED_EDGE('',*,*,#18014,.F.);
#25498=ORIENTED_EDGE('',*,*,#18011,.T.);
#25499=ORIENTED_EDGE('',*,*,#18016,.T.);
#25500=ORIENTED_EDGE('',*,*,#18017,.F.);
#25501=ORIENTED_EDGE('',*,*,#18016,.F.);
#25502=ORIENTED_EDGE('',*,*,#18010,.F.);
#25503=ORIENTED_EDGE('',*,*,#18018,.F.);
#25504=ORIENTED_EDGE('',*,*,#18019,.T.);
#25505=ORIENTED_EDGE('',*,*,#18020,.F.);
#25506=ORIENTED_EDGE('',*,*,#18021,.F.);
#25507=ORIENTED_EDGE('',*,*,#18022,.F.);
#25508=ORIENTED_EDGE('',*,*,#18021,.T.);
#25509=ORIENTED_EDGE('',*,*,#18023,.T.);
#25510=ORIENTED_EDGE('',*,*,#18024,.F.);
#25511=ORIENTED_EDGE('',*,*,#18023,.F.);
#25512=ORIENTED_EDGE('',*,*,#18020,.T.);
#25513=ORIENTED_EDGE('',*,*,#18025,.T.);
#25514=ORIENTED_EDGE('',*,*,#18026,.F.);
#25515=ORIENTED_EDGE('',*,*,#18025,.F.);
#25516=ORIENTED_EDGE('',*,*,#18019,.F.);
#25517=ORIENTED_EDGE('',*,*,#18027,.F.);
#25518=ORIENTED_EDGE('',*,*,#18028,.T.);
#25519=ORIENTED_EDGE('',*,*,#18029,.F.);
#25520=ORIENTED_EDGE('',*,*,#18030,.F.);
#25521=ORIENTED_EDGE('',*,*,#18031,.F.);
#25522=ORIENTED_EDGE('',*,*,#18030,.T.);
#25523=ORIENTED_EDGE('',*,*,#18032,.T.);
#25524=ORIENTED_EDGE('',*,*,#18033,.F.);
#25525=ORIENTED_EDGE('',*,*,#18032,.F.);
#25526=ORIENTED_EDGE('',*,*,#18029,.T.);
#25527=ORIENTED_EDGE('',*,*,#18034,.T.);
#25528=ORIENTED_EDGE('',*,*,#18035,.F.);
#25529=ORIENTED_EDGE('',*,*,#18034,.F.);
#25530=ORIENTED_EDGE('',*,*,#18028,.F.);
#25531=ORIENTED_EDGE('',*,*,#18036,.F.);
#25532=ORIENTED_EDGE('',*,*,#18037,.T.);
#25533=ORIENTED_EDGE('',*,*,#18038,.F.);
#25534=ORIENTED_EDGE('',*,*,#18039,.F.);
#25535=ORIENTED_EDGE('',*,*,#18040,.F.);
#25536=ORIENTED_EDGE('',*,*,#18039,.T.);
#25537=ORIENTED_EDGE('',*,*,#18041,.T.);
#25538=ORIENTED_EDGE('',*,*,#18042,.F.);
#25539=ORIENTED_EDGE('',*,*,#18041,.F.);
#25540=ORIENTED_EDGE('',*,*,#18038,.T.);
#25541=ORIENTED_EDGE('',*,*,#18043,.T.);
#25542=ORIENTED_EDGE('',*,*,#18044,.F.);
#25543=ORIENTED_EDGE('',*,*,#18043,.F.);
#25544=ORIENTED_EDGE('',*,*,#18037,.F.);
#25545=ORIENTED_EDGE('',*,*,#18045,.F.);
#25546=ORIENTED_EDGE('',*,*,#18046,.T.);
#25547=ORIENTED_EDGE('',*,*,#18047,.F.);
#25548=ORIENTED_EDGE('',*,*,#18048,.F.);
#25549=ORIENTED_EDGE('',*,*,#18049,.F.);
#25550=ORIENTED_EDGE('',*,*,#18048,.T.);
#25551=ORIENTED_EDGE('',*,*,#18050,.T.);
#25552=ORIENTED_EDGE('',*,*,#18051,.F.);
#25553=ORIENTED_EDGE('',*,*,#18050,.F.);
#25554=ORIENTED_EDGE('',*,*,#18047,.T.);
#25555=ORIENTED_EDGE('',*,*,#18052,.T.);
#25556=ORIENTED_EDGE('',*,*,#18053,.F.);
#25557=ORIENTED_EDGE('',*,*,#18052,.F.);
#25558=ORIENTED_EDGE('',*,*,#18046,.F.);
#25559=ORIENTED_EDGE('',*,*,#18054,.F.);
#25560=ORIENTED_EDGE('',*,*,#18055,.T.);
#25561=ORIENTED_EDGE('',*,*,#18056,.F.);
#25562=ORIENTED_EDGE('',*,*,#18057,.F.);
#25563=ORIENTED_EDGE('',*,*,#18058,.F.);
#25564=ORIENTED_EDGE('',*,*,#18057,.T.);
#25565=ORIENTED_EDGE('',*,*,#18059,.T.);
#25566=ORIENTED_EDGE('',*,*,#18060,.F.);
#25567=ORIENTED_EDGE('',*,*,#18059,.F.);
#25568=ORIENTED_EDGE('',*,*,#18056,.T.);
#25569=ORIENTED_EDGE('',*,*,#18061,.T.);
#25570=ORIENTED_EDGE('',*,*,#18062,.F.);
#25571=ORIENTED_EDGE('',*,*,#18061,.F.);
#25572=ORIENTED_EDGE('',*,*,#18055,.F.);
#25573=ORIENTED_EDGE('',*,*,#18063,.F.);
#25574=ORIENTED_EDGE('',*,*,#18064,.T.);
#25575=ORIENTED_EDGE('',*,*,#18065,.F.);
#25576=ORIENTED_EDGE('',*,*,#18066,.F.);
#25577=ORIENTED_EDGE('',*,*,#18067,.F.);
#25578=ORIENTED_EDGE('',*,*,#18066,.T.);
#25579=ORIENTED_EDGE('',*,*,#18068,.T.);
#25580=ORIENTED_EDGE('',*,*,#18069,.F.);
#25581=ORIENTED_EDGE('',*,*,#18068,.F.);
#25582=ORIENTED_EDGE('',*,*,#18065,.T.);
#25583=ORIENTED_EDGE('',*,*,#18070,.T.);
#25584=ORIENTED_EDGE('',*,*,#18071,.F.);
#25585=ORIENTED_EDGE('',*,*,#18070,.F.);
#25586=ORIENTED_EDGE('',*,*,#18064,.F.);
#25587=ORIENTED_EDGE('',*,*,#18072,.F.);
#25588=ORIENTED_EDGE('',*,*,#18073,.T.);
#25589=ORIENTED_EDGE('',*,*,#18074,.F.);
#25590=ORIENTED_EDGE('',*,*,#18075,.F.);
#25591=ORIENTED_EDGE('',*,*,#18076,.F.);
#25592=ORIENTED_EDGE('',*,*,#18075,.T.);
#25593=ORIENTED_EDGE('',*,*,#18077,.T.);
#25594=ORIENTED_EDGE('',*,*,#18078,.F.);
#25595=ORIENTED_EDGE('',*,*,#18077,.F.);
#25596=ORIENTED_EDGE('',*,*,#18074,.T.);
#25597=ORIENTED_EDGE('',*,*,#18079,.T.);
#25598=ORIENTED_EDGE('',*,*,#18080,.F.);
#25599=ORIENTED_EDGE('',*,*,#18079,.F.);
#25600=ORIENTED_EDGE('',*,*,#18073,.F.);
#25601=ORIENTED_EDGE('',*,*,#18081,.F.);
#25602=ORIENTED_EDGE('',*,*,#18082,.T.);
#25603=ORIENTED_EDGE('',*,*,#18083,.F.);
#25604=ORIENTED_EDGE('',*,*,#18084,.F.);
#25605=ORIENTED_EDGE('',*,*,#18085,.F.);
#25606=ORIENTED_EDGE('',*,*,#18084,.T.);
#25607=ORIENTED_EDGE('',*,*,#18086,.T.);
#25608=ORIENTED_EDGE('',*,*,#18087,.F.);
#25609=ORIENTED_EDGE('',*,*,#18086,.F.);
#25610=ORIENTED_EDGE('',*,*,#18083,.T.);
#25611=ORIENTED_EDGE('',*,*,#18088,.T.);
#25612=ORIENTED_EDGE('',*,*,#18089,.F.);
#25613=ORIENTED_EDGE('',*,*,#18088,.F.);
#25614=ORIENTED_EDGE('',*,*,#18082,.F.);
#25615=ORIENTED_EDGE('',*,*,#18090,.F.);
#25616=ORIENTED_EDGE('',*,*,#18091,.T.);
#25617=ORIENTED_EDGE('',*,*,#18092,.F.);
#25618=ORIENTED_EDGE('',*,*,#18093,.F.);
#25619=ORIENTED_EDGE('',*,*,#18094,.F.);
#25620=ORIENTED_EDGE('',*,*,#18093,.T.);
#25621=ORIENTED_EDGE('',*,*,#18095,.T.);
#25622=ORIENTED_EDGE('',*,*,#18096,.F.);
#25623=ORIENTED_EDGE('',*,*,#18095,.F.);
#25624=ORIENTED_EDGE('',*,*,#18092,.T.);
#25625=ORIENTED_EDGE('',*,*,#18097,.T.);
#25626=ORIENTED_EDGE('',*,*,#18098,.F.);
#25627=ORIENTED_EDGE('',*,*,#18097,.F.);
#25628=ORIENTED_EDGE('',*,*,#18091,.F.);
#25629=ORIENTED_EDGE('',*,*,#18099,.F.);
#25630=ORIENTED_EDGE('',*,*,#18100,.T.);
#25631=ORIENTED_EDGE('',*,*,#18101,.F.);
#25632=ORIENTED_EDGE('',*,*,#18102,.F.);
#25633=ORIENTED_EDGE('',*,*,#18103,.F.);
#25634=ORIENTED_EDGE('',*,*,#18102,.T.);
#25635=ORIENTED_EDGE('',*,*,#18104,.T.);
#25636=ORIENTED_EDGE('',*,*,#18105,.F.);
#25637=ORIENTED_EDGE('',*,*,#18104,.F.);
#25638=ORIENTED_EDGE('',*,*,#18101,.T.);
#25639=ORIENTED_EDGE('',*,*,#18106,.T.);
#25640=ORIENTED_EDGE('',*,*,#18107,.F.);
#25641=ORIENTED_EDGE('',*,*,#18106,.F.);
#25642=ORIENTED_EDGE('',*,*,#18100,.F.);
#25643=ORIENTED_EDGE('',*,*,#18108,.F.);
#25644=ORIENTED_EDGE('',*,*,#18109,.T.);
#25645=ORIENTED_EDGE('',*,*,#18110,.F.);
#25646=ORIENTED_EDGE('',*,*,#18111,.F.);
#25647=ORIENTED_EDGE('',*,*,#18112,.F.);
#25648=ORIENTED_EDGE('',*,*,#18111,.T.);
#25649=ORIENTED_EDGE('',*,*,#18113,.T.);
#25650=ORIENTED_EDGE('',*,*,#18114,.F.);
#25651=ORIENTED_EDGE('',*,*,#18113,.F.);
#25652=ORIENTED_EDGE('',*,*,#18110,.T.);
#25653=ORIENTED_EDGE('',*,*,#18115,.T.);
#25654=ORIENTED_EDGE('',*,*,#18116,.F.);
#25655=ORIENTED_EDGE('',*,*,#18115,.F.);
#25656=ORIENTED_EDGE('',*,*,#18109,.F.);
#25657=ORIENTED_EDGE('',*,*,#18117,.F.);
#25658=ORIENTED_EDGE('',*,*,#18118,.T.);
#25659=ORIENTED_EDGE('',*,*,#18119,.F.);
#25660=ORIENTED_EDGE('',*,*,#18120,.F.);
#25661=ORIENTED_EDGE('',*,*,#18121,.F.);
#25662=ORIENTED_EDGE('',*,*,#18120,.T.);
#25663=ORIENTED_EDGE('',*,*,#18122,.T.);
#25664=ORIENTED_EDGE('',*,*,#18123,.F.);
#25665=ORIENTED_EDGE('',*,*,#18122,.F.);
#25666=ORIENTED_EDGE('',*,*,#18119,.T.);
#25667=ORIENTED_EDGE('',*,*,#18124,.T.);
#25668=ORIENTED_EDGE('',*,*,#18125,.F.);
#25669=ORIENTED_EDGE('',*,*,#18124,.F.);
#25670=ORIENTED_EDGE('',*,*,#18118,.F.);
#25671=ORIENTED_EDGE('',*,*,#18126,.F.);
#25672=ORIENTED_EDGE('',*,*,#18127,.T.);
#25673=ORIENTED_EDGE('',*,*,#18128,.F.);
#25674=ORIENTED_EDGE('',*,*,#18129,.F.);
#25675=ORIENTED_EDGE('',*,*,#18130,.F.);
#25676=ORIENTED_EDGE('',*,*,#18129,.T.);
#25677=ORIENTED_EDGE('',*,*,#18131,.T.);
#25678=ORIENTED_EDGE('',*,*,#18132,.F.);
#25679=ORIENTED_EDGE('',*,*,#18131,.F.);
#25680=ORIENTED_EDGE('',*,*,#18128,.T.);
#25681=ORIENTED_EDGE('',*,*,#18133,.T.);
#25682=ORIENTED_EDGE('',*,*,#18134,.F.);
#25683=ORIENTED_EDGE('',*,*,#18133,.F.);
#25684=ORIENTED_EDGE('',*,*,#18127,.F.);
#25685=ORIENTED_EDGE('',*,*,#18135,.F.);
#25686=ORIENTED_EDGE('',*,*,#18136,.T.);
#25687=ORIENTED_EDGE('',*,*,#18137,.F.);
#25688=ORIENTED_EDGE('',*,*,#18138,.F.);
#25689=ORIENTED_EDGE('',*,*,#18139,.F.);
#25690=ORIENTED_EDGE('',*,*,#18138,.T.);
#25691=ORIENTED_EDGE('',*,*,#18140,.T.);
#25692=ORIENTED_EDGE('',*,*,#18141,.F.);
#25693=ORIENTED_EDGE('',*,*,#18140,.F.);
#25694=ORIENTED_EDGE('',*,*,#18137,.T.);
#25695=ORIENTED_EDGE('',*,*,#18142,.T.);
#25696=ORIENTED_EDGE('',*,*,#18143,.F.);
#25697=ORIENTED_EDGE('',*,*,#18142,.F.);
#25698=ORIENTED_EDGE('',*,*,#18136,.F.);
#25699=ORIENTED_EDGE('',*,*,#18144,.F.);
#25700=ORIENTED_EDGE('',*,*,#18145,.T.);
#25701=ORIENTED_EDGE('',*,*,#18146,.F.);
#25702=ORIENTED_EDGE('',*,*,#18147,.F.);
#25703=ORIENTED_EDGE('',*,*,#18148,.F.);
#25704=ORIENTED_EDGE('',*,*,#18147,.T.);
#25705=ORIENTED_EDGE('',*,*,#18149,.T.);
#25706=ORIENTED_EDGE('',*,*,#18150,.F.);
#25707=ORIENTED_EDGE('',*,*,#18149,.F.);
#25708=ORIENTED_EDGE('',*,*,#18146,.T.);
#25709=ORIENTED_EDGE('',*,*,#18151,.T.);
#25710=ORIENTED_EDGE('',*,*,#18152,.F.);
#25711=ORIENTED_EDGE('',*,*,#18151,.F.);
#25712=ORIENTED_EDGE('',*,*,#18145,.F.);
#25713=ORIENTED_EDGE('',*,*,#18153,.T.);
#25714=ORIENTED_EDGE('',*,*,#18154,.F.);
#25715=ORIENTED_EDGE('',*,*,#18153,.F.);
#25716=ORIENTED_EDGE('',*,*,#18155,.F.);
#25717=ORIENTED_EDGE('',*,*,#18156,.T.);
#25718=ORIENTED_EDGE('',*,*,#18157,.T.);
#25719=ORIENTED_EDGE('',*,*,#18158,.F.);
#25720=ORIENTED_EDGE('',*,*,#18159,.F.);
#25721=ORIENTED_EDGE('',*,*,#18160,.T.);
#25722=ORIENTED_EDGE('',*,*,#18161,.T.);
#25723=ORIENTED_EDGE('',*,*,#18156,.F.);
#25724=ORIENTED_EDGE('',*,*,#18162,.F.);
#25725=ORIENTED_EDGE('',*,*,#18163,.T.);
#25726=ORIENTED_EDGE('',*,*,#18164,.T.);
#25727=ORIENTED_EDGE('',*,*,#18160,.F.);
#25728=ORIENTED_EDGE('',*,*,#18165,.F.);
#25729=ORIENTED_EDGE('',*,*,#18166,.T.);
#25730=ORIENTED_EDGE('',*,*,#18167,.T.);
#25731=ORIENTED_EDGE('',*,*,#18163,.F.);
#25732=ORIENTED_EDGE('',*,*,#18168,.F.);
#25733=ORIENTED_EDGE('',*,*,#18169,.T.);
#25734=ORIENTED_EDGE('',*,*,#18170,.T.);
#25735=ORIENTED_EDGE('',*,*,#18166,.F.);
#25736=ORIENTED_EDGE('',*,*,#18171,.F.);
#25737=ORIENTED_EDGE('',*,*,#18158,.T.);
#25738=ORIENTED_EDGE('',*,*,#18172,.T.);
#25739=ORIENTED_EDGE('',*,*,#18169,.F.);
#25740=ORIENTED_EDGE('',*,*,#18172,.F.);
#25741=ORIENTED_EDGE('',*,*,#18157,.F.);
#25742=ORIENTED_EDGE('',*,*,#18161,.F.);
#25743=ORIENTED_EDGE('',*,*,#18164,.F.);
#25744=ORIENTED_EDGE('',*,*,#18167,.F.);
#25745=ORIENTED_EDGE('',*,*,#18170,.F.);
#25746=ORIENTED_EDGE('',*,*,#18154,.T.);
#25747=ORIENTED_EDGE('',*,*,#18173,.F.);
#25748=ORIENTED_EDGE('',*,*,#17817,.F.);
#25749=ORIENTED_EDGE('',*,*,#17396,.F.);
#25750=ORIENTED_EDGE('',*,*,#17818,.F.);
#25751=ORIENTED_EDGE('',*,*,#18174,.T.);
#25752=ORIENTED_EDGE('',*,*,#18173,.T.);
#25753=ORIENTED_EDGE('',*,*,#18174,.F.);
#25754=ORIENTED_EDGE('',*,*,#18175,.F.);
#25755=ORIENTED_EDGE('',*,*,#18176,.T.);
#25756=ORIENTED_EDGE('',*,*,#17990,.T.);
#25757=ORIENTED_EDGE('',*,*,#17980,.T.);
#25758=ORIENTED_EDGE('',*,*,#17984,.T.);
#25759=ORIENTED_EDGE('',*,*,#18177,.T.);
#25760=ORIENTED_EDGE('',*,*,#17826,.T.);
#25761=ORIENTED_EDGE('',*,*,#18177,.F.);
#25762=ORIENTED_EDGE('',*,*,#17986,.T.);
#25763=ORIENTED_EDGE('',*,*,#17987,.T.);
#25764=ORIENTED_EDGE('',*,*,#17989,.T.);
#25765=ORIENTED_EDGE('',*,*,#18176,.F.);
#25766=ORIENTED_EDGE('',*,*,#17833,.T.);
#25767=ORIENTED_EDGE('',*,*,#17835,.T.);
#25768=ORIENTED_EDGE('',*,*,#17827,.T.);
#25769=ORIENTED_EDGE('',*,*,#17831,.T.);
#25770=ORIENTED_EDGE('',*,*,#17842,.T.);
#25771=ORIENTED_EDGE('',*,*,#17844,.T.);
#25772=ORIENTED_EDGE('',*,*,#17836,.T.);
#25773=ORIENTED_EDGE('',*,*,#17840,.T.);
#25774=ORIENTED_EDGE('',*,*,#17851,.T.);
#25775=ORIENTED_EDGE('',*,*,#17853,.T.);
#25776=ORIENTED_EDGE('',*,*,#17845,.T.);
#25777=ORIENTED_EDGE('',*,*,#17849,.T.);
#25778=ORIENTED_EDGE('',*,*,#17860,.T.);
#25779=ORIENTED_EDGE('',*,*,#17862,.T.);
#25780=ORIENTED_EDGE('',*,*,#17854,.T.);
#25781=ORIENTED_EDGE('',*,*,#17858,.T.);
#25782=ORIENTED_EDGE('',*,*,#17869,.T.);
#25783=ORIENTED_EDGE('',*,*,#17871,.T.);
#25784=ORIENTED_EDGE('',*,*,#17863,.T.);
#25785=ORIENTED_EDGE('',*,*,#17867,.T.);
#25786=ORIENTED_EDGE('',*,*,#17878,.T.);
#25787=ORIENTED_EDGE('',*,*,#17880,.T.);
#25788=ORIENTED_EDGE('',*,*,#17872,.T.);
#25789=ORIENTED_EDGE('',*,*,#17876,.T.);
#25790=ORIENTED_EDGE('',*,*,#17887,.T.);
#25791=ORIENTED_EDGE('',*,*,#17889,.T.);
#25792=ORIENTED_EDGE('',*,*,#17881,.T.);
#25793=ORIENTED_EDGE('',*,*,#17885,.T.);
#25794=ORIENTED_EDGE('',*,*,#17896,.T.);
#25795=ORIENTED_EDGE('',*,*,#17898,.T.);
#25796=ORIENTED_EDGE('',*,*,#17890,.T.);
#25797=ORIENTED_EDGE('',*,*,#17894,.T.);
#25798=ORIENTED_EDGE('',*,*,#17905,.T.);
#25799=ORIENTED_EDGE('',*,*,#17907,.T.);
#25800=ORIENTED_EDGE('',*,*,#17899,.T.);
#25801=ORIENTED_EDGE('',*,*,#17903,.T.);
#25802=ORIENTED_EDGE('',*,*,#17914,.T.);
#25803=ORIENTED_EDGE('',*,*,#17916,.T.);
#25804=ORIENTED_EDGE('',*,*,#17908,.T.);
#25805=ORIENTED_EDGE('',*,*,#17912,.T.);
#25806=ORIENTED_EDGE('',*,*,#17923,.T.);
#25807=ORIENTED_EDGE('',*,*,#17925,.T.);
#25808=ORIENTED_EDGE('',*,*,#17917,.T.);
#25809=ORIENTED_EDGE('',*,*,#17921,.T.);
#25810=ORIENTED_EDGE('',*,*,#17932,.T.);
#25811=ORIENTED_EDGE('',*,*,#17934,.T.);
#25812=ORIENTED_EDGE('',*,*,#17926,.T.);
#25813=ORIENTED_EDGE('',*,*,#17930,.T.);
#25814=ORIENTED_EDGE('',*,*,#17941,.T.);
#25815=ORIENTED_EDGE('',*,*,#17943,.T.);
#25816=ORIENTED_EDGE('',*,*,#17935,.T.);
#25817=ORIENTED_EDGE('',*,*,#17939,.T.);
#25818=ORIENTED_EDGE('',*,*,#17950,.T.);
#25819=ORIENTED_EDGE('',*,*,#17952,.T.);
#25820=ORIENTED_EDGE('',*,*,#17944,.T.);
#25821=ORIENTED_EDGE('',*,*,#17948,.T.);
#25822=ORIENTED_EDGE('',*,*,#17959,.T.);
#25823=ORIENTED_EDGE('',*,*,#17961,.T.);
#25824=ORIENTED_EDGE('',*,*,#17953,.T.);
#25825=ORIENTED_EDGE('',*,*,#17957,.T.);
#25826=ORIENTED_EDGE('',*,*,#17968,.T.);
#25827=ORIENTED_EDGE('',*,*,#17970,.T.);
#25828=ORIENTED_EDGE('',*,*,#17962,.T.);
#25829=ORIENTED_EDGE('',*,*,#17966,.T.);
#25830=ORIENTED_EDGE('',*,*,#17977,.T.);
#25831=ORIENTED_EDGE('',*,*,#17979,.T.);
#25832=ORIENTED_EDGE('',*,*,#17971,.T.);
#25833=ORIENTED_EDGE('',*,*,#17975,.T.);
#25834=ORIENTED_EDGE('',*,*,#17997,.T.);
#25835=ORIENTED_EDGE('',*,*,#17999,.T.);
#25836=ORIENTED_EDGE('',*,*,#17991,.T.);
#25837=ORIENTED_EDGE('',*,*,#17995,.T.);
#25838=ORIENTED_EDGE('',*,*,#18006,.T.);
#25839=ORIENTED_EDGE('',*,*,#18008,.T.);
#25840=ORIENTED_EDGE('',*,*,#18000,.T.);
#25841=ORIENTED_EDGE('',*,*,#18004,.T.);
#25842=ORIENTED_EDGE('',*,*,#18015,.T.);
#25843=ORIENTED_EDGE('',*,*,#18017,.T.);
#25844=ORIENTED_EDGE('',*,*,#18009,.T.);
#25845=ORIENTED_EDGE('',*,*,#18013,.T.);
#25846=ORIENTED_EDGE('',*,*,#18024,.T.);
#25847=ORIENTED_EDGE('',*,*,#18026,.T.);
#25848=ORIENTED_EDGE('',*,*,#18018,.T.);
#25849=ORIENTED_EDGE('',*,*,#18022,.T.);
#25850=ORIENTED_EDGE('',*,*,#18033,.T.);
#25851=ORIENTED_EDGE('',*,*,#18035,.T.);
#25852=ORIENTED_EDGE('',*,*,#18027,.T.);
#25853=ORIENTED_EDGE('',*,*,#18031,.T.);
#25854=ORIENTED_EDGE('',*,*,#18042,.T.);
#25855=ORIENTED_EDGE('',*,*,#18044,.T.);
#25856=ORIENTED_EDGE('',*,*,#18036,.T.);
#25857=ORIENTED_EDGE('',*,*,#18040,.T.);
#25858=ORIENTED_EDGE('',*,*,#18051,.T.);
#25859=ORIENTED_EDGE('',*,*,#18053,.T.);
#25860=ORIENTED_EDGE('',*,*,#18045,.T.);
#25861=ORIENTED_EDGE('',*,*,#18049,.T.);
#25862=ORIENTED_EDGE('',*,*,#18060,.T.);
#25863=ORIENTED_EDGE('',*,*,#18062,.T.);
#25864=ORIENTED_EDGE('',*,*,#18054,.T.);
#25865=ORIENTED_EDGE('',*,*,#18058,.T.);
#25866=ORIENTED_EDGE('',*,*,#18069,.T.);
#25867=ORIENTED_EDGE('',*,*,#18071,.T.);
#25868=ORIENTED_EDGE('',*,*,#18063,.T.);
#25869=ORIENTED_EDGE('',*,*,#18067,.T.);
#25870=ORIENTED_EDGE('',*,*,#18078,.T.);
#25871=ORIENTED_EDGE('',*,*,#18080,.T.);
#25872=ORIENTED_EDGE('',*,*,#18072,.T.);
#25873=ORIENTED_EDGE('',*,*,#18076,.T.);
#25874=ORIENTED_EDGE('',*,*,#18087,.T.);
#25875=ORIENTED_EDGE('',*,*,#18089,.T.);
#25876=ORIENTED_EDGE('',*,*,#18081,.T.);
#25877=ORIENTED_EDGE('',*,*,#18085,.T.);
#25878=ORIENTED_EDGE('',*,*,#18096,.T.);
#25879=ORIENTED_EDGE('',*,*,#18098,.T.);
#25880=ORIENTED_EDGE('',*,*,#18090,.T.);
#25881=ORIENTED_EDGE('',*,*,#18094,.T.);
#25882=ORIENTED_EDGE('',*,*,#18105,.T.);
#25883=ORIENTED_EDGE('',*,*,#18107,.T.);
#25884=ORIENTED_EDGE('',*,*,#18099,.T.);
#25885=ORIENTED_EDGE('',*,*,#18103,.T.);
#25886=ORIENTED_EDGE('',*,*,#18114,.T.);
#25887=ORIENTED_EDGE('',*,*,#18116,.T.);
#25888=ORIENTED_EDGE('',*,*,#18108,.T.);
#25889=ORIENTED_EDGE('',*,*,#18112,.T.);
#25890=ORIENTED_EDGE('',*,*,#18123,.T.);
#25891=ORIENTED_EDGE('',*,*,#18125,.T.);
#25892=ORIENTED_EDGE('',*,*,#18117,.T.);
#25893=ORIENTED_EDGE('',*,*,#18121,.T.);
#25894=ORIENTED_EDGE('',*,*,#18132,.T.);
#25895=ORIENTED_EDGE('',*,*,#18134,.T.);
#25896=ORIENTED_EDGE('',*,*,#18126,.T.);
#25897=ORIENTED_EDGE('',*,*,#18130,.T.);
#25898=ORIENTED_EDGE('',*,*,#18141,.T.);
#25899=ORIENTED_EDGE('',*,*,#18143,.T.);
#25900=ORIENTED_EDGE('',*,*,#18135,.T.);
#25901=ORIENTED_EDGE('',*,*,#18139,.T.);
#25902=ORIENTED_EDGE('',*,*,#18150,.T.);
#25903=ORIENTED_EDGE('',*,*,#18152,.T.);
#25904=ORIENTED_EDGE('',*,*,#18144,.T.);
#25905=ORIENTED_EDGE('',*,*,#18148,.T.);
#25906=ORIENTED_EDGE('',*,*,#18178,.F.);
#25907=ORIENTED_EDGE('',*,*,#18179,.T.);
#25908=ORIENTED_EDGE('',*,*,#18175,.T.);
#25909=ORIENTED_EDGE('',*,*,#18179,.F.);
#25910=ORIENTED_EDGE('',*,*,#18178,.T.);
#25911=ORIENTED_EDGE('',*,*,#18155,.T.);
#25912=ORIENTED_EDGE('',*,*,#18171,.T.);
#25913=ORIENTED_EDGE('',*,*,#18168,.T.);
#25914=ORIENTED_EDGE('',*,*,#18165,.T.);
#25915=ORIENTED_EDGE('',*,*,#18162,.T.);
#25916=ORIENTED_EDGE('',*,*,#18159,.T.);
#25917=ORIENTED_EDGE('',*,*,#18180,.T.);
#25918=ORIENTED_EDGE('',*,*,#18181,.T.);
#25919=ORIENTED_EDGE('',*,*,#18182,.T.);
#25920=ORIENTED_EDGE('',*,*,#18183,.T.);
#25921=ORIENTED_EDGE('',*,*,#18181,.F.);
#25922=ORIENTED_EDGE('',*,*,#18184,.F.);
#25923=ORIENTED_EDGE('',*,*,#18185,.F.);
#25924=ORIENTED_EDGE('',*,*,#18186,.T.);
#25925=ORIENTED_EDGE('',*,*,#18187,.T.);
#25926=ORIENTED_EDGE('',*,*,#18188,.T.);
#25927=ORIENTED_EDGE('',*,*,#18189,.T.);
#25928=ORIENTED_EDGE('',*,*,#18190,.T.);
#25929=ORIENTED_EDGE('',*,*,#18188,.F.);
#25930=ORIENTED_EDGE('',*,*,#18191,.F.);
#25931=ORIENTED_EDGE('',*,*,#18192,.F.);
#25932=ORIENTED_EDGE('',*,*,#18193,.T.);
#25933=ORIENTED_EDGE('',*,*,#18187,.F.);
#25934=ORIENTED_EDGE('',*,*,#18194,.T.);
#25935=ORIENTED_EDGE('',*,*,#18195,.F.);
#25936=ORIENTED_EDGE('',*,*,#18196,.T.);
#25937=ORIENTED_EDGE('',*,*,#18197,.F.);
#25938=ORIENTED_EDGE('',*,*,#18191,.T.);
#25939=ORIENTED_EDGE('',*,*,#18198,.T.);
#25940=ORIENTED_EDGE('',*,*,#18199,.T.);
#25941=ORIENTED_EDGE('',*,*,#18200,.T.);
#25942=ORIENTED_EDGE('',*,*,#18201,.T.);
#25943=ORIENTED_EDGE('',*,*,#18201,.F.);
#25944=ORIENTED_EDGE('',*,*,#18202,.F.);
#25945=ORIENTED_EDGE('',*,*,#18203,.F.);
#25946=ORIENTED_EDGE('',*,*,#18182,.F.);
#25947=ORIENTED_EDGE('',*,*,#18186,.F.);
#25948=ORIENTED_EDGE('',*,*,#18204,.F.);
#25949=ORIENTED_EDGE('',*,*,#18205,.F.);
#25950=ORIENTED_EDGE('',*,*,#18206,.F.);
#25951=ORIENTED_EDGE('',*,*,#18200,.F.);
#25952=ORIENTED_EDGE('',*,*,#18207,.T.);
#25953=ORIENTED_EDGE('',*,*,#18208,.F.);
#25954=ORIENTED_EDGE('',*,*,#18209,.T.);
#25955=ORIENTED_EDGE('',*,*,#18210,.F.);
#25956=ORIENTED_EDGE('',*,*,#18202,.T.);
#25957=ORIENTED_EDGE('',*,*,#18211,.T.);
#25958=ORIENTED_EDGE('',*,*,#18212,.T.);
#25959=ORIENTED_EDGE('',*,*,#18213,.T.);
#25960=ORIENTED_EDGE('',*,*,#18214,.T.);
#25961=ORIENTED_EDGE('',*,*,#18212,.F.);
#25962=ORIENTED_EDGE('',*,*,#18215,.F.);
#25963=ORIENTED_EDGE('',*,*,#18216,.F.);
#25964=ORIENTED_EDGE('',*,*,#18217,.T.);
#25965=ORIENTED_EDGE('',*,*,#18208,.T.);
#25966=ORIENTED_EDGE('',*,*,#18218,.T.);
#25967=ORIENTED_EDGE('',*,*,#18219,.T.);
#25968=ORIENTED_EDGE('',*,*,#18220,.T.);
#25969=ORIENTED_EDGE('',*,*,#18220,.F.);
#25970=ORIENTED_EDGE('',*,*,#18221,.F.);
#25971=ORIENTED_EDGE('',*,*,#18222,.F.);
#25972=ORIENTED_EDGE('',*,*,#18223,.F.);
#25973=ORIENTED_EDGE('',*,*,#18215,.T.);
#25974=ORIENTED_EDGE('',*,*,#18211,.F.);
#25975=ORIENTED_EDGE('',*,*,#18224,.F.);
#25976=ORIENTED_EDGE('',*,*,#18209,.F.);
#25977=ORIENTED_EDGE('',*,*,#18225,.T.);
#25978=ORIENTED_EDGE('',*,*,#18226,.T.);
#25979=ORIENTED_EDGE('',*,*,#18227,.T.);
#25980=ORIENTED_EDGE('',*,*,#18228,.T.);
#25981=ORIENTED_EDGE('',*,*,#18226,.F.);
#25982=ORIENTED_EDGE('',*,*,#18229,.T.);
#25983=ORIENTED_EDGE('',*,*,#18230,.F.);
#25984=ORIENTED_EDGE('',*,*,#18231,.F.);
#25985=ORIENTED_EDGE('',*,*,#18225,.F.);
#25986=ORIENTED_EDGE('',*,*,#18232,.T.);
#25987=ORIENTED_EDGE('',*,*,#18233,.T.);
#25988=ORIENTED_EDGE('',*,*,#18234,.T.);
#25989=ORIENTED_EDGE('',*,*,#18235,.F.);
#25990=ORIENTED_EDGE('',*,*,#18229,.F.);
#25991=ORIENTED_EDGE('',*,*,#18236,.T.);
#25992=ORIENTED_EDGE('',*,*,#18237,.T.);
#25993=ORIENTED_EDGE('',*,*,#18238,.T.);
#25994=ORIENTED_EDGE('',*,*,#18239,.T.);
#25995=ORIENTED_EDGE('',*,*,#18237,.F.);
#25996=ORIENTED_EDGE('',*,*,#18240,.F.);
#25997=ORIENTED_EDGE('',*,*,#18241,.F.);
#25998=ORIENTED_EDGE('',*,*,#18242,.T.);
#25999=ORIENTED_EDGE('',*,*,#18243,.T.);
#26000=ORIENTED_EDGE('',*,*,#18230,.T.);
#26001=ORIENTED_EDGE('',*,*,#18235,.T.);
#26002=ORIENTED_EDGE('',*,*,#18244,.T.);
#26003=ORIENTED_EDGE('',*,*,#18227,.F.);
#26004=ORIENTED_EDGE('',*,*,#18231,.T.);
#26005=ORIENTED_EDGE('',*,*,#18243,.F.);
#26006=ORIENTED_EDGE('',*,*,#18245,.T.);
#26007=ORIENTED_EDGE('',*,*,#18246,.F.);
#26008=ORIENTED_EDGE('',*,*,#18247,.T.);
#26009=ORIENTED_EDGE('',*,*,#18244,.F.);
#26010=ORIENTED_EDGE('',*,*,#18234,.F.);
#26011=ORIENTED_EDGE('',*,*,#18248,.F.);
#26012=ORIENTED_EDGE('',*,*,#18249,.F.);
#26013=ORIENTED_EDGE('',*,*,#18240,.T.);
#26014=ORIENTED_EDGE('',*,*,#18236,.F.);
#26015=ORIENTED_EDGE('',*,*,#18250,.F.);
#26016=ORIENTED_EDGE('',*,*,#18245,.F.);
#26017=ORIENTED_EDGE('',*,*,#18251,.T.);
#26018=ORIENTED_EDGE('',*,*,#18252,.T.);
#26019=ORIENTED_EDGE('',*,*,#18253,.T.);
#26020=ORIENTED_EDGE('',*,*,#18254,.T.);
#26021=ORIENTED_EDGE('',*,*,#18252,.F.);
#26022=ORIENTED_EDGE('',*,*,#18255,.T.);
#26023=ORIENTED_EDGE('',*,*,#18256,.F.);
#26024=ORIENTED_EDGE('',*,*,#18257,.F.);
#26025=ORIENTED_EDGE('',*,*,#18251,.F.);
#26026=ORIENTED_EDGE('',*,*,#18258,.T.);
#26027=ORIENTED_EDGE('',*,*,#18259,.T.);
#26028=ORIENTED_EDGE('',*,*,#18260,.T.);
#26029=ORIENTED_EDGE('',*,*,#18261,.F.);
#26030=ORIENTED_EDGE('',*,*,#18255,.F.);
#26031=ORIENTED_EDGE('',*,*,#18204,.T.);
#26032=ORIENTED_EDGE('',*,*,#18185,.T.);
#26033=ORIENTED_EDGE('',*,*,#18262,.T.);
#26034=ORIENTED_EDGE('',*,*,#18263,.T.);
#26035=ORIENTED_EDGE('',*,*,#18264,.T.);
#26036=ORIENTED_EDGE('',*,*,#18216,.T.);
#26037=ORIENTED_EDGE('',*,*,#18223,.T.);
#26038=ORIENTED_EDGE('',*,*,#18265,.T.);
#26039=ORIENTED_EDGE('',*,*,#18266,.T.);
#26040=ORIENTED_EDGE('',*,*,#18241,.T.);
#26041=ORIENTED_EDGE('',*,*,#18249,.T.);
#26042=ORIENTED_EDGE('',*,*,#18267,.T.);
#26043=ORIENTED_EDGE('',*,*,#18268,.T.);
#26044=ORIENTED_EDGE('',*,*,#18269,.T.);
#26045=ORIENTED_EDGE('',*,*,#18270,.T.);
#26046=ORIENTED_EDGE('',*,*,#18271,.T.);
#26047=ORIENTED_EDGE('',*,*,#18269,.F.);
#26048=ORIENTED_EDGE('',*,*,#18272,.F.);
#26049=ORIENTED_EDGE('',*,*,#18273,.F.);
#26050=ORIENTED_EDGE('',*,*,#18274,.T.);
#26051=ORIENTED_EDGE('',*,*,#18275,.T.);
#26052=ORIENTED_EDGE('',*,*,#18273,.T.);
#26053=ORIENTED_EDGE('',*,*,#18276,.T.);
#26054=ORIENTED_EDGE('',*,*,#18277,.T.);
#26055=ORIENTED_EDGE('',*,*,#18278,.T.);
#26056=ORIENTED_EDGE('',*,*,#18192,.T.);
#26057=ORIENTED_EDGE('',*,*,#18197,.T.);
#26058=ORIENTED_EDGE('',*,*,#18279,.T.);
#26059=ORIENTED_EDGE('',*,*,#18189,.F.);
#26060=ORIENTED_EDGE('',*,*,#18193,.F.);
#26061=ORIENTED_EDGE('',*,*,#18278,.F.);
#26062=ORIENTED_EDGE('',*,*,#18280,.T.);
#26063=ORIENTED_EDGE('',*,*,#18281,.T.);
#26064=ORIENTED_EDGE('',*,*,#18282,.T.);
#26065=ORIENTED_EDGE('',*,*,#18279,.F.);
#26066=ORIENTED_EDGE('',*,*,#18196,.F.);
#26067=ORIENTED_EDGE('',*,*,#18283,.F.);
#26068=ORIENTED_EDGE('',*,*,#18270,.F.);
#26069=ORIENTED_EDGE('',*,*,#18274,.F.);
#26070=ORIENTED_EDGE('',*,*,#18275,.F.);
#26071=ORIENTED_EDGE('',*,*,#18284,.F.);
#26072=ORIENTED_EDGE('',*,*,#18280,.F.);
#26073=ORIENTED_EDGE('',*,*,#18285,.T.);
#26074=ORIENTED_EDGE('',*,*,#18256,.T.);
#26075=ORIENTED_EDGE('',*,*,#18261,.T.);
#26076=ORIENTED_EDGE('',*,*,#18286,.T.);
#26077=ORIENTED_EDGE('',*,*,#18253,.F.);
#26078=ORIENTED_EDGE('',*,*,#18257,.T.);
#26079=ORIENTED_EDGE('',*,*,#18285,.F.);
#26080=ORIENTED_EDGE('',*,*,#18287,.T.);
#26081=ORIENTED_EDGE('',*,*,#18288,.F.);
#26082=ORIENTED_EDGE('',*,*,#18289,.T.);
#26083=ORIENTED_EDGE('',*,*,#18286,.F.);
#26084=ORIENTED_EDGE('',*,*,#18260,.F.);
#26085=ORIENTED_EDGE('',*,*,#18290,.F.);
#26086=ORIENTED_EDGE('',*,*,#18276,.F.);
#26087=ORIENTED_EDGE('',*,*,#18272,.T.);
#26088=ORIENTED_EDGE('',*,*,#18268,.F.);
#26089=ORIENTED_EDGE('',*,*,#18291,.F.);
#26090=ORIENTED_EDGE('',*,*,#18287,.F.);
#26091=ORIENTED_EDGE('',*,*,#18292,.T.);
#26092=ORIENTED_EDGE('',*,*,#18281,.F.);
#26093=ORIENTED_EDGE('',*,*,#18284,.T.);
#26094=ORIENTED_EDGE('',*,*,#18277,.F.);
#26095=ORIENTED_EDGE('',*,*,#18290,.T.);
#26096=ORIENTED_EDGE('',*,*,#18259,.F.);
#26097=ORIENTED_EDGE('',*,*,#18293,.T.);
#26098=ORIENTED_EDGE('',*,*,#18267,.F.);
#26099=ORIENTED_EDGE('',*,*,#18248,.T.);
#26100=ORIENTED_EDGE('',*,*,#18233,.F.);
#26101=ORIENTED_EDGE('',*,*,#18294,.T.);
#26102=ORIENTED_EDGE('',*,*,#18265,.F.);
#26103=ORIENTED_EDGE('',*,*,#18222,.T.);
#26104=ORIENTED_EDGE('',*,*,#18295,.F.);
#26105=ORIENTED_EDGE('',*,*,#18205,.T.);
#26106=ORIENTED_EDGE('',*,*,#18263,.F.);
#26107=ORIENTED_EDGE('',*,*,#18296,.T.);
#26108=ORIENTED_EDGE('',*,*,#18254,.F.);
#26109=ORIENTED_EDGE('',*,*,#18289,.F.);
#26110=ORIENTED_EDGE('',*,*,#18297,.F.);
#26111=ORIENTED_EDGE('',*,*,#18238,.F.);
#26112=ORIENTED_EDGE('',*,*,#18242,.F.);
#26113=ORIENTED_EDGE('',*,*,#18266,.F.);
#26114=ORIENTED_EDGE('',*,*,#18293,.F.);
#26115=ORIENTED_EDGE('',*,*,#18258,.F.);
#26116=ORIENTED_EDGE('',*,*,#18228,.F.);
#26117=ORIENTED_EDGE('',*,*,#18247,.F.);
#26118=ORIENTED_EDGE('',*,*,#18298,.F.);
#26119=ORIENTED_EDGE('',*,*,#18213,.F.);
#26120=ORIENTED_EDGE('',*,*,#18217,.F.);
#26121=ORIENTED_EDGE('',*,*,#18264,.F.);
#26122=ORIENTED_EDGE('',*,*,#18294,.F.);
#26123=ORIENTED_EDGE('',*,*,#18232,.F.);
#26124=ORIENTED_EDGE('',*,*,#18199,.F.);
#26125=ORIENTED_EDGE('',*,*,#18299,.T.);
#26126=ORIENTED_EDGE('',*,*,#18218,.F.);
#26127=ORIENTED_EDGE('',*,*,#18207,.F.);
#26128=ORIENTED_EDGE('',*,*,#18198,.F.);
#26129=ORIENTED_EDGE('',*,*,#18206,.T.);
#26130=ORIENTED_EDGE('',*,*,#18295,.T.);
#26131=ORIENTED_EDGE('',*,*,#18221,.T.);
#26132=ORIENTED_EDGE('',*,*,#18219,.F.);
#26133=ORIENTED_EDGE('',*,*,#18299,.F.);
#26134=ORIENTED_EDGE('',*,*,#18190,.F.);
#26135=ORIENTED_EDGE('',*,*,#18282,.F.);
#26136=ORIENTED_EDGE('',*,*,#18292,.F.);
#26137=ORIENTED_EDGE('',*,*,#18262,.F.);
#26138=ORIENTED_EDGE('',*,*,#18184,.T.);
#26139=ORIENTED_EDGE('',*,*,#18180,.F.);
#26140=ORIENTED_EDGE('',*,*,#18300,.F.);
#26141=ORIENTED_EDGE('',*,*,#18194,.F.);
#26142=ORIENTED_EDGE('',*,*,#18301,.T.);
#26143=ORIENTED_EDGE('',*,*,#18302,.T.);
#26144=ORIENTED_EDGE('',*,*,#18296,.F.);
#26145=ORIENTED_EDGE('',*,*,#18302,.F.);
#26146=ORIENTED_EDGE('',*,*,#18203,.T.);
#26147=ORIENTED_EDGE('',*,*,#18210,.T.);
#26148=ORIENTED_EDGE('',*,*,#18224,.T.);
#26149=ORIENTED_EDGE('',*,*,#18214,.F.);
#26150=ORIENTED_EDGE('',*,*,#18298,.T.);
#26151=ORIENTED_EDGE('',*,*,#18246,.T.);
#26152=ORIENTED_EDGE('',*,*,#18250,.T.);
#26153=ORIENTED_EDGE('',*,*,#18239,.F.);
#26154=ORIENTED_EDGE('',*,*,#18297,.T.);
#26155=ORIENTED_EDGE('',*,*,#18288,.T.);
#26156=ORIENTED_EDGE('',*,*,#18291,.T.);
#26157=ORIENTED_EDGE('',*,*,#18271,.F.);
#26158=ORIENTED_EDGE('',*,*,#18283,.T.);
#26159=ORIENTED_EDGE('',*,*,#18195,.T.);
#26160=ORIENTED_EDGE('',*,*,#18300,.T.);
#26161=ORIENTED_EDGE('',*,*,#18183,.F.);
#26162=ORIENTED_EDGE('',*,*,#18301,.F.);
#26163=ORIENTED_EDGE('',*,*,#18303,.F.);
#26164=ORIENTED_EDGE('',*,*,#18304,.T.);
#26165=ORIENTED_EDGE('',*,*,#18305,.T.);
#26166=ORIENTED_EDGE('',*,*,#18306,.T.);
#26167=ORIENTED_EDGE('',*,*,#18307,.F.);
#26168=ORIENTED_EDGE('',*,*,#18308,.T.);
#26169=ORIENTED_EDGE('',*,*,#18303,.T.);
#26170=ORIENTED_EDGE('',*,*,#18309,.T.);
#26171=ORIENTED_EDGE('',*,*,#18310,.F.);
#26172=ORIENTED_EDGE('',*,*,#18311,.T.);
#26173=ORIENTED_EDGE('',*,*,#18307,.T.);
#26174=ORIENTED_EDGE('',*,*,#18312,.T.);
#26175=ORIENTED_EDGE('',*,*,#18313,.F.);
#26176=ORIENTED_EDGE('',*,*,#18314,.T.);
#26177=ORIENTED_EDGE('',*,*,#18310,.T.);
#26178=ORIENTED_EDGE('',*,*,#18315,.T.);
#26179=ORIENTED_EDGE('',*,*,#18316,.F.);
#26180=ORIENTED_EDGE('',*,*,#18317,.T.);
#26181=ORIENTED_EDGE('',*,*,#18313,.T.);
#26182=ORIENTED_EDGE('',*,*,#18318,.T.);
#26183=ORIENTED_EDGE('',*,*,#18319,.F.);
#26184=ORIENTED_EDGE('',*,*,#18320,.T.);
#26185=ORIENTED_EDGE('',*,*,#18316,.T.);
#26186=ORIENTED_EDGE('',*,*,#18321,.T.);
#26187=ORIENTED_EDGE('',*,*,#18322,.F.);
#26188=ORIENTED_EDGE('',*,*,#18323,.T.);
#26189=ORIENTED_EDGE('',*,*,#18319,.T.);
#26190=ORIENTED_EDGE('',*,*,#18324,.T.);
#26191=ORIENTED_EDGE('',*,*,#18325,.F.);
#26192=ORIENTED_EDGE('',*,*,#18326,.T.);
#26193=ORIENTED_EDGE('',*,*,#18322,.T.);
#26194=ORIENTED_EDGE('',*,*,#18327,.T.);
#26195=ORIENTED_EDGE('',*,*,#18328,.F.);
#26196=ORIENTED_EDGE('',*,*,#18329,.T.);
#26197=ORIENTED_EDGE('',*,*,#18325,.T.);
#26198=ORIENTED_EDGE('',*,*,#18330,.T.);
#26199=ORIENTED_EDGE('',*,*,#18331,.F.);
#26200=ORIENTED_EDGE('',*,*,#18332,.T.);
#26201=ORIENTED_EDGE('',*,*,#18328,.T.);
#26202=ORIENTED_EDGE('',*,*,#18333,.T.);
#26203=ORIENTED_EDGE('',*,*,#18334,.F.);
#26204=ORIENTED_EDGE('',*,*,#18335,.T.);
#26205=ORIENTED_EDGE('',*,*,#18331,.T.);
#26206=ORIENTED_EDGE('',*,*,#18336,.T.);
#26207=ORIENTED_EDGE('',*,*,#18337,.F.);
#26208=ORIENTED_EDGE('',*,*,#18338,.T.);
#26209=ORIENTED_EDGE('',*,*,#18334,.T.);
#26210=ORIENTED_EDGE('',*,*,#18339,.T.);
#26211=ORIENTED_EDGE('',*,*,#18340,.F.);
#26212=ORIENTED_EDGE('',*,*,#18341,.T.);
#26213=ORIENTED_EDGE('',*,*,#18337,.T.);
#26214=ORIENTED_EDGE('',*,*,#18342,.T.);
#26215=ORIENTED_EDGE('',*,*,#18343,.F.);
#26216=ORIENTED_EDGE('',*,*,#18344,.T.);
#26217=ORIENTED_EDGE('',*,*,#18340,.T.);
#26218=ORIENTED_EDGE('',*,*,#18345,.T.);
#26219=ORIENTED_EDGE('',*,*,#18346,.F.);
#26220=ORIENTED_EDGE('',*,*,#18347,.T.);
#26221=ORIENTED_EDGE('',*,*,#18343,.T.);
#26222=ORIENTED_EDGE('',*,*,#18348,.T.);
#26223=ORIENTED_EDGE('',*,*,#18349,.F.);
#26224=ORIENTED_EDGE('',*,*,#18350,.T.);
#26225=ORIENTED_EDGE('',*,*,#18346,.T.);
#26226=ORIENTED_EDGE('',*,*,#18351,.T.);
#26227=ORIENTED_EDGE('',*,*,#18352,.F.);
#26228=ORIENTED_EDGE('',*,*,#18353,.T.);
#26229=ORIENTED_EDGE('',*,*,#18354,.F.);
#26230=ORIENTED_EDGE('',*,*,#18355,.F.);
#26231=ORIENTED_EDGE('',*,*,#18356,.T.);
#26232=ORIENTED_EDGE('',*,*,#18352,.T.);
#26233=ORIENTED_EDGE('',*,*,#18357,.F.);
#26234=ORIENTED_EDGE('',*,*,#18358,.F.);
#26235=ORIENTED_EDGE('',*,*,#18359,.F.);
#26236=ORIENTED_EDGE('',*,*,#18360,.T.);
#26237=ORIENTED_EDGE('',*,*,#18355,.T.);
#26238=ORIENTED_EDGE('',*,*,#18361,.F.);
#26239=ORIENTED_EDGE('',*,*,#18362,.F.);
#26240=ORIENTED_EDGE('',*,*,#18363,.T.);
#26241=ORIENTED_EDGE('',*,*,#18359,.T.);
#26242=ORIENTED_EDGE('',*,*,#18364,.F.);
#26243=ORIENTED_EDGE('',*,*,#18365,.F.);
#26244=ORIENTED_EDGE('',*,*,#18366,.T.);
#26245=ORIENTED_EDGE('',*,*,#18362,.T.);
#26246=ORIENTED_EDGE('',*,*,#18367,.F.);
#26247=ORIENTED_EDGE('',*,*,#18368,.F.);
#26248=ORIENTED_EDGE('',*,*,#18369,.T.);
#26249=ORIENTED_EDGE('',*,*,#18365,.T.);
#26250=ORIENTED_EDGE('',*,*,#18370,.F.);
#26251=ORIENTED_EDGE('',*,*,#18371,.F.);
#26252=ORIENTED_EDGE('',*,*,#18372,.T.);
#26253=ORIENTED_EDGE('',*,*,#18368,.T.);
#26254=ORIENTED_EDGE('',*,*,#18373,.F.);
#26255=ORIENTED_EDGE('',*,*,#18374,.F.);
#26256=ORIENTED_EDGE('',*,*,#18375,.T.);
#26257=ORIENTED_EDGE('',*,*,#18371,.T.);
#26258=ORIENTED_EDGE('',*,*,#18376,.F.);
#26259=ORIENTED_EDGE('',*,*,#18377,.F.);
#26260=ORIENTED_EDGE('',*,*,#18378,.T.);
#26261=ORIENTED_EDGE('',*,*,#18374,.T.);
#26262=ORIENTED_EDGE('',*,*,#18379,.F.);
#26263=ORIENTED_EDGE('',*,*,#18380,.F.);
#26264=ORIENTED_EDGE('',*,*,#18381,.T.);
#26265=ORIENTED_EDGE('',*,*,#18377,.T.);
#26266=ORIENTED_EDGE('',*,*,#18382,.F.);
#26267=ORIENTED_EDGE('',*,*,#18383,.F.);
#26268=ORIENTED_EDGE('',*,*,#18384,.T.);
#26269=ORIENTED_EDGE('',*,*,#18380,.T.);
#26270=ORIENTED_EDGE('',*,*,#18385,.F.);
#26271=ORIENTED_EDGE('',*,*,#18386,.F.);
#26272=ORIENTED_EDGE('',*,*,#18387,.T.);
#26273=ORIENTED_EDGE('',*,*,#18383,.T.);
#26274=ORIENTED_EDGE('',*,*,#18388,.F.);
#26275=ORIENTED_EDGE('',*,*,#18389,.F.);
#26276=ORIENTED_EDGE('',*,*,#18390,.T.);
#26277=ORIENTED_EDGE('',*,*,#18386,.T.);
#26278=ORIENTED_EDGE('',*,*,#18391,.F.);
#26279=ORIENTED_EDGE('',*,*,#18392,.F.);
#26280=ORIENTED_EDGE('',*,*,#18393,.T.);
#26281=ORIENTED_EDGE('',*,*,#18389,.T.);
#26282=ORIENTED_EDGE('',*,*,#18394,.F.);
#26283=ORIENTED_EDGE('',*,*,#18395,.F.);
#26284=ORIENTED_EDGE('',*,*,#18396,.T.);
#26285=ORIENTED_EDGE('',*,*,#18392,.T.);
#26286=ORIENTED_EDGE('',*,*,#18397,.F.);
#26287=ORIENTED_EDGE('',*,*,#18398,.F.);
#26288=ORIENTED_EDGE('',*,*,#18399,.T.);
#26289=ORIENTED_EDGE('',*,*,#18395,.T.);
#26290=ORIENTED_EDGE('',*,*,#18400,.F.);
#26291=ORIENTED_EDGE('',*,*,#18401,.T.);
#26292=ORIENTED_EDGE('',*,*,#18402,.T.);
#26293=ORIENTED_EDGE('',*,*,#18403,.T.);
#26294=ORIENTED_EDGE('',*,*,#18404,.T.);
#26295=ORIENTED_EDGE('',*,*,#18402,.F.);
#26296=ORIENTED_EDGE('',*,*,#18405,.F.);
#26297=ORIENTED_EDGE('',*,*,#18406,.F.);
#26298=ORIENTED_EDGE('',*,*,#18407,.T.);
#26299=ORIENTED_EDGE('',*,*,#18403,.F.);
#26300=ORIENTED_EDGE('',*,*,#18404,.F.);
#26301=ORIENTED_EDGE('',*,*,#18407,.F.);
#26302=ORIENTED_EDGE('',*,*,#18408,.T.);
#26303=ORIENTED_EDGE('',*,*,#18409,.T.);
#26304=ORIENTED_EDGE('',*,*,#18410,.T.);
#26305=ORIENTED_EDGE('',*,*,#18411,.T.);
#26306=ORIENTED_EDGE('',*,*,#18412,.T.);
#26307=ORIENTED_EDGE('',*,*,#18413,.F.);
#26308=ORIENTED_EDGE('',*,*,#18401,.F.);
#26309=ORIENTED_EDGE('',*,*,#18405,.T.);
#26310=ORIENTED_EDGE('',*,*,#18406,.T.);
#26311=ORIENTED_EDGE('',*,*,#18414,.T.);
#26312=ORIENTED_EDGE('',*,*,#18415,.T.);
#26313=ORIENTED_EDGE('',*,*,#18414,.F.);
#26314=ORIENTED_EDGE('',*,*,#18416,.T.);
#26315=ORIENTED_EDGE('',*,*,#18415,.F.);
#26316=ORIENTED_EDGE('',*,*,#18417,.T.);
#26317=ORIENTED_EDGE('',*,*,#18418,.T.);
#26318=ORIENTED_EDGE('',*,*,#18419,.T.);
#26319=ORIENTED_EDGE('',*,*,#18417,.F.);
#26320=ORIENTED_EDGE('',*,*,#18420,.T.);
#26321=ORIENTED_EDGE('',*,*,#18418,.F.);
#26322=ORIENTED_EDGE('',*,*,#18419,.F.);
#26323=ORIENTED_EDGE('',*,*,#18421,.T.);
#26324=ORIENTED_EDGE('',*,*,#18408,.F.);
#26325=ORIENTED_EDGE('',*,*,#18422,.T.);
#26326=ORIENTED_EDGE('',*,*,#18411,.F.);
#26327=ORIENTED_EDGE('',*,*,#18423,.T.);
#26328=ORIENTED_EDGE('',*,*,#18409,.F.);
#26329=ORIENTED_EDGE('',*,*,#18421,.F.);
#26330=ORIENTED_EDGE('',*,*,#18424,.F.);
#26331=ORIENTED_EDGE('',*,*,#18425,.T.);
#26332=ORIENTED_EDGE('',*,*,#18426,.T.);
#26333=ORIENTED_EDGE('',*,*,#18425,.F.);
#26334=ORIENTED_EDGE('',*,*,#18420,.F.);
#26335=ORIENTED_EDGE('',*,*,#18427,.F.);
#26336=ORIENTED_EDGE('',*,*,#18428,.F.);
#26337=ORIENTED_EDGE('',*,*,#18351,.F.);
#26338=ORIENTED_EDGE('',*,*,#18348,.F.);
#26339=ORIENTED_EDGE('',*,*,#18345,.F.);
#26340=ORIENTED_EDGE('',*,*,#18342,.F.);
#26341=ORIENTED_EDGE('',*,*,#18339,.F.);
#26342=ORIENTED_EDGE('',*,*,#18336,.F.);
#26343=ORIENTED_EDGE('',*,*,#18333,.F.);
#26344=ORIENTED_EDGE('',*,*,#18330,.F.);
#26345=ORIENTED_EDGE('',*,*,#18327,.F.);
#26346=ORIENTED_EDGE('',*,*,#18324,.F.);
#26347=ORIENTED_EDGE('',*,*,#18321,.F.);
#26348=ORIENTED_EDGE('',*,*,#18318,.F.);
#26349=ORIENTED_EDGE('',*,*,#18315,.F.);
#26350=ORIENTED_EDGE('',*,*,#18312,.F.);
#26351=ORIENTED_EDGE('',*,*,#18309,.F.);
#26352=ORIENTED_EDGE('',*,*,#18306,.F.);
#26353=ORIENTED_EDGE('',*,*,#18429,.F.);
#26354=ORIENTED_EDGE('',*,*,#18430,.T.);
#26355=ORIENTED_EDGE('',*,*,#18400,.T.);
#26356=ORIENTED_EDGE('',*,*,#18397,.T.);
#26357=ORIENTED_EDGE('',*,*,#18394,.T.);
#26358=ORIENTED_EDGE('',*,*,#18391,.T.);
#26359=ORIENTED_EDGE('',*,*,#18388,.T.);
#26360=ORIENTED_EDGE('',*,*,#18385,.T.);
#26361=ORIENTED_EDGE('',*,*,#18382,.T.);
#26362=ORIENTED_EDGE('',*,*,#18379,.T.);
#26363=ORIENTED_EDGE('',*,*,#18376,.T.);
#26364=ORIENTED_EDGE('',*,*,#18373,.T.);
#26365=ORIENTED_EDGE('',*,*,#18370,.T.);
#26366=ORIENTED_EDGE('',*,*,#18367,.T.);
#26367=ORIENTED_EDGE('',*,*,#18364,.T.);
#26368=ORIENTED_EDGE('',*,*,#18361,.T.);
#26369=ORIENTED_EDGE('',*,*,#18358,.T.);
#26370=ORIENTED_EDGE('',*,*,#18431,.T.);
#26371=ORIENTED_EDGE('',*,*,#18432,.T.);
#26372=ORIENTED_EDGE('',*,*,#18433,.T.);
#26373=ORIENTED_EDGE('',*,*,#18434,.T.);
#26374=ORIENTED_EDGE('',*,*,#18429,.T.);
#26375=ORIENTED_EDGE('',*,*,#18398,.T.);
#26376=ORIENTED_EDGE('',*,*,#18430,.F.);
#26377=ORIENTED_EDGE('',*,*,#18434,.F.);
#26378=ORIENTED_EDGE('',*,*,#18435,.T.);
#26379=ORIENTED_EDGE('',*,*,#18436,.F.);
#26380=ORIENTED_EDGE('',*,*,#18353,.F.);
#26381=ORIENTED_EDGE('',*,*,#18356,.F.);
#26382=ORIENTED_EDGE('',*,*,#18360,.F.);
#26383=ORIENTED_EDGE('',*,*,#18363,.F.);
#26384=ORIENTED_EDGE('',*,*,#18366,.F.);
#26385=ORIENTED_EDGE('',*,*,#18369,.F.);
#26386=ORIENTED_EDGE('',*,*,#18372,.F.);
#26387=ORIENTED_EDGE('',*,*,#18375,.F.);
#26388=ORIENTED_EDGE('',*,*,#18378,.F.);
#26389=ORIENTED_EDGE('',*,*,#18381,.F.);
#26390=ORIENTED_EDGE('',*,*,#18384,.F.);
#26391=ORIENTED_EDGE('',*,*,#18387,.F.);
#26392=ORIENTED_EDGE('',*,*,#18390,.F.);
#26393=ORIENTED_EDGE('',*,*,#18393,.F.);
#26394=ORIENTED_EDGE('',*,*,#18396,.F.);
#26395=ORIENTED_EDGE('',*,*,#18399,.F.);
#26396=ORIENTED_EDGE('',*,*,#18435,.F.);
#26397=ORIENTED_EDGE('',*,*,#18433,.F.);
#26398=ORIENTED_EDGE('',*,*,#18304,.F.);
#26399=ORIENTED_EDGE('',*,*,#18308,.F.);
#26400=ORIENTED_EDGE('',*,*,#18311,.F.);
#26401=ORIENTED_EDGE('',*,*,#18314,.F.);
#26402=ORIENTED_EDGE('',*,*,#18317,.F.);
#26403=ORIENTED_EDGE('',*,*,#18320,.F.);
#26404=ORIENTED_EDGE('',*,*,#18323,.F.);
#26405=ORIENTED_EDGE('',*,*,#18326,.F.);
#26406=ORIENTED_EDGE('',*,*,#18329,.F.);
#26407=ORIENTED_EDGE('',*,*,#18332,.F.);
#26408=ORIENTED_EDGE('',*,*,#18335,.F.);
#26409=ORIENTED_EDGE('',*,*,#18338,.F.);
#26410=ORIENTED_EDGE('',*,*,#18341,.F.);
#26411=ORIENTED_EDGE('',*,*,#18344,.F.);
#26412=ORIENTED_EDGE('',*,*,#18347,.F.);
#26413=ORIENTED_EDGE('',*,*,#18350,.F.);
#26414=ORIENTED_EDGE('',*,*,#18437,.F.);
#26415=ORIENTED_EDGE('',*,*,#18412,.F.);
#26416=ORIENTED_EDGE('',*,*,#18422,.F.);
#26417=ORIENTED_EDGE('',*,*,#18410,.F.);
#26418=ORIENTED_EDGE('',*,*,#18423,.F.);
#26419=ORIENTED_EDGE('',*,*,#18431,.F.);
#26420=ORIENTED_EDGE('',*,*,#18305,.F.);
#26421=ORIENTED_EDGE('',*,*,#18432,.F.);
#26422=ORIENTED_EDGE('',*,*,#18438,.T.);
#26423=ORIENTED_EDGE('',*,*,#18413,.T.);
#26424=ORIENTED_EDGE('',*,*,#18438,.F.);
#26425=ORIENTED_EDGE('',*,*,#18349,.T.);
#26426=ORIENTED_EDGE('',*,*,#18428,.T.);
#26427=ORIENTED_EDGE('',*,*,#18439,.F.);
#26428=ORIENTED_EDGE('',*,*,#18437,.T.);
#26429=ORIENTED_EDGE('',*,*,#18440,.F.);
#26430=ORIENTED_EDGE('',*,*,#18439,.T.);
#26431=ORIENTED_EDGE('',*,*,#18427,.T.);
#26432=ORIENTED_EDGE('',*,*,#18357,.T.);
#26433=ORIENTED_EDGE('',*,*,#18354,.T.);
#26434=ORIENTED_EDGE('',*,*,#18436,.T.);
#26435=ORIENTED_EDGE('',*,*,#18426,.F.);
#26436=ORIENTED_EDGE('',*,*,#18441,.T.);
#26437=ORIENTED_EDGE('',*,*,#18440,.T.);
#26438=ORIENTED_EDGE('',*,*,#18441,.F.);
#26439=ORIENTED_EDGE('',*,*,#18442,.F.);
#26440=ORIENTED_EDGE('',*,*,#18443,.T.);
#26441=ORIENTED_EDGE('',*,*,#18424,.T.);
#26442=ORIENTED_EDGE('',*,*,#18443,.F.);
#26443=ORIENTED_EDGE('',*,*,#18442,.T.);
#26444=ORIENTED_EDGE('',*,*,#18444,.F.);
#26445=ORIENTED_EDGE('',*,*,#18445,.F.);
#26446=ORIENTED_EDGE('',*,*,#18446,.T.);
#26447=ORIENTED_EDGE('',*,*,#18444,.T.);
#26448=ORIENTED_EDGE('',*,*,#18446,.F.);
#26449=ORIENTED_EDGE('',*,*,#18416,.F.);
#26450=ORIENTED_EDGE('',*,*,#18447,.T.);
#26451=ORIENTED_EDGE('',*,*,#18445,.T.);
#26452=ORIENTED_EDGE('',*,*,#18447,.F.);
#26453=ORIENTED_EDGE('',*,*,#18448,.F.);
#26454=ORIENTED_EDGE('',*,*,#18449,.T.);
#26455=ORIENTED_EDGE('',*,*,#18450,.T.);
#26456=ORIENTED_EDGE('',*,*,#18451,.T.);
#26457=ORIENTED_EDGE('',*,*,#18452,.F.);
#26458=ORIENTED_EDGE('',*,*,#18453,.T.);
#26459=ORIENTED_EDGE('',*,*,#18448,.T.);
#26460=ORIENTED_EDGE('',*,*,#18454,.T.);
#26461=ORIENTED_EDGE('',*,*,#18455,.F.);
#26462=ORIENTED_EDGE('',*,*,#18456,.T.);
#26463=ORIENTED_EDGE('',*,*,#18452,.T.);
#26464=ORIENTED_EDGE('',*,*,#18457,.T.);
#26465=ORIENTED_EDGE('',*,*,#18458,.F.);
#26466=ORIENTED_EDGE('',*,*,#18459,.T.);
#26467=ORIENTED_EDGE('',*,*,#18455,.T.);
#26468=ORIENTED_EDGE('',*,*,#18460,.T.);
#26469=ORIENTED_EDGE('',*,*,#18461,.F.);
#26470=ORIENTED_EDGE('',*,*,#18462,.T.);
#26471=ORIENTED_EDGE('',*,*,#18458,.T.);
#26472=ORIENTED_EDGE('',*,*,#18463,.T.);
#26473=ORIENTED_EDGE('',*,*,#18464,.F.);
#26474=ORIENTED_EDGE('',*,*,#18465,.T.);
#26475=ORIENTED_EDGE('',*,*,#18461,.T.);
#26476=ORIENTED_EDGE('',*,*,#18466,.T.);
#26477=ORIENTED_EDGE('',*,*,#18467,.F.);
#26478=ORIENTED_EDGE('',*,*,#18468,.T.);
#26479=ORIENTED_EDGE('',*,*,#18464,.T.);
#26480=ORIENTED_EDGE('',*,*,#18469,.T.);
#26481=ORIENTED_EDGE('',*,*,#18470,.F.);
#26482=ORIENTED_EDGE('',*,*,#18471,.T.);
#26483=ORIENTED_EDGE('',*,*,#18467,.T.);
#26484=ORIENTED_EDGE('',*,*,#18472,.T.);
#26485=ORIENTED_EDGE('',*,*,#18473,.F.);
#26486=ORIENTED_EDGE('',*,*,#18474,.T.);
#26487=ORIENTED_EDGE('',*,*,#18470,.T.);
#26488=ORIENTED_EDGE('',*,*,#18475,.T.);
#26489=ORIENTED_EDGE('',*,*,#18476,.F.);
#26490=ORIENTED_EDGE('',*,*,#18477,.T.);
#26491=ORIENTED_EDGE('',*,*,#18473,.T.);
#26492=ORIENTED_EDGE('',*,*,#18478,.T.);
#26493=ORIENTED_EDGE('',*,*,#18479,.F.);
#26494=ORIENTED_EDGE('',*,*,#18480,.T.);
#26495=ORIENTED_EDGE('',*,*,#18476,.T.);
#26496=ORIENTED_EDGE('',*,*,#18481,.T.);
#26497=ORIENTED_EDGE('',*,*,#18482,.F.);
#26498=ORIENTED_EDGE('',*,*,#18483,.T.);
#26499=ORIENTED_EDGE('',*,*,#18479,.T.);
#26500=ORIENTED_EDGE('',*,*,#18484,.T.);
#26501=ORIENTED_EDGE('',*,*,#18485,.F.);
#26502=ORIENTED_EDGE('',*,*,#18486,.T.);
#26503=ORIENTED_EDGE('',*,*,#18482,.T.);
#26504=ORIENTED_EDGE('',*,*,#18487,.T.);
#26505=ORIENTED_EDGE('',*,*,#18488,.F.);
#26506=ORIENTED_EDGE('',*,*,#18489,.T.);
#26507=ORIENTED_EDGE('',*,*,#18485,.T.);
#26508=ORIENTED_EDGE('',*,*,#18490,.T.);
#26509=ORIENTED_EDGE('',*,*,#18491,.F.);
#26510=ORIENTED_EDGE('',*,*,#18492,.T.);
#26511=ORIENTED_EDGE('',*,*,#18488,.T.);
#26512=ORIENTED_EDGE('',*,*,#18493,.T.);
#26513=ORIENTED_EDGE('',*,*,#18494,.F.);
#26514=ORIENTED_EDGE('',*,*,#18495,.T.);
#26515=ORIENTED_EDGE('',*,*,#18491,.T.);
#26516=ORIENTED_EDGE('',*,*,#18496,.T.);
#26517=ORIENTED_EDGE('',*,*,#18497,.F.);
#26518=ORIENTED_EDGE('',*,*,#18498,.T.);
#26519=ORIENTED_EDGE('',*,*,#18494,.T.);
#26520=ORIENTED_EDGE('',*,*,#18499,.T.);
#26521=ORIENTED_EDGE('',*,*,#18500,.F.);
#26522=ORIENTED_EDGE('',*,*,#18501,.T.);
#26523=ORIENTED_EDGE('',*,*,#18497,.T.);
#26524=ORIENTED_EDGE('',*,*,#18502,.T.);
#26525=ORIENTED_EDGE('',*,*,#18503,.F.);
#26526=ORIENTED_EDGE('',*,*,#18504,.T.);
#26527=ORIENTED_EDGE('',*,*,#18500,.T.);
#26528=ORIENTED_EDGE('',*,*,#18505,.T.);
#26529=ORIENTED_EDGE('',*,*,#18506,.F.);
#26530=ORIENTED_EDGE('',*,*,#18507,.T.);
#26531=ORIENTED_EDGE('',*,*,#18503,.T.);
#26532=ORIENTED_EDGE('',*,*,#18508,.T.);
#26533=ORIENTED_EDGE('',*,*,#18509,.F.);
#26534=ORIENTED_EDGE('',*,*,#18510,.T.);
#26535=ORIENTED_EDGE('',*,*,#18506,.T.);
#26536=ORIENTED_EDGE('',*,*,#18511,.T.);
#26537=ORIENTED_EDGE('',*,*,#18512,.F.);
#26538=ORIENTED_EDGE('',*,*,#18513,.T.);
#26539=ORIENTED_EDGE('',*,*,#18509,.T.);
#26540=ORIENTED_EDGE('',*,*,#18514,.T.);
#26541=ORIENTED_EDGE('',*,*,#18515,.F.);
#26542=ORIENTED_EDGE('',*,*,#18516,.T.);
#26543=ORIENTED_EDGE('',*,*,#18512,.T.);
#26544=ORIENTED_EDGE('',*,*,#18517,.T.);
#26545=ORIENTED_EDGE('',*,*,#18518,.F.);
#26546=ORIENTED_EDGE('',*,*,#18519,.T.);
#26547=ORIENTED_EDGE('',*,*,#18515,.T.);
#26548=ORIENTED_EDGE('',*,*,#18520,.T.);
#26549=ORIENTED_EDGE('',*,*,#18521,.F.);
#26550=ORIENTED_EDGE('',*,*,#18522,.T.);
#26551=ORIENTED_EDGE('',*,*,#18518,.T.);
#26552=ORIENTED_EDGE('',*,*,#18523,.T.);
#26553=ORIENTED_EDGE('',*,*,#18524,.F.);
#26554=ORIENTED_EDGE('',*,*,#18525,.T.);
#26555=ORIENTED_EDGE('',*,*,#18521,.T.);
#26556=ORIENTED_EDGE('',*,*,#18526,.T.);
#26557=ORIENTED_EDGE('',*,*,#18527,.F.);
#26558=ORIENTED_EDGE('',*,*,#18528,.T.);
#26559=ORIENTED_EDGE('',*,*,#18524,.T.);
#26560=ORIENTED_EDGE('',*,*,#18529,.T.);
#26561=ORIENTED_EDGE('',*,*,#18530,.F.);
#26562=ORIENTED_EDGE('',*,*,#18531,.T.);
#26563=ORIENTED_EDGE('',*,*,#18527,.T.);
#26564=ORIENTED_EDGE('',*,*,#18532,.T.);
#26565=ORIENTED_EDGE('',*,*,#18533,.F.);
#26566=ORIENTED_EDGE('',*,*,#18534,.T.);
#26567=ORIENTED_EDGE('',*,*,#18530,.T.);
#26568=ORIENTED_EDGE('',*,*,#18535,.T.);
#26569=ORIENTED_EDGE('',*,*,#18536,.F.);
#26570=ORIENTED_EDGE('',*,*,#18537,.T.);
#26571=ORIENTED_EDGE('',*,*,#18533,.T.);
#26572=ORIENTED_EDGE('',*,*,#18538,.T.);
#26573=ORIENTED_EDGE('',*,*,#18539,.F.);
#26574=ORIENTED_EDGE('',*,*,#18540,.T.);
#26575=ORIENTED_EDGE('',*,*,#18536,.T.);
#26576=ORIENTED_EDGE('',*,*,#18541,.T.);
#26577=ORIENTED_EDGE('',*,*,#18542,.F.);
#26578=ORIENTED_EDGE('',*,*,#18543,.T.);
#26579=ORIENTED_EDGE('',*,*,#18539,.T.);
#26580=ORIENTED_EDGE('',*,*,#18544,.T.);
#26581=ORIENTED_EDGE('',*,*,#18545,.F.);
#26582=ORIENTED_EDGE('',*,*,#18546,.T.);
#26583=ORIENTED_EDGE('',*,*,#18542,.T.);
#26584=ORIENTED_EDGE('',*,*,#18547,.T.);
#26585=ORIENTED_EDGE('',*,*,#18548,.F.);
#26586=ORIENTED_EDGE('',*,*,#18549,.T.);
#26587=ORIENTED_EDGE('',*,*,#18545,.T.);
#26588=ORIENTED_EDGE('',*,*,#18550,.T.);
#26589=ORIENTED_EDGE('',*,*,#18551,.F.);
#26590=ORIENTED_EDGE('',*,*,#18552,.T.);
#26591=ORIENTED_EDGE('',*,*,#18548,.T.);
#26592=ORIENTED_EDGE('',*,*,#18553,.T.);
#26593=ORIENTED_EDGE('',*,*,#18554,.F.);
#26594=ORIENTED_EDGE('',*,*,#18555,.T.);
#26595=ORIENTED_EDGE('',*,*,#18551,.T.);
#26596=ORIENTED_EDGE('',*,*,#18556,.T.);
#26597=ORIENTED_EDGE('',*,*,#18557,.F.);
#26598=ORIENTED_EDGE('',*,*,#18558,.T.);
#26599=ORIENTED_EDGE('',*,*,#18554,.T.);
#26600=ORIENTED_EDGE('',*,*,#18559,.T.);
#26601=ORIENTED_EDGE('',*,*,#18560,.F.);
#26602=ORIENTED_EDGE('',*,*,#18561,.T.);
#26603=ORIENTED_EDGE('',*,*,#18557,.T.);
#26604=ORIENTED_EDGE('',*,*,#18562,.T.);
#26605=ORIENTED_EDGE('',*,*,#18563,.F.);
#26606=ORIENTED_EDGE('',*,*,#18564,.T.);
#26607=ORIENTED_EDGE('',*,*,#18560,.T.);
#26608=ORIENTED_EDGE('',*,*,#18565,.T.);
#26609=ORIENTED_EDGE('',*,*,#18566,.F.);
#26610=ORIENTED_EDGE('',*,*,#18567,.T.);
#26611=ORIENTED_EDGE('',*,*,#18563,.T.);
#26612=ORIENTED_EDGE('',*,*,#18568,.T.);
#26613=ORIENTED_EDGE('',*,*,#18569,.F.);
#26614=ORIENTED_EDGE('',*,*,#18570,.T.);
#26615=ORIENTED_EDGE('',*,*,#18566,.T.);
#26616=ORIENTED_EDGE('',*,*,#18571,.T.);
#26617=ORIENTED_EDGE('',*,*,#18572,.F.);
#26618=ORIENTED_EDGE('',*,*,#18573,.T.);
#26619=ORIENTED_EDGE('',*,*,#18569,.T.);
#26620=ORIENTED_EDGE('',*,*,#18574,.T.);
#26621=ORIENTED_EDGE('',*,*,#18575,.F.);
#26622=ORIENTED_EDGE('',*,*,#18576,.T.);
#26623=ORIENTED_EDGE('',*,*,#18572,.T.);
#26624=ORIENTED_EDGE('',*,*,#18577,.T.);
#26625=ORIENTED_EDGE('',*,*,#18578,.F.);
#26626=ORIENTED_EDGE('',*,*,#18579,.T.);
#26627=ORIENTED_EDGE('',*,*,#18575,.T.);
#26628=ORIENTED_EDGE('',*,*,#18580,.T.);
#26629=ORIENTED_EDGE('',*,*,#18581,.F.);
#26630=ORIENTED_EDGE('',*,*,#18582,.T.);
#26631=ORIENTED_EDGE('',*,*,#18578,.T.);
#26632=ORIENTED_EDGE('',*,*,#18583,.T.);
#26633=ORIENTED_EDGE('',*,*,#18584,.F.);
#26634=ORIENTED_EDGE('',*,*,#18585,.T.);
#26635=ORIENTED_EDGE('',*,*,#18581,.T.);
#26636=ORIENTED_EDGE('',*,*,#18586,.T.);
#26637=ORIENTED_EDGE('',*,*,#18587,.F.);
#26638=ORIENTED_EDGE('',*,*,#18588,.T.);
#26639=ORIENTED_EDGE('',*,*,#18584,.T.);
#26640=ORIENTED_EDGE('',*,*,#18589,.T.);
#26641=ORIENTED_EDGE('',*,*,#18590,.F.);
#26642=ORIENTED_EDGE('',*,*,#18591,.T.);
#26643=ORIENTED_EDGE('',*,*,#18587,.T.);
#26644=ORIENTED_EDGE('',*,*,#18592,.T.);
#26645=ORIENTED_EDGE('',*,*,#18593,.F.);
#26646=ORIENTED_EDGE('',*,*,#18594,.T.);
#26647=ORIENTED_EDGE('',*,*,#18590,.T.);
#26648=ORIENTED_EDGE('',*,*,#18595,.T.);
#26649=ORIENTED_EDGE('',*,*,#18596,.F.);
#26650=ORIENTED_EDGE('',*,*,#18597,.T.);
#26651=ORIENTED_EDGE('',*,*,#18593,.T.);
#26652=ORIENTED_EDGE('',*,*,#18598,.T.);
#26653=ORIENTED_EDGE('',*,*,#18599,.F.);
#26654=ORIENTED_EDGE('',*,*,#18600,.T.);
#26655=ORIENTED_EDGE('',*,*,#18596,.T.);
#26656=ORIENTED_EDGE('',*,*,#18601,.T.);
#26657=ORIENTED_EDGE('',*,*,#18602,.F.);
#26658=ORIENTED_EDGE('',*,*,#18603,.T.);
#26659=ORIENTED_EDGE('',*,*,#18599,.T.);
#26660=ORIENTED_EDGE('',*,*,#18604,.T.);
#26661=ORIENTED_EDGE('',*,*,#18605,.F.);
#26662=ORIENTED_EDGE('',*,*,#18606,.T.);
#26663=ORIENTED_EDGE('',*,*,#18602,.T.);
#26664=ORIENTED_EDGE('',*,*,#18607,.T.);
#26665=ORIENTED_EDGE('',*,*,#18608,.F.);
#26666=ORIENTED_EDGE('',*,*,#18609,.T.);
#26667=ORIENTED_EDGE('',*,*,#18605,.T.);
#26668=ORIENTED_EDGE('',*,*,#18610,.T.);
#26669=ORIENTED_EDGE('',*,*,#18611,.F.);
#26670=ORIENTED_EDGE('',*,*,#18612,.T.);
#26671=ORIENTED_EDGE('',*,*,#18608,.T.);
#26672=ORIENTED_EDGE('',*,*,#18613,.T.);
#26673=ORIENTED_EDGE('',*,*,#18614,.F.);
#26674=ORIENTED_EDGE('',*,*,#18615,.T.);
#26675=ORIENTED_EDGE('',*,*,#18611,.T.);
#26676=ORIENTED_EDGE('',*,*,#18616,.T.);
#26677=ORIENTED_EDGE('',*,*,#18617,.F.);
#26678=ORIENTED_EDGE('',*,*,#18618,.T.);
#26679=ORIENTED_EDGE('',*,*,#18614,.T.);
#26680=ORIENTED_EDGE('',*,*,#18619,.T.);
#26681=ORIENTED_EDGE('',*,*,#18620,.F.);
#26682=ORIENTED_EDGE('',*,*,#18621,.T.);
#26683=ORIENTED_EDGE('',*,*,#18617,.T.);
#26684=ORIENTED_EDGE('',*,*,#18622,.T.);
#26685=ORIENTED_EDGE('',*,*,#18623,.F.);
#26686=ORIENTED_EDGE('',*,*,#18624,.T.);
#26687=ORIENTED_EDGE('',*,*,#18620,.T.);
#26688=ORIENTED_EDGE('',*,*,#18625,.T.);
#26689=ORIENTED_EDGE('',*,*,#18626,.F.);
#26690=ORIENTED_EDGE('',*,*,#18627,.T.);
#26691=ORIENTED_EDGE('',*,*,#18623,.T.);
#26692=ORIENTED_EDGE('',*,*,#18628,.T.);
#26693=ORIENTED_EDGE('',*,*,#18629,.F.);
#26694=ORIENTED_EDGE('',*,*,#18630,.T.);
#26695=ORIENTED_EDGE('',*,*,#18626,.T.);
#26696=ORIENTED_EDGE('',*,*,#18631,.T.);
#26697=ORIENTED_EDGE('',*,*,#18632,.F.);
#26698=ORIENTED_EDGE('',*,*,#18633,.T.);
#26699=ORIENTED_EDGE('',*,*,#18629,.T.);
#26700=ORIENTED_EDGE('',*,*,#18634,.T.);
#26701=ORIENTED_EDGE('',*,*,#18635,.F.);
#26702=ORIENTED_EDGE('',*,*,#18636,.T.);
#26703=ORIENTED_EDGE('',*,*,#18632,.T.);
#26704=ORIENTED_EDGE('',*,*,#18637,.T.);
#26705=ORIENTED_EDGE('',*,*,#18638,.F.);
#26706=ORIENTED_EDGE('',*,*,#18639,.T.);
#26707=ORIENTED_EDGE('',*,*,#18635,.T.);
#26708=ORIENTED_EDGE('',*,*,#18640,.T.);
#26709=ORIENTED_EDGE('',*,*,#18641,.F.);
#26710=ORIENTED_EDGE('',*,*,#18642,.T.);
#26711=ORIENTED_EDGE('',*,*,#18638,.T.);
#26712=ORIENTED_EDGE('',*,*,#18643,.T.);
#26713=ORIENTED_EDGE('',*,*,#18644,.F.);
#26714=ORIENTED_EDGE('',*,*,#18645,.T.);
#26715=ORIENTED_EDGE('',*,*,#18641,.T.);
#26716=ORIENTED_EDGE('',*,*,#18646,.T.);
#26717=ORIENTED_EDGE('',*,*,#18647,.F.);
#26718=ORIENTED_EDGE('',*,*,#18648,.T.);
#26719=ORIENTED_EDGE('',*,*,#18644,.T.);
#26720=ORIENTED_EDGE('',*,*,#18649,.T.);
#26721=ORIENTED_EDGE('',*,*,#18650,.F.);
#26722=ORIENTED_EDGE('',*,*,#18651,.T.);
#26723=ORIENTED_EDGE('',*,*,#18647,.T.);
#26724=ORIENTED_EDGE('',*,*,#18652,.T.);
#26725=ORIENTED_EDGE('',*,*,#18653,.F.);
#26726=ORIENTED_EDGE('',*,*,#18654,.T.);
#26727=ORIENTED_EDGE('',*,*,#18650,.T.);
#26728=ORIENTED_EDGE('',*,*,#18655,.T.);
#26729=ORIENTED_EDGE('',*,*,#18656,.F.);
#26730=ORIENTED_EDGE('',*,*,#18657,.T.);
#26731=ORIENTED_EDGE('',*,*,#18653,.T.);
#26732=ORIENTED_EDGE('',*,*,#18658,.T.);
#26733=ORIENTED_EDGE('',*,*,#18659,.F.);
#26734=ORIENTED_EDGE('',*,*,#18660,.T.);
#26735=ORIENTED_EDGE('',*,*,#18656,.T.);
#26736=ORIENTED_EDGE('',*,*,#18661,.T.);
#26737=ORIENTED_EDGE('',*,*,#18662,.F.);
#26738=ORIENTED_EDGE('',*,*,#18663,.T.);
#26739=ORIENTED_EDGE('',*,*,#18659,.T.);
#26740=ORIENTED_EDGE('',*,*,#18664,.T.);
#26741=ORIENTED_EDGE('',*,*,#18665,.F.);
#26742=ORIENTED_EDGE('',*,*,#18666,.T.);
#26743=ORIENTED_EDGE('',*,*,#18662,.T.);
#26744=ORIENTED_EDGE('',*,*,#18667,.T.);
#26745=ORIENTED_EDGE('',*,*,#18668,.F.);
#26746=ORIENTED_EDGE('',*,*,#18669,.T.);
#26747=ORIENTED_EDGE('',*,*,#18665,.T.);
#26748=ORIENTED_EDGE('',*,*,#18670,.T.);
#26749=ORIENTED_EDGE('',*,*,#18671,.F.);
#26750=ORIENTED_EDGE('',*,*,#18672,.T.);
#26751=ORIENTED_EDGE('',*,*,#18668,.T.);
#26752=ORIENTED_EDGE('',*,*,#18673,.T.);
#26753=ORIENTED_EDGE('',*,*,#18674,.F.);
#26754=ORIENTED_EDGE('',*,*,#18675,.T.);
#26755=ORIENTED_EDGE('',*,*,#18676,.F.);
#26756=ORIENTED_EDGE('',*,*,#18677,.F.);
#26757=ORIENTED_EDGE('',*,*,#18678,.F.);
#26758=ORIENTED_EDGE('',*,*,#18679,.T.);
#26759=ORIENTED_EDGE('',*,*,#18674,.T.);
#26760=ORIENTED_EDGE('',*,*,#18680,.F.);
#26761=ORIENTED_EDGE('',*,*,#18681,.F.);
#26762=ORIENTED_EDGE('',*,*,#18682,.T.);
#26763=ORIENTED_EDGE('',*,*,#18678,.T.);
#26764=ORIENTED_EDGE('',*,*,#18683,.F.);
#26765=ORIENTED_EDGE('',*,*,#18684,.F.);
#26766=ORIENTED_EDGE('',*,*,#18685,.T.);
#26767=ORIENTED_EDGE('',*,*,#18681,.T.);
#26768=ORIENTED_EDGE('',*,*,#18686,.F.);
#26769=ORIENTED_EDGE('',*,*,#18687,.F.);
#26770=ORIENTED_EDGE('',*,*,#18688,.T.);
#26771=ORIENTED_EDGE('',*,*,#18684,.T.);
#26772=ORIENTED_EDGE('',*,*,#18689,.F.);
#26773=ORIENTED_EDGE('',*,*,#18690,.F.);
#26774=ORIENTED_EDGE('',*,*,#18691,.T.);
#26775=ORIENTED_EDGE('',*,*,#18687,.T.);
#26776=ORIENTED_EDGE('',*,*,#18692,.F.);
#26777=ORIENTED_EDGE('',*,*,#18693,.F.);
#26778=ORIENTED_EDGE('',*,*,#18694,.T.);
#26779=ORIENTED_EDGE('',*,*,#18690,.T.);
#26780=ORIENTED_EDGE('',*,*,#18695,.F.);
#26781=ORIENTED_EDGE('',*,*,#18696,.F.);
#26782=ORIENTED_EDGE('',*,*,#18697,.T.);
#26783=ORIENTED_EDGE('',*,*,#18693,.T.);
#26784=ORIENTED_EDGE('',*,*,#18698,.F.);
#26785=ORIENTED_EDGE('',*,*,#18699,.F.);
#26786=ORIENTED_EDGE('',*,*,#18700,.T.);
#26787=ORIENTED_EDGE('',*,*,#18696,.T.);
#26788=ORIENTED_EDGE('',*,*,#18701,.F.);
#26789=ORIENTED_EDGE('',*,*,#18702,.F.);
#26790=ORIENTED_EDGE('',*,*,#18703,.T.);
#26791=ORIENTED_EDGE('',*,*,#18699,.T.);
#26792=ORIENTED_EDGE('',*,*,#18704,.F.);
#26793=ORIENTED_EDGE('',*,*,#18705,.F.);
#26794=ORIENTED_EDGE('',*,*,#18706,.T.);
#26795=ORIENTED_EDGE('',*,*,#18702,.T.);
#26796=ORIENTED_EDGE('',*,*,#18707,.F.);
#26797=ORIENTED_EDGE('',*,*,#18708,.F.);
#26798=ORIENTED_EDGE('',*,*,#18709,.T.);
#26799=ORIENTED_EDGE('',*,*,#18705,.T.);
#26800=ORIENTED_EDGE('',*,*,#18710,.F.);
#26801=ORIENTED_EDGE('',*,*,#18711,.F.);
#26802=ORIENTED_EDGE('',*,*,#18712,.T.);
#26803=ORIENTED_EDGE('',*,*,#18708,.T.);
#26804=ORIENTED_EDGE('',*,*,#18713,.F.);
#26805=ORIENTED_EDGE('',*,*,#18714,.F.);
#26806=ORIENTED_EDGE('',*,*,#18715,.T.);
#26807=ORIENTED_EDGE('',*,*,#18711,.T.);
#26808=ORIENTED_EDGE('',*,*,#18716,.F.);
#26809=ORIENTED_EDGE('',*,*,#18717,.F.);
#26810=ORIENTED_EDGE('',*,*,#18718,.T.);
#26811=ORIENTED_EDGE('',*,*,#18714,.T.);
#26812=ORIENTED_EDGE('',*,*,#18719,.F.);
#26813=ORIENTED_EDGE('',*,*,#18720,.F.);
#26814=ORIENTED_EDGE('',*,*,#18721,.T.);
#26815=ORIENTED_EDGE('',*,*,#18717,.T.);
#26816=ORIENTED_EDGE('',*,*,#18722,.F.);
#26817=ORIENTED_EDGE('',*,*,#18723,.F.);
#26818=ORIENTED_EDGE('',*,*,#18724,.T.);
#26819=ORIENTED_EDGE('',*,*,#18720,.T.);
#26820=ORIENTED_EDGE('',*,*,#18725,.F.);
#26821=ORIENTED_EDGE('',*,*,#18726,.F.);
#26822=ORIENTED_EDGE('',*,*,#18727,.T.);
#26823=ORIENTED_EDGE('',*,*,#18723,.T.);
#26824=ORIENTED_EDGE('',*,*,#18728,.F.);
#26825=ORIENTED_EDGE('',*,*,#18729,.F.);
#26826=ORIENTED_EDGE('',*,*,#18730,.T.);
#26827=ORIENTED_EDGE('',*,*,#18726,.T.);
#26828=ORIENTED_EDGE('',*,*,#18731,.F.);
#26829=ORIENTED_EDGE('',*,*,#18732,.F.);
#26830=ORIENTED_EDGE('',*,*,#18733,.T.);
#26831=ORIENTED_EDGE('',*,*,#18729,.T.);
#26832=ORIENTED_EDGE('',*,*,#18734,.F.);
#26833=ORIENTED_EDGE('',*,*,#18735,.F.);
#26834=ORIENTED_EDGE('',*,*,#18736,.T.);
#26835=ORIENTED_EDGE('',*,*,#18732,.T.);
#26836=ORIENTED_EDGE('',*,*,#18737,.F.);
#26837=ORIENTED_EDGE('',*,*,#18738,.F.);
#26838=ORIENTED_EDGE('',*,*,#18739,.T.);
#26839=ORIENTED_EDGE('',*,*,#18735,.T.);
#26840=ORIENTED_EDGE('',*,*,#18740,.F.);
#26841=ORIENTED_EDGE('',*,*,#18741,.F.);
#26842=ORIENTED_EDGE('',*,*,#18742,.T.);
#26843=ORIENTED_EDGE('',*,*,#18738,.T.);
#26844=ORIENTED_EDGE('',*,*,#18743,.F.);
#26845=ORIENTED_EDGE('',*,*,#18744,.F.);
#26846=ORIENTED_EDGE('',*,*,#18745,.T.);
#26847=ORIENTED_EDGE('',*,*,#18741,.T.);
#26848=ORIENTED_EDGE('',*,*,#18746,.F.);
#26849=ORIENTED_EDGE('',*,*,#18747,.F.);
#26850=ORIENTED_EDGE('',*,*,#18748,.T.);
#26851=ORIENTED_EDGE('',*,*,#18744,.T.);
#26852=ORIENTED_EDGE('',*,*,#18749,.F.);
#26853=ORIENTED_EDGE('',*,*,#18750,.F.);
#26854=ORIENTED_EDGE('',*,*,#18751,.T.);
#26855=ORIENTED_EDGE('',*,*,#18747,.T.);
#26856=ORIENTED_EDGE('',*,*,#18752,.F.);
#26857=ORIENTED_EDGE('',*,*,#18753,.F.);
#26858=ORIENTED_EDGE('',*,*,#18754,.T.);
#26859=ORIENTED_EDGE('',*,*,#18750,.T.);
#26860=ORIENTED_EDGE('',*,*,#18755,.F.);
#26861=ORIENTED_EDGE('',*,*,#18756,.F.);
#26862=ORIENTED_EDGE('',*,*,#18757,.T.);
#26863=ORIENTED_EDGE('',*,*,#18753,.T.);
#26864=ORIENTED_EDGE('',*,*,#18758,.F.);
#26865=ORIENTED_EDGE('',*,*,#18759,.F.);
#26866=ORIENTED_EDGE('',*,*,#18760,.T.);
#26867=ORIENTED_EDGE('',*,*,#18756,.T.);
#26868=ORIENTED_EDGE('',*,*,#18761,.F.);
#26869=ORIENTED_EDGE('',*,*,#18762,.F.);
#26870=ORIENTED_EDGE('',*,*,#18763,.T.);
#26871=ORIENTED_EDGE('',*,*,#18759,.T.);
#26872=ORIENTED_EDGE('',*,*,#18764,.F.);
#26873=ORIENTED_EDGE('',*,*,#18765,.F.);
#26874=ORIENTED_EDGE('',*,*,#18766,.T.);
#26875=ORIENTED_EDGE('',*,*,#18762,.T.);
#26876=ORIENTED_EDGE('',*,*,#18767,.F.);
#26877=ORIENTED_EDGE('',*,*,#18768,.F.);
#26878=ORIENTED_EDGE('',*,*,#18769,.T.);
#26879=ORIENTED_EDGE('',*,*,#18765,.T.);
#26880=ORIENTED_EDGE('',*,*,#18770,.F.);
#26881=ORIENTED_EDGE('',*,*,#18771,.F.);
#26882=ORIENTED_EDGE('',*,*,#18772,.T.);
#26883=ORIENTED_EDGE('',*,*,#18768,.T.);
#26884=ORIENTED_EDGE('',*,*,#18773,.F.);
#26885=ORIENTED_EDGE('',*,*,#18774,.F.);
#26886=ORIENTED_EDGE('',*,*,#18775,.T.);
#26887=ORIENTED_EDGE('',*,*,#18771,.T.);
#26888=ORIENTED_EDGE('',*,*,#18776,.F.);
#26889=ORIENTED_EDGE('',*,*,#18777,.F.);
#26890=ORIENTED_EDGE('',*,*,#18778,.T.);
#26891=ORIENTED_EDGE('',*,*,#18774,.T.);
#26892=ORIENTED_EDGE('',*,*,#18779,.F.);
#26893=ORIENTED_EDGE('',*,*,#18780,.F.);
#26894=ORIENTED_EDGE('',*,*,#18781,.T.);
#26895=ORIENTED_EDGE('',*,*,#18777,.T.);
#26896=ORIENTED_EDGE('',*,*,#18782,.F.);
#26897=ORIENTED_EDGE('',*,*,#18783,.F.);
#26898=ORIENTED_EDGE('',*,*,#18784,.T.);
#26899=ORIENTED_EDGE('',*,*,#18780,.T.);
#26900=ORIENTED_EDGE('',*,*,#18785,.F.);
#26901=ORIENTED_EDGE('',*,*,#18786,.F.);
#26902=ORIENTED_EDGE('',*,*,#18787,.T.);
#26903=ORIENTED_EDGE('',*,*,#18783,.T.);
#26904=ORIENTED_EDGE('',*,*,#18788,.F.);
#26905=ORIENTED_EDGE('',*,*,#18789,.F.);
#26906=ORIENTED_EDGE('',*,*,#18790,.T.);
#26907=ORIENTED_EDGE('',*,*,#18786,.T.);
#26908=ORIENTED_EDGE('',*,*,#18791,.F.);
#26909=ORIENTED_EDGE('',*,*,#18792,.F.);
#26910=ORIENTED_EDGE('',*,*,#18793,.T.);
#26911=ORIENTED_EDGE('',*,*,#18789,.T.);
#26912=ORIENTED_EDGE('',*,*,#18794,.F.);
#26913=ORIENTED_EDGE('',*,*,#18795,.F.);
#26914=ORIENTED_EDGE('',*,*,#18796,.T.);
#26915=ORIENTED_EDGE('',*,*,#18792,.T.);
#26916=ORIENTED_EDGE('',*,*,#18797,.F.);
#26917=ORIENTED_EDGE('',*,*,#18798,.F.);
#26918=ORIENTED_EDGE('',*,*,#18799,.T.);
#26919=ORIENTED_EDGE('',*,*,#18795,.T.);
#26920=ORIENTED_EDGE('',*,*,#18800,.F.);
#26921=ORIENTED_EDGE('',*,*,#18801,.F.);
#26922=ORIENTED_EDGE('',*,*,#18802,.T.);
#26923=ORIENTED_EDGE('',*,*,#18798,.T.);
#26924=ORIENTED_EDGE('',*,*,#18803,.F.);
#26925=ORIENTED_EDGE('',*,*,#18804,.F.);
#26926=ORIENTED_EDGE('',*,*,#18805,.T.);
#26927=ORIENTED_EDGE('',*,*,#18801,.T.);
#26928=ORIENTED_EDGE('',*,*,#18806,.F.);
#26929=ORIENTED_EDGE('',*,*,#18807,.F.);
#26930=ORIENTED_EDGE('',*,*,#18808,.T.);
#26931=ORIENTED_EDGE('',*,*,#18804,.T.);
#26932=ORIENTED_EDGE('',*,*,#18809,.F.);
#26933=ORIENTED_EDGE('',*,*,#18810,.F.);
#26934=ORIENTED_EDGE('',*,*,#18811,.T.);
#26935=ORIENTED_EDGE('',*,*,#18807,.T.);
#26936=ORIENTED_EDGE('',*,*,#18812,.F.);
#26937=ORIENTED_EDGE('',*,*,#18813,.F.);
#26938=ORIENTED_EDGE('',*,*,#18814,.T.);
#26939=ORIENTED_EDGE('',*,*,#18810,.T.);
#26940=ORIENTED_EDGE('',*,*,#18815,.F.);
#26941=ORIENTED_EDGE('',*,*,#18816,.F.);
#26942=ORIENTED_EDGE('',*,*,#18817,.T.);
#26943=ORIENTED_EDGE('',*,*,#18813,.T.);
#26944=ORIENTED_EDGE('',*,*,#18818,.F.);
#26945=ORIENTED_EDGE('',*,*,#18819,.F.);
#26946=ORIENTED_EDGE('',*,*,#18820,.T.);
#26947=ORIENTED_EDGE('',*,*,#18816,.T.);
#26948=ORIENTED_EDGE('',*,*,#18821,.F.);
#26949=ORIENTED_EDGE('',*,*,#18822,.F.);
#26950=ORIENTED_EDGE('',*,*,#18823,.T.);
#26951=ORIENTED_EDGE('',*,*,#18819,.T.);
#26952=ORIENTED_EDGE('',*,*,#18824,.F.);
#26953=ORIENTED_EDGE('',*,*,#18825,.F.);
#26954=ORIENTED_EDGE('',*,*,#18826,.T.);
#26955=ORIENTED_EDGE('',*,*,#18822,.T.);
#26956=ORIENTED_EDGE('',*,*,#18827,.F.);
#26957=ORIENTED_EDGE('',*,*,#18828,.F.);
#26958=ORIENTED_EDGE('',*,*,#18829,.T.);
#26959=ORIENTED_EDGE('',*,*,#18825,.T.);
#26960=ORIENTED_EDGE('',*,*,#18830,.F.);
#26961=ORIENTED_EDGE('',*,*,#18831,.F.);
#26962=ORIENTED_EDGE('',*,*,#18832,.T.);
#26963=ORIENTED_EDGE('',*,*,#18828,.T.);
#26964=ORIENTED_EDGE('',*,*,#18833,.F.);
#26965=ORIENTED_EDGE('',*,*,#18834,.F.);
#26966=ORIENTED_EDGE('',*,*,#18835,.T.);
#26967=ORIENTED_EDGE('',*,*,#18831,.T.);
#26968=ORIENTED_EDGE('',*,*,#18836,.F.);
#26969=ORIENTED_EDGE('',*,*,#18837,.F.);
#26970=ORIENTED_EDGE('',*,*,#18838,.T.);
#26971=ORIENTED_EDGE('',*,*,#18834,.T.);
#26972=ORIENTED_EDGE('',*,*,#18839,.F.);
#26973=ORIENTED_EDGE('',*,*,#18840,.F.);
#26974=ORIENTED_EDGE('',*,*,#18841,.T.);
#26975=ORIENTED_EDGE('',*,*,#18837,.T.);
#26976=ORIENTED_EDGE('',*,*,#18842,.F.);
#26977=ORIENTED_EDGE('',*,*,#18843,.F.);
#26978=ORIENTED_EDGE('',*,*,#18844,.T.);
#26979=ORIENTED_EDGE('',*,*,#18840,.T.);
#26980=ORIENTED_EDGE('',*,*,#18845,.F.);
#26981=ORIENTED_EDGE('',*,*,#18846,.F.);
#26982=ORIENTED_EDGE('',*,*,#18847,.T.);
#26983=ORIENTED_EDGE('',*,*,#18843,.T.);
#26984=ORIENTED_EDGE('',*,*,#18848,.F.);
#26985=ORIENTED_EDGE('',*,*,#18849,.F.);
#26986=ORIENTED_EDGE('',*,*,#18850,.T.);
#26987=ORIENTED_EDGE('',*,*,#18846,.T.);
#26988=ORIENTED_EDGE('',*,*,#18851,.F.);
#26989=ORIENTED_EDGE('',*,*,#18852,.F.);
#26990=ORIENTED_EDGE('',*,*,#18853,.T.);
#26991=ORIENTED_EDGE('',*,*,#18849,.T.);
#26992=ORIENTED_EDGE('',*,*,#18854,.F.);
#26993=ORIENTED_EDGE('',*,*,#18855,.F.);
#26994=ORIENTED_EDGE('',*,*,#18856,.T.);
#26995=ORIENTED_EDGE('',*,*,#18852,.T.);
#26996=ORIENTED_EDGE('',*,*,#18857,.F.);
#26997=ORIENTED_EDGE('',*,*,#18858,.F.);
#26998=ORIENTED_EDGE('',*,*,#18859,.T.);
#26999=ORIENTED_EDGE('',*,*,#18855,.T.);
#27000=ORIENTED_EDGE('',*,*,#18860,.F.);
#27001=ORIENTED_EDGE('',*,*,#18861,.F.);
#27002=ORIENTED_EDGE('',*,*,#18862,.T.);
#27003=ORIENTED_EDGE('',*,*,#18858,.T.);
#27004=ORIENTED_EDGE('',*,*,#18863,.F.);
#27005=ORIENTED_EDGE('',*,*,#18864,.F.);
#27006=ORIENTED_EDGE('',*,*,#18865,.T.);
#27007=ORIENTED_EDGE('',*,*,#18861,.T.);
#27008=ORIENTED_EDGE('',*,*,#18866,.F.);
#27009=ORIENTED_EDGE('',*,*,#18867,.F.);
#27010=ORIENTED_EDGE('',*,*,#18868,.T.);
#27011=ORIENTED_EDGE('',*,*,#18864,.T.);
#27012=ORIENTED_EDGE('',*,*,#18869,.F.);
#27013=ORIENTED_EDGE('',*,*,#18870,.F.);
#27014=ORIENTED_EDGE('',*,*,#18871,.T.);
#27015=ORIENTED_EDGE('',*,*,#18867,.T.);
#27016=ORIENTED_EDGE('',*,*,#18872,.F.);
#27017=ORIENTED_EDGE('',*,*,#18873,.F.);
#27018=ORIENTED_EDGE('',*,*,#18874,.T.);
#27019=ORIENTED_EDGE('',*,*,#18870,.T.);
#27020=ORIENTED_EDGE('',*,*,#18875,.F.);
#27021=ORIENTED_EDGE('',*,*,#18876,.F.);
#27022=ORIENTED_EDGE('',*,*,#18877,.T.);
#27023=ORIENTED_EDGE('',*,*,#18873,.T.);
#27024=ORIENTED_EDGE('',*,*,#18878,.F.);
#27025=ORIENTED_EDGE('',*,*,#18879,.F.);
#27026=ORIENTED_EDGE('',*,*,#18880,.T.);
#27027=ORIENTED_EDGE('',*,*,#18876,.T.);
#27028=ORIENTED_EDGE('',*,*,#18881,.F.);
#27029=ORIENTED_EDGE('',*,*,#18882,.F.);
#27030=ORIENTED_EDGE('',*,*,#18883,.T.);
#27031=ORIENTED_EDGE('',*,*,#18879,.T.);
#27032=ORIENTED_EDGE('',*,*,#18884,.F.);
#27033=ORIENTED_EDGE('',*,*,#18885,.F.);
#27034=ORIENTED_EDGE('',*,*,#18886,.T.);
#27035=ORIENTED_EDGE('',*,*,#18882,.T.);
#27036=ORIENTED_EDGE('',*,*,#18887,.F.);
#27037=ORIENTED_EDGE('',*,*,#18888,.F.);
#27038=ORIENTED_EDGE('',*,*,#18889,.T.);
#27039=ORIENTED_EDGE('',*,*,#18885,.T.);
#27040=ORIENTED_EDGE('',*,*,#18890,.F.);
#27041=ORIENTED_EDGE('',*,*,#18891,.F.);
#27042=ORIENTED_EDGE('',*,*,#18892,.T.);
#27043=ORIENTED_EDGE('',*,*,#18888,.T.);
#27044=ORIENTED_EDGE('',*,*,#18893,.F.);
#27045=ORIENTED_EDGE('',*,*,#18894,.F.);
#27046=ORIENTED_EDGE('',*,*,#18895,.T.);
#27047=ORIENTED_EDGE('',*,*,#18891,.T.);
#27048=ORIENTED_EDGE('',*,*,#18896,.F.);
#27049=ORIENTED_EDGE('',*,*,#18897,.F.);
#27050=ORIENTED_EDGE('',*,*,#18898,.T.);
#27051=ORIENTED_EDGE('',*,*,#18894,.T.);
#27052=ORIENTED_EDGE('',*,*,#18899,.F.);
#27053=ORIENTED_EDGE('',*,*,#18676,.T.);
#27054=ORIENTED_EDGE('',*,*,#18900,.T.);
#27055=ORIENTED_EDGE('',*,*,#18901,.F.);
#27056=ORIENTED_EDGE('',*,*,#18902,.F.);
#27057=ORIENTED_EDGE('',*,*,#18903,.T.);
#27058=ORIENTED_EDGE('',*,*,#18903,.F.);
#27059=ORIENTED_EDGE('',*,*,#18904,.F.);
#27060=ORIENTED_EDGE('',*,*,#18673,.F.);
#27061=ORIENTED_EDGE('',*,*,#18670,.F.);
#27062=ORIENTED_EDGE('',*,*,#18667,.F.);
#27063=ORIENTED_EDGE('',*,*,#18664,.F.);
#27064=ORIENTED_EDGE('',*,*,#18661,.F.);
#27065=ORIENTED_EDGE('',*,*,#18658,.F.);
#27066=ORIENTED_EDGE('',*,*,#18655,.F.);
#27067=ORIENTED_EDGE('',*,*,#18652,.F.);
#27068=ORIENTED_EDGE('',*,*,#18649,.F.);
#27069=ORIENTED_EDGE('',*,*,#18646,.F.);
#27070=ORIENTED_EDGE('',*,*,#18643,.F.);
#27071=ORIENTED_EDGE('',*,*,#18640,.F.);
#27072=ORIENTED_EDGE('',*,*,#18637,.F.);
#27073=ORIENTED_EDGE('',*,*,#18634,.F.);
#27074=ORIENTED_EDGE('',*,*,#18631,.F.);
#27075=ORIENTED_EDGE('',*,*,#18628,.F.);
#27076=ORIENTED_EDGE('',*,*,#18625,.F.);
#27077=ORIENTED_EDGE('',*,*,#18622,.F.);
#27078=ORIENTED_EDGE('',*,*,#18619,.F.);
#27079=ORIENTED_EDGE('',*,*,#18616,.F.);
#27080=ORIENTED_EDGE('',*,*,#18613,.F.);
#27081=ORIENTED_EDGE('',*,*,#18610,.F.);
#27082=ORIENTED_EDGE('',*,*,#18607,.F.);
#27083=ORIENTED_EDGE('',*,*,#18604,.F.);
#27084=ORIENTED_EDGE('',*,*,#18601,.F.);
#27085=ORIENTED_EDGE('',*,*,#18598,.F.);
#27086=ORIENTED_EDGE('',*,*,#18595,.F.);
#27087=ORIENTED_EDGE('',*,*,#18592,.F.);
#27088=ORIENTED_EDGE('',*,*,#18589,.F.);
#27089=ORIENTED_EDGE('',*,*,#18586,.F.);
#27090=ORIENTED_EDGE('',*,*,#18583,.F.);
#27091=ORIENTED_EDGE('',*,*,#18580,.F.);
#27092=ORIENTED_EDGE('',*,*,#18577,.F.);
#27093=ORIENTED_EDGE('',*,*,#18574,.F.);
#27094=ORIENTED_EDGE('',*,*,#18571,.F.);
#27095=ORIENTED_EDGE('',*,*,#18568,.F.);
#27096=ORIENTED_EDGE('',*,*,#18565,.F.);
#27097=ORIENTED_EDGE('',*,*,#18562,.F.);
#27098=ORIENTED_EDGE('',*,*,#18559,.F.);
#27099=ORIENTED_EDGE('',*,*,#18556,.F.);
#27100=ORIENTED_EDGE('',*,*,#18553,.F.);
#27101=ORIENTED_EDGE('',*,*,#18550,.F.);
#27102=ORIENTED_EDGE('',*,*,#18547,.F.);
#27103=ORIENTED_EDGE('',*,*,#18544,.F.);
#27104=ORIENTED_EDGE('',*,*,#18541,.F.);
#27105=ORIENTED_EDGE('',*,*,#18538,.F.);
#27106=ORIENTED_EDGE('',*,*,#18535,.F.);
#27107=ORIENTED_EDGE('',*,*,#18532,.F.);
#27108=ORIENTED_EDGE('',*,*,#18529,.F.);
#27109=ORIENTED_EDGE('',*,*,#18526,.F.);
#27110=ORIENTED_EDGE('',*,*,#18523,.F.);
#27111=ORIENTED_EDGE('',*,*,#18520,.F.);
#27112=ORIENTED_EDGE('',*,*,#18517,.F.);
#27113=ORIENTED_EDGE('',*,*,#18514,.F.);
#27114=ORIENTED_EDGE('',*,*,#18511,.F.);
#27115=ORIENTED_EDGE('',*,*,#18508,.F.);
#27116=ORIENTED_EDGE('',*,*,#18505,.F.);
#27117=ORIENTED_EDGE('',*,*,#18502,.F.);
#27118=ORIENTED_EDGE('',*,*,#18499,.F.);
#27119=ORIENTED_EDGE('',*,*,#18496,.F.);
#27120=ORIENTED_EDGE('',*,*,#18493,.F.);
#27121=ORIENTED_EDGE('',*,*,#18490,.F.);
#27122=ORIENTED_EDGE('',*,*,#18487,.F.);
#27123=ORIENTED_EDGE('',*,*,#18484,.F.);
#27124=ORIENTED_EDGE('',*,*,#18481,.F.);
#27125=ORIENTED_EDGE('',*,*,#18478,.F.);
#27126=ORIENTED_EDGE('',*,*,#18475,.F.);
#27127=ORIENTED_EDGE('',*,*,#18472,.F.);
#27128=ORIENTED_EDGE('',*,*,#18469,.F.);
#27129=ORIENTED_EDGE('',*,*,#18466,.F.);
#27130=ORIENTED_EDGE('',*,*,#18463,.F.);
#27131=ORIENTED_EDGE('',*,*,#18460,.F.);
#27132=ORIENTED_EDGE('',*,*,#18457,.F.);
#27133=ORIENTED_EDGE('',*,*,#18454,.F.);
#27134=ORIENTED_EDGE('',*,*,#18451,.F.);
#27135=ORIENTED_EDGE('',*,*,#18905,.F.);
#27136=ORIENTED_EDGE('',*,*,#18906,.T.);
#27137=ORIENTED_EDGE('',*,*,#18899,.T.);
#27138=ORIENTED_EDGE('',*,*,#18896,.T.);
#27139=ORIENTED_EDGE('',*,*,#18893,.T.);
#27140=ORIENTED_EDGE('',*,*,#18890,.T.);
#27141=ORIENTED_EDGE('',*,*,#18887,.T.);
#27142=ORIENTED_EDGE('',*,*,#18884,.T.);
#27143=ORIENTED_EDGE('',*,*,#18881,.T.);
#27144=ORIENTED_EDGE('',*,*,#18878,.T.);
#27145=ORIENTED_EDGE('',*,*,#18875,.T.);
#27146=ORIENTED_EDGE('',*,*,#18872,.T.);
#27147=ORIENTED_EDGE('',*,*,#18869,.T.);
#27148=ORIENTED_EDGE('',*,*,#18866,.T.);
#27149=ORIENTED_EDGE('',*,*,#18863,.T.);
#27150=ORIENTED_EDGE('',*,*,#18860,.T.);
#27151=ORIENTED_EDGE('',*,*,#18857,.T.);
#27152=ORIENTED_EDGE('',*,*,#18854,.T.);
#27153=ORIENTED_EDGE('',*,*,#18851,.T.);
#27154=ORIENTED_EDGE('',*,*,#18848,.T.);
#27155=ORIENTED_EDGE('',*,*,#18845,.T.);
#27156=ORIENTED_EDGE('',*,*,#18842,.T.);
#27157=ORIENTED_EDGE('',*,*,#18839,.T.);
#27158=ORIENTED_EDGE('',*,*,#18836,.T.);
#27159=ORIENTED_EDGE('',*,*,#18833,.T.);
#27160=ORIENTED_EDGE('',*,*,#18830,.T.);
#27161=ORIENTED_EDGE('',*,*,#18827,.T.);
#27162=ORIENTED_EDGE('',*,*,#18824,.T.);
#27163=ORIENTED_EDGE('',*,*,#18821,.T.);
#27164=ORIENTED_EDGE('',*,*,#18818,.T.);
#27165=ORIENTED_EDGE('',*,*,#18815,.T.);
#27166=ORIENTED_EDGE('',*,*,#18812,.T.);
#27167=ORIENTED_EDGE('',*,*,#18809,.T.);
#27168=ORIENTED_EDGE('',*,*,#18806,.T.);
#27169=ORIENTED_EDGE('',*,*,#18803,.T.);
#27170=ORIENTED_EDGE('',*,*,#18800,.T.);
#27171=ORIENTED_EDGE('',*,*,#18797,.T.);
#27172=ORIENTED_EDGE('',*,*,#18794,.T.);
#27173=ORIENTED_EDGE('',*,*,#18791,.T.);
#27174=ORIENTED_EDGE('',*,*,#18788,.T.);
#27175=ORIENTED_EDGE('',*,*,#18785,.T.);
#27176=ORIENTED_EDGE('',*,*,#18782,.T.);
#27177=ORIENTED_EDGE('',*,*,#18779,.T.);
#27178=ORIENTED_EDGE('',*,*,#18776,.T.);
#27179=ORIENTED_EDGE('',*,*,#18773,.T.);
#27180=ORIENTED_EDGE('',*,*,#18770,.T.);
#27181=ORIENTED_EDGE('',*,*,#18767,.T.);
#27182=ORIENTED_EDGE('',*,*,#18764,.T.);
#27183=ORIENTED_EDGE('',*,*,#18761,.T.);
#27184=ORIENTED_EDGE('',*,*,#18758,.T.);
#27185=ORIENTED_EDGE('',*,*,#18755,.T.);
#27186=ORIENTED_EDGE('',*,*,#18752,.T.);
#27187=ORIENTED_EDGE('',*,*,#18749,.T.);
#27188=ORIENTED_EDGE('',*,*,#18746,.T.);
#27189=ORIENTED_EDGE('',*,*,#18743,.T.);
#27190=ORIENTED_EDGE('',*,*,#18740,.T.);
#27191=ORIENTED_EDGE('',*,*,#18737,.T.);
#27192=ORIENTED_EDGE('',*,*,#18734,.T.);
#27193=ORIENTED_EDGE('',*,*,#18731,.T.);
#27194=ORIENTED_EDGE('',*,*,#18728,.T.);
#27195=ORIENTED_EDGE('',*,*,#18725,.T.);
#27196=ORIENTED_EDGE('',*,*,#18722,.T.);
#27197=ORIENTED_EDGE('',*,*,#18719,.T.);
#27198=ORIENTED_EDGE('',*,*,#18716,.T.);
#27199=ORIENTED_EDGE('',*,*,#18713,.T.);
#27200=ORIENTED_EDGE('',*,*,#18710,.T.);
#27201=ORIENTED_EDGE('',*,*,#18707,.T.);
#27202=ORIENTED_EDGE('',*,*,#18704,.T.);
#27203=ORIENTED_EDGE('',*,*,#18701,.T.);
#27204=ORIENTED_EDGE('',*,*,#18698,.T.);
#27205=ORIENTED_EDGE('',*,*,#18695,.T.);
#27206=ORIENTED_EDGE('',*,*,#18692,.T.);
#27207=ORIENTED_EDGE('',*,*,#18689,.T.);
#27208=ORIENTED_EDGE('',*,*,#18686,.T.);
#27209=ORIENTED_EDGE('',*,*,#18683,.T.);
#27210=ORIENTED_EDGE('',*,*,#18680,.T.);
#27211=ORIENTED_EDGE('',*,*,#18677,.T.);
#27212=ORIENTED_EDGE('',*,*,#18907,.T.);
#27213=ORIENTED_EDGE('',*,*,#18908,.T.);
#27214=ORIENTED_EDGE('',*,*,#18909,.T.);
#27215=ORIENTED_EDGE('',*,*,#18910,.T.);
#27216=ORIENTED_EDGE('',*,*,#18905,.T.);
#27217=ORIENTED_EDGE('',*,*,#18897,.T.);
#27218=ORIENTED_EDGE('',*,*,#18906,.F.);
#27219=ORIENTED_EDGE('',*,*,#18910,.F.);
#27220=ORIENTED_EDGE('',*,*,#18911,.T.);
#27221=ORIENTED_EDGE('',*,*,#18900,.F.);
#27222=ORIENTED_EDGE('',*,*,#18675,.F.);
#27223=ORIENTED_EDGE('',*,*,#18679,.F.);
#27224=ORIENTED_EDGE('',*,*,#18682,.F.);
#27225=ORIENTED_EDGE('',*,*,#18685,.F.);
#27226=ORIENTED_EDGE('',*,*,#18688,.F.);
#27227=ORIENTED_EDGE('',*,*,#18691,.F.);
#27228=ORIENTED_EDGE('',*,*,#18694,.F.);
#27229=ORIENTED_EDGE('',*,*,#18697,.F.);
#27230=ORIENTED_EDGE('',*,*,#18700,.F.);
#27231=ORIENTED_EDGE('',*,*,#18703,.F.);
#27232=ORIENTED_EDGE('',*,*,#18706,.F.);
#27233=ORIENTED_EDGE('',*,*,#18709,.F.);
#27234=ORIENTED_EDGE('',*,*,#18712,.F.);
#27235=ORIENTED_EDGE('',*,*,#18715,.F.);
#27236=ORIENTED_EDGE('',*,*,#18718,.F.);
#27237=ORIENTED_EDGE('',*,*,#18721,.F.);
#27238=ORIENTED_EDGE('',*,*,#18724,.F.);
#27239=ORIENTED_EDGE('',*,*,#18727,.F.);
#27240=ORIENTED_EDGE('',*,*,#18730,.F.);
#27241=ORIENTED_EDGE('',*,*,#18733,.F.);
#27242=ORIENTED_EDGE('',*,*,#18736,.F.);
#27243=ORIENTED_EDGE('',*,*,#18739,.F.);
#27244=ORIENTED_EDGE('',*,*,#18742,.F.);
#27245=ORIENTED_EDGE('',*,*,#18745,.F.);
#27246=ORIENTED_EDGE('',*,*,#18748,.F.);
#27247=ORIENTED_EDGE('',*,*,#18751,.F.);
#27248=ORIENTED_EDGE('',*,*,#18754,.F.);
#27249=ORIENTED_EDGE('',*,*,#18757,.F.);
#27250=ORIENTED_EDGE('',*,*,#18760,.F.);
#27251=ORIENTED_EDGE('',*,*,#18763,.F.);
#27252=ORIENTED_EDGE('',*,*,#18766,.F.);
#27253=ORIENTED_EDGE('',*,*,#18769,.F.);
#27254=ORIENTED_EDGE('',*,*,#18772,.F.);
#27255=ORIENTED_EDGE('',*,*,#18775,.F.);
#27256=ORIENTED_EDGE('',*,*,#18778,.F.);
#27257=ORIENTED_EDGE('',*,*,#18781,.F.);
#27258=ORIENTED_EDGE('',*,*,#18784,.F.);
#27259=ORIENTED_EDGE('',*,*,#18787,.F.);
#27260=ORIENTED_EDGE('',*,*,#18790,.F.);
#27261=ORIENTED_EDGE('',*,*,#18793,.F.);
#27262=ORIENTED_EDGE('',*,*,#18796,.F.);
#27263=ORIENTED_EDGE('',*,*,#18799,.F.);
#27264=ORIENTED_EDGE('',*,*,#18802,.F.);
#27265=ORIENTED_EDGE('',*,*,#18805,.F.);
#27266=ORIENTED_EDGE('',*,*,#18808,.F.);
#27267=ORIENTED_EDGE('',*,*,#18811,.F.);
#27268=ORIENTED_EDGE('',*,*,#18814,.F.);
#27269=ORIENTED_EDGE('',*,*,#18817,.F.);
#27270=ORIENTED_EDGE('',*,*,#18820,.F.);
#27271=ORIENTED_EDGE('',*,*,#18823,.F.);
#27272=ORIENTED_EDGE('',*,*,#18826,.F.);
#27273=ORIENTED_EDGE('',*,*,#18829,.F.);
#27274=ORIENTED_EDGE('',*,*,#18832,.F.);
#27275=ORIENTED_EDGE('',*,*,#18835,.F.);
#27276=ORIENTED_EDGE('',*,*,#18838,.F.);
#27277=ORIENTED_EDGE('',*,*,#18841,.F.);
#27278=ORIENTED_EDGE('',*,*,#18844,.F.);
#27279=ORIENTED_EDGE('',*,*,#18847,.F.);
#27280=ORIENTED_EDGE('',*,*,#18850,.F.);
#27281=ORIENTED_EDGE('',*,*,#18853,.F.);
#27282=ORIENTED_EDGE('',*,*,#18856,.F.);
#27283=ORIENTED_EDGE('',*,*,#18859,.F.);
#27284=ORIENTED_EDGE('',*,*,#18862,.F.);
#27285=ORIENTED_EDGE('',*,*,#18865,.F.);
#27286=ORIENTED_EDGE('',*,*,#18868,.F.);
#27287=ORIENTED_EDGE('',*,*,#18871,.F.);
#27288=ORIENTED_EDGE('',*,*,#18874,.F.);
#27289=ORIENTED_EDGE('',*,*,#18877,.F.);
#27290=ORIENTED_EDGE('',*,*,#18880,.F.);
#27291=ORIENTED_EDGE('',*,*,#18883,.F.);
#27292=ORIENTED_EDGE('',*,*,#18886,.F.);
#27293=ORIENTED_EDGE('',*,*,#18889,.F.);
#27294=ORIENTED_EDGE('',*,*,#18892,.F.);
#27295=ORIENTED_EDGE('',*,*,#18895,.F.);
#27296=ORIENTED_EDGE('',*,*,#18898,.F.);
#27297=ORIENTED_EDGE('',*,*,#18911,.F.);
#27298=ORIENTED_EDGE('',*,*,#18909,.F.);
#27299=ORIENTED_EDGE('',*,*,#18449,.F.);
#27300=ORIENTED_EDGE('',*,*,#18453,.F.);
#27301=ORIENTED_EDGE('',*,*,#18456,.F.);
#27302=ORIENTED_EDGE('',*,*,#18459,.F.);
#27303=ORIENTED_EDGE('',*,*,#18462,.F.);
#27304=ORIENTED_EDGE('',*,*,#18465,.F.);
#27305=ORIENTED_EDGE('',*,*,#18468,.F.);
#27306=ORIENTED_EDGE('',*,*,#18471,.F.);
#27307=ORIENTED_EDGE('',*,*,#18474,.F.);
#27308=ORIENTED_EDGE('',*,*,#18477,.F.);
#27309=ORIENTED_EDGE('',*,*,#18480,.F.);
#27310=ORIENTED_EDGE('',*,*,#18483,.F.);
#27311=ORIENTED_EDGE('',*,*,#18486,.F.);
#27312=ORIENTED_EDGE('',*,*,#18489,.F.);
#27313=ORIENTED_EDGE('',*,*,#18492,.F.);
#27314=ORIENTED_EDGE('',*,*,#18495,.F.);
#27315=ORIENTED_EDGE('',*,*,#18498,.F.);
#27316=ORIENTED_EDGE('',*,*,#18501,.F.);
#27317=ORIENTED_EDGE('',*,*,#18504,.F.);
#27318=ORIENTED_EDGE('',*,*,#18507,.F.);
#27319=ORIENTED_EDGE('',*,*,#18510,.F.);
#27320=ORIENTED_EDGE('',*,*,#18513,.F.);
#27321=ORIENTED_EDGE('',*,*,#18516,.F.);
#27322=ORIENTED_EDGE('',*,*,#18519,.F.);
#27323=ORIENTED_EDGE('',*,*,#18522,.F.);
#27324=ORIENTED_EDGE('',*,*,#18525,.F.);
#27325=ORIENTED_EDGE('',*,*,#18528,.F.);
#27326=ORIENTED_EDGE('',*,*,#18531,.F.);
#27327=ORIENTED_EDGE('',*,*,#18534,.F.);
#27328=ORIENTED_EDGE('',*,*,#18537,.F.);
#27329=ORIENTED_EDGE('',*,*,#18540,.F.);
#27330=ORIENTED_EDGE('',*,*,#18543,.F.);
#27331=ORIENTED_EDGE('',*,*,#18546,.F.);
#27332=ORIENTED_EDGE('',*,*,#18549,.F.);
#27333=ORIENTED_EDGE('',*,*,#18552,.F.);
#27334=ORIENTED_EDGE('',*,*,#18555,.F.);
#27335=ORIENTED_EDGE('',*,*,#18558,.F.);
#27336=ORIENTED_EDGE('',*,*,#18561,.F.);
#27337=ORIENTED_EDGE('',*,*,#18564,.F.);
#27338=ORIENTED_EDGE('',*,*,#18567,.F.);
#27339=ORIENTED_EDGE('',*,*,#18570,.F.);
#27340=ORIENTED_EDGE('',*,*,#18573,.F.);
#27341=ORIENTED_EDGE('',*,*,#18576,.F.);
#27342=ORIENTED_EDGE('',*,*,#18579,.F.);
#27343=ORIENTED_EDGE('',*,*,#18582,.F.);
#27344=ORIENTED_EDGE('',*,*,#18585,.F.);
#27345=ORIENTED_EDGE('',*,*,#18588,.F.);
#27346=ORIENTED_EDGE('',*,*,#18591,.F.);
#27347=ORIENTED_EDGE('',*,*,#18594,.F.);
#27348=ORIENTED_EDGE('',*,*,#18597,.F.);
#27349=ORIENTED_EDGE('',*,*,#18600,.F.);
#27350=ORIENTED_EDGE('',*,*,#18603,.F.);
#27351=ORIENTED_EDGE('',*,*,#18606,.F.);
#27352=ORIENTED_EDGE('',*,*,#18609,.F.);
#27353=ORIENTED_EDGE('',*,*,#18612,.F.);
#27354=ORIENTED_EDGE('',*,*,#18615,.F.);
#27355=ORIENTED_EDGE('',*,*,#18618,.F.);
#27356=ORIENTED_EDGE('',*,*,#18621,.F.);
#27357=ORIENTED_EDGE('',*,*,#18624,.F.);
#27358=ORIENTED_EDGE('',*,*,#18627,.F.);
#27359=ORIENTED_EDGE('',*,*,#18630,.F.);
#27360=ORIENTED_EDGE('',*,*,#18633,.F.);
#27361=ORIENTED_EDGE('',*,*,#18636,.F.);
#27362=ORIENTED_EDGE('',*,*,#18639,.F.);
#27363=ORIENTED_EDGE('',*,*,#18642,.F.);
#27364=ORIENTED_EDGE('',*,*,#18645,.F.);
#27365=ORIENTED_EDGE('',*,*,#18648,.F.);
#27366=ORIENTED_EDGE('',*,*,#18651,.F.);
#27367=ORIENTED_EDGE('',*,*,#18654,.F.);
#27368=ORIENTED_EDGE('',*,*,#18657,.F.);
#27369=ORIENTED_EDGE('',*,*,#18660,.F.);
#27370=ORIENTED_EDGE('',*,*,#18663,.F.);
#27371=ORIENTED_EDGE('',*,*,#18666,.F.);
#27372=ORIENTED_EDGE('',*,*,#18669,.F.);
#27373=ORIENTED_EDGE('',*,*,#18672,.F.);
#27374=ORIENTED_EDGE('',*,*,#18912,.F.);
#27375=ORIENTED_EDGE('',*,*,#18913,.F.);
#27376=ORIENTED_EDGE('',*,*,#18914,.T.);
#27377=ORIENTED_EDGE('',*,*,#18915,.T.);
#27378=ORIENTED_EDGE('',*,*,#18914,.F.);
#27379=ORIENTED_EDGE('',*,*,#18907,.F.);
#27380=ORIENTED_EDGE('',*,*,#18450,.F.);
#27381=ORIENTED_EDGE('',*,*,#18908,.F.);
#27382=ORIENTED_EDGE('',*,*,#18916,.T.);
#27383=ORIENTED_EDGE('',*,*,#18913,.T.);
#27384=ORIENTED_EDGE('',*,*,#18916,.F.);
#27385=ORIENTED_EDGE('',*,*,#18671,.T.);
#27386=ORIENTED_EDGE('',*,*,#18904,.T.);
#27387=ORIENTED_EDGE('',*,*,#18917,.F.);
#27388=ORIENTED_EDGE('',*,*,#18912,.T.);
#27389=ORIENTED_EDGE('',*,*,#18918,.F.);
#27390=ORIENTED_EDGE('',*,*,#18919,.T.);
#27391=ORIENTED_EDGE('',*,*,#18901,.T.);
#27392=ORIENTED_EDGE('',*,*,#18917,.T.);
#27393=ORIENTED_EDGE('',*,*,#18902,.T.);
#27394=ORIENTED_EDGE('',*,*,#18919,.F.);
#27395=ORIENTED_EDGE('',*,*,#18918,.T.);
#27396=ORIENTED_EDGE('',*,*,#18920,.T.);
#27397=ORIENTED_EDGE('',*,*,#18920,.F.);
#27398=ORIENTED_EDGE('',*,*,#18915,.F.);
#27399=ORIENTED_EDGE('',*,*,#18921,.T.);
#27400=ORIENTED_EDGE('',*,*,#18922,.T.);
#27401=ORIENTED_EDGE('',*,*,#18923,.T.);
#27402=ORIENTED_EDGE('',*,*,#18924,.T.);
#27403=ORIENTED_EDGE('',*,*,#18922,.F.);
#27404=ORIENTED_EDGE('',*,*,#18925,.T.);
#27405=ORIENTED_EDGE('',*,*,#18926,.T.);
#27406=ORIENTED_EDGE('',*,*,#18923,.F.);
#27407=ORIENTED_EDGE('',*,*,#18924,.F.);
#27408=ORIENTED_EDGE('',*,*,#18926,.F.);
#27409=ORIENTED_EDGE('',*,*,#18927,.F.);
#27410=ORIENTED_EDGE('',*,*,#18921,.F.);
#27411=ORIENTED_EDGE('',*,*,#18928,.T.);
#27412=ORIENTED_EDGE('',*,*,#18929,.T.);
#27413=ORIENTED_EDGE('',*,*,#18930,.T.);
#27414=ORIENTED_EDGE('',*,*,#18931,.T.);
#27415=ORIENTED_EDGE('',*,*,#18931,.F.);
#27416=ORIENTED_EDGE('',*,*,#18932,.F.);
#27417=ORIENTED_EDGE('',*,*,#18933,.F.);
#27418=ORIENTED_EDGE('',*,*,#18934,.F.);
#27419=ORIENTED_EDGE('',*,*,#18935,.F.);
#27420=ORIENTED_EDGE('',*,*,#18936,.F.);
#27421=ORIENTED_EDGE('',*,*,#18937,.T.);
#27422=ORIENTED_EDGE('',*,*,#18933,.T.);
#27423=ORIENTED_EDGE('',*,*,#18938,.T.);
#27424=ORIENTED_EDGE('',*,*,#18939,.T.);
#27425=ORIENTED_EDGE('',*,*,#18937,.F.);
#27426=ORIENTED_EDGE('',*,*,#18940,.T.);
#27427=ORIENTED_EDGE('',*,*,#18941,.F.);
#27428=ORIENTED_EDGE('',*,*,#18942,.T.);
#27429=ORIENTED_EDGE('',*,*,#18943,.F.);
#27430=ORIENTED_EDGE('',*,*,#18934,.T.);
#27431=ORIENTED_EDGE('',*,*,#18929,.F.);
#27432=ORIENTED_EDGE('',*,*,#18944,.F.);
#27433=ORIENTED_EDGE('',*,*,#18945,.F.);
#27434=ORIENTED_EDGE('',*,*,#18946,.T.);
#27435=ORIENTED_EDGE('',*,*,#18947,.F.);
#27436=ORIENTED_EDGE('',*,*,#18948,.F.);
#27437=ORIENTED_EDGE('',*,*,#18949,.F.);
#27438=ORIENTED_EDGE('',*,*,#18950,.T.);
#27439=ORIENTED_EDGE('',*,*,#18951,.F.);
#27440=ORIENTED_EDGE('',*,*,#18952,.F.);
#27441=ORIENTED_EDGE('',*,*,#18953,.F.);
#27442=ORIENTED_EDGE('',*,*,#18954,.T.);
#27443=ORIENTED_EDGE('',*,*,#18955,.F.);
#27444=ORIENTED_EDGE('',*,*,#18956,.F.);
#27445=ORIENTED_EDGE('',*,*,#18957,.F.);
#27446=ORIENTED_EDGE('',*,*,#18958,.T.);
#27447=ORIENTED_EDGE('',*,*,#18959,.F.);
#27448=ORIENTED_EDGE('',*,*,#18960,.F.);
#27449=ORIENTED_EDGE('',*,*,#18961,.F.);
#27450=ORIENTED_EDGE('',*,*,#18962,.T.);
#27451=ORIENTED_EDGE('',*,*,#18963,.F.);
#27452=ORIENTED_EDGE('',*,*,#18964,.F.);
#27453=ORIENTED_EDGE('',*,*,#18965,.F.);
#27454=ORIENTED_EDGE('',*,*,#18966,.T.);
#27455=ORIENTED_EDGE('',*,*,#18967,.F.);
#27456=ORIENTED_EDGE('',*,*,#18968,.F.);
#27457=ORIENTED_EDGE('',*,*,#18969,.F.);
#27458=ORIENTED_EDGE('',*,*,#18970,.T.);
#27459=ORIENTED_EDGE('',*,*,#18971,.F.);
#27460=ORIENTED_EDGE('',*,*,#18972,.F.);
#27461=ORIENTED_EDGE('',*,*,#18973,.T.);
#27462=ORIENTED_EDGE('',*,*,#18974,.T.);
#27463=ORIENTED_EDGE('',*,*,#18973,.F.);
#27464=ORIENTED_EDGE('',*,*,#18975,.F.);
#27465=ORIENTED_EDGE('',*,*,#18976,.F.);
#27466=ORIENTED_EDGE('',*,*,#18977,.T.);
#27467=ORIENTED_EDGE('',*,*,#18978,.F.);
#27468=ORIENTED_EDGE('',*,*,#18979,.F.);
#27469=ORIENTED_EDGE('',*,*,#18980,.F.);
#27470=ORIENTED_EDGE('',*,*,#18981,.T.);
#27471=ORIENTED_EDGE('',*,*,#18982,.F.);
#27472=ORIENTED_EDGE('',*,*,#18983,.F.);
#27473=ORIENTED_EDGE('',*,*,#18984,.F.);
#27474=ORIENTED_EDGE('',*,*,#18985,.T.);
#27475=ORIENTED_EDGE('',*,*,#18986,.F.);
#27476=ORIENTED_EDGE('',*,*,#18987,.F.);
#27477=ORIENTED_EDGE('',*,*,#18988,.F.);
#27478=ORIENTED_EDGE('',*,*,#18989,.T.);
#27479=ORIENTED_EDGE('',*,*,#18990,.F.);
#27480=ORIENTED_EDGE('',*,*,#18991,.F.);
#27481=ORIENTED_EDGE('',*,*,#18992,.F.);
#27482=ORIENTED_EDGE('',*,*,#18993,.T.);
#27483=ORIENTED_EDGE('',*,*,#18994,.F.);
#27484=ORIENTED_EDGE('',*,*,#18995,.F.);
#27485=ORIENTED_EDGE('',*,*,#18996,.F.);
#27486=ORIENTED_EDGE('',*,*,#18997,.T.);
#27487=ORIENTED_EDGE('',*,*,#18998,.F.);
#27488=ORIENTED_EDGE('',*,*,#18999,.F.);
#27489=ORIENTED_EDGE('',*,*,#19000,.F.);
#27490=ORIENTED_EDGE('',*,*,#19001,.T.);
#27491=ORIENTED_EDGE('',*,*,#19002,.F.);
#27492=ORIENTED_EDGE('',*,*,#18940,.F.);
#27493=ORIENTED_EDGE('',*,*,#18939,.F.);
#27494=ORIENTED_EDGE('',*,*,#19003,.T.);
#27495=ORIENTED_EDGE('',*,*,#18941,.T.);
#27496=ORIENTED_EDGE('',*,*,#19002,.T.);
#27497=ORIENTED_EDGE('',*,*,#19004,.T.);
#27498=ORIENTED_EDGE('',*,*,#19005,.T.);
#27499=ORIENTED_EDGE('',*,*,#19005,.F.);
#27500=ORIENTED_EDGE('',*,*,#19006,.F.);
#27501=ORIENTED_EDGE('',*,*,#19007,.F.);
#27502=ORIENTED_EDGE('',*,*,#19008,.F.);
#27503=ORIENTED_EDGE('',*,*,#19009,.F.);
#27504=ORIENTED_EDGE('',*,*,#18942,.F.);
#27505=ORIENTED_EDGE('',*,*,#19010,.T.);
#27506=ORIENTED_EDGE('',*,*,#19007,.T.);
#27507=ORIENTED_EDGE('',*,*,#19011,.T.);
#27508=ORIENTED_EDGE('',*,*,#19000,.T.);
#27509=ORIENTED_EDGE('',*,*,#19010,.F.);
#27510=ORIENTED_EDGE('',*,*,#18999,.T.);
#27511=ORIENTED_EDGE('',*,*,#19012,.F.);
#27512=ORIENTED_EDGE('',*,*,#19013,.T.);
#27513=ORIENTED_EDGE('',*,*,#19014,.F.);
#27514=ORIENTED_EDGE('',*,*,#19008,.T.);
#27515=ORIENTED_EDGE('',*,*,#19012,.T.);
#27516=ORIENTED_EDGE('',*,*,#18998,.T.);
#27517=ORIENTED_EDGE('',*,*,#19015,.T.);
#27518=ORIENTED_EDGE('',*,*,#19016,.T.);
#27519=ORIENTED_EDGE('',*,*,#19016,.F.);
#27520=ORIENTED_EDGE('',*,*,#19017,.F.);
#27521=ORIENTED_EDGE('',*,*,#19018,.F.);
#27522=ORIENTED_EDGE('',*,*,#19019,.F.);
#27523=ORIENTED_EDGE('',*,*,#19020,.F.);
#27524=ORIENTED_EDGE('',*,*,#19013,.F.);
#27525=ORIENTED_EDGE('',*,*,#19021,.T.);
#27526=ORIENTED_EDGE('',*,*,#19018,.T.);
#27527=ORIENTED_EDGE('',*,*,#19022,.T.);
#27528=ORIENTED_EDGE('',*,*,#18996,.T.);
#27529=ORIENTED_EDGE('',*,*,#19021,.F.);
#27530=ORIENTED_EDGE('',*,*,#18995,.T.);
#27531=ORIENTED_EDGE('',*,*,#19023,.F.);
#27532=ORIENTED_EDGE('',*,*,#19024,.T.);
#27533=ORIENTED_EDGE('',*,*,#19025,.F.);
#27534=ORIENTED_EDGE('',*,*,#19019,.T.);
#27535=ORIENTED_EDGE('',*,*,#19023,.T.);
#27536=ORIENTED_EDGE('',*,*,#18994,.T.);
#27537=ORIENTED_EDGE('',*,*,#19026,.T.);
#27538=ORIENTED_EDGE('',*,*,#19027,.T.);
#27539=ORIENTED_EDGE('',*,*,#19027,.F.);
#27540=ORIENTED_EDGE('',*,*,#19028,.F.);
#27541=ORIENTED_EDGE('',*,*,#19029,.F.);
#27542=ORIENTED_EDGE('',*,*,#19030,.F.);
#27543=ORIENTED_EDGE('',*,*,#19031,.F.);
#27544=ORIENTED_EDGE('',*,*,#19024,.F.);
#27545=ORIENTED_EDGE('',*,*,#19032,.T.);
#27546=ORIENTED_EDGE('',*,*,#19029,.T.);
#27547=ORIENTED_EDGE('',*,*,#19033,.T.);
#27548=ORIENTED_EDGE('',*,*,#18992,.T.);
#27549=ORIENTED_EDGE('',*,*,#19032,.F.);
#27550=ORIENTED_EDGE('',*,*,#18991,.T.);
#27551=ORIENTED_EDGE('',*,*,#19034,.F.);
#27552=ORIENTED_EDGE('',*,*,#19035,.T.);
#27553=ORIENTED_EDGE('',*,*,#19036,.F.);
#27554=ORIENTED_EDGE('',*,*,#19030,.T.);
#27555=ORIENTED_EDGE('',*,*,#19034,.T.);
#27556=ORIENTED_EDGE('',*,*,#18990,.T.);
#27557=ORIENTED_EDGE('',*,*,#19037,.T.);
#27558=ORIENTED_EDGE('',*,*,#19038,.T.);
#27559=ORIENTED_EDGE('',*,*,#19038,.F.);
#27560=ORIENTED_EDGE('',*,*,#19039,.F.);
#27561=ORIENTED_EDGE('',*,*,#19040,.F.);
#27562=ORIENTED_EDGE('',*,*,#19041,.F.);
#27563=ORIENTED_EDGE('',*,*,#19042,.F.);
#27564=ORIENTED_EDGE('',*,*,#19035,.F.);
#27565=ORIENTED_EDGE('',*,*,#19043,.T.);
#27566=ORIENTED_EDGE('',*,*,#19040,.T.);
#27567=ORIENTED_EDGE('',*,*,#19044,.T.);
#27568=ORIENTED_EDGE('',*,*,#18988,.T.);
#27569=ORIENTED_EDGE('',*,*,#19043,.F.);
#27570=ORIENTED_EDGE('',*,*,#18987,.T.);
#27571=ORIENTED_EDGE('',*,*,#19045,.F.);
#27572=ORIENTED_EDGE('',*,*,#19046,.T.);
#27573=ORIENTED_EDGE('',*,*,#19047,.F.);
#27574=ORIENTED_EDGE('',*,*,#19041,.T.);
#27575=ORIENTED_EDGE('',*,*,#19045,.T.);
#27576=ORIENTED_EDGE('',*,*,#18986,.T.);
#27577=ORIENTED_EDGE('',*,*,#19048,.T.);
#27578=ORIENTED_EDGE('',*,*,#19049,.T.);
#27579=ORIENTED_EDGE('',*,*,#19049,.F.);
#27580=ORIENTED_EDGE('',*,*,#19050,.F.);
#27581=ORIENTED_EDGE('',*,*,#19051,.F.);
#27582=ORIENTED_EDGE('',*,*,#19052,.F.);
#27583=ORIENTED_EDGE('',*,*,#19053,.F.);
#27584=ORIENTED_EDGE('',*,*,#19046,.F.);
#27585=ORIENTED_EDGE('',*,*,#19054,.T.);
#27586=ORIENTED_EDGE('',*,*,#19051,.T.);
#27587=ORIENTED_EDGE('',*,*,#19055,.T.);
#27588=ORIENTED_EDGE('',*,*,#18984,.T.);
#27589=ORIENTED_EDGE('',*,*,#19054,.F.);
#27590=ORIENTED_EDGE('',*,*,#18983,.T.);
#27591=ORIENTED_EDGE('',*,*,#19056,.F.);
#27592=ORIENTED_EDGE('',*,*,#19057,.T.);
#27593=ORIENTED_EDGE('',*,*,#19058,.F.);
#27594=ORIENTED_EDGE('',*,*,#19052,.T.);
#27595=ORIENTED_EDGE('',*,*,#19056,.T.);
#27596=ORIENTED_EDGE('',*,*,#18982,.T.);
#27597=ORIENTED_EDGE('',*,*,#19059,.T.);
#27598=ORIENTED_EDGE('',*,*,#19060,.T.);
#27599=ORIENTED_EDGE('',*,*,#19060,.F.);
#27600=ORIENTED_EDGE('',*,*,#19061,.F.);
#27601=ORIENTED_EDGE('',*,*,#19062,.F.);
#27602=ORIENTED_EDGE('',*,*,#19063,.F.);
#27603=ORIENTED_EDGE('',*,*,#19064,.F.);
#27604=ORIENTED_EDGE('',*,*,#19057,.F.);
#27605=ORIENTED_EDGE('',*,*,#19065,.T.);
#27606=ORIENTED_EDGE('',*,*,#19062,.T.);
#27607=ORIENTED_EDGE('',*,*,#19066,.T.);
#27608=ORIENTED_EDGE('',*,*,#18980,.T.);
#27609=ORIENTED_EDGE('',*,*,#19065,.F.);
#27610=ORIENTED_EDGE('',*,*,#18979,.T.);
#27611=ORIENTED_EDGE('',*,*,#19067,.F.);
#27612=ORIENTED_EDGE('',*,*,#19068,.T.);
#27613=ORIENTED_EDGE('',*,*,#19069,.F.);
#27614=ORIENTED_EDGE('',*,*,#19063,.T.);
#27615=ORIENTED_EDGE('',*,*,#19067,.T.);
#27616=ORIENTED_EDGE('',*,*,#18978,.T.);
#27617=ORIENTED_EDGE('',*,*,#19070,.T.);
#27618=ORIENTED_EDGE('',*,*,#19071,.T.);
#27619=ORIENTED_EDGE('',*,*,#19071,.F.);
#27620=ORIENTED_EDGE('',*,*,#19072,.F.);
#27621=ORIENTED_EDGE('',*,*,#19073,.F.);
#27622=ORIENTED_EDGE('',*,*,#19074,.F.);
#27623=ORIENTED_EDGE('',*,*,#19075,.F.);
#27624=ORIENTED_EDGE('',*,*,#19068,.F.);
#27625=ORIENTED_EDGE('',*,*,#19076,.T.);
#27626=ORIENTED_EDGE('',*,*,#19073,.T.);
#27627=ORIENTED_EDGE('',*,*,#19077,.T.);
#27628=ORIENTED_EDGE('',*,*,#18976,.T.);
#27629=ORIENTED_EDGE('',*,*,#19076,.F.);
#27630=ORIENTED_EDGE('',*,*,#18975,.T.);
#27631=ORIENTED_EDGE('',*,*,#18972,.T.);
#27632=ORIENTED_EDGE('',*,*,#19078,.F.);
#27633=ORIENTED_EDGE('',*,*,#19079,.T.);
#27634=ORIENTED_EDGE('',*,*,#19080,.F.);
#27635=ORIENTED_EDGE('',*,*,#19074,.T.);
#27636=ORIENTED_EDGE('',*,*,#19078,.T.);
#27637=ORIENTED_EDGE('',*,*,#18971,.T.);
#27638=ORIENTED_EDGE('',*,*,#19081,.T.);
#27639=ORIENTED_EDGE('',*,*,#19082,.T.);
#27640=ORIENTED_EDGE('',*,*,#19082,.F.);
#27641=ORIENTED_EDGE('',*,*,#19083,.F.);
#27642=ORIENTED_EDGE('',*,*,#19084,.F.);
#27643=ORIENTED_EDGE('',*,*,#19085,.F.);
#27644=ORIENTED_EDGE('',*,*,#19086,.F.);
#27645=ORIENTED_EDGE('',*,*,#19079,.F.);
#27646=ORIENTED_EDGE('',*,*,#19087,.T.);
#27647=ORIENTED_EDGE('',*,*,#19084,.T.);
#27648=ORIENTED_EDGE('',*,*,#19088,.T.);
#27649=ORIENTED_EDGE('',*,*,#18969,.T.);
#27650=ORIENTED_EDGE('',*,*,#19087,.F.);
#27651=ORIENTED_EDGE('',*,*,#18968,.T.);
#27652=ORIENTED_EDGE('',*,*,#19089,.F.);
#27653=ORIENTED_EDGE('',*,*,#19090,.T.);
#27654=ORIENTED_EDGE('',*,*,#19091,.F.);
#27655=ORIENTED_EDGE('',*,*,#19085,.T.);
#27656=ORIENTED_EDGE('',*,*,#19089,.T.);
#27657=ORIENTED_EDGE('',*,*,#18967,.T.);
#27658=ORIENTED_EDGE('',*,*,#19092,.T.);
#27659=ORIENTED_EDGE('',*,*,#19093,.T.);
#27660=ORIENTED_EDGE('',*,*,#19093,.F.);
#27661=ORIENTED_EDGE('',*,*,#19094,.F.);
#27662=ORIENTED_EDGE('',*,*,#19095,.F.);
#27663=ORIENTED_EDGE('',*,*,#19096,.F.);
#27664=ORIENTED_EDGE('',*,*,#19097,.F.);
#27665=ORIENTED_EDGE('',*,*,#19090,.F.);
#27666=ORIENTED_EDGE('',*,*,#19098,.T.);
#27667=ORIENTED_EDGE('',*,*,#19095,.T.);
#27668=ORIENTED_EDGE('',*,*,#19099,.T.);
#27669=ORIENTED_EDGE('',*,*,#18965,.T.);
#27670=ORIENTED_EDGE('',*,*,#19098,.F.);
#27671=ORIENTED_EDGE('',*,*,#18964,.T.);
#27672=ORIENTED_EDGE('',*,*,#19100,.F.);
#27673=ORIENTED_EDGE('',*,*,#19101,.T.);
#27674=ORIENTED_EDGE('',*,*,#19102,.F.);
#27675=ORIENTED_EDGE('',*,*,#19096,.T.);
#27676=ORIENTED_EDGE('',*,*,#19100,.T.);
#27677=ORIENTED_EDGE('',*,*,#18963,.T.);
#27678=ORIENTED_EDGE('',*,*,#19103,.T.);
#27679=ORIENTED_EDGE('',*,*,#19104,.T.);
#27680=ORIENTED_EDGE('',*,*,#19104,.F.);
#27681=ORIENTED_EDGE('',*,*,#19105,.F.);
#27682=ORIENTED_EDGE('',*,*,#19106,.F.);
#27683=ORIENTED_EDGE('',*,*,#19107,.F.);
#27684=ORIENTED_EDGE('',*,*,#19108,.F.);
#27685=ORIENTED_EDGE('',*,*,#19101,.F.);
#27686=ORIENTED_EDGE('',*,*,#19109,.T.);
#27687=ORIENTED_EDGE('',*,*,#19106,.T.);
#27688=ORIENTED_EDGE('',*,*,#19110,.T.);
#27689=ORIENTED_EDGE('',*,*,#18961,.T.);
#27690=ORIENTED_EDGE('',*,*,#19109,.F.);
#27691=ORIENTED_EDGE('',*,*,#18960,.T.);
#27692=ORIENTED_EDGE('',*,*,#19111,.F.);
#27693=ORIENTED_EDGE('',*,*,#19112,.T.);
#27694=ORIENTED_EDGE('',*,*,#19113,.F.);
#27695=ORIENTED_EDGE('',*,*,#19107,.T.);
#27696=ORIENTED_EDGE('',*,*,#19111,.T.);
#27697=ORIENTED_EDGE('',*,*,#18959,.T.);
#27698=ORIENTED_EDGE('',*,*,#19114,.T.);
#27699=ORIENTED_EDGE('',*,*,#19115,.T.);
#27700=ORIENTED_EDGE('',*,*,#19115,.F.);
#27701=ORIENTED_EDGE('',*,*,#19116,.F.);
#27702=ORIENTED_EDGE('',*,*,#19117,.F.);
#27703=ORIENTED_EDGE('',*,*,#19118,.F.);
#27704=ORIENTED_EDGE('',*,*,#19119,.F.);
#27705=ORIENTED_EDGE('',*,*,#19112,.F.);
#27706=ORIENTED_EDGE('',*,*,#19120,.T.);
#27707=ORIENTED_EDGE('',*,*,#19117,.T.);
#27708=ORIENTED_EDGE('',*,*,#19121,.T.);
#27709=ORIENTED_EDGE('',*,*,#18957,.T.);
#27710=ORIENTED_EDGE('',*,*,#19120,.F.);
#27711=ORIENTED_EDGE('',*,*,#18956,.T.);
#27712=ORIENTED_EDGE('',*,*,#19122,.F.);
#27713=ORIENTED_EDGE('',*,*,#19123,.T.);
#27714=ORIENTED_EDGE('',*,*,#19124,.F.);
#27715=ORIENTED_EDGE('',*,*,#19118,.T.);
#27716=ORIENTED_EDGE('',*,*,#19122,.T.);
#27717=ORIENTED_EDGE('',*,*,#18955,.T.);
#27718=ORIENTED_EDGE('',*,*,#19125,.T.);
#27719=ORIENTED_EDGE('',*,*,#19126,.T.);
#27720=ORIENTED_EDGE('',*,*,#19126,.F.);
#27721=ORIENTED_EDGE('',*,*,#19127,.F.);
#27722=ORIENTED_EDGE('',*,*,#19128,.F.);
#27723=ORIENTED_EDGE('',*,*,#19129,.F.);
#27724=ORIENTED_EDGE('',*,*,#19130,.F.);
#27725=ORIENTED_EDGE('',*,*,#19123,.F.);
#27726=ORIENTED_EDGE('',*,*,#19131,.T.);
#27727=ORIENTED_EDGE('',*,*,#19128,.T.);
#27728=ORIENTED_EDGE('',*,*,#19132,.T.);
#27729=ORIENTED_EDGE('',*,*,#18953,.T.);
#27730=ORIENTED_EDGE('',*,*,#19131,.F.);
#27731=ORIENTED_EDGE('',*,*,#18952,.T.);
#27732=ORIENTED_EDGE('',*,*,#19133,.F.);
#27733=ORIENTED_EDGE('',*,*,#19134,.T.);
#27734=ORIENTED_EDGE('',*,*,#19135,.F.);
#27735=ORIENTED_EDGE('',*,*,#19129,.T.);
#27736=ORIENTED_EDGE('',*,*,#19133,.T.);
#27737=ORIENTED_EDGE('',*,*,#18951,.T.);
#27738=ORIENTED_EDGE('',*,*,#19136,.T.);
#27739=ORIENTED_EDGE('',*,*,#19137,.T.);
#27740=ORIENTED_EDGE('',*,*,#19137,.F.);
#27741=ORIENTED_EDGE('',*,*,#19138,.F.);
#27742=ORIENTED_EDGE('',*,*,#19139,.F.);
#27743=ORIENTED_EDGE('',*,*,#19140,.F.);
#27744=ORIENTED_EDGE('',*,*,#19141,.F.);
#27745=ORIENTED_EDGE('',*,*,#19134,.F.);
#27746=ORIENTED_EDGE('',*,*,#19142,.T.);
#27747=ORIENTED_EDGE('',*,*,#19139,.T.);
#27748=ORIENTED_EDGE('',*,*,#19143,.T.);
#27749=ORIENTED_EDGE('',*,*,#18949,.T.);
#27750=ORIENTED_EDGE('',*,*,#19142,.F.);
#27751=ORIENTED_EDGE('',*,*,#18948,.T.);
#27752=ORIENTED_EDGE('',*,*,#19144,.F.);
#27753=ORIENTED_EDGE('',*,*,#19145,.T.);
#27754=ORIENTED_EDGE('',*,*,#19146,.F.);
#27755=ORIENTED_EDGE('',*,*,#19140,.T.);
#27756=ORIENTED_EDGE('',*,*,#19144,.T.);
#27757=ORIENTED_EDGE('',*,*,#18947,.T.);
#27758=ORIENTED_EDGE('',*,*,#19147,.T.);
#27759=ORIENTED_EDGE('',*,*,#19148,.T.);
#27760=ORIENTED_EDGE('',*,*,#19148,.F.);
#27761=ORIENTED_EDGE('',*,*,#19149,.F.);
#27762=ORIENTED_EDGE('',*,*,#19150,.F.);
#27763=ORIENTED_EDGE('',*,*,#19151,.F.);
#27764=ORIENTED_EDGE('',*,*,#19152,.F.);
#27765=ORIENTED_EDGE('',*,*,#19145,.F.);
#27766=ORIENTED_EDGE('',*,*,#19153,.T.);
#27767=ORIENTED_EDGE('',*,*,#19150,.T.);
#27768=ORIENTED_EDGE('',*,*,#19154,.T.);
#27769=ORIENTED_EDGE('',*,*,#18945,.T.);
#27770=ORIENTED_EDGE('',*,*,#19155,.T.);
#27771=ORIENTED_EDGE('',*,*,#19156,.T.);
#27772=ORIENTED_EDGE('',*,*,#19157,.T.);
#27773=ORIENTED_EDGE('',*,*,#19158,.F.);
#27774=ORIENTED_EDGE('',*,*,#19159,.T.);
#27775=ORIENTED_EDGE('',*,*,#19160,.T.);
#27776=ORIENTED_EDGE('',*,*,#19161,.T.);
#27777=ORIENTED_EDGE('',*,*,#19156,.F.);
#27778=ORIENTED_EDGE('',*,*,#19162,.T.);
#27779=ORIENTED_EDGE('',*,*,#19163,.T.);
#27780=ORIENTED_EDGE('',*,*,#19164,.T.);
#27781=ORIENTED_EDGE('',*,*,#19165,.T.);
#27782=ORIENTED_EDGE('',*,*,#19166,.T.);
#27783=ORIENTED_EDGE('',*,*,#19163,.F.);
#27784=ORIENTED_EDGE('',*,*,#19167,.T.);
#27785=ORIENTED_EDGE('',*,*,#19168,.T.);
#27786=ORIENTED_EDGE('',*,*,#19169,.T.);
#27787=ORIENTED_EDGE('',*,*,#19165,.F.);
#27788=ORIENTED_EDGE('',*,*,#19170,.T.);
#27789=ORIENTED_EDGE('',*,*,#19160,.F.);
#27790=ORIENTED_EDGE('',*,*,#19171,.T.);
#27791=ORIENTED_EDGE('',*,*,#19168,.F.);
#27792=ORIENTED_EDGE('',*,*,#19172,.T.);
#27793=ORIENTED_EDGE('',*,*,#19158,.T.);
#27794=ORIENTED_EDGE('',*,*,#19161,.F.);
#27795=ORIENTED_EDGE('',*,*,#19173,.T.);
#27796=ORIENTED_EDGE('',*,*,#19174,.T.);
#27797=ORIENTED_EDGE('',*,*,#19175,.F.);
#27798=ORIENTED_EDGE('',*,*,#19170,.F.);
#27799=ORIENTED_EDGE('',*,*,#19176,.T.);
#27800=ORIENTED_EDGE('',*,*,#19177,.T.);
#27801=ORIENTED_EDGE('',*,*,#19173,.F.);
#27802=ORIENTED_EDGE('',*,*,#19164,.F.);
#27803=ORIENTED_EDGE('',*,*,#19178,.T.);
#27804=ORIENTED_EDGE('',*,*,#19179,.T.);
#27805=ORIENTED_EDGE('',*,*,#19176,.F.);
#27806=ORIENTED_EDGE('',*,*,#19152,.T.);
#27807=ORIENTED_EDGE('',*,*,#19180,.T.);
#27808=ORIENTED_EDGE('',*,*,#18935,.T.);
#27809=ORIENTED_EDGE('',*,*,#18943,.T.);
#27810=ORIENTED_EDGE('',*,*,#19009,.T.);
#27811=ORIENTED_EDGE('',*,*,#19014,.T.);
#27812=ORIENTED_EDGE('',*,*,#19020,.T.);
#27813=ORIENTED_EDGE('',*,*,#19025,.T.);
#27814=ORIENTED_EDGE('',*,*,#19031,.T.);
#27815=ORIENTED_EDGE('',*,*,#19036,.T.);
#27816=ORIENTED_EDGE('',*,*,#19042,.T.);
#27817=ORIENTED_EDGE('',*,*,#19047,.T.);
#27818=ORIENTED_EDGE('',*,*,#19053,.T.);
#27819=ORIENTED_EDGE('',*,*,#19058,.T.);
#27820=ORIENTED_EDGE('',*,*,#19064,.T.);
#27821=ORIENTED_EDGE('',*,*,#19069,.T.);
#27822=ORIENTED_EDGE('',*,*,#19075,.T.);
#27823=ORIENTED_EDGE('',*,*,#19080,.T.);
#27824=ORIENTED_EDGE('',*,*,#19086,.T.);
#27825=ORIENTED_EDGE('',*,*,#19091,.T.);
#27826=ORIENTED_EDGE('',*,*,#19097,.T.);
#27827=ORIENTED_EDGE('',*,*,#19102,.T.);
#27828=ORIENTED_EDGE('',*,*,#19108,.T.);
#27829=ORIENTED_EDGE('',*,*,#19113,.T.);
#27830=ORIENTED_EDGE('',*,*,#19119,.T.);
#27831=ORIENTED_EDGE('',*,*,#19124,.T.);
#27832=ORIENTED_EDGE('',*,*,#19130,.T.);
#27833=ORIENTED_EDGE('',*,*,#19135,.T.);
#27834=ORIENTED_EDGE('',*,*,#19141,.T.);
#27835=ORIENTED_EDGE('',*,*,#19146,.T.);
#27836=ORIENTED_EDGE('',*,*,#19162,.F.);
#27837=ORIENTED_EDGE('',*,*,#19169,.F.);
#27838=ORIENTED_EDGE('',*,*,#19159,.F.);
#27839=ORIENTED_EDGE('',*,*,#19155,.F.);
#27840=ORIENTED_EDGE('',*,*,#19172,.F.);
#27841=ORIENTED_EDGE('',*,*,#19167,.F.);
#27842=ORIENTED_EDGE('',*,*,#19166,.F.);
#27843=ORIENTED_EDGE('',*,*,#19181,.T.);
#27844=ORIENTED_EDGE('',*,*,#19182,.T.);
#27845=ORIENTED_EDGE('',*,*,#19178,.F.);
#27846=ORIENTED_EDGE('',*,*,#19171,.F.);
#27847=ORIENTED_EDGE('',*,*,#19183,.T.);
#27848=ORIENTED_EDGE('',*,*,#19184,.T.);
#27849=ORIENTED_EDGE('',*,*,#19181,.F.);
#27850=ORIENTED_EDGE('',*,*,#19157,.F.);
#27851=ORIENTED_EDGE('',*,*,#19175,.T.);
#27852=ORIENTED_EDGE('',*,*,#19185,.T.);
#27853=ORIENTED_EDGE('',*,*,#19183,.F.);
#27854=ORIENTED_EDGE('',*,*,#19177,.F.);
#27855=ORIENTED_EDGE('',*,*,#19179,.F.);
#27856=ORIENTED_EDGE('',*,*,#19182,.F.);
#27857=ORIENTED_EDGE('',*,*,#19184,.F.);
#27858=ORIENTED_EDGE('',*,*,#19185,.F.);
#27859=ORIENTED_EDGE('',*,*,#19174,.F.);
#27860=ORIENTED_EDGE('',*,*,#18946,.F.);
#27861=ORIENTED_EDGE('',*,*,#19154,.F.);
#27862=ORIENTED_EDGE('',*,*,#19149,.T.);
#27863=ORIENTED_EDGE('',*,*,#19147,.F.);
#27864=ORIENTED_EDGE('',*,*,#18950,.F.);
#27865=ORIENTED_EDGE('',*,*,#19143,.F.);
#27866=ORIENTED_EDGE('',*,*,#19138,.T.);
#27867=ORIENTED_EDGE('',*,*,#19136,.F.);
#27868=ORIENTED_EDGE('',*,*,#18954,.F.);
#27869=ORIENTED_EDGE('',*,*,#19132,.F.);
#27870=ORIENTED_EDGE('',*,*,#19127,.T.);
#27871=ORIENTED_EDGE('',*,*,#19125,.F.);
#27872=ORIENTED_EDGE('',*,*,#18958,.F.);
#27873=ORIENTED_EDGE('',*,*,#19121,.F.);
#27874=ORIENTED_EDGE('',*,*,#19116,.T.);
#27875=ORIENTED_EDGE('',*,*,#19114,.F.);
#27876=ORIENTED_EDGE('',*,*,#18962,.F.);
#27877=ORIENTED_EDGE('',*,*,#19110,.F.);
#27878=ORIENTED_EDGE('',*,*,#19105,.T.);
#27879=ORIENTED_EDGE('',*,*,#19103,.F.);
#27880=ORIENTED_EDGE('',*,*,#18966,.F.);
#27881=ORIENTED_EDGE('',*,*,#19099,.F.);
#27882=ORIENTED_EDGE('',*,*,#19094,.T.);
#27883=ORIENTED_EDGE('',*,*,#19092,.F.);
#27884=ORIENTED_EDGE('',*,*,#18970,.F.);
#27885=ORIENTED_EDGE('',*,*,#19088,.F.);
#27886=ORIENTED_EDGE('',*,*,#19083,.T.);
#27887=ORIENTED_EDGE('',*,*,#19081,.F.);
#27888=ORIENTED_EDGE('',*,*,#18977,.F.);
#27889=ORIENTED_EDGE('',*,*,#19077,.F.);
#27890=ORIENTED_EDGE('',*,*,#19072,.T.);
#27891=ORIENTED_EDGE('',*,*,#19070,.F.);
#27892=ORIENTED_EDGE('',*,*,#18981,.F.);
#27893=ORIENTED_EDGE('',*,*,#19066,.F.);
#27894=ORIENTED_EDGE('',*,*,#19061,.T.);
#27895=ORIENTED_EDGE('',*,*,#19059,.F.);
#27896=ORIENTED_EDGE('',*,*,#18985,.F.);
#27897=ORIENTED_EDGE('',*,*,#19055,.F.);
#27898=ORIENTED_EDGE('',*,*,#19050,.T.);
#27899=ORIENTED_EDGE('',*,*,#19048,.F.);
#27900=ORIENTED_EDGE('',*,*,#18989,.F.);
#27901=ORIENTED_EDGE('',*,*,#19044,.F.);
#27902=ORIENTED_EDGE('',*,*,#19039,.T.);
#27903=ORIENTED_EDGE('',*,*,#19037,.F.);
#27904=ORIENTED_EDGE('',*,*,#18993,.F.);
#27905=ORIENTED_EDGE('',*,*,#19033,.F.);
#27906=ORIENTED_EDGE('',*,*,#19028,.T.);
#27907=ORIENTED_EDGE('',*,*,#19026,.F.);
#27908=ORIENTED_EDGE('',*,*,#18997,.F.);
#27909=ORIENTED_EDGE('',*,*,#19022,.F.);
#27910=ORIENTED_EDGE('',*,*,#19017,.T.);
#27911=ORIENTED_EDGE('',*,*,#19015,.F.);
#27912=ORIENTED_EDGE('',*,*,#19001,.F.);
#27913=ORIENTED_EDGE('',*,*,#19011,.F.);
#27914=ORIENTED_EDGE('',*,*,#19006,.T.);
#27915=ORIENTED_EDGE('',*,*,#19004,.F.);
#27916=ORIENTED_EDGE('',*,*,#19003,.F.);
#27917=ORIENTED_EDGE('',*,*,#18938,.F.);
#27918=ORIENTED_EDGE('',*,*,#18932,.T.);
#27919=ORIENTED_EDGE('',*,*,#18930,.F.);
#27920=ORIENTED_EDGE('',*,*,#18928,.F.);
#27921=ORIENTED_EDGE('',*,*,#18936,.T.);
#27922=ORIENTED_EDGE('',*,*,#19180,.F.);
#27923=ORIENTED_EDGE('',*,*,#19151,.T.);
#27924=ORIENTED_EDGE('',*,*,#19153,.F.);
#27925=ORIENTED_EDGE('',*,*,#18944,.T.);
#27926=ORIENTED_EDGE('',*,*,#19186,.F.);
#27927=ORIENTED_EDGE('',*,*,#19187,.T.);
#27928=ORIENTED_EDGE('',*,*,#18927,.T.);
#27929=ORIENTED_EDGE('',*,*,#19187,.F.);
#27930=ORIENTED_EDGE('',*,*,#19188,.F.);
#27931=ORIENTED_EDGE('',*,*,#19189,.T.);
#27932=ORIENTED_EDGE('',*,*,#19186,.T.);
#27933=ORIENTED_EDGE('',*,*,#19189,.F.);
#27934=ORIENTED_EDGE('',*,*,#19190,.F.);
#27935=ORIENTED_EDGE('',*,*,#19188,.T.);
#27936=ORIENTED_EDGE('',*,*,#18974,.F.);
#27937=ORIENTED_EDGE('',*,*,#19191,.T.);
#27938=ORIENTED_EDGE('',*,*,#19190,.T.);
#27939=ORIENTED_EDGE('',*,*,#19191,.F.);
#27940=ORIENTED_EDGE('',*,*,#18925,.F.);
#27941=ORIENTED_EDGE('',*,*,#19192,.F.);
#27942=ORIENTED_EDGE('',*,*,#19193,.T.);
#27943=ORIENTED_EDGE('',*,*,#19194,.T.);
#27944=ORIENTED_EDGE('',*,*,#19195,.T.);
#27945=ORIENTED_EDGE('',*,*,#19196,.F.);
#27946=ORIENTED_EDGE('',*,*,#19197,.T.);
#27947=ORIENTED_EDGE('',*,*,#19192,.T.);
#27948=ORIENTED_EDGE('',*,*,#19198,.T.);
#27949=ORIENTED_EDGE('',*,*,#19199,.F.);
#27950=ORIENTED_EDGE('',*,*,#19200,.T.);
#27951=ORIENTED_EDGE('',*,*,#19196,.T.);
#27952=ORIENTED_EDGE('',*,*,#19201,.T.);
#27953=ORIENTED_EDGE('',*,*,#19202,.F.);
#27954=ORIENTED_EDGE('',*,*,#19203,.T.);
#27955=ORIENTED_EDGE('',*,*,#19199,.T.);
#27956=ORIENTED_EDGE('',*,*,#19204,.T.);
#27957=ORIENTED_EDGE('',*,*,#19205,.F.);
#27958=ORIENTED_EDGE('',*,*,#19206,.T.);
#27959=ORIENTED_EDGE('',*,*,#19202,.T.);
#27960=ORIENTED_EDGE('',*,*,#19207,.T.);
#27961=ORIENTED_EDGE('',*,*,#19208,.F.);
#27962=ORIENTED_EDGE('',*,*,#19209,.T.);
#27963=ORIENTED_EDGE('',*,*,#19205,.T.);
#27964=ORIENTED_EDGE('',*,*,#19210,.T.);
#27965=ORIENTED_EDGE('',*,*,#19211,.F.);
#27966=ORIENTED_EDGE('',*,*,#19212,.T.);
#27967=ORIENTED_EDGE('',*,*,#19208,.T.);
#27968=ORIENTED_EDGE('',*,*,#19213,.T.);
#27969=ORIENTED_EDGE('',*,*,#19214,.F.);
#27970=ORIENTED_EDGE('',*,*,#19215,.T.);
#27971=ORIENTED_EDGE('',*,*,#19216,.F.);
#27972=ORIENTED_EDGE('',*,*,#19217,.F.);
#27973=ORIENTED_EDGE('',*,*,#19218,.F.);
#27974=ORIENTED_EDGE('',*,*,#19219,.T.);
#27975=ORIENTED_EDGE('',*,*,#19214,.T.);
#27976=ORIENTED_EDGE('',*,*,#19220,.F.);
#27977=ORIENTED_EDGE('',*,*,#19221,.F.);
#27978=ORIENTED_EDGE('',*,*,#19222,.T.);
#27979=ORIENTED_EDGE('',*,*,#19218,.T.);
#27980=ORIENTED_EDGE('',*,*,#19223,.F.);
#27981=ORIENTED_EDGE('',*,*,#19224,.F.);
#27982=ORIENTED_EDGE('',*,*,#19225,.T.);
#27983=ORIENTED_EDGE('',*,*,#19221,.T.);
#27984=ORIENTED_EDGE('',*,*,#19226,.F.);
#27985=ORIENTED_EDGE('',*,*,#19227,.F.);
#27986=ORIENTED_EDGE('',*,*,#19228,.T.);
#27987=ORIENTED_EDGE('',*,*,#19224,.T.);
#27988=ORIENTED_EDGE('',*,*,#19229,.F.);
#27989=ORIENTED_EDGE('',*,*,#19230,.F.);
#27990=ORIENTED_EDGE('',*,*,#19231,.T.);
#27991=ORIENTED_EDGE('',*,*,#19227,.T.);
#27992=ORIENTED_EDGE('',*,*,#19232,.F.);
#27993=ORIENTED_EDGE('',*,*,#19216,.T.);
#27994=ORIENTED_EDGE('',*,*,#19233,.T.);
#27995=ORIENTED_EDGE('',*,*,#19234,.F.);
#27996=ORIENTED_EDGE('',*,*,#19235,.F.);
#27997=ORIENTED_EDGE('',*,*,#19236,.T.);
#27998=ORIENTED_EDGE('',*,*,#19236,.F.);
#27999=ORIENTED_EDGE('',*,*,#19237,.F.);
#28000=ORIENTED_EDGE('',*,*,#19213,.F.);
#28001=ORIENTED_EDGE('',*,*,#19210,.F.);
#28002=ORIENTED_EDGE('',*,*,#19207,.F.);
#28003=ORIENTED_EDGE('',*,*,#19204,.F.);
#28004=ORIENTED_EDGE('',*,*,#19201,.F.);
#28005=ORIENTED_EDGE('',*,*,#19198,.F.);
#28006=ORIENTED_EDGE('',*,*,#19195,.F.);
#28007=ORIENTED_EDGE('',*,*,#19238,.F.);
#28008=ORIENTED_EDGE('',*,*,#19239,.T.);
#28009=ORIENTED_EDGE('',*,*,#19232,.T.);
#28010=ORIENTED_EDGE('',*,*,#19229,.T.);
#28011=ORIENTED_EDGE('',*,*,#19226,.T.);
#28012=ORIENTED_EDGE('',*,*,#19223,.T.);
#28013=ORIENTED_EDGE('',*,*,#19220,.T.);
#28014=ORIENTED_EDGE('',*,*,#19217,.T.);
#28015=ORIENTED_EDGE('',*,*,#19240,.T.);
#28016=ORIENTED_EDGE('',*,*,#19241,.T.);
#28017=ORIENTED_EDGE('',*,*,#19242,.T.);
#28018=ORIENTED_EDGE('',*,*,#19243,.T.);
#28019=ORIENTED_EDGE('',*,*,#19238,.T.);
#28020=ORIENTED_EDGE('',*,*,#19230,.T.);
#28021=ORIENTED_EDGE('',*,*,#19239,.F.);
#28022=ORIENTED_EDGE('',*,*,#19243,.F.);
#28023=ORIENTED_EDGE('',*,*,#19244,.T.);
#28024=ORIENTED_EDGE('',*,*,#19233,.F.);
#28025=ORIENTED_EDGE('',*,*,#19215,.F.);
#28026=ORIENTED_EDGE('',*,*,#19219,.F.);
#28027=ORIENTED_EDGE('',*,*,#19222,.F.);
#28028=ORIENTED_EDGE('',*,*,#19225,.F.);
#28029=ORIENTED_EDGE('',*,*,#19228,.F.);
#28030=ORIENTED_EDGE('',*,*,#19231,.F.);
#28031=ORIENTED_EDGE('',*,*,#19244,.F.);
#28032=ORIENTED_EDGE('',*,*,#19242,.F.);
#28033=ORIENTED_EDGE('',*,*,#19193,.F.);
#28034=ORIENTED_EDGE('',*,*,#19197,.F.);
#28035=ORIENTED_EDGE('',*,*,#19200,.F.);
#28036=ORIENTED_EDGE('',*,*,#19203,.F.);
#28037=ORIENTED_EDGE('',*,*,#19206,.F.);
#28038=ORIENTED_EDGE('',*,*,#19209,.F.);
#28039=ORIENTED_EDGE('',*,*,#19212,.F.);
#28040=ORIENTED_EDGE('',*,*,#19245,.F.);
#28041=ORIENTED_EDGE('',*,*,#19246,.F.);
#28042=ORIENTED_EDGE('',*,*,#19247,.T.);
#28043=ORIENTED_EDGE('',*,*,#19248,.T.);
#28044=ORIENTED_EDGE('',*,*,#19249,.F.);
#28045=ORIENTED_EDGE('',*,*,#19250,.F.);
#28046=ORIENTED_EDGE('',*,*,#19251,.T.);
#28047=ORIENTED_EDGE('',*,*,#19252,.T.);
#28048=ORIENTED_EDGE('',*,*,#19247,.F.);
#28049=ORIENTED_EDGE('',*,*,#19253,.F.);
#28050=ORIENTED_EDGE('',*,*,#19254,.T.);
#28051=ORIENTED_EDGE('',*,*,#19255,.T.);
#28052=ORIENTED_EDGE('',*,*,#19251,.F.);
#28053=ORIENTED_EDGE('',*,*,#19256,.F.);
#28054=ORIENTED_EDGE('',*,*,#19257,.T.);
#28055=ORIENTED_EDGE('',*,*,#19258,.T.);
#28056=ORIENTED_EDGE('',*,*,#19254,.F.);
#28057=ORIENTED_EDGE('',*,*,#19259,.F.);
#28058=ORIENTED_EDGE('',*,*,#19260,.T.);
#28059=ORIENTED_EDGE('',*,*,#19261,.T.);
#28060=ORIENTED_EDGE('',*,*,#19257,.F.);
#28061=ORIENTED_EDGE('',*,*,#19262,.F.);
#28062=ORIENTED_EDGE('',*,*,#19249,.T.);
#28063=ORIENTED_EDGE('',*,*,#19263,.T.);
#28064=ORIENTED_EDGE('',*,*,#19260,.F.);
#28065=ORIENTED_EDGE('',*,*,#19263,.F.);
#28066=ORIENTED_EDGE('',*,*,#19248,.F.);
#28067=ORIENTED_EDGE('',*,*,#19252,.F.);
#28068=ORIENTED_EDGE('',*,*,#19255,.F.);
#28069=ORIENTED_EDGE('',*,*,#19258,.F.);
#28070=ORIENTED_EDGE('',*,*,#19261,.F.);
#28071=ORIENTED_EDGE('',*,*,#19264,.F.);
#28072=ORIENTED_EDGE('',*,*,#19240,.F.);
#28073=ORIENTED_EDGE('',*,*,#19194,.F.);
#28074=ORIENTED_EDGE('',*,*,#19241,.F.);
#28075=ORIENTED_EDGE('',*,*,#19265,.T.);
#28076=ORIENTED_EDGE('',*,*,#19264,.T.);
#28077=ORIENTED_EDGE('',*,*,#19265,.F.);
#28078=ORIENTED_EDGE('',*,*,#19211,.T.);
#28079=ORIENTED_EDGE('',*,*,#19237,.T.);
#28080=ORIENTED_EDGE('',*,*,#19266,.F.);
#28081=ORIENTED_EDGE('',*,*,#19245,.T.);
#28082=ORIENTED_EDGE('',*,*,#19267,.F.);
#28083=ORIENTED_EDGE('',*,*,#19268,.T.);
#28084=ORIENTED_EDGE('',*,*,#19234,.T.);
#28085=ORIENTED_EDGE('',*,*,#19266,.T.);
#28086=ORIENTED_EDGE('',*,*,#19235,.T.);
#28087=ORIENTED_EDGE('',*,*,#19268,.F.);
#28088=ORIENTED_EDGE('',*,*,#19267,.T.);
#28089=ORIENTED_EDGE('',*,*,#19246,.T.);
#28090=ORIENTED_EDGE('',*,*,#19262,.T.);
#28091=ORIENTED_EDGE('',*,*,#19259,.T.);
#28092=ORIENTED_EDGE('',*,*,#19256,.T.);
#28093=ORIENTED_EDGE('',*,*,#19253,.T.);
#28094=ORIENTED_EDGE('',*,*,#19250,.T.);
#28095=PLANE('',#30892);
#28096=PLANE('',#30893);
#28097=PLANE('',#30894);
#28098=PLANE('',#30895);
#28099=PLANE('',#30896);
#28100=PLANE('',#30897);
#28101=PLANE('',#30898);
#28102=PLANE('',#30899);
#28103=PLANE('',#30900);
#28104=PLANE('',#30901);
#28105=PLANE('',#30905);
#28106=PLANE('',#30918);
#28107=PLANE('',#30925);
#28108=PLANE('',#30932);
#28109=PLANE('',#30939);
#28110=PLANE('',#30941);
#28111=PLANE('',#30942);
#28112=PLANE('',#30943);
#28113=PLANE('',#30944);
#28114=PLANE('',#30945);
#28115=PLANE('',#30946);
#28116=PLANE('',#30947);
#28117=PLANE('',#30948);
#28118=PLANE('',#30949);
#28119=PLANE('',#30950);
#28120=PLANE('',#30951);
#28121=PLANE('',#30952);
#28122=PLANE('',#30953);
#28123=PLANE('',#30954);
#28124=PLANE('',#30955);
#28125=PLANE('',#30973);
#28126=PLANE('',#30974);
#28127=PLANE('',#30980);
#28128=PLANE('',#30981);
#28129=PLANE('',#30982);
#28130=PLANE('',#30983);
#28131=PLANE('',#30984);
#28132=PLANE('',#30985);
#28133=PLANE('',#30986);
#28134=PLANE('',#30987);
#28135=PLANE('',#30988);
#28136=PLANE('',#30989);
#28137=PLANE('',#30990);
#28138=PLANE('',#30991);
#28139=PLANE('',#30992);
#28140=PLANE('',#30993);
#28141=PLANE('',#30994);
#28142=PLANE('',#30995);
#28143=PLANE('',#30996);
#28144=PLANE('',#30997);
#28145=PLANE('',#30998);
#28146=PLANE('',#30999);
#28147=PLANE('',#31000);
#28148=PLANE('',#31001);
#28149=PLANE('',#31002);
#28150=PLANE('',#31003);
#28151=PLANE('',#31004);
#28152=PLANE('',#31005);
#28153=PLANE('',#31006);
#28154=PLANE('',#31007);
#28155=PLANE('',#31008);
#28156=PLANE('',#31009);
#28157=PLANE('',#31010);
#28158=PLANE('',#31011);
#28159=PLANE('',#31012);
#28160=PLANE('',#31013);
#28161=PLANE('',#31014);
#28162=PLANE('',#31015);
#28163=PLANE('',#31016);
#28164=PLANE('',#31017);
#28165=PLANE('',#31018);
#28166=PLANE('',#31019);
#28167=PLANE('',#31020);
#28168=PLANE('',#31021);
#28169=PLANE('',#31022);
#28170=PLANE('',#31023);
#28171=PLANE('',#31024);
#28172=PLANE('',#31025);
#28173=PLANE('',#31026);
#28174=PLANE('',#31027);
#28175=PLANE('',#31028);
#28176=PLANE('',#31029);
#28177=PLANE('',#31030);
#28178=PLANE('',#31031);
#28179=PLANE('',#31032);
#28180=PLANE('',#31033);
#28181=PLANE('',#31034);
#28182=PLANE('',#31035);
#28183=PLANE('',#31104);
#28184=PLANE('',#31105);
#28185=PLANE('',#31106);
#28186=PLANE('',#31107);
#28187=PLANE('',#31108);
#28188=PLANE('',#31109);
#28189=PLANE('',#31110);
#28190=PLANE('',#31111);
#28191=PLANE('',#31112);
#28192=PLANE('',#31113);
#28193=PLANE('',#31114);
#28194=PLANE('',#31115);
#28195=PLANE('',#31116);
#28196=PLANE('',#31117);
#28197=PLANE('',#31120);
#28198=PLANE('',#31121);
#28199=PLANE('',#31126);
#28200=PLANE('',#31154);
#28201=PLANE('',#31157);
#28202=PLANE('',#31160);
#28203=PLANE('',#31163);
#28204=PLANE('',#31164);
#28205=PLANE('',#31165);
#28206=PLANE('',#31169);
#28207=PLANE('',#31173);
#28208=PLANE('',#31177);
#28209=PLANE('',#31179);
#28210=PLANE('',#31181);
#28211=PLANE('',#31182);
#28212=PLANE('',#31186);
#28213=PLANE('',#31209);
#28214=PLANE('',#31212);
#28215=PLANE('',#31215);
#28216=PLANE('',#31218);
#28217=PLANE('',#31221);
#28218=PLANE('',#31224);
#28219=PLANE('',#31225);
#28220=PLANE('',#31229);
#28221=PLANE('',#31233);
#28222=PLANE('',#31237);
#28223=PLANE('',#31243);
#28224=PLANE('',#31246);
#28225=PLANE('',#31250);
#28226=PLANE('',#31253);
#28227=PLANE('',#31256);
#28228=PLANE('',#31259);
#28229=PLANE('',#31262);
#28230=PLANE('',#31265);
#28231=PLANE('',#31268);
#28232=PLANE('',#31271);
#28233=PLANE('',#31273);
#28234=PLANE('',#31275);
#28235=PLANE('',#31276);
#28236=PLANE('',#31278);
#28237=PLANE('',#31280);
#28238=PLANE('',#31282);
#28239=PLANE('',#31284);
#28240=PLANE('',#31286);
#28241=PLANE('',#31288);
#28242=PLANE('',#31290);
#28243=PLANE('',#31300);
#28244=PLANE('',#31303);
#28245=PLANE('',#31306);
#28246=PLANE('',#31307);
#28247=PLANE('',#31308);
#28248=PLANE('',#31311);
#28249=PLANE('',#31314);
#28250=PLANE('',#31317);
#28251=PLANE('',#31319);
#28252=PLANE('',#31327);
#28253=PLANE('',#31334);
#28254=PLANE('',#31341);
#28255=PLANE('',#31348);
#28256=PLANE('',#31355);
#28257=PLANE('',#31362);
#28258=PLANE('',#31369);
#28259=PLANE('',#31376);
#28260=PLANE('',#31383);
#28261=PLANE('',#31385);
#28262=PLANE('',#31386);
#28263=PLANE('',#31387);
#28264=PLANE('',#31388);
#28265=PLANE('',#31394);
#28266=PLANE('',#31401);
#28267=PLANE('',#31403);
#28268=PLANE('',#31404);
#28269=PLANE('',#31405);
#28270=PLANE('',#31406);
#28271=PLANE('',#31407);
#28272=PLANE('',#31408);
#28273=PLANE('',#31414);
#28274=PLANE('',#31421);
#28275=PLANE('',#31425);
#28276=PLANE('',#31484);
#28277=PLANE('',#31485);
#28278=PLANE('',#31486);
#28279=PLANE('',#31597);
#28280=PLANE('',#31598);
#28281=PLANE('',#31599);
#28282=PLANE('',#31709);
#28283=PLANE('',#31722);
#28284=PLANE('',#31725);
#28285=PLANE('',#31726);
#28286=PLANE('',#31727);
#28287=PLANE('',#31728);
#28288=PLANE('',#31729);
#28289=PLANE('',#31730);
#28290=PLANE('',#31731);
#28291=PLANE('',#31732);
#28292=PLANE('',#31733);
#28293=PLANE('',#31734);
#28294=PLANE('',#31737);
#28295=PLANE('',#31740);
#28296=PLANE('',#31741);
#28297=PLANE('',#31742);
#28298=PLANE('',#31743);
#28299=PLANE('',#31744);
#28300=PLANE('',#31745);
#28301=PLANE('',#31746);
#28302=PLANE('',#31747);
#28303=PLANE('',#31749);
#28304=PLANE('',#31751);
#28305=PLANE('',#31753);
#28306=PLANE('',#31760);
#28307=PLANE('',#31763);
#28308=PLANE('',#31765);
#28309=PLANE('',#31770);
#28310=PLANE('',#31774);
#28311=PLANE('',#31778);
#28312=PLANE('',#31782);
#28313=PLANE('',#31807);
#28314=PLANE('',#31810);
#28315=PLANE('',#31815);
#28316=PLANE('',#31816);
#28317=PLANE('',#31818);
#28318=PLANE('',#31819);
#28319=PLANE('',#31821);
#28320=PLANE('',#31822);
#28321=PLANE('',#31824);
#28322=PLANE('',#31825);
#28323=PLANE('',#31827);
#28324=PLANE('',#31828);
#28325=PLANE('',#31830);
#28326=PLANE('',#31831);
#28327=PLANE('',#31833);
#28328=PLANE('',#31834);
#28329=PLANE('',#31836);
#28330=PLANE('',#31837);
#28331=PLANE('',#31839);
#28332=PLANE('',#31840);
#28333=PLANE('',#31842);
#28334=PLANE('',#31843);
#28335=PLANE('',#31845);
#28336=PLANE('',#31846);
#28337=PLANE('',#31848);
#28338=PLANE('',#31849);
#28339=PLANE('',#31851);
#28340=PLANE('',#31852);
#28341=PLANE('',#31854);
#28342=PLANE('',#31855);
#28343=PLANE('',#31857);
#28344=PLANE('',#31858);
#28345=PLANE('',#31860);
#28346=PLANE('',#31861);
#28347=PLANE('',#31863);
#28348=PLANE('',#31864);
#28349=PLANE('',#31866);
#28350=PLANE('',#31867);
#28351=PLANE('',#31869);
#28352=PLANE('',#31870);
#28353=PLANE('',#31872);
#28354=PLANE('',#31873);
#28355=PLANE('',#31875);
#28356=PLANE('',#31876);
#28357=PLANE('',#31878);
#28358=PLANE('',#31879);
#28359=PLANE('',#31881);
#28360=PLANE('',#31882);
#28361=PLANE('',#31884);
#28362=PLANE('',#31885);
#28363=PLANE('',#31887);
#28364=PLANE('',#31888);
#28365=PLANE('',#31890);
#28366=PLANE('',#31891);
#28367=PLANE('',#31893);
#28368=PLANE('',#31894);
#28369=PLANE('',#31896);
#28370=PLANE('',#31897);
#28371=PLANE('',#31899);
#28372=PLANE('',#31900);
#28373=PLANE('',#31902);
#28374=PLANE('',#31903);
#28375=PLANE('',#31905);
#28376=PLANE('',#31906);
#28377=PLANE('',#31908);
#28378=PLANE('',#31909);
#28379=PLANE('',#31911);
#28380=PLANE('',#31912);
#28381=PLANE('',#31914);
#28382=PLANE('',#31915);
#28383=PLANE('',#31917);
#28384=PLANE('',#31918);
#28385=PLANE('',#31921);
#28386=PLANE('',#31922);
#28387=PLANE('',#31925);
#28388=PLANE('',#31926);
#28389=PLANE('',#31928);
#28390=PLANE('',#31929);
#28391=PLANE('',#31931);
#28392=PLANE('',#31932);
#28393=PLANE('',#31934);
#28394=PLANE('',#31935);
#28395=PLANE('',#31937);
#28396=PLANE('',#31938);
#28397=PLANE('',#31940);
#28398=PLANE('',#31941);
#28399=PLANE('',#31943);
#28400=PLANE('',#31944);
#28401=PLANE('',#31946);
#28402=PLANE('',#31947);
#28403=PLANE('',#31949);
#28404=PLANE('',#31950);
#28405=PLANE('',#31952);
#28406=PLANE('',#31953);
#28407=PLANE('',#31955);
#28408=PLANE('',#31956);
#28409=PLANE('',#31958);
#28410=PLANE('',#31959);
#28411=PLANE('',#31961);
#28412=PLANE('',#31962);
#28413=PLANE('',#31964);
#28414=PLANE('',#31965);
#28415=PLANE('',#31967);
#28416=PLANE('',#31968);
#28417=PLANE('',#31970);
#28418=PLANE('',#31971);
#28419=PLANE('',#31973);
#28420=PLANE('',#31974);
#28421=PLANE('',#31976);
#28422=PLANE('',#31977);
#28423=PLANE('',#31979);
#28424=PLANE('',#31980);
#28425=PLANE('',#31982);
#28426=PLANE('',#31983);
#28427=PLANE('',#31985);
#28428=PLANE('',#31986);
#28429=PLANE('',#31988);
#28430=PLANE('',#31989);
#28431=PLANE('',#31991);
#28432=PLANE('',#31992);
#28433=PLANE('',#31994);
#28434=PLANE('',#31995);
#28435=PLANE('',#31997);
#28436=PLANE('',#31998);
#28437=PLANE('',#32000);
#28438=PLANE('',#32001);
#28439=PLANE('',#32003);
#28440=PLANE('',#32004);
#28441=PLANE('',#32006);
#28442=PLANE('',#32007);
#28443=PLANE('',#32009);
#28444=PLANE('',#32010);
#28445=PLANE('',#32012);
#28446=PLANE('',#32013);
#28447=PLANE('',#32015);
#28448=PLANE('',#32016);
#28449=PLANE('',#32018);
#28450=PLANE('',#32019);
#28451=PLANE('',#32021);
#28452=PLANE('',#32022);
#28453=PLANE('',#32024);
#28454=PLANE('',#32025);
#28455=PLANE('',#32027);
#28456=PLANE('',#32028);
#28457=PLANE('',#32030);
#28458=PLANE('',#32031);
#28459=PLANE('',#32035);
#28460=PLANE('',#32036);
#28461=PLANE('',#32037);
#28462=PLANE('',#32038);
#28463=PLANE('',#32039);
#28464=PLANE('',#32040);
#28465=PLANE('',#32041);
#28466=PLANE('',#32049);
#28467=PLANE('',#32051);
#28468=PLANE('',#32060);
#28469=PLANE('',#32065);
#28470=PLANE('',#32070);
#28471=PLANE('',#32074);
#28472=PLANE('',#32079);
#28473=PLANE('',#32087);
#28474=PLANE('',#32091);
#28475=PLANE('',#32092);
#28476=PLANE('',#32100);
#28477=PLANE('',#32104);
#28478=PLANE('',#32194);
#28479=PLANE('',#32196);
#28480=PLANE('',#32207);
#28481=PLANE('',#32209);
#28482=PLANE('',#32210);
#28483=PLANE('',#32212);
#28484=PLANE('',#32213);
#28485=PLANE('',#32215);
#28486=PLANE('',#32216);
#28487=PLANE('',#32218);
#28488=PLANE('',#32219);
#28489=PLANE('',#32221);
#28490=PLANE('',#32222);
#28491=PLANE('',#32224);
#28492=PLANE('',#32225);
#28493=PLANE('',#32227);
#28494=PLANE('',#32228);
#28495=PLANE('',#32230);
#28496=PLANE('',#32231);
#28497=PLANE('',#32233);
#28498=PLANE('',#32234);
#28499=PLANE('',#32236);
#28500=PLANE('',#32237);
#28501=PLANE('',#32239);
#28502=PLANE('',#32240);
#28503=PLANE('',#32242);
#28504=PLANE('',#32243);
#28505=PLANE('',#32245);
#28506=PLANE('',#32246);
#28507=PLANE('',#32248);
#28508=PLANE('',#32249);
#28509=PLANE('',#32251);
#28510=PLANE('',#32252);
#28511=PLANE('',#32254);
#28512=PLANE('',#32255);
#28513=PLANE('',#32257);
#28514=PLANE('',#32258);
#28515=PLANE('',#32260);
#28516=PLANE('',#32261);
#28517=PLANE('',#32263);
#28518=PLANE('',#32264);
#28519=PLANE('',#32266);
#28520=PLANE('',#32267);
#28521=PLANE('',#32269);
#28522=PLANE('',#32270);
#28523=PLANE('',#32272);
#28524=PLANE('',#32273);
#28525=PLANE('',#32275);
#28526=PLANE('',#32276);
#28527=PLANE('',#32278);
#28528=PLANE('',#32279);
#28529=PLANE('',#32281);
#28530=PLANE('',#32282);
#28531=PLANE('',#32284);
#28532=PLANE('',#32285);
#28533=PLANE('',#32287);
#28534=PLANE('',#32288);
#28535=PLANE('',#32290);
#28536=PLANE('',#32291);
#28537=PLANE('',#32293);
#28538=PLANE('',#32294);
#28539=PLANE('',#32296);
#28540=PLANE('',#32297);
#28541=PLANE('',#32299);
#28542=PLANE('',#32300);
#28543=PLANE('',#32302);
#28544=PLANE('',#32303);
#28545=PLANE('',#32305);
#28546=PLANE('',#32306);
#28547=PLANE('',#32308);
#28548=PLANE('',#32309);
#28549=PLANE('',#32311);
#28550=PLANE('',#32312);
#28551=PLANE('',#32315);
#28552=PLANE('',#32316);
#28553=PLANE('',#32319);
#28554=PLANE('',#32320);
#28555=PLANE('',#32322);
#28556=PLANE('',#32323);
#28557=PLANE('',#32325);
#28558=PLANE('',#32326);
#28559=PLANE('',#32328);
#28560=PLANE('',#32329);
#28561=PLANE('',#32331);
#28562=PLANE('',#32332);
#28563=PLANE('',#32334);
#28564=PLANE('',#32335);
#28565=PLANE('',#32337);
#28566=PLANE('',#32338);
#28567=PLANE('',#32340);
#28568=PLANE('',#32341);
#28569=PLANE('',#32343);
#28570=PLANE('',#32344);
#28571=PLANE('',#32346);
#28572=PLANE('',#32347);
#28573=PLANE('',#32349);
#28574=PLANE('',#32350);
#28575=PLANE('',#32352);
#28576=PLANE('',#32353);
#28577=PLANE('',#32355);
#28578=PLANE('',#32356);
#28579=PLANE('',#32358);
#28580=PLANE('',#32359);
#28581=PLANE('',#32361);
#28582=PLANE('',#32362);
#28583=PLANE('',#32364);
#28584=PLANE('',#32365);
#28585=PLANE('',#32367);
#28586=PLANE('',#32368);
#28587=PLANE('',#32370);
#28588=PLANE('',#32371);
#28589=PLANE('',#32373);
#28590=PLANE('',#32374);
#28591=PLANE('',#32376);
#28592=PLANE('',#32377);
#28593=PLANE('',#32379);
#28594=PLANE('',#32380);
#28595=PLANE('',#32382);
#28596=PLANE('',#32383);
#28597=PLANE('',#32385);
#28598=PLANE('',#32386);
#28599=PLANE('',#32388);
#28600=PLANE('',#32389);
#28601=PLANE('',#32391);
#28602=PLANE('',#32392);
#28603=PLANE('',#32394);
#28604=PLANE('',#32395);
#28605=PLANE('',#32397);
#28606=PLANE('',#32398);
#28607=PLANE('',#32400);
#28608=PLANE('',#32401);
#28609=PLANE('',#32403);
#28610=PLANE('',#32404);
#28611=PLANE('',#32406);
#28612=PLANE('',#32407);
#28613=PLANE('',#32409);
#28614=PLANE('',#32410);
#28615=PLANE('',#32412);
#28616=PLANE('',#32413);
#28617=PLANE('',#32415);
#28618=PLANE('',#32416);
#28619=PLANE('',#32418);
#28620=PLANE('',#32419);
#28621=PLANE('',#32421);
#28622=PLANE('',#32422);
#28623=PLANE('',#32424);
#28624=PLANE('',#32425);
#28625=PLANE('',#32429);
#28626=PLANE('',#32430);
#28627=PLANE('',#32431);
#28628=PLANE('',#32432);
#28629=PLANE('',#32433);
#28630=PLANE('',#32434);
#28631=PLANE('',#32435);
#28632=PLANE('',#32436);
#28633=PLANE('',#32443);
#28634=PLANE('',#32445);
#28635=PLANE('',#32453);
#28636=PLANE('',#32595);
#28637=PLANE('',#32598);
#28638=PLANE('',#32608);
#28639=PLANE('',#32610);
#28640=PLANE('',#32611);
#28641=PLANE('',#32613);
#28642=PLANE('',#32614);
#28643=PLANE('',#32616);
#28644=PLANE('',#32617);
#28645=PLANE('',#32619);
#28646=PLANE('',#32620);
#28647=PLANE('',#32622);
#28648=PLANE('',#32623);
#28649=PLANE('',#32625);
#28650=PLANE('',#32626);
#28651=PLANE('',#32628);
#28652=PLANE('',#32629);
#28653=PLANE('',#32631);
#28654=PLANE('',#32632);
#28655=PLANE('',#32634);
#28656=PLANE('',#32635);
#28657=PLANE('',#32637);
#28658=PLANE('',#32638);
#28659=PLANE('',#32640);
#28660=PLANE('',#32641);
#28661=PLANE('',#32643);
#28662=PLANE('',#32644);
#28663=PLANE('',#32646);
#28664=PLANE('',#32647);
#28665=PLANE('',#32649);
#28666=PLANE('',#32650);
#28667=PLANE('',#32652);
#28668=PLANE('',#32653);
#28669=PLANE('',#32655);
#28670=PLANE('',#32656);
#28671=PLANE('',#32658);
#28672=PLANE('',#32659);
#28673=PLANE('',#32661);
#28674=PLANE('',#32662);
#28675=PLANE('',#32664);
#28676=PLANE('',#32665);
#28677=PLANE('',#32667);
#28678=PLANE('',#32668);
#28679=PLANE('',#32670);
#28680=PLANE('',#32671);
#28681=PLANE('',#32673);
#28682=PLANE('',#32674);
#28683=PLANE('',#32676);
#28684=PLANE('',#32677);
#28685=PLANE('',#32679);
#28686=PLANE('',#32680);
#28687=PLANE('',#32682);
#28688=PLANE('',#32683);
#28689=PLANE('',#32685);
#28690=PLANE('',#32686);
#28691=PLANE('',#32688);
#28692=PLANE('',#32689);
#28693=PLANE('',#32691);
#28694=PLANE('',#32692);
#28695=PLANE('',#32694);
#28696=PLANE('',#32695);
#28697=PLANE('',#32697);
#28698=PLANE('',#32698);
#28699=PLANE('',#32700);
#28700=PLANE('',#32701);
#28701=PLANE('',#32703);
#28702=PLANE('',#32704);
#28703=PLANE('',#32706);
#28704=PLANE('',#32707);
#28705=PLANE('',#32709);
#28706=PLANE('',#32710);
#28707=PLANE('',#32712);
#28708=PLANE('',#32713);
#28709=PLANE('',#32716);
#28710=PLANE('',#32717);
#28711=PLANE('',#32720);
#28712=PLANE('',#32721);
#28713=PLANE('',#32723);
#28714=PLANE('',#32724);
#28715=PLANE('',#32726);
#28716=PLANE('',#32727);
#28717=PLANE('',#32729);
#28718=PLANE('',#32730);
#28719=PLANE('',#32732);
#28720=PLANE('',#32733);
#28721=PLANE('',#32735);
#28722=PLANE('',#32736);
#28723=PLANE('',#32738);
#28724=PLANE('',#32739);
#28725=PLANE('',#32741);
#28726=PLANE('',#32742);
#28727=PLANE('',#32744);
#28728=PLANE('',#32745);
#28729=PLANE('',#32747);
#28730=PLANE('',#32748);
#28731=PLANE('',#32750);
#28732=PLANE('',#32751);
#28733=PLANE('',#32753);
#28734=PLANE('',#32754);
#28735=PLANE('',#32756);
#28736=PLANE('',#32757);
#28737=PLANE('',#32759);
#28738=PLANE('',#32760);
#28739=PLANE('',#32762);
#28740=PLANE('',#32763);
#28741=PLANE('',#32765);
#28742=PLANE('',#32766);
#28743=PLANE('',#32768);
#28744=PLANE('',#32769);
#28745=PLANE('',#32771);
#28746=PLANE('',#32772);
#28747=PLANE('',#32774);
#28748=PLANE('',#32775);
#28749=PLANE('',#32777);
#28750=PLANE('',#32778);
#28751=PLANE('',#32780);
#28752=PLANE('',#32781);
#28753=PLANE('',#32783);
#28754=PLANE('',#32784);
#28755=PLANE('',#32786);
#28756=PLANE('',#32787);
#28757=PLANE('',#32789);
#28758=PLANE('',#32790);
#28759=PLANE('',#32792);
#28760=PLANE('',#32793);
#28761=PLANE('',#32795);
#28762=PLANE('',#32796);
#28763=PLANE('',#32798);
#28764=PLANE('',#32799);
#28765=PLANE('',#32801);
#28766=PLANE('',#32802);
#28767=PLANE('',#32804);
#28768=PLANE('',#32805);
#28769=PLANE('',#32807);
#28770=PLANE('',#32808);
#28771=PLANE('',#32810);
#28772=PLANE('',#32811);
#28773=PLANE('',#32813);
#28774=PLANE('',#32814);
#28775=PLANE('',#32816);
#28776=PLANE('',#32817);
#28777=PLANE('',#32819);
#28778=PLANE('',#32820);
#28779=PLANE('',#32822);
#28780=PLANE('',#32823);
#28781=PLANE('',#32825);
#28782=PLANE('',#32826);
#28783=PLANE('',#32830);
#28784=PLANE('',#32831);
#28785=PLANE('',#32832);
#28786=PLANE('',#32833);
#28787=PLANE('',#32834);
#28788=PLANE('',#32835);
#28789=PLANE('',#32836);
#28790=PLANE('',#32837);
#28791=PLANE('',#32844);
#28792=PLANE('',#32846);
#28793=PLANE('',#32847);
#28794=PLANE('',#32848);
#28795=PLANE('',#32854);
#28796=PLANE('',#32855);
#28797=PLANE('',#32859);
#28798=PLANE('',#32860);
#28799=PLANE('',#32861);
#28800=PLANE('',#32862);
#28801=PLANE('',#32863);
#28802=PLANE('',#32869);
#28803=PLANE('',#32870);
#28804=PLANE('',#32871);
#28805=PLANE('',#32874);
#28806=PLANE('',#32875);
#28807=PLANE('',#32881);
#28808=PLANE('',#32882);
#28809=PLANE('',#32883);
#28810=PLANE('',#32884);
#28811=PLANE('',#32885);
#28812=PLANE('',#32886);
#28813=PLANE('',#32887);
#28814=PLANE('',#32890);
#28815=PLANE('',#32891);
#28816=PLANE('',#32894);
#28817=PLANE('',#32895);
#28818=PLANE('',#32898);
#28819=PLANE('',#32899);
#28820=PLANE('',#32903);
#28821=PLANE('',#32906);
#28822=PLANE('',#32950);
#28823=PLANE('',#32954);
#28824=PLANE('',#32962);
#28825=PLANE('',#32967);
#28826=PLANE('',#32968);
#28827=PLANE('',#32972);
#28828=PLANE('',#32977);
#28829=PLANE('',#33135);
#28830=PLANE('',#33138);
#28831=PLANE('',#33151);
#28832=PLANE('',#33161);
#28833=PLANE('',#33163);
#28834=PLANE('',#33167);
#28835=PLANE('',#33203);
#28836=PLANE('',#33207);
#28837=PLANE('',#33210);
#28838=PLANE('',#33214);
#28839=PLANE('',#33217);
#28840=PLANE('',#33221);
#28841=PLANE('',#33224);
#28842=PLANE('',#33228);
#28843=PLANE('',#33231);
#28844=PLANE('',#33235);
#28845=PLANE('',#33238);
#28846=PLANE('',#33242);
#28847=PLANE('',#33245);
#28848=PLANE('',#33249);
#28849=PLANE('',#33252);
#28850=PLANE('',#33256);
#28851=PLANE('',#33259);
#28852=PLANE('',#33263);
#28853=PLANE('',#33266);
#28854=PLANE('',#33270);
#28855=PLANE('',#33273);
#28856=PLANE('',#33277);
#28857=PLANE('',#33280);
#28858=PLANE('',#33284);
#28859=PLANE('',#33287);
#28860=PLANE('',#33291);
#28861=PLANE('',#33294);
#28862=PLANE('',#33298);
#28863=PLANE('',#33299);
#28864=PLANE('',#33300);
#28865=PLANE('',#33301);
#28866=PLANE('',#33302);
#28867=PLANE('',#33303);
#28868=PLANE('',#33304);
#28869=PLANE('',#33305);
#28870=PLANE('',#33306);
#28871=PLANE('',#33307);
#28872=PLANE('',#33308);
#28873=PLANE('',#33310);
#28874=PLANE('',#33311);
#28875=PLANE('',#33312);
#28876=PLANE('',#33313);
#28877=PLANE('',#33314);
#28878=PLANE('',#33315);
#28879=PLANE('',#33316);
#28880=PLANE('',#33317);
#28881=PLANE('',#33318);
#28882=PLANE('',#33319);
#28883=PLANE('',#33320);
#28884=PLANE('',#33321);
#28885=PLANE('',#33322);
#28886=PLANE('',#33323);
#28887=PLANE('',#33324);
#28888=PLANE('',#33325);
#28889=PLANE('',#33326);
#28890=PLANE('',#33327);
#28891=PLANE('',#33328);
#28892=PLANE('',#33334);
#28893=PLANE('',#33337);
#28894=PLANE('',#33354);
#28895=PLANE('',#33357);
#28896=PLANE('',#33362);
#28897=PLANE('',#33363);
#28898=PLANE('',#33364);
#28899=PLANE('',#33365);
#28900=PLANE('',#33366);
#28901=PLANE('',#33367);
#28902=PLANE('',#33368);
#28903=PLANE('',#33369);
#28904=PLANE('',#33376);
#28905=ADVANCED_FACE('',(#3577),#28095,.T.);
#28906=ADVANCED_FACE('',(#3578),#28096,.T.);
#28907=ADVANCED_FACE('',(#3579),#28097,.T.);
#28908=ADVANCED_FACE('',(#3580),#28098,.T.);
#28909=ADVANCED_FACE('',(#3581),#28099,.T.);
#28910=ADVANCED_FACE('',(#3582),#28100,.T.);
#28911=ADVANCED_FACE('',(#3583),#28101,.T.);
#28912=ADVANCED_FACE('',(#3584,#3284,#3285,#3286,#3287,#3288,#3289,#3290,
#3291),#28102,.T.);
#28913=ADVANCED_FACE('',(#3585),#28103,.T.);
#28914=ADVANCED_FACE('',(#3586),#28104,.T.);
#28915=ADVANCED_FACE('',(#3587),#1872,.F.);
#28916=ADVANCED_FACE('',(#3588,#3292,#3293),#28105,.T.);
#28917=ADVANCED_FACE('',(#3589),#433,.F.);
#28918=ADVANCED_FACE('',(#3590),#1873,.F.);
#28919=ADVANCED_FACE('',(#3591),#434,.F.);
#28920=ADVANCED_FACE('',(#3592),#1874,.F.);
#28921=ADVANCED_FACE('',(#3593),#435,.F.);
#28922=ADVANCED_FACE('',(#3594,#3294),#28106,.T.);
#28923=ADVANCED_FACE('',(#3595),#1875,.F.);
#28924=ADVANCED_FACE('',(#3596),#436,.F.);
#28925=ADVANCED_FACE('',(#3597,#3295),#28107,.T.);
#28926=ADVANCED_FACE('',(#3598),#1876,.F.);
#28927=ADVANCED_FACE('',(#3599),#437,.F.);
#28928=ADVANCED_FACE('',(#3600,#3296),#28108,.T.);
#28929=ADVANCED_FACE('',(#3601),#1877,.F.);
#28930=ADVANCED_FACE('',(#3602),#438,.F.);
#28931=ADVANCED_FACE('',(#3603,#3297),#28109,.T.);
#28932=ADVANCED_FACE('',(#3604),#28110,.T.);
#28933=ADVANCED_FACE('',(#3605),#28111,.T.);
#28934=ADVANCED_FACE('',(#3606),#28112,.T.);
#28935=ADVANCED_FACE('',(#3607),#28113,.T.);
#28936=ADVANCED_FACE('',(#3608),#28114,.T.);
#28937=ADVANCED_FACE('',(#3609),#28115,.T.);
#28938=ADVANCED_FACE('',(#3610),#28116,.T.);
#28939=ADVANCED_FACE('',(#3611),#28117,.T.);
#28940=ADVANCED_FACE('',(#3612),#28118,.T.);
#28941=ADVANCED_FACE('',(#3613),#28119,.T.);
#28942=ADVANCED_FACE('',(#3614),#28120,.T.);
#28943=ADVANCED_FACE('',(#3615),#28121,.T.);
#28944=ADVANCED_FACE('',(#3616),#28122,.T.);
#28945=ADVANCED_FACE('',(#3617),#28123,.T.);
#28946=ADVANCED_FACE('',(#3618,#3298,#3299,#3300,#3301,#3302,#3303,#3304,
#3305,#3306,#3307,#3308,#3309,#3310,#3311,#3312,#3313,#3314),#28124,.T.);
#28947=ADVANCED_FACE('',(#3619),#28125,.T.);
#28948=ADVANCED_FACE('',(#3620,#3315,#3316,#3317,#3318,#3319),#28126,.F.);
#28949=ADVANCED_FACE('',(#3621),#28127,.F.);
#28950=ADVANCED_FACE('',(#3622),#28128,.F.);
#28951=ADVANCED_FACE('',(#3623),#28129,.F.);
#28952=ADVANCED_FACE('',(#3624),#28130,.F.);
#28953=ADVANCED_FACE('',(#3625),#28131,.F.);
#28954=ADVANCED_FACE('',(#3626),#28132,.F.);
#28955=ADVANCED_FACE('',(#3627),#28133,.F.);
#28956=ADVANCED_FACE('',(#3628),#28134,.F.);
#28957=ADVANCED_FACE('',(#3629),#28135,.F.);
#28958=ADVANCED_FACE('',(#3630),#28136,.F.);
#28959=ADVANCED_FACE('',(#3631),#28137,.F.);
#28960=ADVANCED_FACE('',(#3632),#28138,.F.);
#28961=ADVANCED_FACE('',(#3633),#28139,.F.);
#28962=ADVANCED_FACE('',(#3634),#28140,.F.);
#28963=ADVANCED_FACE('',(#3635),#308,.F.);
#28964=ADVANCED_FACE('',(#3636),#309,.F.);
#28965=ADVANCED_FACE('',(#3637),#310,.F.);
#28966=ADVANCED_FACE('',(#3638),#311,.F.);
#28967=ADVANCED_FACE('',(#3639),#28141,.F.);
#28968=ADVANCED_FACE('',(#3640),#28142,.F.);
#28969=ADVANCED_FACE('',(#3641),#28143,.F.);
#28970=ADVANCED_FACE('',(#3642),#312,.F.);
#28971=ADVANCED_FACE('',(#3643),#313,.F.);
#28972=ADVANCED_FACE('',(#3644),#314,.F.);
#28973=ADVANCED_FACE('',(#3645),#315,.F.);
#28974=ADVANCED_FACE('',(#3646),#316,.F.);
#28975=ADVANCED_FACE('',(#3647),#317,.F.);
#28976=ADVANCED_FACE('',(#3648),#318,.F.);
#28977=ADVANCED_FACE('',(#3649),#28144,.F.);
#28978=ADVANCED_FACE('',(#3650),#28145,.F.);
#28979=ADVANCED_FACE('',(#3651),#28146,.F.);
#28980=ADVANCED_FACE('',(#3652),#28147,.F.);
#28981=ADVANCED_FACE('',(#3653),#28148,.T.);
#28982=ADVANCED_FACE('',(#3654),#28149,.F.);
#28983=ADVANCED_FACE('',(#3655),#28150,.F.);
#28984=ADVANCED_FACE('',(#3656),#28151,.F.);
#28985=ADVANCED_FACE('',(#3657),#28152,.F.);
#28986=ADVANCED_FACE('',(#3658),#28153,.F.);
#28987=ADVANCED_FACE('',(#3659),#28154,.F.);
#28988=ADVANCED_FACE('',(#3660),#28155,.F.);
#28989=ADVANCED_FACE('',(#3661),#28156,.F.);
#28990=ADVANCED_FACE('',(#3662),#28157,.F.);
#28991=ADVANCED_FACE('',(#3663),#28158,.F.);
#28992=ADVANCED_FACE('',(#3664),#28159,.F.);
#28993=ADVANCED_FACE('',(#3665),#28160,.F.);
#28994=ADVANCED_FACE('',(#3666),#28161,.F.);
#28995=ADVANCED_FACE('',(#3667),#319,.F.);
#28996=ADVANCED_FACE('',(#3668),#320,.F.);
#28997=ADVANCED_FACE('',(#3669),#28162,.F.);
#28998=ADVANCED_FACE('',(#3670),#321,.F.);
#28999=ADVANCED_FACE('',(#3671),#322,.F.);
#29000=ADVANCED_FACE('',(#3672),#323,.F.);
#29001=ADVANCED_FACE('',(#3673),#28163,.F.);
#29002=ADVANCED_FACE('',(#3674),#28164,.F.);
#29003=ADVANCED_FACE('',(#3675),#28165,.F.);
#29004=ADVANCED_FACE('',(#3676),#28166,.F.);
#29005=ADVANCED_FACE('',(#3677),#324,.F.);
#29006=ADVANCED_FACE('',(#3678),#28167,.T.);
#29007=ADVANCED_FACE('',(#3679),#325,.F.);
#29008=ADVANCED_FACE('',(#3680),#326,.F.);
#29009=ADVANCED_FACE('',(#3681),#327,.F.);
#29010=ADVANCED_FACE('',(#3682),#328,.F.);
#29011=ADVANCED_FACE('',(#3683),#329,.F.);
#29012=ADVANCED_FACE('',(#3684),#330,.F.);
#29013=ADVANCED_FACE('',(#3685),#331,.F.);
#29014=ADVANCED_FACE('',(#3686),#332,.F.);
#29015=ADVANCED_FACE('',(#3687),#333,.F.);
#29016=ADVANCED_FACE('',(#3688),#334,.F.);
#29017=ADVANCED_FACE('',(#3689),#335,.F.);
#29018=ADVANCED_FACE('',(#3690),#336,.F.);
#29019=ADVANCED_FACE('',(#3691),#337,.F.);
#29020=ADVANCED_FACE('',(#3692),#28168,.F.);
#29021=ADVANCED_FACE('',(#3693),#338,.F.);
#29022=ADVANCED_FACE('',(#3694),#339,.F.);
#29023=ADVANCED_FACE('',(#3695),#340,.F.);
#29024=ADVANCED_FACE('',(#3696),#341,.F.);
#29025=ADVANCED_FACE('',(#3697),#342,.F.);
#29026=ADVANCED_FACE('',(#3698),#343,.F.);
#29027=ADVANCED_FACE('',(#3699),#344,.F.);
#29028=ADVANCED_FACE('',(#3700),#345,.F.);
#29029=ADVANCED_FACE('',(#3701),#346,.F.);
#29030=ADVANCED_FACE('',(#3702),#347,.F.);
#29031=ADVANCED_FACE('',(#3703),#348,.F.);
#29032=ADVANCED_FACE('',(#3704),#349,.F.);
#29033=ADVANCED_FACE('',(#3705),#350,.F.);
#29034=ADVANCED_FACE('',(#3706),#351,.F.);
#29035=ADVANCED_FACE('',(#3707),#352,.F.);
#29036=ADVANCED_FACE('',(#3708),#353,.F.);
#29037=ADVANCED_FACE('',(#3709),#354,.F.);
#29038=ADVANCED_FACE('',(#3710),#355,.F.);
#29039=ADVANCED_FACE('',(#3711),#28169,.F.);
#29040=ADVANCED_FACE('',(#3712),#356,.F.);
#29041=ADVANCED_FACE('',(#3713),#357,.F.);
#29042=ADVANCED_FACE('',(#3714),#28170,.T.);
#29043=ADVANCED_FACE('',(#3715),#358,.F.);
#29044=ADVANCED_FACE('',(#3716),#359,.F.);
#29045=ADVANCED_FACE('',(#3717),#360,.F.);
#29046=ADVANCED_FACE('',(#3718),#361,.F.);
#29047=ADVANCED_FACE('',(#3719),#362,.F.);
#29048=ADVANCED_FACE('',(#3720),#363,.F.);
#29049=ADVANCED_FACE('',(#3721),#364,.F.);
#29050=ADVANCED_FACE('',(#3722),#365,.F.);
#29051=ADVANCED_FACE('',(#3723),#366,.F.);
#29052=ADVANCED_FACE('',(#3724),#367,.F.);
#29053=ADVANCED_FACE('',(#3725),#368,.F.);
#29054=ADVANCED_FACE('',(#3726),#28171,.F.);
#29055=ADVANCED_FACE('',(#3727),#369,.F.);
#29056=ADVANCED_FACE('',(#3728),#370,.F.);
#29057=ADVANCED_FACE('',(#3729),#371,.F.);
#29058=ADVANCED_FACE('',(#3730),#372,.F.);
#29059=ADVANCED_FACE('',(#3731),#373,.F.);
#29060=ADVANCED_FACE('',(#3732),#374,.F.);
#29061=ADVANCED_FACE('',(#3733),#375,.F.);
#29062=ADVANCED_FACE('',(#3734),#28172,.F.);
#29063=ADVANCED_FACE('',(#3735),#376,.F.);
#29064=ADVANCED_FACE('',(#3736),#377,.F.);
#29065=ADVANCED_FACE('',(#3737),#378,.F.);
#29066=ADVANCED_FACE('',(#3738),#379,.F.);
#29067=ADVANCED_FACE('',(#3739),#380,.F.);
#29068=ADVANCED_FACE('',(#3740),#381,.F.);
#29069=ADVANCED_FACE('',(#3741),#382,.F.);
#29070=ADVANCED_FACE('',(#3742),#28173,.F.);
#29071=ADVANCED_FACE('',(#3743),#383,.F.);
#29072=ADVANCED_FACE('',(#3744),#384,.F.);
#29073=ADVANCED_FACE('',(#3745),#28174,.T.);
#29074=ADVANCED_FACE('',(#3746),#28175,.F.);
#29075=ADVANCED_FACE('',(#3747),#28176,.F.);
#29076=ADVANCED_FACE('',(#3748),#28177,.F.);
#29077=ADVANCED_FACE('',(#3749),#28178,.F.);
#29078=ADVANCED_FACE('',(#3750),#28179,.F.);
#29079=ADVANCED_FACE('',(#3751),#385,.F.);
#29080=ADVANCED_FACE('',(#3752),#386,.F.);
#29081=ADVANCED_FACE('',(#3753),#387,.F.);
#29082=ADVANCED_FACE('',(#3754),#388,.F.);
#29083=ADVANCED_FACE('',(#3755),#389,.F.);
#29084=ADVANCED_FACE('',(#3756),#390,.F.);
#29085=ADVANCED_FACE('',(#3757),#391,.F.);
#29086=ADVANCED_FACE('',(#3758),#392,.F.);
#29087=ADVANCED_FACE('',(#3759),#393,.F.);
#29088=ADVANCED_FACE('',(#3760),#394,.F.);
#29089=ADVANCED_FACE('',(#3761),#395,.F.);
#29090=ADVANCED_FACE('',(#3762),#396,.F.);
#29091=ADVANCED_FACE('',(#3763),#397,.F.);
#29092=ADVANCED_FACE('',(#3764),#28180,.F.);
#29093=ADVANCED_FACE('',(#3765),#398,.F.);
#29094=ADVANCED_FACE('',(#3766),#399,.F.);
#29095=ADVANCED_FACE('',(#3767),#400,.F.);
#29096=ADVANCED_FACE('',(#3768),#401,.F.);
#29097=ADVANCED_FACE('',(#3769),#402,.F.);
#29098=ADVANCED_FACE('',(#3770),#403,.F.);
#29099=ADVANCED_FACE('',(#3771),#404,.F.);
#29100=ADVANCED_FACE('',(#3772),#405,.F.);
#29101=ADVANCED_FACE('',(#3773),#406,.F.);
#29102=ADVANCED_FACE('',(#3774),#407,.F.);
#29103=ADVANCED_FACE('',(#3775),#408,.F.);
#29104=ADVANCED_FACE('',(#3776),#409,.F.);
#29105=ADVANCED_FACE('',(#3777),#410,.F.);
#29106=ADVANCED_FACE('',(#3778),#411,.F.);
#29107=ADVANCED_FACE('',(#3779),#412,.F.);
#29108=ADVANCED_FACE('',(#3780),#413,.F.);
#29109=ADVANCED_FACE('',(#3781),#414,.F.);
#29110=ADVANCED_FACE('',(#3782),#415,.F.);
#29111=ADVANCED_FACE('',(#3783),#28181,.F.);
#29112=ADVANCED_FACE('',(#3784),#416,.F.);
#29113=ADVANCED_FACE('',(#3785),#417,.F.);
#29114=ADVANCED_FACE('',(#3786),#28182,.T.);
#29115=ADVANCED_FACE('',(#3787),#1878,.F.);
#29116=ADVANCED_FACE('',(#3788),#439,.F.);
#29117=ADVANCED_FACE('',(#3789),#1879,.F.);
#29118=ADVANCED_FACE('',(#3790),#440,.F.);
#29119=ADVANCED_FACE('',(#3791),#1880,.F.);
#29120=ADVANCED_FACE('',(#3792),#441,.F.);
#29121=ADVANCED_FACE('',(#3793),#1881,.F.);
#29122=ADVANCED_FACE('',(#3794),#442,.F.);
#29123=ADVANCED_FACE('',(#3795),#1882,.F.);
#29124=ADVANCED_FACE('',(#3796),#443,.F.);
#29125=ADVANCED_FACE('',(#3797),#1883,.F.);
#29126=ADVANCED_FACE('',(#3798),#444,.F.);
#29127=ADVANCED_FACE('',(#3799),#1884,.F.);
#29128=ADVANCED_FACE('',(#3800),#445,.F.);
#29129=ADVANCED_FACE('',(#3801),#1885,.F.);
#29130=ADVANCED_FACE('',(#3802),#446,.F.);
#29131=ADVANCED_FACE('',(#3803),#1886,.F.);
#29132=ADVANCED_FACE('',(#3804),#447,.F.);
#29133=ADVANCED_FACE('',(#3805),#1887,.F.);
#29134=ADVANCED_FACE('',(#3806),#448,.F.);
#29135=ADVANCED_FACE('',(#3807),#1888,.F.);
#29136=ADVANCED_FACE('',(#3808),#449,.F.);
#29137=ADVANCED_FACE('',(#3809),#1889,.F.);
#29138=ADVANCED_FACE('',(#3810),#450,.F.);
#29139=ADVANCED_FACE('',(#3811),#1890,.F.);
#29140=ADVANCED_FACE('',(#3812),#451,.F.);
#29141=ADVANCED_FACE('',(#3813),#1891,.F.);
#29142=ADVANCED_FACE('',(#3814),#452,.F.);
#29143=ADVANCED_FACE('',(#3815),#1892,.F.);
#29144=ADVANCED_FACE('',(#3816),#453,.F.);
#29145=ADVANCED_FACE('',(#3817),#1893,.F.);
#29146=ADVANCED_FACE('',(#3818),#454,.F.);
#29147=ADVANCED_FACE('',(#3819),#1894,.F.);
#29148=ADVANCED_FACE('',(#3820),#455,.F.);
#29149=ADVANCED_FACE('',(#3821),#1895,.F.);
#29150=ADVANCED_FACE('',(#3822),#1896,.F.);
#29151=ADVANCED_FACE('',(#3823),#1897,.F.);
#29152=ADVANCED_FACE('',(#3824),#1898,.F.);
#29153=ADVANCED_FACE('',(#3825),#28183,.F.);
#29154=ADVANCED_FACE('',(#3826),#28184,.F.);
#29155=ADVANCED_FACE('',(#3827),#28185,.T.);
#29156=ADVANCED_FACE('',(#3828),#28186,.T.);
#29157=ADVANCED_FACE('',(#3829),#28187,.T.);
#29158=ADVANCED_FACE('',(#3830),#28188,.T.);
#29159=ADVANCED_FACE('',(#3831),#28189,.T.);
#29160=ADVANCED_FACE('',(#3832),#28190,.T.);
#29161=ADVANCED_FACE('',(#3833),#28191,.T.);
#29162=ADVANCED_FACE('',(#3834),#28192,.T.);
#29163=ADVANCED_FACE('',(#3835),#28193,.T.);
#29164=ADVANCED_FACE('',(#3836),#28194,.T.);
#29165=ADVANCED_FACE('',(#3837),#28195,.T.);
#29166=ADVANCED_FACE('',(#3838),#28196,.T.);
#29167=ADVANCED_FACE('',(#3839),#456,.F.);
#29168=ADVANCED_FACE('',(#3840,#3320),#28197,.T.);
#29169=ADVANCED_FACE('',(#3841),#28198,.T.);
#29170=ADVANCED_FACE('',(#3842),#1899,.F.);
#29171=ADVANCED_FACE('',(#3843,#3321,#3322,#3323,#3324,#3325,#3326,#3327,
#3328,#3329,#3330),#28199,.T.);
#29172=ADVANCED_FACE('',(#3844),#457,.F.);
#29173=ADVANCED_FACE('',(#3845),#1900,.F.);
#29174=ADVANCED_FACE('',(#3846),#458,.F.);
#29175=ADVANCED_FACE('',(#3847),#28200,.T.);
#29176=ADVANCED_FACE('',(#3848),#1901,.T.);
#29177=ADVANCED_FACE('',(#3849),#28201,.T.);
#29178=ADVANCED_FACE('',(#3850),#1902,.F.);
#29179=ADVANCED_FACE('',(#3851),#28202,.T.);
#29180=ADVANCED_FACE('',(#3852),#1903,.F.);
#29181=ADVANCED_FACE('',(#3853),#28203,.T.);
#29182=ADVANCED_FACE('',(#3854),#28204,.T.);
#29183=ADVANCED_FACE('',(#3855),#28205,.T.);
#29184=ADVANCED_FACE('',(#3856),#1904,.T.);
#29185=ADVANCED_FACE('',(#3857),#28206,.T.);
#29186=ADVANCED_FACE('',(#3858),#1905,.F.);
#29187=ADVANCED_FACE('',(#3859),#28207,.T.);
#29188=ADVANCED_FACE('',(#3860),#1906,.F.);
#29189=ADVANCED_FACE('',(#3861),#28208,.T.);
#29190=ADVANCED_FACE('',(#3862),#459,.F.);
#29191=ADVANCED_FACE('',(#3863),#28209,.T.);
#29192=ADVANCED_FACE('',(#3864),#460,.F.);
#29193=ADVANCED_FACE('',(#3865),#28210,.T.);
#29194=ADVANCED_FACE('',(#3866),#28211,.T.);
#29195=ADVANCED_FACE('',(#3867),#1907,.F.);
#29196=ADVANCED_FACE('',(#3868,#3331,#3332,#3333,#3334),#28212,.F.);
#29197=ADVANCED_FACE('',(#3869),#461,.F.);
#29198=ADVANCED_FACE('',(#3870),#1908,.F.);
#29199=ADVANCED_FACE('',(#3871),#462,.F.);
#29200=ADVANCED_FACE('',(#3872),#1909,.F.);
#29201=ADVANCED_FACE('',(#3873),#463,.F.);
#29202=ADVANCED_FACE('',(#3874),#1910,.F.);
#29203=ADVANCED_FACE('',(#3875),#28213,.T.);
#29204=ADVANCED_FACE('',(#3876),#1911,.T.);
#29205=ADVANCED_FACE('',(#3877),#28214,.T.);
#29206=ADVANCED_FACE('',(#3878),#1912,.T.);
#29207=ADVANCED_FACE('',(#3879),#28215,.T.);
#29208=ADVANCED_FACE('',(#3880),#1913,.T.);
#29209=ADVANCED_FACE('',(#3881),#28216,.T.);
#29210=ADVANCED_FACE('',(#3882),#1914,.T.);
#29211=ADVANCED_FACE('',(#3883),#28217,.T.);
#29212=ADVANCED_FACE('',(#3884),#1915,.F.);
#29213=ADVANCED_FACE('',(#3885),#28218,.T.);
#29214=ADVANCED_FACE('',(#3886),#28219,.T.);
#29215=ADVANCED_FACE('',(#3887),#1916,.T.);
#29216=ADVANCED_FACE('',(#3888),#28220,.T.);
#29217=ADVANCED_FACE('',(#3889),#1917,.T.);
#29218=ADVANCED_FACE('',(#3890),#28221,.T.);
#29219=ADVANCED_FACE('',(#3891),#1918,.T.);
#29220=ADVANCED_FACE('',(#3892),#28222,.T.);
#29221=ADVANCED_FACE('',(#3893),#1919,.T.);
#29222=ADVANCED_FACE('',(#3894),#464,.T.);
#29223=ADVANCED_FACE('',(#3895),#28223,.T.);
#29224=ADVANCED_FACE('',(#3896),#465,.T.);
#29225=ADVANCED_FACE('',(#3897,#3335),#28224,.T.);
#29226=ADVANCED_FACE('',(#3898),#28225,.F.);
#29227=ADVANCED_FACE('',(#3899),#1920,.F.);
#29228=ADVANCED_FACE('',(#3900),#28226,.T.);
#29229=ADVANCED_FACE('',(#3901),#1921,.T.);
#29230=ADVANCED_FACE('',(#3902),#28227,.T.);
#29231=ADVANCED_FACE('',(#3903),#1922,.T.);
#29232=ADVANCED_FACE('',(#3904),#28228,.T.);
#29233=ADVANCED_FACE('',(#3905),#1923,.T.);
#29234=ADVANCED_FACE('',(#3906),#28229,.T.);
#29235=ADVANCED_FACE('',(#3907),#1924,.T.);
#29236=ADVANCED_FACE('',(#3908),#28230,.T.);
#29237=ADVANCED_FACE('',(#3909),#1925,.F.);
#29238=ADVANCED_FACE('',(#3910),#28231,.T.);
#29239=ADVANCED_FACE('',(#3911),#1926,.T.);
#29240=ADVANCED_FACE('',(#3912),#28232,.T.);
#29241=ADVANCED_FACE('',(#3913),#1927,.T.);
#29242=ADVANCED_FACE('',(#3914),#28233,.T.);
#29243=ADVANCED_FACE('',(#3915),#1928,.T.);
#29244=ADVANCED_FACE('',(#3916),#28234,.T.);
#29245=ADVANCED_FACE('',(#3917),#28235,.T.);
#29246=ADVANCED_FACE('',(#3918),#466,.T.);
#29247=ADVANCED_FACE('',(#3919),#28236,.T.);
#29248=ADVANCED_FACE('',(#3920),#467,.F.);
#29249=ADVANCED_FACE('',(#3921),#28237,.T.);
#29250=ADVANCED_FACE('',(#3922),#468,.T.);
#29251=ADVANCED_FACE('',(#3923),#28238,.T.);
#29252=ADVANCED_FACE('',(#3924),#469,.T.);
#29253=ADVANCED_FACE('',(#3925),#28239,.T.);
#29254=ADVANCED_FACE('',(#3926),#470,.T.);
#29255=ADVANCED_FACE('',(#3927),#28240,.T.);
#29256=ADVANCED_FACE('',(#3928),#471,.T.);
#29257=ADVANCED_FACE('',(#3929),#28241,.T.);
#29258=ADVANCED_FACE('',(#3930),#472,.F.);
#29259=ADVANCED_FACE('',(#3931),#28242,.T.);
#29260=ADVANCED_FACE('',(#3932),#1929,.F.);
#29261=ADVANCED_FACE('',(#3933),#1930,.F.);
#29262=ADVANCED_FACE('',(#3934),#1931,.F.);
#29263=ADVANCED_FACE('',(#3935),#1932,.F.);
#29264=ADVANCED_FACE('',(#3936),#473,.F.);
#29265=ADVANCED_FACE('',(#3937),#474,.F.);
#29266=ADVANCED_FACE('',(#3938),#475,.F.);
#29267=ADVANCED_FACE('',(#3939),#28243,.T.);
#29268=ADVANCED_FACE('',(#3940,#3336),#476,.F.);
#29269=ADVANCED_FACE('',(#3941),#28244,.T.);
#29270=ADVANCED_FACE('',(#3942),#477,.F.);
#29271=ADVANCED_FACE('',(#3943),#28245,.T.);
#29272=ADVANCED_FACE('',(#3944),#28246,.T.);
#29273=ADVANCED_FACE('',(#3945),#28247,.T.);
#29274=ADVANCED_FACE('',(#3946),#478,.F.);
#29275=ADVANCED_FACE('',(#3947),#28248,.T.);
#29276=ADVANCED_FACE('',(#3948),#479,.F.);
#29277=ADVANCED_FACE('',(#3949),#28249,.T.);
#29278=ADVANCED_FACE('',(#3950),#480,.F.);
#29279=ADVANCED_FACE('',(#3951),#28250,.T.);
#29280=ADVANCED_FACE('',(#3952),#481,.T.);
#29281=ADVANCED_FACE('',(#3953),#28251,.T.);
#29282=ADVANCED_FACE('',(#3954),#482,.T.);
#29283=ADVANCED_FACE('',(#3955),#1933,.F.);
#29284=ADVANCED_FACE('',(#3956),#483,.F.);
#29285=ADVANCED_FACE('',(#3957,#3337),#28252,.T.);
#29286=ADVANCED_FACE('',(#3958),#1934,.F.);
#29287=ADVANCED_FACE('',(#3959),#484,.F.);
#29288=ADVANCED_FACE('',(#3960,#3338),#28253,.T.);
#29289=ADVANCED_FACE('',(#3961),#1935,.F.);
#29290=ADVANCED_FACE('',(#3962),#485,.F.);
#29291=ADVANCED_FACE('',(#3963,#3339),#28254,.T.);
#29292=ADVANCED_FACE('',(#3964),#1936,.F.);
#29293=ADVANCED_FACE('',(#3965),#486,.F.);
#29294=ADVANCED_FACE('',(#3966,#3340),#28255,.T.);
#29295=ADVANCED_FACE('',(#3967),#1937,.F.);
#29296=ADVANCED_FACE('',(#3968),#487,.F.);
#29297=ADVANCED_FACE('',(#3969,#3341),#28256,.T.);
#29298=ADVANCED_FACE('',(#3970),#1938,.F.);
#29299=ADVANCED_FACE('',(#3971),#488,.F.);
#29300=ADVANCED_FACE('',(#3972,#3342),#28257,.T.);
#29301=ADVANCED_FACE('',(#3973),#1939,.F.);
#29302=ADVANCED_FACE('',(#3974),#489,.F.);
#29303=ADVANCED_FACE('',(#3975,#3343),#28258,.T.);
#29304=ADVANCED_FACE('',(#3976),#1940,.F.);
#29305=ADVANCED_FACE('',(#3977),#490,.F.);
#29306=ADVANCED_FACE('',(#3978,#3344),#28259,.T.);
#29307=ADVANCED_FACE('',(#3979),#1941,.F.);
#29308=ADVANCED_FACE('',(#3980),#491,.F.);
#29309=ADVANCED_FACE('',(#3981,#3345),#28260,.F.);
#29310=ADVANCED_FACE('',(#3982),#28261,.T.);
#29311=ADVANCED_FACE('',(#3983),#28262,.T.);
#29312=ADVANCED_FACE('',(#3984),#28263,.T.);
#29313=ADVANCED_FACE('',(#3985),#28264,.T.);
#29314=ADVANCED_FACE('',(#3986),#1942,.F.);
#29315=ADVANCED_FACE('',(#3987),#492,.F.);
#29316=ADVANCED_FACE('',(#3988,#3346),#28265,.T.);
#29317=ADVANCED_FACE('',(#3989),#1943,.F.);
#29318=ADVANCED_FACE('',(#3990),#493,.F.);
#29319=ADVANCED_FACE('',(#3991,#3347),#28266,.T.);
#29320=ADVANCED_FACE('',(#3992),#28267,.T.);
#29321=ADVANCED_FACE('',(#3993),#28268,.T.);
#29322=ADVANCED_FACE('',(#3994),#28269,.T.);
#29323=ADVANCED_FACE('',(#3995),#28270,.T.);
#29324=ADVANCED_FACE('',(#3996),#28271,.T.);
#29325=ADVANCED_FACE('',(#3997),#28272,.T.);
#29326=ADVANCED_FACE('',(#3998),#1944,.F.);
#29327=ADVANCED_FACE('',(#3999),#494,.F.);
#29328=ADVANCED_FACE('',(#4000,#3348),#28273,.T.);
#29329=ADVANCED_FACE('',(#4001),#1945,.F.);
#29330=ADVANCED_FACE('',(#4002),#495,.F.);
#29331=ADVANCED_FACE('',(#4003,#3349),#28274,.T.);
#29332=ADVANCED_FACE('',(#4004),#1946,.F.);
#29333=ADVANCED_FACE('',(#4005,#3350,#3351,#3352,#3353,#3354,#3355,#3356,
#3357,#3358,#3359,#3360,#3361,#3362,#3363,#3364,#3365,#3366,#3367,#3368,
#3369,#3370,#3371,#3372,#3373,#3374,#3375,#3376,#3377,#3378,#3379,#3380,
#3381,#3382,#3383,#3384,#3385,#3386,#3387,#3388,#3389,#3390,#3391),#28275,
 .F.);
#29334=ADVANCED_FACE('',(#4006),#1947,.F.);
#29335=ADVANCED_FACE('',(#4007),#1948,.F.);
#29336=ADVANCED_FACE('',(#4008),#1949,.F.);
#29337=ADVANCED_FACE('',(#4009),#1950,.F.);
#29338=ADVANCED_FACE('',(#4010),#1951,.F.);
#29339=ADVANCED_FACE('',(#4011),#1952,.F.);
#29340=ADVANCED_FACE('',(#4012),#1953,.F.);
#29341=ADVANCED_FACE('',(#4013),#1954,.F.);
#29342=ADVANCED_FACE('',(#4014),#496,.F.);
#29343=ADVANCED_FACE('',(#4015),#1955,.F.);
#29344=ADVANCED_FACE('',(#4016),#497,.F.);
#29345=ADVANCED_FACE('',(#4017),#1956,.F.);
#29346=ADVANCED_FACE('',(#4018),#1957,.F.);
#29347=ADVANCED_FACE('',(#4019),#28276,.T.);
#29348=ADVANCED_FACE('',(#4020),#28277,.T.);
#29349=ADVANCED_FACE('',(#4021),#28278,.T.);
#29350=ADVANCED_FACE('',(#4022),#1958,.F.);
#29351=ADVANCED_FACE('',(#4023),#498,.F.);
#29352=ADVANCED_FACE('',(#4024),#1959,.F.);
#29353=ADVANCED_FACE('',(#4025),#499,.F.);
#29354=ADVANCED_FACE('',(#4026),#1960,.F.);
#29355=ADVANCED_FACE('',(#4027),#500,.F.);
#29356=ADVANCED_FACE('',(#4028),#1961,.F.);
#29357=ADVANCED_FACE('',(#4029),#501,.F.);
#29358=ADVANCED_FACE('',(#4030),#1962,.F.);
#29359=ADVANCED_FACE('',(#4031),#502,.F.);
#29360=ADVANCED_FACE('',(#4032),#1963,.F.);
#29361=ADVANCED_FACE('',(#4033),#503,.F.);
#29362=ADVANCED_FACE('',(#4034),#1964,.F.);
#29363=ADVANCED_FACE('',(#4035),#504,.F.);
#29364=ADVANCED_FACE('',(#4036),#1965,.F.);
#29365=ADVANCED_FACE('',(#4037),#505,.F.);
#29366=ADVANCED_FACE('',(#4038),#1966,.F.);
#29367=ADVANCED_FACE('',(#4039),#506,.F.);
#29368=ADVANCED_FACE('',(#4040),#1967,.F.);
#29369=ADVANCED_FACE('',(#4041),#507,.F.);
#29370=ADVANCED_FACE('',(#4042),#1968,.F.);
#29371=ADVANCED_FACE('',(#4043),#508,.F.);
#29372=ADVANCED_FACE('',(#4044),#1969,.F.);
#29373=ADVANCED_FACE('',(#4045),#509,.F.);
#29374=ADVANCED_FACE('',(#4046),#1970,.F.);
#29375=ADVANCED_FACE('',(#4047),#1971,.F.);
#29376=ADVANCED_FACE('',(#4048),#1972,.F.);
#29377=ADVANCED_FACE('',(#4049),#510,.F.);
#29378=ADVANCED_FACE('',(#4050),#1973,.F.);
#29379=ADVANCED_FACE('',(#4051),#511,.F.);
#29380=ADVANCED_FACE('',(#4052),#1974,.F.);
#29381=ADVANCED_FACE('',(#4053),#512,.F.);
#29382=ADVANCED_FACE('',(#4054),#1975,.F.);
#29383=ADVANCED_FACE('',(#4055),#513,.F.);
#29384=ADVANCED_FACE('',(#4056),#1976,.F.);
#29385=ADVANCED_FACE('',(#4057),#514,.F.);
#29386=ADVANCED_FACE('',(#4058),#1977,.F.);
#29387=ADVANCED_FACE('',(#4059),#515,.F.);
#29388=ADVANCED_FACE('',(#4060),#1978,.F.);
#29389=ADVANCED_FACE('',(#4061),#516,.F.);
#29390=ADVANCED_FACE('',(#4062),#1979,.F.);
#29391=ADVANCED_FACE('',(#4063),#517,.F.);
#29392=ADVANCED_FACE('',(#4064),#1980,.F.);
#29393=ADVANCED_FACE('',(#4065),#518,.F.);
#29394=ADVANCED_FACE('',(#4066),#1981,.F.);
#29395=ADVANCED_FACE('',(#4067),#519,.F.);
#29396=ADVANCED_FACE('',(#4068),#1982,.F.);
#29397=ADVANCED_FACE('',(#4069),#520,.F.);
#29398=ADVANCED_FACE('',(#4070),#1983,.F.);
#29399=ADVANCED_FACE('',(#4071),#521,.F.);
#29400=ADVANCED_FACE('',(#4072),#1984,.F.);
#29401=ADVANCED_FACE('',(#4073),#522,.F.);
#29402=ADVANCED_FACE('',(#4074),#1985,.F.);
#29403=ADVANCED_FACE('',(#4075),#523,.F.);
#29404=ADVANCED_FACE('',(#4076),#1986,.F.);
#29405=ADVANCED_FACE('',(#4077),#524,.F.);
#29406=ADVANCED_FACE('',(#4078),#28279,.T.);
#29407=ADVANCED_FACE('',(#4079),#28280,.T.);
#29408=ADVANCED_FACE('',(#4080,#3392,#3393,#3394,#3395,#3396,#3397,#3398,
#3399,#3400,#3401,#3402,#3403,#3404,#3405,#3406,#3407,#3408,#3409,#3410,
#3411,#3412,#3413,#3414,#3415,#3416,#3417,#3418,#3419,#3420,#3421,#3422,
#3423,#3424,#3425,#3426,#3427,#3428,#3429,#3430,#3431,#3432,#3433),#28281,
 .T.);
#29409=ADVANCED_FACE('',(#4081),#1987,.F.);
#29410=ADVANCED_FACE('',(#4082),#1988,.F.);
#29411=ADVANCED_FACE('',(#4083),#1989,.F.);
#29412=ADVANCED_FACE('',(#4084),#1990,.F.);
#29413=ADVANCED_FACE('',(#4085),#1991,.F.);
#29414=ADVANCED_FACE('',(#4086),#1992,.F.);
#29415=ADVANCED_FACE('',(#4087),#1993,.F.);
#29416=ADVANCED_FACE('',(#4088),#1994,.F.);
#29417=ADVANCED_FACE('',(#4089),#1995,.F.);
#29418=ADVANCED_FACE('',(#4090),#525,.F.);
#29419=ADVANCED_FACE('',(#4091),#1996,.F.);
#29420=ADVANCED_FACE('',(#4092),#526,.F.);
#29421=ADVANCED_FACE('',(#4093),#1997,.F.);
#29422=ADVANCED_FACE('',(#4094),#527,.F.);
#29423=ADVANCED_FACE('',(#4095),#1998,.F.);
#29424=ADVANCED_FACE('',(#4096),#528,.F.);
#29425=ADVANCED_FACE('',(#4097),#1999,.F.);
#29426=ADVANCED_FACE('',(#4098),#529,.F.);
#29427=ADVANCED_FACE('',(#4099),#2000,.F.);
#29428=ADVANCED_FACE('',(#4100),#530,.F.);
#29429=ADVANCED_FACE('',(#4101),#2001,.F.);
#29430=ADVANCED_FACE('',(#4102),#531,.F.);
#29431=ADVANCED_FACE('',(#4103),#2002,.F.);
#29432=ADVANCED_FACE('',(#4104),#532,.F.);
#29433=ADVANCED_FACE('',(#4105),#2003,.F.);
#29434=ADVANCED_FACE('',(#4106),#533,.F.);
#29435=ADVANCED_FACE('',(#4107),#2004,.F.);
#29436=ADVANCED_FACE('',(#4108),#534,.F.);
#29437=ADVANCED_FACE('',(#4109),#2005,.F.);
#29438=ADVANCED_FACE('',(#4110),#2006,.F.);
#29439=ADVANCED_FACE('',(#4111),#2007,.F.);
#29440=ADVANCED_FACE('',(#4112),#2008,.F.);
#29441=ADVANCED_FACE('',(#4113),#2009,.F.);
#29442=ADVANCED_FACE('',(#4114),#2010,.F.);
#29443=ADVANCED_FACE('',(#4115),#2011,.F.);
#29444=ADVANCED_FACE('',(#4116),#2012,.F.);
#29445=ADVANCED_FACE('',(#4117),#2013,.F.);
#29446=ADVANCED_FACE('',(#4118),#2014,.F.);
#29447=ADVANCED_FACE('',(#4119),#2015,.F.);
#29448=ADVANCED_FACE('',(#4120),#2016,.F.);
#29449=ADVANCED_FACE('',(#4121),#2017,.F.);
#29450=ADVANCED_FACE('',(#4122),#2018,.F.);
#29451=ADVANCED_FACE('',(#4123),#2019,.F.);
#29452=ADVANCED_FACE('',(#4124),#2020,.F.);
#29453=ADVANCED_FACE('',(#4125),#2021,.F.);
#29454=ADVANCED_FACE('',(#4126),#2022,.F.);
#29455=ADVANCED_FACE('',(#4127),#2023,.F.);
#29456=ADVANCED_FACE('',(#4128),#2024,.F.);
#29457=ADVANCED_FACE('',(#4129),#2025,.F.);
#29458=ADVANCED_FACE('',(#4130),#2026,.F.);
#29459=ADVANCED_FACE('',(#4131),#2027,.F.);
#29460=ADVANCED_FACE('',(#4132),#535,.F.);
#29461=ADVANCED_FACE('',(#4133),#2028,.F.);
#29462=ADVANCED_FACE('',(#4134),#536,.F.);
#29463=ADVANCED_FACE('',(#4135),#537,.F.);
#29464=ADVANCED_FACE('',(#4136),#28282,.T.);
#29465=ADVANCED_FACE('',(#4137),#2029,.F.);
#29466=ADVANCED_FACE('',(#4138),#2030,.F.);
#29467=ADVANCED_FACE('',(#4139),#538,.F.);
#29468=ADVANCED_FACE('',(#4140),#28283,.T.);
#29469=ADVANCED_FACE('',(#4141),#539,.F.);
#29470=ADVANCED_FACE('',(#4142),#28284,.T.);
#29471=ADVANCED_FACE('',(#4143),#28285,.T.);
#29472=ADVANCED_FACE('',(#4144),#28286,.T.);
#29473=ADVANCED_FACE('',(#4145),#28287,.T.);
#29474=ADVANCED_FACE('',(#4146),#28288,.T.);
#29475=ADVANCED_FACE('',(#4147),#28289,.T.);
#29476=ADVANCED_FACE('',(#4148),#28290,.T.);
#29477=ADVANCED_FACE('',(#4149),#28291,.T.);
#29478=ADVANCED_FACE('',(#4150),#28292,.T.);
#29479=ADVANCED_FACE('',(#4151,#3434,#3435),#28293,.T.);
#29480=ADVANCED_FACE('',(#4152,#3436,#3437),#28294,.T.);
#29481=ADVANCED_FACE('',(#4153),#28295,.T.);
#29482=ADVANCED_FACE('',(#4154),#28296,.T.);
#29483=ADVANCED_FACE('',(#4155),#28297,.F.);
#29484=ADVANCED_FACE('',(#4156),#28298,.T.);
#29485=ADVANCED_FACE('',(#4157),#28299,.T.);
#29486=ADVANCED_FACE('',(#4158),#28300,.T.);
#29487=ADVANCED_FACE('',(#4159),#28301,.T.);
#29488=ADVANCED_FACE('',(#4160,#3438),#28302,.T.);
#29489=ADVANCED_FACE('',(#4161,#3439),#28303,.T.);
#29490=ADVANCED_FACE('',(#4162,#3440),#28304,.F.);
#29491=ADVANCED_FACE('',(#4163,#3441),#28305,.F.);
#29492=ADVANCED_FACE('',(#4164),#540,.F.);
#29493=ADVANCED_FACE('',(#4165),#541,.F.);
#29494=ADVANCED_FACE('',(#4166),#542,.F.);
#29495=ADVANCED_FACE('',(#4167),#543,.F.);
#29496=ADVANCED_FACE('',(#4168),#28306,.T.);
#29497=ADVANCED_FACE('',(#4169,#3442),#544,.F.);
#29498=ADVANCED_FACE('',(#4170),#28307,.F.);
#29499=ADVANCED_FACE('',(#4171),#545,.F.);
#29500=ADVANCED_FACE('',(#4172),#28308,.T.);
#29501=ADVANCED_FACE('',(#4173),#546,.T.);
#29502=ADVANCED_FACE('',(#4174),#28309,.T.);
#29503=ADVANCED_FACE('',(#4175,#3443),#157,.T.);
#29504=ADVANCED_FACE('',(#4176),#28310,.T.);
#29505=ADVANCED_FACE('',(#4177),#547,.T.);
#29506=ADVANCED_FACE('',(#4178),#28311,.T.);
#29507=ADVANCED_FACE('',(#4179,#3444),#158,.T.);
#29508=ADVANCED_FACE('',(#4180),#28312,.F.);
#29509=ADVANCED_FACE('',(#4181),#418,.T.);
#29510=ADVANCED_FACE('',(#4182),#548,.T.);
#29511=ADVANCED_FACE('',(#4183),#549,.T.);
#29512=ADVANCED_FACE('',(#4184),#550,.T.);
#29513=ADVANCED_FACE('',(#4185),#551,.T.);
#29514=ADVANCED_FACE('',(#4186),#552,.T.);
#29515=ADVANCED_FACE('',(#4187),#553,.T.);
#29516=ADVANCED_FACE('',(#4188),#554,.T.);
#29517=ADVANCED_FACE('',(#4189),#555,.T.);
#29518=ADVANCED_FACE('',(#4190),#556,.T.);
#29519=ADVANCED_FACE('',(#4191),#557,.T.);
#29520=ADVANCED_FACE('',(#4192),#558,.T.);
#29521=ADVANCED_FACE('',(#4193),#559,.T.);
#29522=ADVANCED_FACE('',(#4194),#560,.T.);
#29523=ADVANCED_FACE('',(#4195),#561,.T.);
#29524=ADVANCED_FACE('',(#4196),#562,.T.);
#29525=ADVANCED_FACE('',(#4197),#563,.T.);
#29526=ADVANCED_FACE('',(#4198),#564,.T.);
#29527=ADVANCED_FACE('',(#4199),#565,.T.);
#29528=ADVANCED_FACE('',(#4200),#566,.T.);
#29529=ADVANCED_FACE('',(#4201),#567,.T.);
#29530=ADVANCED_FACE('',(#4202),#28313,.F.);
#29531=ADVANCED_FACE('',(#4203),#419,.F.);
#29532=ADVANCED_FACE('',(#4204),#28314,.T.);
#29533=ADVANCED_FACE('',(#4205),#568,.T.);
#29534=ADVANCED_FACE('',(#4206),#420,.F.);
#29535=ADVANCED_FACE('',(#4207),#28315,.F.);
#29536=ADVANCED_FACE('',(#4208),#28316,.T.);
#29537=ADVANCED_FACE('',(#4209),#28317,.F.);
#29538=ADVANCED_FACE('',(#4210),#28318,.F.);
#29539=ADVANCED_FACE('',(#4211),#28319,.F.);
#29540=ADVANCED_FACE('',(#4212),#28320,.T.);
#29541=ADVANCED_FACE('',(#4213),#28321,.F.);
#29542=ADVANCED_FACE('',(#4214),#28322,.F.);
#29543=ADVANCED_FACE('',(#4215),#28323,.F.);
#29544=ADVANCED_FACE('',(#4216),#28324,.T.);
#29545=ADVANCED_FACE('',(#4217),#28325,.F.);
#29546=ADVANCED_FACE('',(#4218),#28326,.F.);
#29547=ADVANCED_FACE('',(#4219),#28327,.F.);
#29548=ADVANCED_FACE('',(#4220),#28328,.T.);
#29549=ADVANCED_FACE('',(#4221),#28329,.F.);
#29550=ADVANCED_FACE('',(#4222),#28330,.F.);
#29551=ADVANCED_FACE('',(#4223),#28331,.F.);
#29552=ADVANCED_FACE('',(#4224),#28332,.T.);
#29553=ADVANCED_FACE('',(#4225),#28333,.F.);
#29554=ADVANCED_FACE('',(#4226),#28334,.F.);
#29555=ADVANCED_FACE('',(#4227),#28335,.F.);
#29556=ADVANCED_FACE('',(#4228),#28336,.T.);
#29557=ADVANCED_FACE('',(#4229),#28337,.F.);
#29558=ADVANCED_FACE('',(#4230),#28338,.F.);
#29559=ADVANCED_FACE('',(#4231),#28339,.F.);
#29560=ADVANCED_FACE('',(#4232),#28340,.T.);
#29561=ADVANCED_FACE('',(#4233),#28341,.F.);
#29562=ADVANCED_FACE('',(#4234),#28342,.F.);
#29563=ADVANCED_FACE('',(#4235),#28343,.F.);
#29564=ADVANCED_FACE('',(#4236),#28344,.T.);
#29565=ADVANCED_FACE('',(#4237),#28345,.F.);
#29566=ADVANCED_FACE('',(#4238),#28346,.F.);
#29567=ADVANCED_FACE('',(#4239),#28347,.F.);
#29568=ADVANCED_FACE('',(#4240),#28348,.T.);
#29569=ADVANCED_FACE('',(#4241),#28349,.F.);
#29570=ADVANCED_FACE('',(#4242),#28350,.F.);
#29571=ADVANCED_FACE('',(#4243),#28351,.F.);
#29572=ADVANCED_FACE('',(#4244),#28352,.T.);
#29573=ADVANCED_FACE('',(#4245),#28353,.F.);
#29574=ADVANCED_FACE('',(#4246),#28354,.F.);
#29575=ADVANCED_FACE('',(#4247),#28355,.F.);
#29576=ADVANCED_FACE('',(#4248),#28356,.T.);
#29577=ADVANCED_FACE('',(#4249),#28357,.F.);
#29578=ADVANCED_FACE('',(#4250),#28358,.F.);
#29579=ADVANCED_FACE('',(#4251),#28359,.F.);
#29580=ADVANCED_FACE('',(#4252),#28360,.T.);
#29581=ADVANCED_FACE('',(#4253),#28361,.F.);
#29582=ADVANCED_FACE('',(#4254),#28362,.F.);
#29583=ADVANCED_FACE('',(#4255),#28363,.F.);
#29584=ADVANCED_FACE('',(#4256),#28364,.T.);
#29585=ADVANCED_FACE('',(#4257),#28365,.F.);
#29586=ADVANCED_FACE('',(#4258),#28366,.F.);
#29587=ADVANCED_FACE('',(#4259),#28367,.F.);
#29588=ADVANCED_FACE('',(#4260),#28368,.T.);
#29589=ADVANCED_FACE('',(#4261),#28369,.F.);
#29590=ADVANCED_FACE('',(#4262),#28370,.F.);
#29591=ADVANCED_FACE('',(#4263),#28371,.F.);
#29592=ADVANCED_FACE('',(#4264),#28372,.T.);
#29593=ADVANCED_FACE('',(#4265),#28373,.F.);
#29594=ADVANCED_FACE('',(#4266),#28374,.F.);
#29595=ADVANCED_FACE('',(#4267),#28375,.F.);
#29596=ADVANCED_FACE('',(#4268),#28376,.T.);
#29597=ADVANCED_FACE('',(#4269),#28377,.F.);
#29598=ADVANCED_FACE('',(#4270),#28378,.F.);
#29599=ADVANCED_FACE('',(#4271),#28379,.F.);
#29600=ADVANCED_FACE('',(#4272),#28380,.T.);
#29601=ADVANCED_FACE('',(#4273),#28381,.F.);
#29602=ADVANCED_FACE('',(#4274),#28382,.F.);
#29603=ADVANCED_FACE('',(#4275),#28383,.F.);
#29604=ADVANCED_FACE('',(#4276),#28384,.T.);
#29605=ADVANCED_FACE('',(#4277),#28385,.F.);
#29606=ADVANCED_FACE('',(#4278),#28386,.F.);
#29607=ADVANCED_FACE('',(#4279),#28387,.F.);
#29608=ADVANCED_FACE('',(#4280),#28388,.T.);
#29609=ADVANCED_FACE('',(#4281),#28389,.F.);
#29610=ADVANCED_FACE('',(#4282),#28390,.F.);
#29611=ADVANCED_FACE('',(#4283),#28391,.F.);
#29612=ADVANCED_FACE('',(#4284),#28392,.T.);
#29613=ADVANCED_FACE('',(#4285),#28393,.F.);
#29614=ADVANCED_FACE('',(#4286),#28394,.F.);
#29615=ADVANCED_FACE('',(#4287),#28395,.F.);
#29616=ADVANCED_FACE('',(#4288),#28396,.T.);
#29617=ADVANCED_FACE('',(#4289),#28397,.F.);
#29618=ADVANCED_FACE('',(#4290),#28398,.F.);
#29619=ADVANCED_FACE('',(#4291),#28399,.F.);
#29620=ADVANCED_FACE('',(#4292),#28400,.T.);
#29621=ADVANCED_FACE('',(#4293),#28401,.F.);
#29622=ADVANCED_FACE('',(#4294),#28402,.F.);
#29623=ADVANCED_FACE('',(#4295),#28403,.F.);
#29624=ADVANCED_FACE('',(#4296),#28404,.T.);
#29625=ADVANCED_FACE('',(#4297),#28405,.F.);
#29626=ADVANCED_FACE('',(#4298),#28406,.F.);
#29627=ADVANCED_FACE('',(#4299),#28407,.F.);
#29628=ADVANCED_FACE('',(#4300),#28408,.T.);
#29629=ADVANCED_FACE('',(#4301),#28409,.F.);
#29630=ADVANCED_FACE('',(#4302),#28410,.F.);
#29631=ADVANCED_FACE('',(#4303),#28411,.F.);
#29632=ADVANCED_FACE('',(#4304),#28412,.T.);
#29633=ADVANCED_FACE('',(#4305),#28413,.F.);
#29634=ADVANCED_FACE('',(#4306),#28414,.F.);
#29635=ADVANCED_FACE('',(#4307),#28415,.F.);
#29636=ADVANCED_FACE('',(#4308),#28416,.T.);
#29637=ADVANCED_FACE('',(#4309),#28417,.F.);
#29638=ADVANCED_FACE('',(#4310),#28418,.F.);
#29639=ADVANCED_FACE('',(#4311),#28419,.F.);
#29640=ADVANCED_FACE('',(#4312),#28420,.T.);
#29641=ADVANCED_FACE('',(#4313),#28421,.F.);
#29642=ADVANCED_FACE('',(#4314),#28422,.F.);
#29643=ADVANCED_FACE('',(#4315),#28423,.F.);
#29644=ADVANCED_FACE('',(#4316),#28424,.T.);
#29645=ADVANCED_FACE('',(#4317),#28425,.F.);
#29646=ADVANCED_FACE('',(#4318),#28426,.F.);
#29647=ADVANCED_FACE('',(#4319),#28427,.F.);
#29648=ADVANCED_FACE('',(#4320),#28428,.T.);
#29649=ADVANCED_FACE('',(#4321),#28429,.F.);
#29650=ADVANCED_FACE('',(#4322),#28430,.F.);
#29651=ADVANCED_FACE('',(#4323),#28431,.F.);
#29652=ADVANCED_FACE('',(#4324),#28432,.T.);
#29653=ADVANCED_FACE('',(#4325),#28433,.F.);
#29654=ADVANCED_FACE('',(#4326),#28434,.F.);
#29655=ADVANCED_FACE('',(#4327),#28435,.F.);
#29656=ADVANCED_FACE('',(#4328),#28436,.T.);
#29657=ADVANCED_FACE('',(#4329),#28437,.F.);
#29658=ADVANCED_FACE('',(#4330),#28438,.F.);
#29659=ADVANCED_FACE('',(#4331),#28439,.F.);
#29660=ADVANCED_FACE('',(#4332),#28440,.T.);
#29661=ADVANCED_FACE('',(#4333),#28441,.F.);
#29662=ADVANCED_FACE('',(#4334),#28442,.F.);
#29663=ADVANCED_FACE('',(#4335),#28443,.F.);
#29664=ADVANCED_FACE('',(#4336),#28444,.T.);
#29665=ADVANCED_FACE('',(#4337),#28445,.F.);
#29666=ADVANCED_FACE('',(#4338),#28446,.F.);
#29667=ADVANCED_FACE('',(#4339),#28447,.F.);
#29668=ADVANCED_FACE('',(#4340),#28448,.T.);
#29669=ADVANCED_FACE('',(#4341),#28449,.F.);
#29670=ADVANCED_FACE('',(#4342),#28450,.F.);
#29671=ADVANCED_FACE('',(#4343),#28451,.F.);
#29672=ADVANCED_FACE('',(#4344),#28452,.T.);
#29673=ADVANCED_FACE('',(#4345),#28453,.F.);
#29674=ADVANCED_FACE('',(#4346),#28454,.F.);
#29675=ADVANCED_FACE('',(#4347),#28455,.F.);
#29676=ADVANCED_FACE('',(#4348),#28456,.T.);
#29677=ADVANCED_FACE('',(#4349),#28457,.F.);
#29678=ADVANCED_FACE('',(#4350),#28458,.F.);
#29679=ADVANCED_FACE('',(#4351),#2031,.F.);
#29680=ADVANCED_FACE('',(#4352),#28459,.F.);
#29681=ADVANCED_FACE('',(#4353),#28460,.F.);
#29682=ADVANCED_FACE('',(#4354),#28461,.F.);
#29683=ADVANCED_FACE('',(#4355),#28462,.F.);
#29684=ADVANCED_FACE('',(#4356),#28463,.F.);
#29685=ADVANCED_FACE('',(#4357),#28464,.F.);
#29686=ADVANCED_FACE('',(#4358,#3445),#28465,.F.);
#29687=ADVANCED_FACE('',(#4359),#159,.F.);
#29688=ADVANCED_FACE('',(#4360),#569,.T.);
#29689=ADVANCED_FACE('',(#4361,#3446),#28466,.T.);
#29690=ADVANCED_FACE('',(#4362),#28467,.T.);
#29691=ADVANCED_FACE('',(#4363),#2032,.T.);
#29692=ADVANCED_FACE('',(#4364),#570,.T.);
#29693=ADVANCED_FACE('',(#4365),#2033,.T.);
#29694=ADVANCED_FACE('',(#4366),#571,.T.);
#29695=ADVANCED_FACE('',(#4367,#3447),#28468,.T.);
#29696=ADVANCED_FACE('',(#4368,#3448,#3449,#3450,#3451,#3452,#3453,#3454,
#3455,#3456,#3457,#3458,#3459,#3460,#3461,#3462,#3463,#3464,#3465,#3466,
#3467,#3468,#3469,#3470,#3471,#3472,#3473,#3474,#3475,#3476,#3477,#3478,
#3479,#3480,#3481,#3482),#572,.T.);
#29697=ADVANCED_FACE('',(#4369),#2034,.T.);
#29698=ADVANCED_FACE('',(#4370,#3483),#28469,.T.);
#29699=ADVANCED_FACE('',(#4371),#573,.F.);
#29700=ADVANCED_FACE('',(#4372,#3484),#28470,.T.);
#29701=ADVANCED_FACE('',(#4373),#574,.T.);
#29702=ADVANCED_FACE('',(#4374,#3485),#28471,.T.);
#29703=ADVANCED_FACE('',(#4375),#155,.T.);
#29704=ADVANCED_FACE('',(#4376),#28472,.T.);
#29705=ADVANCED_FACE('',(#4377),#2035,.T.);
#29706=ADVANCED_FACE('',(#4378),#575,.T.);
#29707=ADVANCED_FACE('',(#4379),#2036,.T.);
#29708=ADVANCED_FACE('',(#4380),#28473,.T.);
#29709=ADVANCED_FACE('',(#4381),#421,.T.);
#29710=ADVANCED_FACE('',(#4382),#28474,.T.);
#29711=ADVANCED_FACE('',(#4383),#28475,.F.);
#29712=ADVANCED_FACE('',(#4384),#2037,.T.);
#29713=ADVANCED_FACE('',(#4385),#576,.T.);
#29714=ADVANCED_FACE('',(#4386,#3486),#28476,.T.);
#29715=ADVANCED_FACE('',(#4387),#577,.F.);
#29716=ADVANCED_FACE('',(#4388,#3487),#28477,.T.);
#29717=ADVANCED_FACE('',(#4389),#2038,.T.);
#29718=ADVANCED_FACE('',(#4390),#578,.T.);
#29719=ADVANCED_FACE('',(#4391),#579,.T.);
#29720=ADVANCED_FACE('',(#4392),#580,.T.);
#29721=ADVANCED_FACE('',(#4393),#581,.T.);
#29722=ADVANCED_FACE('',(#4394),#582,.T.);
#29723=ADVANCED_FACE('',(#4395),#583,.T.);
#29724=ADVANCED_FACE('',(#4396),#584,.T.);
#29725=ADVANCED_FACE('',(#4397),#585,.T.);
#29726=ADVANCED_FACE('',(#4398),#586,.T.);
#29727=ADVANCED_FACE('',(#4399),#587,.T.);
#29728=ADVANCED_FACE('',(#4400),#588,.T.);
#29729=ADVANCED_FACE('',(#4401),#589,.T.);
#29730=ADVANCED_FACE('',(#4402),#590,.T.);
#29731=ADVANCED_FACE('',(#4403),#591,.T.);
#29732=ADVANCED_FACE('',(#4404),#592,.T.);
#29733=ADVANCED_FACE('',(#4405),#593,.T.);
#29734=ADVANCED_FACE('',(#4406),#594,.T.);
#29735=ADVANCED_FACE('',(#4407),#595,.T.);
#29736=ADVANCED_FACE('',(#4408),#596,.T.);
#29737=ADVANCED_FACE('',(#4409),#597,.T.);
#29738=ADVANCED_FACE('',(#4410),#598,.T.);
#29739=ADVANCED_FACE('',(#4411),#599,.T.);
#29740=ADVANCED_FACE('',(#4412),#600,.T.);
#29741=ADVANCED_FACE('',(#4413),#601,.T.);
#29742=ADVANCED_FACE('',(#4414),#602,.T.);
#29743=ADVANCED_FACE('',(#4415),#603,.T.);
#29744=ADVANCED_FACE('',(#4416),#604,.T.);
#29745=ADVANCED_FACE('',(#4417),#605,.T.);
#29746=ADVANCED_FACE('',(#4418),#606,.T.);
#29747=ADVANCED_FACE('',(#4419),#607,.T.);
#29748=ADVANCED_FACE('',(#4420),#608,.T.);
#29749=ADVANCED_FACE('',(#4421),#609,.T.);
#29750=ADVANCED_FACE('',(#4422),#610,.T.);
#29751=ADVANCED_FACE('',(#4423),#611,.T.);
#29752=ADVANCED_FACE('',(#4424),#612,.T.);
#29753=ADVANCED_FACE('',(#4425),#613,.T.);
#29754=ADVANCED_FACE('',(#4426),#614,.T.);
#29755=ADVANCED_FACE('',(#4427),#615,.T.);
#29756=ADVANCED_FACE('',(#4428),#616,.T.);
#29757=ADVANCED_FACE('',(#4429),#617,.T.);
#29758=ADVANCED_FACE('',(#4430),#618,.T.);
#29759=ADVANCED_FACE('',(#4431),#619,.T.);
#29760=ADVANCED_FACE('',(#4432),#620,.T.);
#29761=ADVANCED_FACE('',(#4433),#621,.T.);
#29762=ADVANCED_FACE('',(#4434),#622,.T.);
#29763=ADVANCED_FACE('',(#4435),#623,.T.);
#29764=ADVANCED_FACE('',(#4436),#624,.T.);
#29765=ADVANCED_FACE('',(#4437),#625,.T.);
#29766=ADVANCED_FACE('',(#4438),#626,.T.);
#29767=ADVANCED_FACE('',(#4439),#627,.T.);
#29768=ADVANCED_FACE('',(#4440),#628,.T.);
#29769=ADVANCED_FACE('',(#4441),#629,.T.);
#29770=ADVANCED_FACE('',(#4442),#630,.T.);
#29771=ADVANCED_FACE('',(#4443),#631,.T.);
#29772=ADVANCED_FACE('',(#4444),#632,.T.);
#29773=ADVANCED_FACE('',(#4445),#633,.T.);
#29774=ADVANCED_FACE('',(#4446),#634,.T.);
#29775=ADVANCED_FACE('',(#4447),#635,.T.);
#29776=ADVANCED_FACE('',(#4448),#636,.T.);
#29777=ADVANCED_FACE('',(#4449),#637,.T.);
#29778=ADVANCED_FACE('',(#4450),#638,.T.);
#29779=ADVANCED_FACE('',(#4451),#639,.T.);
#29780=ADVANCED_FACE('',(#4452),#640,.T.);
#29781=ADVANCED_FACE('',(#4453),#641,.T.);
#29782=ADVANCED_FACE('',(#4454),#642,.T.);
#29783=ADVANCED_FACE('',(#4455),#643,.T.);
#29784=ADVANCED_FACE('',(#4456),#644,.T.);
#29785=ADVANCED_FACE('',(#4457),#645,.T.);
#29786=ADVANCED_FACE('',(#4458),#646,.T.);
#29787=ADVANCED_FACE('',(#4459),#647,.T.);
#29788=ADVANCED_FACE('',(#4460),#648,.T.);
#29789=ADVANCED_FACE('',(#4461),#649,.T.);
#29790=ADVANCED_FACE('',(#4462),#650,.T.);
#29791=ADVANCED_FACE('',(#4463),#651,.T.);
#29792=ADVANCED_FACE('',(#4464),#652,.T.);
#29793=ADVANCED_FACE('',(#4465),#653,.T.);
#29794=ADVANCED_FACE('',(#4466),#654,.T.);
#29795=ADVANCED_FACE('',(#4467),#655,.T.);
#29796=ADVANCED_FACE('',(#4468),#656,.T.);
#29797=ADVANCED_FACE('',(#4469),#657,.T.);
#29798=ADVANCED_FACE('',(#4470),#658,.T.);
#29799=ADVANCED_FACE('',(#4471),#659,.T.);
#29800=ADVANCED_FACE('',(#4472),#660,.T.);
#29801=ADVANCED_FACE('',(#4473),#661,.T.);
#29802=ADVANCED_FACE('',(#4474),#28478,.F.);
#29803=ADVANCED_FACE('',(#4475),#422,.F.);
#29804=ADVANCED_FACE('',(#4476),#28479,.T.);
#29805=ADVANCED_FACE('',(#4477),#662,.T.);
#29806=ADVANCED_FACE('',(#4478),#423,.F.);
#29807=ADVANCED_FACE('',(#4479),#160,.F.);
#29808=ADVANCED_FACE('',(#4480),#663,.T.);
#29809=ADVANCED_FACE('',(#4481,#3488),#28480,.T.);
#29810=ADVANCED_FACE('',(#4482),#28481,.F.);
#29811=ADVANCED_FACE('',(#4483),#28482,.T.);
#29812=ADVANCED_FACE('',(#4484),#28483,.F.);
#29813=ADVANCED_FACE('',(#4485),#28484,.F.);
#29814=ADVANCED_FACE('',(#4486),#28485,.F.);
#29815=ADVANCED_FACE('',(#4487),#28486,.T.);
#29816=ADVANCED_FACE('',(#4488),#28487,.F.);
#29817=ADVANCED_FACE('',(#4489),#28488,.F.);
#29818=ADVANCED_FACE('',(#4490),#28489,.F.);
#29819=ADVANCED_FACE('',(#4491),#28490,.T.);
#29820=ADVANCED_FACE('',(#4492),#28491,.F.);
#29821=ADVANCED_FACE('',(#4493),#28492,.F.);
#29822=ADVANCED_FACE('',(#4494),#28493,.F.);
#29823=ADVANCED_FACE('',(#4495),#28494,.T.);
#29824=ADVANCED_FACE('',(#4496),#28495,.F.);
#29825=ADVANCED_FACE('',(#4497),#28496,.F.);
#29826=ADVANCED_FACE('',(#4498),#28497,.F.);
#29827=ADVANCED_FACE('',(#4499),#28498,.T.);
#29828=ADVANCED_FACE('',(#4500),#28499,.F.);
#29829=ADVANCED_FACE('',(#4501),#28500,.F.);
#29830=ADVANCED_FACE('',(#4502),#28501,.F.);
#29831=ADVANCED_FACE('',(#4503),#28502,.T.);
#29832=ADVANCED_FACE('',(#4504),#28503,.F.);
#29833=ADVANCED_FACE('',(#4505),#28504,.F.);
#29834=ADVANCED_FACE('',(#4506),#28505,.F.);
#29835=ADVANCED_FACE('',(#4507),#28506,.T.);
#29836=ADVANCED_FACE('',(#4508),#28507,.F.);
#29837=ADVANCED_FACE('',(#4509),#28508,.F.);
#29838=ADVANCED_FACE('',(#4510),#28509,.F.);
#29839=ADVANCED_FACE('',(#4511),#28510,.T.);
#29840=ADVANCED_FACE('',(#4512),#28511,.F.);
#29841=ADVANCED_FACE('',(#4513),#28512,.F.);
#29842=ADVANCED_FACE('',(#4514),#28513,.F.);
#29843=ADVANCED_FACE('',(#4515),#28514,.T.);
#29844=ADVANCED_FACE('',(#4516),#28515,.F.);
#29845=ADVANCED_FACE('',(#4517),#28516,.F.);
#29846=ADVANCED_FACE('',(#4518),#28517,.F.);
#29847=ADVANCED_FACE('',(#4519),#28518,.T.);
#29848=ADVANCED_FACE('',(#4520),#28519,.F.);
#29849=ADVANCED_FACE('',(#4521),#28520,.F.);
#29850=ADVANCED_FACE('',(#4522),#28521,.F.);
#29851=ADVANCED_FACE('',(#4523),#28522,.T.);
#29852=ADVANCED_FACE('',(#4524),#28523,.F.);
#29853=ADVANCED_FACE('',(#4525),#28524,.F.);
#29854=ADVANCED_FACE('',(#4526),#28525,.F.);
#29855=ADVANCED_FACE('',(#4527),#28526,.T.);
#29856=ADVANCED_FACE('',(#4528),#28527,.F.);
#29857=ADVANCED_FACE('',(#4529),#28528,.F.);
#29858=ADVANCED_FACE('',(#4530),#28529,.F.);
#29859=ADVANCED_FACE('',(#4531),#28530,.T.);
#29860=ADVANCED_FACE('',(#4532),#28531,.F.);
#29861=ADVANCED_FACE('',(#4533),#28532,.F.);
#29862=ADVANCED_FACE('',(#4534),#28533,.F.);
#29863=ADVANCED_FACE('',(#4535),#28534,.T.);
#29864=ADVANCED_FACE('',(#4536),#28535,.F.);
#29865=ADVANCED_FACE('',(#4537),#28536,.F.);
#29866=ADVANCED_FACE('',(#4538),#28537,.F.);
#29867=ADVANCED_FACE('',(#4539),#28538,.T.);
#29868=ADVANCED_FACE('',(#4540),#28539,.F.);
#29869=ADVANCED_FACE('',(#4541),#28540,.F.);
#29870=ADVANCED_FACE('',(#4542),#28541,.F.);
#29871=ADVANCED_FACE('',(#4543),#28542,.T.);
#29872=ADVANCED_FACE('',(#4544),#28543,.F.);
#29873=ADVANCED_FACE('',(#4545),#28544,.F.);
#29874=ADVANCED_FACE('',(#4546),#28545,.F.);
#29875=ADVANCED_FACE('',(#4547),#28546,.T.);
#29876=ADVANCED_FACE('',(#4548),#28547,.F.);
#29877=ADVANCED_FACE('',(#4549),#28548,.F.);
#29878=ADVANCED_FACE('',(#4550),#28549,.F.);
#29879=ADVANCED_FACE('',(#4551),#28550,.T.);
#29880=ADVANCED_FACE('',(#4552),#28551,.F.);
#29881=ADVANCED_FACE('',(#4553),#28552,.F.);
#29882=ADVANCED_FACE('',(#4554),#28553,.F.);
#29883=ADVANCED_FACE('',(#4555),#28554,.T.);
#29884=ADVANCED_FACE('',(#4556),#28555,.F.);
#29885=ADVANCED_FACE('',(#4557),#28556,.F.);
#29886=ADVANCED_FACE('',(#4558),#28557,.F.);
#29887=ADVANCED_FACE('',(#4559),#28558,.T.);
#29888=ADVANCED_FACE('',(#4560),#28559,.F.);
#29889=ADVANCED_FACE('',(#4561),#28560,.F.);
#29890=ADVANCED_FACE('',(#4562),#28561,.F.);
#29891=ADVANCED_FACE('',(#4563),#28562,.T.);
#29892=ADVANCED_FACE('',(#4564),#28563,.F.);
#29893=ADVANCED_FACE('',(#4565),#28564,.F.);
#29894=ADVANCED_FACE('',(#4566),#28565,.F.);
#29895=ADVANCED_FACE('',(#4567),#28566,.T.);
#29896=ADVANCED_FACE('',(#4568),#28567,.F.);
#29897=ADVANCED_FACE('',(#4569),#28568,.F.);
#29898=ADVANCED_FACE('',(#4570),#28569,.F.);
#29899=ADVANCED_FACE('',(#4571),#28570,.T.);
#29900=ADVANCED_FACE('',(#4572),#28571,.F.);
#29901=ADVANCED_FACE('',(#4573),#28572,.F.);
#29902=ADVANCED_FACE('',(#4574),#28573,.F.);
#29903=ADVANCED_FACE('',(#4575),#28574,.T.);
#29904=ADVANCED_FACE('',(#4576),#28575,.F.);
#29905=ADVANCED_FACE('',(#4577),#28576,.F.);
#29906=ADVANCED_FACE('',(#4578),#28577,.F.);
#29907=ADVANCED_FACE('',(#4579),#28578,.T.);
#29908=ADVANCED_FACE('',(#4580),#28579,.F.);
#29909=ADVANCED_FACE('',(#4581),#28580,.F.);
#29910=ADVANCED_FACE('',(#4582),#28581,.F.);
#29911=ADVANCED_FACE('',(#4583),#28582,.T.);
#29912=ADVANCED_FACE('',(#4584),#28583,.F.);
#29913=ADVANCED_FACE('',(#4585),#28584,.F.);
#29914=ADVANCED_FACE('',(#4586),#28585,.F.);
#29915=ADVANCED_FACE('',(#4587),#28586,.T.);
#29916=ADVANCED_FACE('',(#4588),#28587,.F.);
#29917=ADVANCED_FACE('',(#4589),#28588,.F.);
#29918=ADVANCED_FACE('',(#4590),#28589,.F.);
#29919=ADVANCED_FACE('',(#4591),#28590,.T.);
#29920=ADVANCED_FACE('',(#4592),#28591,.F.);
#29921=ADVANCED_FACE('',(#4593),#28592,.F.);
#29922=ADVANCED_FACE('',(#4594),#28593,.F.);
#29923=ADVANCED_FACE('',(#4595),#28594,.T.);
#29924=ADVANCED_FACE('',(#4596),#28595,.F.);
#29925=ADVANCED_FACE('',(#4597),#28596,.F.);
#29926=ADVANCED_FACE('',(#4598),#28597,.F.);
#29927=ADVANCED_FACE('',(#4599),#28598,.T.);
#29928=ADVANCED_FACE('',(#4600),#28599,.F.);
#29929=ADVANCED_FACE('',(#4601),#28600,.F.);
#29930=ADVANCED_FACE('',(#4602),#28601,.F.);
#29931=ADVANCED_FACE('',(#4603),#28602,.T.);
#29932=ADVANCED_FACE('',(#4604),#28603,.F.);
#29933=ADVANCED_FACE('',(#4605),#28604,.F.);
#29934=ADVANCED_FACE('',(#4606),#28605,.F.);
#29935=ADVANCED_FACE('',(#4607),#28606,.T.);
#29936=ADVANCED_FACE('',(#4608),#28607,.F.);
#29937=ADVANCED_FACE('',(#4609),#28608,.F.);
#29938=ADVANCED_FACE('',(#4610),#28609,.F.);
#29939=ADVANCED_FACE('',(#4611),#28610,.T.);
#29940=ADVANCED_FACE('',(#4612),#28611,.F.);
#29941=ADVANCED_FACE('',(#4613),#28612,.F.);
#29942=ADVANCED_FACE('',(#4614),#28613,.F.);
#29943=ADVANCED_FACE('',(#4615),#28614,.T.);
#29944=ADVANCED_FACE('',(#4616),#28615,.F.);
#29945=ADVANCED_FACE('',(#4617),#28616,.F.);
#29946=ADVANCED_FACE('',(#4618),#28617,.F.);
#29947=ADVANCED_FACE('',(#4619),#28618,.T.);
#29948=ADVANCED_FACE('',(#4620),#28619,.F.);
#29949=ADVANCED_FACE('',(#4621),#28620,.F.);
#29950=ADVANCED_FACE('',(#4622),#28621,.F.);
#29951=ADVANCED_FACE('',(#4623),#28622,.T.);
#29952=ADVANCED_FACE('',(#4624),#28623,.F.);
#29953=ADVANCED_FACE('',(#4625),#28624,.F.);
#29954=ADVANCED_FACE('',(#4626),#2039,.F.);
#29955=ADVANCED_FACE('',(#4627),#28625,.F.);
#29956=ADVANCED_FACE('',(#4628),#28626,.F.);
#29957=ADVANCED_FACE('',(#4629),#28627,.F.);
#29958=ADVANCED_FACE('',(#4630),#28628,.F.);
#29959=ADVANCED_FACE('',(#4631),#28629,.F.);
#29960=ADVANCED_FACE('',(#4632),#28630,.F.);
#29961=ADVANCED_FACE('',(#4633,#3489),#28631,.F.);
#29962=ADVANCED_FACE('',(#4634),#28632,.T.);
#29963=ADVANCED_FACE('',(#4635),#2040,.T.);
#29964=ADVANCED_FACE('',(#4636,#3490,#3491,#3492,#3493,#3494,#3495,#3496,
#3497,#3498,#3499,#3500,#3501,#3502,#3503,#3504,#3505,#3506,#3507,#3508,
#3509,#3510,#3511,#3512,#3513,#3514,#3515,#3516,#3517,#3518,#3519,#3520,
#3521,#3522,#3523,#3524),#664,.T.);
#29965=ADVANCED_FACE('',(#4637),#2041,.T.);
#29966=ADVANCED_FACE('',(#4638,#3525),#28633,.T.);
#29967=ADVANCED_FACE('',(#4639),#28634,.T.);
#29968=ADVANCED_FACE('',(#4640),#2042,.T.);
#29969=ADVANCED_FACE('',(#4641),#665,.T.);
#29970=ADVANCED_FACE('',(#4642),#2043,.T.);
#29971=ADVANCED_FACE('',(#4643),#28635,.T.);
#29972=ADVANCED_FACE('',(#4644),#666,.T.);
#29973=ADVANCED_FACE('',(#4645),#667,.T.);
#29974=ADVANCED_FACE('',(#4646),#668,.T.);
#29975=ADVANCED_FACE('',(#4647),#669,.T.);
#29976=ADVANCED_FACE('',(#4648),#670,.T.);
#29977=ADVANCED_FACE('',(#4649),#671,.T.);
#29978=ADVANCED_FACE('',(#4650),#672,.T.);
#29979=ADVANCED_FACE('',(#4651),#673,.T.);
#29980=ADVANCED_FACE('',(#4652),#674,.T.);
#29981=ADVANCED_FACE('',(#4653),#675,.T.);
#29982=ADVANCED_FACE('',(#4654),#676,.T.);
#29983=ADVANCED_FACE('',(#4655),#677,.T.);
#29984=ADVANCED_FACE('',(#4656),#678,.T.);
#29985=ADVANCED_FACE('',(#4657),#679,.T.);
#29986=ADVANCED_FACE('',(#4658),#680,.T.);
#29987=ADVANCED_FACE('',(#4659),#681,.T.);
#29988=ADVANCED_FACE('',(#4660),#682,.T.);
#29989=ADVANCED_FACE('',(#4661),#683,.T.);
#29990=ADVANCED_FACE('',(#4662),#684,.T.);
#29991=ADVANCED_FACE('',(#4663),#685,.T.);
#29992=ADVANCED_FACE('',(#4664),#686,.T.);
#29993=ADVANCED_FACE('',(#4665),#687,.T.);
#29994=ADVANCED_FACE('',(#4666),#688,.T.);
#29995=ADVANCED_FACE('',(#4667),#689,.T.);
#29996=ADVANCED_FACE('',(#4668),#690,.T.);
#29997=ADVANCED_FACE('',(#4669),#691,.T.);
#29998=ADVANCED_FACE('',(#4670),#692,.T.);
#29999=ADVANCED_FACE('',(#4671),#693,.T.);
#30000=ADVANCED_FACE('',(#4672),#694,.T.);
#30001=ADVANCED_FACE('',(#4673),#695,.T.);
#30002=ADVANCED_FACE('',(#4674),#696,.T.);
#30003=ADVANCED_FACE('',(#4675),#697,.T.);
#30004=ADVANCED_FACE('',(#4676),#698,.T.);
#30005=ADVANCED_FACE('',(#4677),#699,.T.);
#30006=ADVANCED_FACE('',(#4678),#700,.T.);
#30007=ADVANCED_FACE('',(#4679),#701,.T.);
#30008=ADVANCED_FACE('',(#4680),#702,.T.);
#30009=ADVANCED_FACE('',(#4681),#703,.T.);
#30010=ADVANCED_FACE('',(#4682),#704,.T.);
#30011=ADVANCED_FACE('',(#4683),#705,.T.);
#30012=ADVANCED_FACE('',(#4684),#706,.T.);
#30013=ADVANCED_FACE('',(#4685),#707,.T.);
#30014=ADVANCED_FACE('',(#4686),#708,.T.);
#30015=ADVANCED_FACE('',(#4687),#709,.T.);
#30016=ADVANCED_FACE('',(#4688),#710,.T.);
#30017=ADVANCED_FACE('',(#4689),#711,.T.);
#30018=ADVANCED_FACE('',(#4690),#712,.T.);
#30019=ADVANCED_FACE('',(#4691),#713,.T.);
#30020=ADVANCED_FACE('',(#4692),#714,.T.);
#30021=ADVANCED_FACE('',(#4693),#715,.T.);
#30022=ADVANCED_FACE('',(#4694),#716,.T.);
#30023=ADVANCED_FACE('',(#4695),#717,.T.);
#30024=ADVANCED_FACE('',(#4696),#718,.T.);
#30025=ADVANCED_FACE('',(#4697),#719,.T.);
#30026=ADVANCED_FACE('',(#4698),#720,.T.);
#30027=ADVANCED_FACE('',(#4699),#721,.T.);
#30028=ADVANCED_FACE('',(#4700),#722,.T.);
#30029=ADVANCED_FACE('',(#4701),#723,.T.);
#30030=ADVANCED_FACE('',(#4702),#724,.T.);
#30031=ADVANCED_FACE('',(#4703),#725,.T.);
#30032=ADVANCED_FACE('',(#4704),#726,.T.);
#30033=ADVANCED_FACE('',(#4705),#727,.T.);
#30034=ADVANCED_FACE('',(#4706),#728,.T.);
#30035=ADVANCED_FACE('',(#4707),#729,.T.);
#30036=ADVANCED_FACE('',(#4708),#730,.T.);
#30037=ADVANCED_FACE('',(#4709),#731,.T.);
#30038=ADVANCED_FACE('',(#4710),#732,.T.);
#30039=ADVANCED_FACE('',(#4711),#733,.T.);
#30040=ADVANCED_FACE('',(#4712),#734,.T.);
#30041=ADVANCED_FACE('',(#4713),#735,.T.);
#30042=ADVANCED_FACE('',(#4714),#736,.T.);
#30043=ADVANCED_FACE('',(#4715),#737,.T.);
#30044=ADVANCED_FACE('',(#4716),#738,.T.);
#30045=ADVANCED_FACE('',(#4717),#739,.T.);
#30046=ADVANCED_FACE('',(#4718),#740,.T.);
#30047=ADVANCED_FACE('',(#4719),#741,.T.);
#30048=ADVANCED_FACE('',(#4720),#742,.T.);
#30049=ADVANCED_FACE('',(#4721),#743,.T.);
#30050=ADVANCED_FACE('',(#4722),#744,.T.);
#30051=ADVANCED_FACE('',(#4723),#745,.T.);
#30052=ADVANCED_FACE('',(#4724),#746,.T.);
#30053=ADVANCED_FACE('',(#4725),#747,.T.);
#30054=ADVANCED_FACE('',(#4726),#748,.T.);
#30055=ADVANCED_FACE('',(#4727),#749,.T.);
#30056=ADVANCED_FACE('',(#4728),#750,.T.);
#30057=ADVANCED_FACE('',(#4729),#751,.T.);
#30058=ADVANCED_FACE('',(#4730),#752,.T.);
#30059=ADVANCED_FACE('',(#4731),#753,.T.);
#30060=ADVANCED_FACE('',(#4732),#754,.T.);
#30061=ADVANCED_FACE('',(#4733),#755,.T.);
#30062=ADVANCED_FACE('',(#4734),#756,.T.);
#30063=ADVANCED_FACE('',(#4735),#757,.T.);
#30064=ADVANCED_FACE('',(#4736),#758,.T.);
#30065=ADVANCED_FACE('',(#4737),#759,.T.);
#30066=ADVANCED_FACE('',(#4738),#760,.T.);
#30067=ADVANCED_FACE('',(#4739),#761,.T.);
#30068=ADVANCED_FACE('',(#4740),#762,.T.);
#30069=ADVANCED_FACE('',(#4741),#763,.T.);
#30070=ADVANCED_FACE('',(#4742),#764,.T.);
#30071=ADVANCED_FACE('',(#4743),#765,.T.);
#30072=ADVANCED_FACE('',(#4744),#766,.T.);
#30073=ADVANCED_FACE('',(#4745),#767,.T.);
#30074=ADVANCED_FACE('',(#4746),#768,.T.);
#30075=ADVANCED_FACE('',(#4747),#769,.T.);
#30076=ADVANCED_FACE('',(#4748),#770,.T.);
#30077=ADVANCED_FACE('',(#4749),#771,.T.);
#30078=ADVANCED_FACE('',(#4750),#772,.T.);
#30079=ADVANCED_FACE('',(#4751),#773,.T.);
#30080=ADVANCED_FACE('',(#4752),#774,.T.);
#30081=ADVANCED_FACE('',(#4753),#775,.T.);
#30082=ADVANCED_FACE('',(#4754),#776,.T.);
#30083=ADVANCED_FACE('',(#4755),#777,.T.);
#30084=ADVANCED_FACE('',(#4756),#778,.T.);
#30085=ADVANCED_FACE('',(#4757),#779,.T.);
#30086=ADVANCED_FACE('',(#4758),#780,.T.);
#30087=ADVANCED_FACE('',(#4759),#781,.T.);
#30088=ADVANCED_FACE('',(#4760),#782,.T.);
#30089=ADVANCED_FACE('',(#4761),#783,.T.);
#30090=ADVANCED_FACE('',(#4762),#784,.T.);
#30091=ADVANCED_FACE('',(#4763),#785,.T.);
#30092=ADVANCED_FACE('',(#4764),#786,.T.);
#30093=ADVANCED_FACE('',(#4765),#787,.T.);
#30094=ADVANCED_FACE('',(#4766),#788,.T.);
#30095=ADVANCED_FACE('',(#4767),#789,.T.);
#30096=ADVANCED_FACE('',(#4768),#790,.T.);
#30097=ADVANCED_FACE('',(#4769),#791,.T.);
#30098=ADVANCED_FACE('',(#4770),#792,.T.);
#30099=ADVANCED_FACE('',(#4771),#793,.T.);
#30100=ADVANCED_FACE('',(#4772),#794,.T.);
#30101=ADVANCED_FACE('',(#4773),#795,.T.);
#30102=ADVANCED_FACE('',(#4774),#796,.T.);
#30103=ADVANCED_FACE('',(#4775),#797,.T.);
#30104=ADVANCED_FACE('',(#4776),#798,.T.);
#30105=ADVANCED_FACE('',(#4777),#799,.T.);
#30106=ADVANCED_FACE('',(#4778),#800,.T.);
#30107=ADVANCED_FACE('',(#4779),#801,.T.);
#30108=ADVANCED_FACE('',(#4780),#802,.T.);
#30109=ADVANCED_FACE('',(#4781),#803,.T.);
#30110=ADVANCED_FACE('',(#4782),#28636,.F.);
#30111=ADVANCED_FACE('',(#4783),#424,.F.);
#30112=ADVANCED_FACE('',(#4784),#28637,.T.);
#30113=ADVANCED_FACE('',(#4785),#804,.T.);
#30114=ADVANCED_FACE('',(#4786),#425,.F.);
#30115=ADVANCED_FACE('',(#4787),#161,.F.);
#30116=ADVANCED_FACE('',(#4788),#805,.T.);
#30117=ADVANCED_FACE('',(#4789,#3526),#28638,.T.);
#30118=ADVANCED_FACE('',(#4790),#28639,.F.);
#30119=ADVANCED_FACE('',(#4791),#28640,.T.);
#30120=ADVANCED_FACE('',(#4792),#28641,.F.);
#30121=ADVANCED_FACE('',(#4793),#28642,.F.);
#30122=ADVANCED_FACE('',(#4794),#28643,.F.);
#30123=ADVANCED_FACE('',(#4795),#28644,.T.);
#30124=ADVANCED_FACE('',(#4796),#28645,.F.);
#30125=ADVANCED_FACE('',(#4797),#28646,.F.);
#30126=ADVANCED_FACE('',(#4798),#28647,.F.);
#30127=ADVANCED_FACE('',(#4799),#28648,.T.);
#30128=ADVANCED_FACE('',(#4800),#28649,.F.);
#30129=ADVANCED_FACE('',(#4801),#28650,.F.);
#30130=ADVANCED_FACE('',(#4802),#28651,.F.);
#30131=ADVANCED_FACE('',(#4803),#28652,.T.);
#30132=ADVANCED_FACE('',(#4804),#28653,.F.);
#30133=ADVANCED_FACE('',(#4805),#28654,.F.);
#30134=ADVANCED_FACE('',(#4806),#28655,.F.);
#30135=ADVANCED_FACE('',(#4807),#28656,.T.);
#30136=ADVANCED_FACE('',(#4808),#28657,.F.);
#30137=ADVANCED_FACE('',(#4809),#28658,.F.);
#30138=ADVANCED_FACE('',(#4810),#28659,.F.);
#30139=ADVANCED_FACE('',(#4811),#28660,.T.);
#30140=ADVANCED_FACE('',(#4812),#28661,.F.);
#30141=ADVANCED_FACE('',(#4813),#28662,.F.);
#30142=ADVANCED_FACE('',(#4814),#28663,.F.);
#30143=ADVANCED_FACE('',(#4815),#28664,.T.);
#30144=ADVANCED_FACE('',(#4816),#28665,.F.);
#30145=ADVANCED_FACE('',(#4817),#28666,.F.);
#30146=ADVANCED_FACE('',(#4818),#28667,.F.);
#30147=ADVANCED_FACE('',(#4819),#28668,.T.);
#30148=ADVANCED_FACE('',(#4820),#28669,.F.);
#30149=ADVANCED_FACE('',(#4821),#28670,.F.);
#30150=ADVANCED_FACE('',(#4822),#28671,.F.);
#30151=ADVANCED_FACE('',(#4823),#28672,.T.);
#30152=ADVANCED_FACE('',(#4824),#28673,.F.);
#30153=ADVANCED_FACE('',(#4825),#28674,.F.);
#30154=ADVANCED_FACE('',(#4826),#28675,.F.);
#30155=ADVANCED_FACE('',(#4827),#28676,.T.);
#30156=ADVANCED_FACE('',(#4828),#28677,.F.);
#30157=ADVANCED_FACE('',(#4829),#28678,.F.);
#30158=ADVANCED_FACE('',(#4830),#28679,.F.);
#30159=ADVANCED_FACE('',(#4831),#28680,.T.);
#30160=ADVANCED_FACE('',(#4832),#28681,.F.);
#30161=ADVANCED_FACE('',(#4833),#28682,.F.);
#30162=ADVANCED_FACE('',(#4834),#28683,.F.);
#30163=ADVANCED_FACE('',(#4835),#28684,.T.);
#30164=ADVANCED_FACE('',(#4836),#28685,.F.);
#30165=ADVANCED_FACE('',(#4837),#28686,.F.);
#30166=ADVANCED_FACE('',(#4838),#28687,.F.);
#30167=ADVANCED_FACE('',(#4839),#28688,.T.);
#30168=ADVANCED_FACE('',(#4840),#28689,.F.);
#30169=ADVANCED_FACE('',(#4841),#28690,.F.);
#30170=ADVANCED_FACE('',(#4842),#28691,.F.);
#30171=ADVANCED_FACE('',(#4843),#28692,.T.);
#30172=ADVANCED_FACE('',(#4844),#28693,.F.);
#30173=ADVANCED_FACE('',(#4845),#28694,.F.);
#30174=ADVANCED_FACE('',(#4846),#28695,.F.);
#30175=ADVANCED_FACE('',(#4847),#28696,.T.);
#30176=ADVANCED_FACE('',(#4848),#28697,.F.);
#30177=ADVANCED_FACE('',(#4849),#28698,.F.);
#30178=ADVANCED_FACE('',(#4850),#28699,.F.);
#30179=ADVANCED_FACE('',(#4851),#28700,.T.);
#30180=ADVANCED_FACE('',(#4852),#28701,.F.);
#30181=ADVANCED_FACE('',(#4853),#28702,.F.);
#30182=ADVANCED_FACE('',(#4854),#28703,.F.);
#30183=ADVANCED_FACE('',(#4855),#28704,.T.);
#30184=ADVANCED_FACE('',(#4856),#28705,.F.);
#30185=ADVANCED_FACE('',(#4857),#28706,.F.);
#30186=ADVANCED_FACE('',(#4858),#28707,.F.);
#30187=ADVANCED_FACE('',(#4859),#28708,.T.);
#30188=ADVANCED_FACE('',(#4860),#28709,.F.);
#30189=ADVANCED_FACE('',(#4861),#28710,.F.);
#30190=ADVANCED_FACE('',(#4862),#28711,.F.);
#30191=ADVANCED_FACE('',(#4863),#28712,.T.);
#30192=ADVANCED_FACE('',(#4864),#28713,.F.);
#30193=ADVANCED_FACE('',(#4865),#28714,.F.);
#30194=ADVANCED_FACE('',(#4866),#28715,.F.);
#30195=ADVANCED_FACE('',(#4867),#28716,.T.);
#30196=ADVANCED_FACE('',(#4868),#28717,.F.);
#30197=ADVANCED_FACE('',(#4869),#28718,.F.);
#30198=ADVANCED_FACE('',(#4870),#28719,.F.);
#30199=ADVANCED_FACE('',(#4871),#28720,.T.);
#30200=ADVANCED_FACE('',(#4872),#28721,.F.);
#30201=ADVANCED_FACE('',(#4873),#28722,.F.);
#30202=ADVANCED_FACE('',(#4874),#28723,.F.);
#30203=ADVANCED_FACE('',(#4875),#28724,.T.);
#30204=ADVANCED_FACE('',(#4876),#28725,.F.);
#30205=ADVANCED_FACE('',(#4877),#28726,.F.);
#30206=ADVANCED_FACE('',(#4878),#28727,.F.);
#30207=ADVANCED_FACE('',(#4879),#28728,.T.);
#30208=ADVANCED_FACE('',(#4880),#28729,.F.);
#30209=ADVANCED_FACE('',(#4881),#28730,.F.);
#30210=ADVANCED_FACE('',(#4882),#28731,.F.);
#30211=ADVANCED_FACE('',(#4883),#28732,.T.);
#30212=ADVANCED_FACE('',(#4884),#28733,.F.);
#30213=ADVANCED_FACE('',(#4885),#28734,.F.);
#30214=ADVANCED_FACE('',(#4886),#28735,.F.);
#30215=ADVANCED_FACE('',(#4887),#28736,.T.);
#30216=ADVANCED_FACE('',(#4888),#28737,.F.);
#30217=ADVANCED_FACE('',(#4889),#28738,.F.);
#30218=ADVANCED_FACE('',(#4890),#28739,.F.);
#30219=ADVANCED_FACE('',(#4891),#28740,.T.);
#30220=ADVANCED_FACE('',(#4892),#28741,.F.);
#30221=ADVANCED_FACE('',(#4893),#28742,.F.);
#30222=ADVANCED_FACE('',(#4894),#28743,.F.);
#30223=ADVANCED_FACE('',(#4895),#28744,.T.);
#30224=ADVANCED_FACE('',(#4896),#28745,.F.);
#30225=ADVANCED_FACE('',(#4897),#28746,.F.);
#30226=ADVANCED_FACE('',(#4898),#28747,.F.);
#30227=ADVANCED_FACE('',(#4899),#28748,.T.);
#30228=ADVANCED_FACE('',(#4900),#28749,.F.);
#30229=ADVANCED_FACE('',(#4901),#28750,.F.);
#30230=ADVANCED_FACE('',(#4902),#28751,.F.);
#30231=ADVANCED_FACE('',(#4903),#28752,.T.);
#30232=ADVANCED_FACE('',(#4904),#28753,.F.);
#30233=ADVANCED_FACE('',(#4905),#28754,.F.);
#30234=ADVANCED_FACE('',(#4906),#28755,.F.);
#30235=ADVANCED_FACE('',(#4907),#28756,.T.);
#30236=ADVANCED_FACE('',(#4908),#28757,.F.);
#30237=ADVANCED_FACE('',(#4909),#28758,.F.);
#30238=ADVANCED_FACE('',(#4910),#28759,.F.);
#30239=ADVANCED_FACE('',(#4911),#28760,.T.);
#30240=ADVANCED_FACE('',(#4912),#28761,.F.);
#30241=ADVANCED_FACE('',(#4913),#28762,.F.);
#30242=ADVANCED_FACE('',(#4914),#28763,.F.);
#30243=ADVANCED_FACE('',(#4915),#28764,.T.);
#30244=ADVANCED_FACE('',(#4916),#28765,.F.);
#30245=ADVANCED_FACE('',(#4917),#28766,.F.);
#30246=ADVANCED_FACE('',(#4918),#28767,.F.);
#30247=ADVANCED_FACE('',(#4919),#28768,.T.);
#30248=ADVANCED_FACE('',(#4920),#28769,.F.);
#30249=ADVANCED_FACE('',(#4921),#28770,.F.);
#30250=ADVANCED_FACE('',(#4922),#28771,.F.);
#30251=ADVANCED_FACE('',(#4923),#28772,.T.);
#30252=ADVANCED_FACE('',(#4924),#28773,.F.);
#30253=ADVANCED_FACE('',(#4925),#28774,.F.);
#30254=ADVANCED_FACE('',(#4926),#28775,.F.);
#30255=ADVANCED_FACE('',(#4927),#28776,.T.);
#30256=ADVANCED_FACE('',(#4928),#28777,.F.);
#30257=ADVANCED_FACE('',(#4929),#28778,.F.);
#30258=ADVANCED_FACE('',(#4930),#28779,.F.);
#30259=ADVANCED_FACE('',(#4931),#28780,.T.);
#30260=ADVANCED_FACE('',(#4932),#28781,.F.);
#30261=ADVANCED_FACE('',(#4933),#28782,.F.);
#30262=ADVANCED_FACE('',(#4934),#2044,.F.);
#30263=ADVANCED_FACE('',(#4935),#28783,.F.);
#30264=ADVANCED_FACE('',(#4936),#28784,.F.);
#30265=ADVANCED_FACE('',(#4937),#28785,.F.);
#30266=ADVANCED_FACE('',(#4938),#28786,.F.);
#30267=ADVANCED_FACE('',(#4939),#28787,.F.);
#30268=ADVANCED_FACE('',(#4940),#28788,.F.);
#30269=ADVANCED_FACE('',(#4941,#3527),#28789,.F.);
#30270=ADVANCED_FACE('',(#4942),#28790,.T.);
#30271=ADVANCED_FACE('',(#4943),#2045,.T.);
#30272=ADVANCED_FACE('',(#4944,#3528,#3529,#3530,#3531,#3532,#3533,#3534,
#3535,#3536,#3537,#3538,#3539,#3540,#3541,#3542,#3543,#3544,#3545,#3546,
#3547,#3548,#3549,#3550,#3551,#3552,#3553,#3554,#3555,#3556,#3557,#3558,
#3559,#3560,#3561,#3562),#806,.T.);
#30273=ADVANCED_FACE('',(#4945),#2046,.T.);
#30274=ADVANCED_FACE('',(#4946,#3563),#28791,.T.);
#30275=ADVANCED_FACE('',(#4947),#28792,.T.);
#30276=ADVANCED_FACE('',(#4948),#28793,.F.);
#30277=ADVANCED_FACE('',(#4949),#28794,.T.);
#30278=ADVANCED_FACE('',(#4950),#807,.T.);
#30279=ADVANCED_FACE('',(#4951),#2047,.T.);
#30280=ADVANCED_FACE('',(#4952),#28795,.T.);
#30281=ADVANCED_FACE('',(#4953),#28796,.F.);
#30282=ADVANCED_FACE('',(#4954),#2048,.T.);
#30283=ADVANCED_FACE('',(#4955),#28797,.T.);
#30284=ADVANCED_FACE('',(#4956),#28798,.F.);
#30285=ADVANCED_FACE('',(#4957),#28799,.T.);
#30286=ADVANCED_FACE('',(#4958),#28800,.F.);
#30287=ADVANCED_FACE('',(#4959),#28801,.T.);
#30288=ADVANCED_FACE('',(#4960),#808,.T.);
#30289=ADVANCED_FACE('',(#4961),#2049,.T.);
#30290=ADVANCED_FACE('',(#4962),#28802,.T.);
#30291=ADVANCED_FACE('',(#4963),#28803,.F.);
#30292=ADVANCED_FACE('',(#4964),#28804,.T.);
#30293=ADVANCED_FACE('',(#4965),#2050,.T.);
#30294=ADVANCED_FACE('',(#4966),#28805,.F.);
#30295=ADVANCED_FACE('',(#4967),#28806,.T.);
#30296=ADVANCED_FACE('',(#4968),#809,.T.);
#30297=ADVANCED_FACE('',(#4969),#2051,.T.);
#30298=ADVANCED_FACE('',(#4970),#28807,.T.);
#30299=ADVANCED_FACE('',(#4971),#28808,.T.);
#30300=ADVANCED_FACE('',(#4972),#28809,.T.);
#30301=ADVANCED_FACE('',(#4973),#28810,.T.);
#30302=ADVANCED_FACE('',(#4974),#28811,.F.);
#30303=ADVANCED_FACE('',(#4975),#28812,.T.);
#30304=ADVANCED_FACE('',(#4976),#28813,.T.);
#30305=ADVANCED_FACE('',(#4977),#2052,.T.);
#30306=ADVANCED_FACE('',(#4978),#28814,.F.);
#30307=ADVANCED_FACE('',(#4979),#28815,.T.);
#30308=ADVANCED_FACE('',(#4980),#2053,.T.);
#30309=ADVANCED_FACE('',(#4981),#28816,.F.);
#30310=ADVANCED_FACE('',(#4982,#3564),#28817,.T.);
#30311=ADVANCED_FACE('',(#4983),#28818,.F.);
#30312=ADVANCED_FACE('',(#4984),#28819,.F.);
#30313=ADVANCED_FACE('',(#4985),#810,.T.);
#30314=ADVANCED_FACE('',(#4986),#2054,.T.);
#30315=ADVANCED_FACE('',(#4987),#28820,.F.);
#30316=ADVANCED_FACE('',(#4988),#811,.F.);
#30317=ADVANCED_FACE('',(#4989,#3565),#28821,.T.);
#30318=ADVANCED_FACE('',(#4990),#812,.T.);
#30319=ADVANCED_FACE('',(#4991),#813,.T.);
#30320=ADVANCED_FACE('',(#4992),#814,.T.);
#30321=ADVANCED_FACE('',(#4993),#815,.T.);
#30322=ADVANCED_FACE('',(#4994),#816,.T.);
#30323=ADVANCED_FACE('',(#4995),#817,.T.);
#30324=ADVANCED_FACE('',(#4996),#818,.T.);
#30325=ADVANCED_FACE('',(#4997),#819,.T.);
#30326=ADVANCED_FACE('',(#4998),#820,.T.);
#30327=ADVANCED_FACE('',(#4999),#821,.T.);
#30328=ADVANCED_FACE('',(#5000),#822,.T.);
#30329=ADVANCED_FACE('',(#5001),#823,.T.);
#30330=ADVANCED_FACE('',(#5002),#824,.T.);
#30331=ADVANCED_FACE('',(#5003),#825,.T.);
#30332=ADVANCED_FACE('',(#5004),#826,.T.);
#30333=ADVANCED_FACE('',(#5005),#827,.T.);
#30334=ADVANCED_FACE('',(#5006),#828,.T.);
#30335=ADVANCED_FACE('',(#5007),#829,.T.);
#30336=ADVANCED_FACE('',(#5008),#830,.T.);
#30337=ADVANCED_FACE('',(#5009),#831,.T.);
#30338=ADVANCED_FACE('',(#5010),#832,.T.);
#30339=ADVANCED_FACE('',(#5011),#833,.T.);
#30340=ADVANCED_FACE('',(#5012),#834,.T.);
#30341=ADVANCED_FACE('',(#5013),#835,.T.);
#30342=ADVANCED_FACE('',(#5014),#836,.T.);
#30343=ADVANCED_FACE('',(#5015),#837,.T.);
#30344=ADVANCED_FACE('',(#5016),#838,.T.);
#30345=ADVANCED_FACE('',(#5017),#839,.T.);
#30346=ADVANCED_FACE('',(#5018),#840,.T.);
#30347=ADVANCED_FACE('',(#5019),#841,.T.);
#30348=ADVANCED_FACE('',(#5020),#842,.T.);
#30349=ADVANCED_FACE('',(#5021),#843,.T.);
#30350=ADVANCED_FACE('',(#5022),#2055,.F.);
#30351=ADVANCED_FACE('',(#5023,#3566),#844,.F.);
#30352=ADVANCED_FACE('',(#5024,#3567),#28822,.T.);
#30353=ADVANCED_FACE('',(#5025),#2056,.F.);
#30354=ADVANCED_FACE('',(#5026,#3568),#28823,.T.);
#30355=ADVANCED_FACE('',(#5027),#426,.T.);
#30356=ADVANCED_FACE('',(#5028),#845,.F.);
#30357=ADVANCED_FACE('',(#5029,#3569),#846,.T.);
#30358=ADVANCED_FACE('',(#5030),#427,.F.);
#30359=ADVANCED_FACE('',(#5031),#28824,.T.);
#30360=ADVANCED_FACE('',(#5032),#847,.T.);
#30361=ADVANCED_FACE('',(#5033),#428,.F.);
#30362=ADVANCED_FACE('',(#5034),#28825,.T.);
#30363=ADVANCED_FACE('',(#5035),#28826,.T.);
#30364=ADVANCED_FACE('',(#5036),#2057,.T.);
#30365=ADVANCED_FACE('',(#5037),#848,.T.);
#30366=ADVANCED_FACE('',(#5038,#3570),#28827,.T.);
#30367=ADVANCED_FACE('',(#5039),#2058,.T.);
#30368=ADVANCED_FACE('',(#5040),#2059,.T.);
#30369=ADVANCED_FACE('',(#5041,#3571),#28828,.T.);
#30370=ADVANCED_FACE('',(#5042),#849,.T.);
#30371=ADVANCED_FACE('',(#5043),#2060,.T.);
#30372=ADVANCED_FACE('',(#5044),#850,.T.);
#30373=ADVANCED_FACE('',(#5045),#851,.T.);
#30374=ADVANCED_FACE('',(#5046),#852,.T.);
#30375=ADVANCED_FACE('',(#5047),#853,.T.);
#30376=ADVANCED_FACE('',(#5048),#854,.T.);
#30377=ADVANCED_FACE('',(#5049),#855,.T.);
#30378=ADVANCED_FACE('',(#5050),#856,.T.);
#30379=ADVANCED_FACE('',(#5051),#857,.T.);
#30380=ADVANCED_FACE('',(#5052),#858,.T.);
#30381=ADVANCED_FACE('',(#5053),#859,.T.);
#30382=ADVANCED_FACE('',(#5054),#860,.T.);
#30383=ADVANCED_FACE('',(#5055),#861,.T.);
#30384=ADVANCED_FACE('',(#5056),#862,.T.);
#30385=ADVANCED_FACE('',(#5057),#863,.T.);
#30386=ADVANCED_FACE('',(#5058),#864,.T.);
#30387=ADVANCED_FACE('',(#5059),#865,.T.);
#30388=ADVANCED_FACE('',(#5060),#866,.T.);
#30389=ADVANCED_FACE('',(#5061),#867,.T.);
#30390=ADVANCED_FACE('',(#5062),#868,.T.);
#30391=ADVANCED_FACE('',(#5063),#869,.T.);
#30392=ADVANCED_FACE('',(#5064),#870,.T.);
#30393=ADVANCED_FACE('',(#5065),#871,.T.);
#30394=ADVANCED_FACE('',(#5066),#872,.T.);
#30395=ADVANCED_FACE('',(#5067),#873,.T.);
#30396=ADVANCED_FACE('',(#5068),#874,.T.);
#30397=ADVANCED_FACE('',(#5069),#875,.T.);
#30398=ADVANCED_FACE('',(#5070),#876,.T.);
#30399=ADVANCED_FACE('',(#5071),#877,.T.);
#30400=ADVANCED_FACE('',(#5072),#878,.T.);
#30401=ADVANCED_FACE('',(#5073),#879,.T.);
#30402=ADVANCED_FACE('',(#5074),#880,.T.);
#30403=ADVANCED_FACE('',(#5075),#881,.T.);
#30404=ADVANCED_FACE('',(#5076),#882,.T.);
#30405=ADVANCED_FACE('',(#5077),#883,.T.);
#30406=ADVANCED_FACE('',(#5078),#884,.T.);
#30407=ADVANCED_FACE('',(#5079),#885,.T.);
#30408=ADVANCED_FACE('',(#5080),#886,.T.);
#30409=ADVANCED_FACE('',(#5081),#887,.T.);
#30410=ADVANCED_FACE('',(#5082),#888,.T.);
#30411=ADVANCED_FACE('',(#5083),#889,.T.);
#30412=ADVANCED_FACE('',(#5084),#890,.T.);
#30413=ADVANCED_FACE('',(#5085),#891,.T.);
#30414=ADVANCED_FACE('',(#5086),#892,.T.);
#30415=ADVANCED_FACE('',(#5087),#893,.T.);
#30416=ADVANCED_FACE('',(#5088),#894,.T.);
#30417=ADVANCED_FACE('',(#5089),#895,.T.);
#30418=ADVANCED_FACE('',(#5090),#896,.T.);
#30419=ADVANCED_FACE('',(#5091),#897,.T.);
#30420=ADVANCED_FACE('',(#5092),#898,.T.);
#30421=ADVANCED_FACE('',(#5093),#899,.T.);
#30422=ADVANCED_FACE('',(#5094),#900,.T.);
#30423=ADVANCED_FACE('',(#5095),#901,.T.);
#30424=ADVANCED_FACE('',(#5096),#902,.T.);
#30425=ADVANCED_FACE('',(#5097),#903,.T.);
#30426=ADVANCED_FACE('',(#5098),#904,.T.);
#30427=ADVANCED_FACE('',(#5099),#905,.T.);
#30428=ADVANCED_FACE('',(#5100),#906,.T.);
#30429=ADVANCED_FACE('',(#5101),#907,.T.);
#30430=ADVANCED_FACE('',(#5102),#908,.T.);
#30431=ADVANCED_FACE('',(#5103),#909,.T.);
#30432=ADVANCED_FACE('',(#5104),#910,.T.);
#30433=ADVANCED_FACE('',(#5105),#911,.T.);
#30434=ADVANCED_FACE('',(#5106),#912,.T.);
#30435=ADVANCED_FACE('',(#5107),#913,.T.);
#30436=ADVANCED_FACE('',(#5108),#914,.T.);
#30437=ADVANCED_FACE('',(#5109),#915,.T.);
#30438=ADVANCED_FACE('',(#5110),#916,.T.);
#30439=ADVANCED_FACE('',(#5111),#917,.T.);
#30440=ADVANCED_FACE('',(#5112),#918,.T.);
#30441=ADVANCED_FACE('',(#5113),#919,.T.);
#30442=ADVANCED_FACE('',(#5114),#920,.T.);
#30443=ADVANCED_FACE('',(#5115),#921,.T.);
#30444=ADVANCED_FACE('',(#5116),#922,.T.);
#30445=ADVANCED_FACE('',(#5117),#923,.T.);
#30446=ADVANCED_FACE('',(#5118),#924,.T.);
#30447=ADVANCED_FACE('',(#5119),#925,.T.);
#30448=ADVANCED_FACE('',(#5120),#926,.T.);
#30449=ADVANCED_FACE('',(#5121),#927,.T.);
#30450=ADVANCED_FACE('',(#5122),#928,.T.);
#30451=ADVANCED_FACE('',(#5123),#929,.T.);
#30452=ADVANCED_FACE('',(#5124),#930,.T.);
#30453=ADVANCED_FACE('',(#5125),#931,.T.);
#30454=ADVANCED_FACE('',(#5126),#932,.T.);
#30455=ADVANCED_FACE('',(#5127),#933,.T.);
#30456=ADVANCED_FACE('',(#5128),#934,.T.);
#30457=ADVANCED_FACE('',(#5129),#935,.T.);
#30458=ADVANCED_FACE('',(#5130),#936,.T.);
#30459=ADVANCED_FACE('',(#5131),#937,.T.);
#30460=ADVANCED_FACE('',(#5132),#938,.T.);
#30461=ADVANCED_FACE('',(#5133),#939,.T.);
#30462=ADVANCED_FACE('',(#5134),#940,.T.);
#30463=ADVANCED_FACE('',(#5135),#941,.T.);
#30464=ADVANCED_FACE('',(#5136),#942,.T.);
#30465=ADVANCED_FACE('',(#5137),#943,.T.);
#30466=ADVANCED_FACE('',(#5138),#944,.T.);
#30467=ADVANCED_FACE('',(#5139),#945,.T.);
#30468=ADVANCED_FACE('',(#5140),#946,.T.);
#30469=ADVANCED_FACE('',(#5141),#947,.T.);
#30470=ADVANCED_FACE('',(#5142),#948,.T.);
#30471=ADVANCED_FACE('',(#5143),#949,.T.);
#30472=ADVANCED_FACE('',(#5144),#950,.T.);
#30473=ADVANCED_FACE('',(#5145),#951,.T.);
#30474=ADVANCED_FACE('',(#5146),#952,.T.);
#30475=ADVANCED_FACE('',(#5147),#953,.T.);
#30476=ADVANCED_FACE('',(#5148),#954,.T.);
#30477=ADVANCED_FACE('',(#5149),#955,.T.);
#30478=ADVANCED_FACE('',(#5150),#956,.T.);
#30479=ADVANCED_FACE('',(#5151),#957,.T.);
#30480=ADVANCED_FACE('',(#5152),#958,.T.);
#30481=ADVANCED_FACE('',(#5153),#959,.T.);
#30482=ADVANCED_FACE('',(#5154),#960,.T.);
#30483=ADVANCED_FACE('',(#5155),#961,.T.);
#30484=ADVANCED_FACE('',(#5156),#962,.T.);
#30485=ADVANCED_FACE('',(#5157),#963,.T.);
#30486=ADVANCED_FACE('',(#5158),#964,.T.);
#30487=ADVANCED_FACE('',(#5159),#965,.T.);
#30488=ADVANCED_FACE('',(#5160),#966,.T.);
#30489=ADVANCED_FACE('',(#5161),#967,.T.);
#30490=ADVANCED_FACE('',(#5162),#968,.T.);
#30491=ADVANCED_FACE('',(#5163),#969,.T.);
#30492=ADVANCED_FACE('',(#5164),#970,.T.);
#30493=ADVANCED_FACE('',(#5165),#971,.T.);
#30494=ADVANCED_FACE('',(#5166),#972,.T.);
#30495=ADVANCED_FACE('',(#5167),#973,.T.);
#30496=ADVANCED_FACE('',(#5168),#974,.T.);
#30497=ADVANCED_FACE('',(#5169),#975,.T.);
#30498=ADVANCED_FACE('',(#5170),#976,.T.);
#30499=ADVANCED_FACE('',(#5171),#977,.T.);
#30500=ADVANCED_FACE('',(#5172),#978,.T.);
#30501=ADVANCED_FACE('',(#5173),#979,.T.);
#30502=ADVANCED_FACE('',(#5174),#980,.T.);
#30503=ADVANCED_FACE('',(#5175),#981,.T.);
#30504=ADVANCED_FACE('',(#5176),#982,.T.);
#30505=ADVANCED_FACE('',(#5177),#983,.T.);
#30506=ADVANCED_FACE('',(#5178),#984,.T.);
#30507=ADVANCED_FACE('',(#5179),#985,.T.);
#30508=ADVANCED_FACE('',(#5180),#986,.T.);
#30509=ADVANCED_FACE('',(#5181),#987,.T.);
#30510=ADVANCED_FACE('',(#5182),#988,.T.);
#30511=ADVANCED_FACE('',(#5183),#989,.T.);
#30512=ADVANCED_FACE('',(#5184),#990,.T.);
#30513=ADVANCED_FACE('',(#5185),#991,.T.);
#30514=ADVANCED_FACE('',(#5186),#992,.T.);
#30515=ADVANCED_FACE('',(#5187),#993,.T.);
#30516=ADVANCED_FACE('',(#5188),#994,.T.);
#30517=ADVANCED_FACE('',(#5189),#995,.T.);
#30518=ADVANCED_FACE('',(#5190),#996,.T.);
#30519=ADVANCED_FACE('',(#5191),#997,.T.);
#30520=ADVANCED_FACE('',(#5192),#998,.T.);
#30521=ADVANCED_FACE('',(#5193),#999,.T.);
#30522=ADVANCED_FACE('',(#5194),#28829,.F.);
#30523=ADVANCED_FACE('',(#5195),#429,.F.);
#30524=ADVANCED_FACE('',(#5196),#28830,.T.);
#30525=ADVANCED_FACE('',(#5197),#1000,.T.);
#30526=ADVANCED_FACE('',(#5198),#430,.F.);
#30527=ADVANCED_FACE('',(#5199),#1001,.T.);
#30528=ADVANCED_FACE('',(#5200),#2061,.T.);
#30529=ADVANCED_FACE('',(#5201),#1002,.T.);
#30530=ADVANCED_FACE('',(#5202),#2062,.T.);
#30531=ADVANCED_FACE('',(#5203),#28831,.T.);
#30532=ADVANCED_FACE('',(#5204,#3572),#156,.T.);
#30533=ADVANCED_FACE('',(#5205),#2063,.F.);
#30534=ADVANCED_FACE('',(#5206),#1003,.F.);
#30535=ADVANCED_FACE('',(#5207,#3573),#28832,.T.);
#30536=ADVANCED_FACE('',(#5208),#28833,.T.);
#30537=ADVANCED_FACE('',(#5209),#1004,.F.);
#30538=ADVANCED_FACE('',(#5210),#28834,.T.);
#30539=ADVANCED_FACE('',(#5211),#2064,.T.);
#30540=ADVANCED_FACE('',(#5212),#1005,.T.);
#30541=ADVANCED_FACE('',(#5213),#28835,.T.);
#30542=ADVANCED_FACE('',(#5214),#1006,.F.);
#30543=ADVANCED_FACE('',(#5215),#28836,.T.);
#30544=ADVANCED_FACE('',(#5216),#2065,.T.);
#30545=ADVANCED_FACE('',(#5217),#28837,.T.);
#30546=ADVANCED_FACE('',(#5218),#1007,.F.);
#30547=ADVANCED_FACE('',(#5219),#28838,.T.);
#30548=ADVANCED_FACE('',(#5220),#2066,.T.);
#30549=ADVANCED_FACE('',(#5221),#28839,.T.);
#30550=ADVANCED_FACE('',(#5222),#1008,.F.);
#30551=ADVANCED_FACE('',(#5223),#28840,.T.);
#30552=ADVANCED_FACE('',(#5224),#2067,.T.);
#30553=ADVANCED_FACE('',(#5225),#28841,.T.);
#30554=ADVANCED_FACE('',(#5226),#1009,.F.);
#30555=ADVANCED_FACE('',(#5227),#28842,.T.);
#30556=ADVANCED_FACE('',(#5228),#2068,.T.);
#30557=ADVANCED_FACE('',(#5229),#28843,.T.);
#30558=ADVANCED_FACE('',(#5230),#1010,.F.);
#30559=ADVANCED_FACE('',(#5231),#28844,.T.);
#30560=ADVANCED_FACE('',(#5232),#2069,.T.);
#30561=ADVANCED_FACE('',(#5233),#28845,.T.);
#30562=ADVANCED_FACE('',(#5234),#1011,.F.);
#30563=ADVANCED_FACE('',(#5235),#28846,.T.);
#30564=ADVANCED_FACE('',(#5236),#2070,.T.);
#30565=ADVANCED_FACE('',(#5237),#28847,.T.);
#30566=ADVANCED_FACE('',(#5238),#1012,.F.);
#30567=ADVANCED_FACE('',(#5239),#28848,.T.);
#30568=ADVANCED_FACE('',(#5240),#2071,.T.);
#30569=ADVANCED_FACE('',(#5241),#28849,.T.);
#30570=ADVANCED_FACE('',(#5242),#1013,.F.);
#30571=ADVANCED_FACE('',(#5243),#28850,.T.);
#30572=ADVANCED_FACE('',(#5244),#2072,.T.);
#30573=ADVANCED_FACE('',(#5245),#28851,.T.);
#30574=ADVANCED_FACE('',(#5246),#1014,.F.);
#30575=ADVANCED_FACE('',(#5247),#28852,.T.);
#30576=ADVANCED_FACE('',(#5248),#2073,.T.);
#30577=ADVANCED_FACE('',(#5249),#28853,.T.);
#30578=ADVANCED_FACE('',(#5250),#1015,.F.);
#30579=ADVANCED_FACE('',(#5251),#28854,.T.);
#30580=ADVANCED_FACE('',(#5252),#2074,.T.);
#30581=ADVANCED_FACE('',(#5253),#28855,.T.);
#30582=ADVANCED_FACE('',(#5254),#1016,.F.);
#30583=ADVANCED_FACE('',(#5255),#28856,.T.);
#30584=ADVANCED_FACE('',(#5256),#2075,.T.);
#30585=ADVANCED_FACE('',(#5257),#28857,.T.);
#30586=ADVANCED_FACE('',(#5258),#1017,.F.);
#30587=ADVANCED_FACE('',(#5259),#28858,.T.);
#30588=ADVANCED_FACE('',(#5260),#2076,.T.);
#30589=ADVANCED_FACE('',(#5261),#28859,.T.);
#30590=ADVANCED_FACE('',(#5262),#1018,.F.);
#30591=ADVANCED_FACE('',(#5263),#28860,.T.);
#30592=ADVANCED_FACE('',(#5264),#2077,.T.);
#30593=ADVANCED_FACE('',(#5265),#28861,.T.);
#30594=ADVANCED_FACE('',(#5266),#1019,.F.);
#30595=ADVANCED_FACE('',(#5267),#28862,.T.);
#30596=ADVANCED_FACE('',(#5268),#28863,.T.);
#30597=ADVANCED_FACE('',(#5269),#28864,.T.);
#30598=ADVANCED_FACE('',(#5270),#28865,.T.);
#30599=ADVANCED_FACE('',(#5271),#28866,.T.);
#30600=ADVANCED_FACE('',(#5272),#28867,.T.);
#30601=ADVANCED_FACE('',(#5273),#28868,.T.);
#30602=ADVANCED_FACE('',(#5274),#28869,.F.);
#30603=ADVANCED_FACE('',(#5275),#28870,.F.);
#30604=ADVANCED_FACE('',(#5276),#28871,.F.);
#30605=ADVANCED_FACE('',(#5277,#3574),#28872,.T.);
#30606=ADVANCED_FACE('',(#5278),#28873,.F.);
#30607=ADVANCED_FACE('',(#5279),#28874,.F.);
#30608=ADVANCED_FACE('',(#5280),#28875,.F.);
#30609=ADVANCED_FACE('',(#5281),#28876,.F.);
#30610=ADVANCED_FACE('',(#5282),#28877,.T.);
#30611=ADVANCED_FACE('',(#5283),#28878,.T.);
#30612=ADVANCED_FACE('',(#5284),#28879,.T.);
#30613=ADVANCED_FACE('',(#5285),#28880,.T.);
#30614=ADVANCED_FACE('',(#5286),#28881,.T.);
#30615=ADVANCED_FACE('',(#5287),#28882,.T.);
#30616=ADVANCED_FACE('',(#5288),#28883,.T.);
#30617=ADVANCED_FACE('',(#5289),#28884,.T.);
#30618=ADVANCED_FACE('',(#5290),#28885,.T.);
#30619=ADVANCED_FACE('',(#5291),#28886,.T.);
#30620=ADVANCED_FACE('',(#5292),#28887,.T.);
#30621=ADVANCED_FACE('',(#5293),#28888,.T.);
#30622=ADVANCED_FACE('',(#5294),#28889,.T.);
#30623=ADVANCED_FACE('',(#5295),#28890,.T.);
#30624=ADVANCED_FACE('',(#5296),#28891,.T.);
#30625=ADVANCED_FACE('',(#5297),#2078,.T.);
#30626=ADVANCED_FACE('',(#5298),#2079,.T.);
#30627=ADVANCED_FACE('',(#5299),#1020,.T.);
#30628=ADVANCED_FACE('',(#5300,#3575),#28892,.T.);
#30629=ADVANCED_FACE('',(#5301),#2080,.T.);
#30630=ADVANCED_FACE('',(#5302),#28893,.T.);
#30631=ADVANCED_FACE('',(#5303),#1021,.T.);
#30632=ADVANCED_FACE('',(#5304),#1022,.T.);
#30633=ADVANCED_FACE('',(#5305),#1023,.T.);
#30634=ADVANCED_FACE('',(#5306),#1024,.T.);
#30635=ADVANCED_FACE('',(#5307),#1025,.T.);
#30636=ADVANCED_FACE('',(#5308),#1026,.T.);
#30637=ADVANCED_FACE('',(#5309),#1027,.T.);
#30638=ADVANCED_FACE('',(#5310),#1028,.T.);
#30639=ADVANCED_FACE('',(#5311),#1029,.T.);
#30640=ADVANCED_FACE('',(#5312),#1030,.T.);
#30641=ADVANCED_FACE('',(#5313),#1031,.T.);
#30642=ADVANCED_FACE('',(#5314),#1032,.T.);
#30643=ADVANCED_FACE('',(#5315),#1033,.T.);
#30644=ADVANCED_FACE('',(#5316),#28894,.F.);
#30645=ADVANCED_FACE('',(#5317),#431,.F.);
#30646=ADVANCED_FACE('',(#5318),#28895,.T.);
#30647=ADVANCED_FACE('',(#5319),#1034,.T.);
#30648=ADVANCED_FACE('',(#5320),#432,.F.);
#30649=ADVANCED_FACE('',(#5321),#28896,.F.);
#30650=ADVANCED_FACE('',(#5322),#28897,.F.);
#30651=ADVANCED_FACE('',(#5323),#28898,.F.);
#30652=ADVANCED_FACE('',(#5324),#28899,.F.);
#30653=ADVANCED_FACE('',(#5325),#28900,.F.);
#30654=ADVANCED_FACE('',(#5326),#28901,.F.);
#30655=ADVANCED_FACE('',(#5327),#28902,.F.);
#30656=ADVANCED_FACE('',(#5328),#28903,.T.);
#30657=ADVANCED_FACE('',(#5329),#2081,.T.);
#30658=ADVANCED_FACE('',(#5330),#1035,.T.);
#30659=ADVANCED_FACE('',(#5331),#2082,.T.);
#30660=ADVANCED_FACE('',(#5332,#3576),#28904,.T.);
#30661=CLOSED_SHELL('',(#28905,#28906,#28907,#28908,#28909,#28910,#28911,
#28912,#28913,#28914,#28915,#28916,#28917,#28918,#28919,#28920,#28921,#28922,
#28923,#28924,#28925,#28926,#28927,#28928,#28929,#28930,#28931,#28932,#28933,
#28934,#28935,#28936,#28937,#28938,#28939,#28940,#28941,#28942,#28943,#28944,
#28945,#28946,#28947,#28948,#28949,#28950,#28951,#28952,#28953,#28954,#28955,
#28956,#28957,#28958,#28959,#28960,#28961,#28962,#28963,#28964,#28965,#28966,
#28967,#28968,#28969,#28970,#28971,#28972,#28973,#28974,#28975,#28976,#28977,
#28978,#28979,#28980,#28981,#28982,#28983,#28984,#28985,#28986,#28987,#28988,
#28989,#28990,#28991,#28992,#28993,#28994,#28995,#28996,#28997,#28998,#28999,
#29000,#29001,#29002,#29003,#29004,#29005,#29006,#29007,#29008,#29009,#29010,
#29011,#29012,#29013,#29014,#29015,#29016,#29017,#29018,#29019,#29020,#29021,
#29022,#29023,#29024,#29025,#29026,#29027,#29028,#29029,#29030,#29031,#29032,
#29033,#29034,#29035,#29036,#29037,#29038,#29039,#29040,#29041,#29042,#29043,
#29044,#29045,#29046,#29047,#29048,#29049,#29050,#29051,#29052,#29053,#29054,
#29055,#29056,#29057,#29058,#29059,#29060,#29061,#29062,#29063,#29064,#29065,
#29066,#29067,#29068,#29069,#29070,#29071,#29072,#29073,#29074,#29075,#29076,
#29077,#29078,#29079,#29080,#29081,#29082,#29083,#29084,#29085,#29086,#29087,
#29088,#29089,#29090,#29091,#29092,#29093,#29094,#29095,#29096,#29097,#29098,
#29099,#29100,#29101,#29102,#29103,#29104,#29105,#29106,#29107,#29108,#29109,
#29110,#29111,#29112,#29113,#29114,#29115,#29116,#29117,#29118,#29119,#29120,
#29121,#29122,#29123,#29124,#29125,#29126,#29127,#29128,#29129,#29130,#29131,
#29132,#29133,#29134,#29135,#29136,#29137,#29138,#29139,#29140,#29141,#29142,
#29143,#29144,#29145,#29146,#29147,#29148,#29149,#29150,#29151,#29152,#29153,
#29154,#29155,#29156,#29157,#29158,#29159,#29160,#29161,#29162,#29163,#29164,
#29165,#29166,#29167,#29168,#29169));
#30662=CLOSED_SHELL('',(#29170,#29171,#29172,#29173,#29174,#29175,#29176,
#29177,#29178,#29179,#29180,#29181,#29182,#29183,#29184,#29185,#29186,#29187,
#29188,#29189,#29190,#29191,#29192,#29193,#29194,#29195,#29196,#29197,#29198,
#29199,#29200,#29201,#29202,#29203,#29204,#29205,#29206,#29207,#29208,#29209,
#29210,#29211,#29212,#29213,#29214,#29215,#29216,#29217,#29218,#29219,#29220,
#29221,#29222,#29223,#29224,#29225,#29226,#29227,#29228,#29229,#29230,#29231,
#29232,#29233,#29234,#29235,#29236,#29237,#29238,#29239,#29240,#29241,#29242,
#29243,#29244,#29245,#29246,#29247,#29248,#29249,#29250,#29251,#29252,#29253,
#29254,#29255,#29256,#29257,#29258,#29259,#29260,#29261,#29262,#29263,#29264,
#29265,#29266,#29267,#29268,#29269,#29270,#29271,#29272,#29273,#29274,#29275,
#29276,#29277,#29278,#29279,#29280,#29281,#29282));
#30663=CLOSED_SHELL('',(#29283,#29284,#29285,#29286,#29287,#29288,#29289,
#29290,#29291,#29292,#29293,#29294,#29295,#29296,#29297,#29298,#29299,#29300,
#29301,#29302,#29303,#29304,#29305,#29306,#29307,#29308,#29309,#29310,#29311,
#29312,#29313,#29314,#29315,#29316,#29317,#29318,#29319,#29320,#29321,#29322,
#29323,#29324,#29325,#29326,#29327,#29328,#29329,#29330,#29331,#29332,#29333,
#29334,#29335,#29336,#29337,#29338,#29339,#29340,#29341,#29342,#29343,#29344,
#29345,#29346,#29347,#29348,#29349,#29350,#29351,#29352,#29353,#29354,#29355,
#29356,#29357,#29358,#29359,#29360,#29361,#29362,#29363,#29364,#29365,#29366,
#29367,#29368,#29369,#29370,#29371,#29372,#29373,#29374,#29375,#29376,#29377,
#29378,#29379,#29380,#29381,#29382,#29383,#29384,#29385,#29386,#29387,#29388,
#29389,#29390,#29391,#29392,#29393,#29394,#29395,#29396,#29397,#29398,#29399,
#29400,#29401,#29402,#29403,#29404,#29405,#29406,#29407,#29408,#29409,#29410,
#29411,#29412,#29413,#29414,#29415,#29416,#29417,#29418,#29419,#29420,#29421,
#29422,#29423,#29424,#29425,#29426,#29427,#29428,#29429,#29430,#29431,#29432,
#29433,#29434,#29435,#29436,#29437,#29438,#29439,#29440,#29441,#29442,#29443,
#29444,#29445,#29446,#29447,#29448,#29449,#29450,#29451,#29452,#29453,#29454,
#29455,#29456,#29457,#29458,#29459,#29460,#29461,#29462,#29463,#29464));
#30664=CLOSED_SHELL('',(#29465,#29466,#29467,#29468,#29469,#29470,#29471,
#29472,#29473,#29474,#29475,#29476,#29477,#29478,#29479,#29480,#29481,#29482,
#29483,#29484,#29485,#29486,#29487,#29488,#29489,#29490,#29491,#29492,#29493,
#29494,#29495,#29496,#29497,#29498,#29499,#29500));
#30665=CLOSED_SHELL('',(#29501,#29502,#29503,#29504,#29505,#29506,#29507,
#29508,#29509));
#30666=CLOSED_SHELL('',(#29510,#29511,#29512,#29513,#29514,#29515,#29516,
#29517,#29518,#29519,#29520,#29521,#29522,#29523,#29524,#29525,#29526,#29527,
#29528,#29529,#29530,#29531,#29532,#29533,#29534,#29535,#29536,#29537,#29538,
#29539,#29540,#29541,#29542,#29543,#29544,#29545,#29546,#29547,#29548,#29549,
#29550,#29551,#29552,#29553,#29554,#29555,#29556,#29557,#29558,#29559,#29560,
#29561,#29562,#29563,#29564,#29565,#29566,#29567,#29568,#29569,#29570,#29571,
#29572,#29573,#29574,#29575,#29576,#29577,#29578,#29579,#29580,#29581,#29582,
#29583,#29584,#29585,#29586,#29587,#29588,#29589,#29590,#29591,#29592,#29593,
#29594,#29595,#29596,#29597,#29598,#29599,#29600,#29601,#29602,#29603,#29604,
#29605,#29606,#29607,#29608,#29609,#29610,#29611,#29612,#29613,#29614,#29615,
#29616,#29617,#29618,#29619,#29620,#29621,#29622,#29623,#29624,#29625,#29626,
#29627,#29628,#29629,#29630,#29631,#29632,#29633,#29634,#29635,#29636,#29637,
#29638,#29639,#29640,#29641,#29642,#29643,#29644,#29645,#29646,#29647,#29648,
#29649,#29650,#29651,#29652,#29653,#29654,#29655,#29656,#29657,#29658,#29659,
#29660,#29661,#29662,#29663,#29664,#29665,#29666,#29667,#29668,#29669,#29670,
#29671,#29672,#29673,#29674,#29675,#29676,#29677,#29678,#29679,#29680,#29681,
#29682,#29683,#29684,#29685,#29686,#29687,#29688,#29689,#29690,#29691,#29692,
#29693,#29694,#29695,#29696,#29697,#29698));
#30667=CLOSED_SHELL('',(#29699,#29700,#29701,#29702));
#30668=CLOSED_SHELL('',(#29703));
#30669=CLOSED_SHELL('',(#29704,#29705,#29706,#29707,#29708));
#30670=CLOSED_SHELL('',(#29709,#29710,#29711));
#30671=CLOSED_SHELL('',(#29712,#29713,#29714,#29715,#29716,#29717));
#30672=CLOSED_SHELL('',(#29718,#29719,#29720,#29721,#29722,#29723,#29724,
#29725,#29726,#29727,#29728,#29729,#29730,#29731,#29732,#29733,#29734,#29735,
#29736,#29737,#29738,#29739,#29740,#29741,#29742,#29743,#29744,#29745,#29746,
#29747,#29748,#29749,#29750,#29751,#29752,#29753,#29754,#29755,#29756,#29757,
#29758,#29759,#29760,#29761,#29762,#29763,#29764,#29765,#29766,#29767,#29768,
#29769,#29770,#29771,#29772,#29773,#29774,#29775,#29776,#29777,#29778,#29779,
#29780,#29781,#29782,#29783,#29784,#29785,#29786,#29787,#29788,#29789,#29790,
#29791,#29792,#29793,#29794,#29795,#29796,#29797,#29798,#29799,#29800,#29801,
#29802,#29803,#29804,#29805,#29806,#29807,#29808,#29809,#29810,#29811,#29812,
#29813,#29814,#29815,#29816,#29817,#29818,#29819,#29820,#29821,#29822,#29823,
#29824,#29825,#29826,#29827,#29828,#29829,#29830,#29831,#29832,#29833,#29834,
#29835,#29836,#29837,#29838,#29839,#29840,#29841,#29842,#29843,#29844,#29845,
#29846,#29847,#29848,#29849,#29850,#29851,#29852,#29853,#29854,#29855,#29856,
#29857,#29858,#29859,#29860,#29861,#29862,#29863,#29864,#29865,#29866,#29867,
#29868,#29869,#29870,#29871,#29872,#29873,#29874,#29875,#29876,#29877,#29878,
#29879,#29880,#29881,#29882,#29883,#29884,#29885,#29886,#29887,#29888,#29889,
#29890,#29891,#29892,#29893,#29894,#29895,#29896,#29897,#29898,#29899,#29900,
#29901,#29902,#29903,#29904,#29905,#29906,#29907,#29908,#29909,#29910,#29911,
#29912,#29913,#29914,#29915,#29916,#29917,#29918,#29919,#29920,#29921,#29922,
#29923,#29924,#29925,#29926,#29927,#29928,#29929,#29930,#29931,#29932,#29933,
#29934,#29935,#29936,#29937,#29938,#29939,#29940,#29941,#29942,#29943,#29944,
#29945,#29946,#29947,#29948,#29949,#29950,#29951,#29952,#29953,#29954,#29955,
#29956,#29957,#29958,#29959,#29960,#29961,#29962,#29963,#29964,#29965,#29966));
#30673=CLOSED_SHELL('',(#29967,#29968,#29969,#29970,#29971));
#30674=CLOSED_SHELL('',(#29972,#29973,#29974,#29975,#29976,#29977,#29978,
#29979,#29980,#29981,#29982,#29983,#29984,#29985,#29986,#29987,#29988,#29989,
#29990,#29991,#29992,#29993,#29994,#29995,#29996,#29997,#29998,#29999,#30000,
#30001,#30002,#30003,#30004,#30005,#30006,#30007,#30008,#30009,#30010,#30011,
#30012,#30013,#30014,#30015,#30016,#30017,#30018,#30019,#30020,#30021,#30022,
#30023,#30024,#30025,#30026,#30027,#30028,#30029,#30030,#30031,#30032,#30033,
#30034,#30035,#30036,#30037,#30038,#30039,#30040,#30041,#30042,#30043,#30044,
#30045,#30046,#30047,#30048,#30049,#30050,#30051,#30052,#30053,#30054,#30055,
#30056,#30057,#30058,#30059,#30060,#30061,#30062,#30063,#30064,#30065,#30066,
#30067,#30068,#30069,#30070,#30071,#30072,#30073,#30074,#30075,#30076,#30077,
#30078,#30079,#30080,#30081,#30082,#30083,#30084,#30085,#30086,#30087,#30088,
#30089,#30090,#30091,#30092,#30093,#30094,#30095,#30096,#30097,#30098,#30099,
#30100,#30101,#30102,#30103,#30104,#30105,#30106,#30107,#30108,#30109,#30110,
#30111,#30112,#30113,#30114,#30115,#30116,#30117,#30118,#30119,#30120,#30121,
#30122,#30123,#30124,#30125,#30126,#30127,#30128,#30129,#30130,#30131,#30132,
#30133,#30134,#30135,#30136,#30137,#30138,#30139,#30140,#30141,#30142,#30143,
#30144,#30145,#30146,#30147,#30148,#30149,#30150,#30151,#30152,#30153,#30154,
#30155,#30156,#30157,#30158,#30159,#30160,#30161,#30162,#30163,#30164,#30165,
#30166,#30167,#30168,#30169,#30170,#30171,#30172,#30173,#30174,#30175,#30176,
#30177,#30178,#30179,#30180,#30181,#30182,#30183,#30184,#30185,#30186,#30187,
#30188,#30189,#30190,#30191,#30192,#30193,#30194,#30195,#30196,#30197,#30198,
#30199,#30200,#30201,#30202,#30203,#30204,#30205,#30206,#30207,#30208,#30209,
#30210,#30211,#30212,#30213,#30214,#30215,#30216,#30217,#30218,#30219,#30220,
#30221,#30222,#30223,#30224,#30225,#30226,#30227,#30228,#30229,#30230,#30231,
#30232,#30233,#30234,#30235,#30236,#30237,#30238,#30239,#30240,#30241,#30242,
#30243,#30244,#30245,#30246,#30247,#30248,#30249,#30250,#30251,#30252,#30253,
#30254,#30255,#30256,#30257,#30258,#30259,#30260,#30261,#30262,#30263,#30264,
#30265,#30266,#30267,#30268,#30269,#30270,#30271,#30272,#30273,#30274));
#30675=CLOSED_SHELL('',(#30275,#30276,#30277,#30278,#30279,#30280,#30281,
#30282,#30283,#30284,#30285,#30286,#30287,#30288,#30289,#30290,#30291,#30292,
#30293,#30294,#30295,#30296,#30297,#30298,#30299,#30300,#30301,#30302,#30303,
#30304,#30305,#30306,#30307,#30308,#30309,#30310,#30311,#30312,#30313,#30314,
#30315,#30316,#30317));
#30676=CLOSED_SHELL('',(#30318,#30319,#30320,#30321,#30322,#30323,#30324,
#30325,#30326,#30327,#30328,#30329,#30330,#30331,#30332,#30333,#30334,#30335,
#30336,#30337,#30338,#30339,#30340,#30341,#30342,#30343,#30344,#30345,#30346,
#30347,#30348,#30349,#30350,#30351,#30352,#30353,#30354,#30355,#30356,#30357,
#30358,#30359,#30360,#30361,#30362,#30363,#30364,#30365,#30366,#30367,#30368,
#30369,#30370,#30371));
#30677=CLOSED_SHELL('',(#30372,#30373,#30374,#30375,#30376,#30377,#30378,
#30379,#30380,#30381,#30382,#30383,#30384,#30385,#30386,#30387,#30388,#30389,
#30390,#30391,#30392,#30393,#30394,#30395,#30396,#30397,#30398,#30399,#30400,
#30401,#30402,#30403,#30404,#30405,#30406,#30407,#30408,#30409,#30410,#30411,
#30412,#30413,#30414,#30415,#30416,#30417,#30418,#30419,#30420,#30421,#30422,
#30423,#30424,#30425,#30426,#30427,#30428,#30429,#30430,#30431,#30432,#30433,
#30434,#30435,#30436,#30437,#30438,#30439,#30440,#30441,#30442,#30443,#30444,
#30445,#30446,#30447,#30448,#30449,#30450,#30451,#30452,#30453,#30454,#30455,
#30456,#30457,#30458,#30459,#30460,#30461,#30462,#30463,#30464,#30465,#30466,
#30467,#30468,#30469,#30470,#30471,#30472,#30473,#30474,#30475,#30476,#30477,
#30478,#30479,#30480,#30481,#30482,#30483,#30484,#30485,#30486,#30487,#30488,
#30489,#30490,#30491,#30492,#30493,#30494,#30495,#30496,#30497,#30498,#30499,
#30500,#30501,#30502,#30503,#30504,#30505,#30506,#30507,#30508,#30509,#30510,
#30511,#30512,#30513,#30514,#30515,#30516,#30517,#30518,#30519,#30520,#30521,
#30522,#30523,#30524,#30525,#30526,#30527,#30528,#30529,#30530,#30531,#30532));
#30678=CLOSED_SHELL('',(#30533,#30534,#30535,#30536,#30537,#30538,#30539,
#30540,#30541,#30542,#30543,#30544,#30545,#30546,#30547,#30548,#30549,#30550,
#30551,#30552,#30553,#30554,#30555,#30556,#30557,#30558,#30559,#30560,#30561,
#30562,#30563,#30564,#30565,#30566,#30567,#30568,#30569,#30570,#30571,#30572,
#30573,#30574,#30575,#30576,#30577,#30578,#30579,#30580,#30581,#30582,#30583,
#30584,#30585,#30586,#30587,#30588,#30589,#30590,#30591,#30592,#30593,#30594,
#30595,#30596,#30597,#30598,#30599,#30600,#30601,#30602,#30603,#30604,#30605,
#30606,#30607,#30608,#30609,#30610,#30611,#30612,#30613,#30614,#30615,#30616,
#30617,#30618,#30619,#30620,#30621,#30622,#30623,#30624,#30625,#30626,#30627,
#30628,#30629,#30630));
#30679=CLOSED_SHELL('',(#30631,#30632,#30633,#30634,#30635,#30636,#30637,
#30638,#30639,#30640,#30641,#30642,#30643,#30644,#30645,#30646,#30647,#30648,
#30649,#30650,#30651,#30652,#30653,#30654,#30655,#30656,#30657,#30658,#30659,
#30660));
#30680=DERIVED_UNIT_ELEMENT(#30718,1.);
#30681=DERIVED_UNIT_ELEMENT(#82386,-3.);
#30682=DERIVED_UNIT_ELEMENT(#30718,1.);
#30683=DERIVED_UNIT_ELEMENT(#82386,-3.);
#30684=DERIVED_UNIT_ELEMENT(#30718,1.);
#30685=DERIVED_UNIT_ELEMENT(#82386,-3.);
#30686=DERIVED_UNIT_ELEMENT(#30718,1.);
#30687=DERIVED_UNIT_ELEMENT(#82386,-3.);
#30688=DERIVED_UNIT_ELEMENT(#30718,1.);
#30689=DERIVED_UNIT_ELEMENT(#82386,-3.);
#30690=DERIVED_UNIT_ELEMENT(#30718,1.);
#30691=DERIVED_UNIT_ELEMENT(#82386,-3.);
#30692=DERIVED_UNIT_ELEMENT(#30718,1.);
#30693=DERIVED_UNIT_ELEMENT(#82386,-3.);
#30694=DERIVED_UNIT_ELEMENT(#30718,1.);
#30695=DERIVED_UNIT_ELEMENT(#82386,-3.);
#30696=DERIVED_UNIT_ELEMENT(#30718,1.);
#30697=DERIVED_UNIT_ELEMENT(#82386,-3.);
#30698=DERIVED_UNIT_ELEMENT(#30718,1.);
#30699=DERIVED_UNIT_ELEMENT(#82386,-3.);
#30700=DERIVED_UNIT_ELEMENT(#30718,1.);
#30701=DERIVED_UNIT_ELEMENT(#82386,-3.);
#30702=DERIVED_UNIT_ELEMENT(#30718,1.);
#30703=DERIVED_UNIT_ELEMENT(#82386,-3.);
#30704=DERIVED_UNIT_ELEMENT(#30718,1.);
#30705=DERIVED_UNIT_ELEMENT(#82386,-3.);
#30706=DERIVED_UNIT_ELEMENT(#30718,1.);
#30707=DERIVED_UNIT_ELEMENT(#82386,-3.);
#30708=DERIVED_UNIT_ELEMENT(#30718,1.);
#30709=DERIVED_UNIT_ELEMENT(#82386,-3.);
#30710=DERIVED_UNIT_ELEMENT(#30718,1.);
#30711=DERIVED_UNIT_ELEMENT(#82386,-3.);
#30712=DERIVED_UNIT_ELEMENT(#30718,1.);
#30713=DERIVED_UNIT_ELEMENT(#82386,-3.);
#30714=DERIVED_UNIT_ELEMENT(#30718,1.);
#30715=DERIVED_UNIT_ELEMENT(#82386,-3.);
#30716=DERIVED_UNIT_ELEMENT(#30718,1.);
#30717=DERIVED_UNIT_ELEMENT(#82386,-3.);
#30718=(
MASS_UNIT()
NAMED_UNIT(*)
SI_UNIT(.KILO.,.GRAM.)
);
#30719=DERIVED_UNIT((#30680,#30681));
#30720=DERIVED_UNIT((#30682,#30683));
#30721=DERIVED_UNIT((#30684,#30685));
#30722=DERIVED_UNIT((#30686,#30687));
#30723=DERIVED_UNIT((#30688,#30689));
#30724=DERIVED_UNIT((#30690,#30691));
#30725=DERIVED_UNIT((#30692,#30693));
#30726=DERIVED_UNIT((#30694,#30695));
#30727=DERIVED_UNIT((#30696,#30697));
#30728=DERIVED_UNIT((#30698,#30699));
#30729=DERIVED_UNIT((#30700,#30701));
#30730=DERIVED_UNIT((#30702,#30703));
#30731=DERIVED_UNIT((#30704,#30705));
#30732=DERIVED_UNIT((#30706,#30707));
#30733=DERIVED_UNIT((#30708,#30709));
#30734=DERIVED_UNIT((#30710,#30711));
#30735=DERIVED_UNIT((#30712,#30713));
#30736=DERIVED_UNIT((#30714,#30715));
#30737=DERIVED_UNIT((#30716,#30717));
#30738=MEASURE_REPRESENTATION_ITEM('density measure',
POSITIVE_RATIO_MEASURE(7850.),#30719);
#30739=MEASURE_REPRESENTATION_ITEM('density measure',
POSITIVE_RATIO_MEASURE(7850.),#30720);
#30740=MEASURE_REPRESENTATION_ITEM('density measure',
POSITIVE_RATIO_MEASURE(7850.),#30721);
#30741=MEASURE_REPRESENTATION_ITEM('density measure',
POSITIVE_RATIO_MEASURE(7850.),#30722);
#30742=MEASURE_REPRESENTATION_ITEM('density measure',
POSITIVE_RATIO_MEASURE(7850.),#30723);
#30743=MEASURE_REPRESENTATION_ITEM('density measure',
POSITIVE_RATIO_MEASURE(7850.),#30724);
#30744=MEASURE_REPRESENTATION_ITEM('density measure',
POSITIVE_RATIO_MEASURE(7850.),#30725);
#30745=MEASURE_REPRESENTATION_ITEM('density measure',
POSITIVE_RATIO_MEASURE(7850.),#30726);
#30746=MEASURE_REPRESENTATION_ITEM('density measure',
POSITIVE_RATIO_MEASURE(7850.),#30727);
#30747=MEASURE_REPRESENTATION_ITEM('density measure',
POSITIVE_RATIO_MEASURE(7850.),#30728);
#30748=MEASURE_REPRESENTATION_ITEM('density measure',
POSITIVE_RATIO_MEASURE(7850.),#30729);
#30749=MEASURE_REPRESENTATION_ITEM('density measure',
POSITIVE_RATIO_MEASURE(7850.),#30730);
#30750=MEASURE_REPRESENTATION_ITEM('density measure',
POSITIVE_RATIO_MEASURE(7850.),#30731);
#30751=MEASURE_REPRESENTATION_ITEM('density measure',
POSITIVE_RATIO_MEASURE(7850.),#30732);
#30752=MEASURE_REPRESENTATION_ITEM('density measure',
POSITIVE_RATIO_MEASURE(7850.),#30733);
#30753=MEASURE_REPRESENTATION_ITEM('density measure',
POSITIVE_RATIO_MEASURE(7850.),#30734);
#30754=MEASURE_REPRESENTATION_ITEM('density measure',
POSITIVE_RATIO_MEASURE(7850.),#30735);
#30755=MEASURE_REPRESENTATION_ITEM('density measure',
POSITIVE_RATIO_MEASURE(7850.),#30736);
#30756=MEASURE_REPRESENTATION_ITEM('density measure',
POSITIVE_RATIO_MEASURE(7850.),#30737);
#30757=PROPERTY_DEFINITION_REPRESENTATION(#30852,#30795);
#30758=PROPERTY_DEFINITION_REPRESENTATION(#30853,#30796);
#30759=PROPERTY_DEFINITION_REPRESENTATION(#30854,#30797);
#30760=PROPERTY_DEFINITION_REPRESENTATION(#30855,#30798);
#30761=PROPERTY_DEFINITION_REPRESENTATION(#30856,#30799);
#30762=PROPERTY_DEFINITION_REPRESENTATION(#30857,#30800);
#30763=PROPERTY_DEFINITION_REPRESENTATION(#30858,#30801);
#30764=PROPERTY_DEFINITION_REPRESENTATION(#30859,#30802);
#30765=PROPERTY_DEFINITION_REPRESENTATION(#30860,#30803);
#30766=PROPERTY_DEFINITION_REPRESENTATION(#30861,#30804);
#30767=PROPERTY_DEFINITION_REPRESENTATION(#30862,#30805);
#30768=PROPERTY_DEFINITION_REPRESENTATION(#30863,#30806);
#30769=PROPERTY_DEFINITION_REPRESENTATION(#30864,#30807);
#30770=PROPERTY_DEFINITION_REPRESENTATION(#30865,#30808);
#30771=PROPERTY_DEFINITION_REPRESENTATION(#30866,#30809);
#30772=PROPERTY_DEFINITION_REPRESENTATION(#30867,#30810);
#30773=PROPERTY_DEFINITION_REPRESENTATION(#30868,#30811);
#30774=PROPERTY_DEFINITION_REPRESENTATION(#30869,#30812);
#30775=PROPERTY_DEFINITION_REPRESENTATION(#30870,#30813);
#30776=PROPERTY_DEFINITION_REPRESENTATION(#30871,#30814);
#30777=PROPERTY_DEFINITION_REPRESENTATION(#30872,#30815);
#30778=PROPERTY_DEFINITION_REPRESENTATION(#30873,#30816);
#30779=PROPERTY_DEFINITION_REPRESENTATION(#30874,#30817);
#30780=PROPERTY_DEFINITION_REPRESENTATION(#30875,#30818);
#30781=PROPERTY_DEFINITION_REPRESENTATION(#30876,#30819);
#30782=PROPERTY_DEFINITION_REPRESENTATION(#30877,#30820);
#30783=PROPERTY_DEFINITION_REPRESENTATION(#30878,#30821);
#30784=PROPERTY_DEFINITION_REPRESENTATION(#30879,#30822);
#30785=PROPERTY_DEFINITION_REPRESENTATION(#30880,#30823);
#30786=PROPERTY_DEFINITION_REPRESENTATION(#30881,#30824);
#30787=PROPERTY_DEFINITION_REPRESENTATION(#30882,#30825);
#30788=PROPERTY_DEFINITION_REPRESENTATION(#30883,#30826);
#30789=PROPERTY_DEFINITION_REPRESENTATION(#30884,#30827);
#30790=PROPERTY_DEFINITION_REPRESENTATION(#30885,#30828);
#30791=PROPERTY_DEFINITION_REPRESENTATION(#30886,#30829);
#30792=PROPERTY_DEFINITION_REPRESENTATION(#30887,#30830);
#30793=PROPERTY_DEFINITION_REPRESENTATION(#30888,#30831);
#30794=PROPERTY_DEFINITION_REPRESENTATION(#30889,#30832);
#30795=REPRESENTATION('material name',(#30833),#82365);
#30796=REPRESENTATION('density',(#30738),#82365);
#30797=REPRESENTATION('material name',(#30834),#82366);
#30798=REPRESENTATION('density',(#30739),#82366);
#30799=REPRESENTATION('material name',(#30835),#82367);
#30800=REPRESENTATION('density',(#30740),#82367);
#30801=REPRESENTATION('material name',(#30836),#82368);
#30802=REPRESENTATION('density',(#30741),#82368);
#30803=REPRESENTATION('material name',(#30837),#82369);
#30804=REPRESENTATION('density',(#30742),#82369);
#30805=REPRESENTATION('material name',(#30838),#82370);
#30806=REPRESENTATION('density',(#30743),#82370);
#30807=REPRESENTATION('material name',(#30839),#82371);
#30808=REPRESENTATION('density',(#30744),#82371);
#30809=REPRESENTATION('material name',(#30840),#82372);
#30810=REPRESENTATION('density',(#30745),#82372);
#30811=REPRESENTATION('material name',(#30841),#82373);
#30812=REPRESENTATION('density',(#30746),#82373);
#30813=REPRESENTATION('material name',(#30842),#82374);
#30814=REPRESENTATION('density',(#30747),#82374);
#30815=REPRESENTATION('material name',(#30843),#82375);
#30816=REPRESENTATION('density',(#30748),#82375);
#30817=REPRESENTATION('material name',(#30844),#82376);
#30818=REPRESENTATION('density',(#30749),#82376);
#30819=REPRESENTATION('material name',(#30845),#82377);
#30820=REPRESENTATION('density',(#30750),#82377);
#30821=REPRESENTATION('material name',(#30846),#82378);
#30822=REPRESENTATION('density',(#30751),#82378);
#30823=REPRESENTATION('material name',(#30847),#82379);
#30824=REPRESENTATION('density',(#30752),#82379);
#30825=REPRESENTATION('material name',(#30848),#82380);
#30826=REPRESENTATION('density',(#30753),#82380);
#30827=REPRESENTATION('material name',(#30849),#82381);
#30828=REPRESENTATION('density',(#30754),#82381);
#30829=REPRESENTATION('material name',(#30850),#82382);
#30830=REPRESENTATION('density',(#30755),#82382);
#30831=REPRESENTATION('material name',(#30851),#82383);
#30832=REPRESENTATION('density',(#30756),#82383);
#30833=DESCRIPTIVE_REPRESENTATION_ITEM('Steel','Steel');
#30834=DESCRIPTIVE_REPRESENTATION_ITEM('Steel','Steel');
#30835=DESCRIPTIVE_REPRESENTATION_ITEM('Steel','Steel');
#30836=DESCRIPTIVE_REPRESENTATION_ITEM('Steel','Steel');
#30837=DESCRIPTIVE_REPRESENTATION_ITEM('Steel','Steel');
#30838=DESCRIPTIVE_REPRESENTATION_ITEM('Steel','Steel');
#30839=DESCRIPTIVE_REPRESENTATION_ITEM('Steel','Steel');
#30840=DESCRIPTIVE_REPRESENTATION_ITEM('Steel','Steel');
#30841=DESCRIPTIVE_REPRESENTATION_ITEM('Steel','Steel');
#30842=DESCRIPTIVE_REPRESENTATION_ITEM('Steel','Steel');
#30843=DESCRIPTIVE_REPRESENTATION_ITEM('Steel','Steel');
#30844=DESCRIPTIVE_REPRESENTATION_ITEM('Steel','Steel');
#30845=DESCRIPTIVE_REPRESENTATION_ITEM('Steel','Steel');
#30846=DESCRIPTIVE_REPRESENTATION_ITEM('Steel','Steel');
#30847=DESCRIPTIVE_REPRESENTATION_ITEM('Steel','Steel');
#30848=DESCRIPTIVE_REPRESENTATION_ITEM('Steel','Steel');
#30849=DESCRIPTIVE_REPRESENTATION_ITEM('Steel','Steel');
#30850=DESCRIPTIVE_REPRESENTATION_ITEM('Steel','Steel');
#30851=DESCRIPTIVE_REPRESENTATION_ITEM('Steel','Steel');
#30852=PROPERTY_DEFINITION('material property','material name',#82487);
#30853=PROPERTY_DEFINITION('material property','density of part',#82487);
#30854=PROPERTY_DEFINITION('material property','material name',#82488);
#30855=PROPERTY_DEFINITION('material property','density of part',#82488);
#30856=PROPERTY_DEFINITION('material property','material name',#82489);
#30857=PROPERTY_DEFINITION('material property','density of part',#82489);
#30858=PROPERTY_DEFINITION('material property','material name',#82490);
#30859=PROPERTY_DEFINITION('material property','density of part',#82490);
#30860=PROPERTY_DEFINITION('material property','material name',#82491);
#30861=PROPERTY_DEFINITION('material property','density of part',#82491);
#30862=PROPERTY_DEFINITION('material property','material name',#82492);
#30863=PROPERTY_DEFINITION('material property','density of part',#82492);
#30864=PROPERTY_DEFINITION('material property','material name',#82493);
#30865=PROPERTY_DEFINITION('material property','density of part',#82493);
#30866=PROPERTY_DEFINITION('material property','material name',#82494);
#30867=PROPERTY_DEFINITION('material property','density of part',#82494);
#30868=PROPERTY_DEFINITION('material property','material name',#82495);
#30869=PROPERTY_DEFINITION('material property','density of part',#82495);
#30870=PROPERTY_DEFINITION('material property','material name',#82496);
#30871=PROPERTY_DEFINITION('material property','density of part',#82496);
#30872=PROPERTY_DEFINITION('material property','material name',#82497);
#30873=PROPERTY_DEFINITION('material property','density of part',#82497);
#30874=PROPERTY_DEFINITION('material property','material name',#82498);
#30875=PROPERTY_DEFINITION('material property','density of part',#82498);
#30876=PROPERTY_DEFINITION('material property','material name',#82499);
#30877=PROPERTY_DEFINITION('material property','density of part',#82499);
#30878=PROPERTY_DEFINITION('material property','material name',#82500);
#30879=PROPERTY_DEFINITION('material property','density of part',#82500);
#30880=PROPERTY_DEFINITION('material property','material name',#82501);
#30881=PROPERTY_DEFINITION('material property','density of part',#82501);
#30882=PROPERTY_DEFINITION('material property','material name',#82502);
#30883=PROPERTY_DEFINITION('material property','density of part',#82502);
#30884=PROPERTY_DEFINITION('material property','material name',#82503);
#30885=PROPERTY_DEFINITION('material property','density of part',#82503);
#30886=PROPERTY_DEFINITION('material property','material name',#82504);
#30887=PROPERTY_DEFINITION('material property','density of part',#82504);
#30888=PROPERTY_DEFINITION('material property','material name',#82505);
#30889=PROPERTY_DEFINITION('material property','density of part',#82505);
#30890=AXIS2_PLACEMENT_3D('',#40765,#33413,#33414);
#30891=AXIS2_PLACEMENT_3D('',#40766,#33415,#33416);
#30892=AXIS2_PLACEMENT_3D('',#40767,#33417,#33418);
#30893=AXIS2_PLACEMENT_3D('',#40780,#33425,#33426);
#30894=AXIS2_PLACEMENT_3D('',#40786,#33430,#33431);
#30895=AXIS2_PLACEMENT_3D('',#40794,#33436,#33437);
#30896=AXIS2_PLACEMENT_3D('',#40800,#33441,#33442);
#30897=AXIS2_PLACEMENT_3D('',#40808,#33447,#33448);
#30898=AXIS2_PLACEMENT_3D('',#40814,#33452,#33453);
#30899=AXIS2_PLACEMENT_3D('',#40822,#33458,#33459);
#30900=AXIS2_PLACEMENT_3D('',#41362,#33510,#33511);
#30901=AXIS2_PLACEMENT_3D('',#41370,#33516,#33517);
#30902=AXIS2_PLACEMENT_3D('',#41376,#33521,#33522);
#30903=AXIS2_PLACEMENT_3D('',#41378,#33523,#33524);
#30904=AXIS2_PLACEMENT_3D('',#41381,#33526,#33527);
#30905=AXIS2_PLACEMENT_3D('',#41382,#33528,#33529);
#30906=AXIS2_PLACEMENT_3D('',#41391,#33534,#33535);
#30907=AXIS2_PLACEMENT_3D('',#41392,#33536,#33537);
#30908=AXIS2_PLACEMENT_3D('',#41395,#33539,#33540);
#30909=AXIS2_PLACEMENT_3D('',#41396,#33541,#33542);
#30910=AXIS2_PLACEMENT_3D('',#41399,#33544,#33545);
#30911=AXIS2_PLACEMENT_3D('',#41400,#33546,#33547);
#30912=AXIS2_PLACEMENT_3D('',#41403,#33549,#33550);
#30913=AXIS2_PLACEMENT_3D('',#41404,#33551,#33552);
#30914=AXIS2_PLACEMENT_3D('',#41406,#33553,#33554);
#30915=AXIS2_PLACEMENT_3D('',#41409,#33556,#33557);
#30916=AXIS2_PLACEMENT_3D('',#41410,#33558,#33559);
#30917=AXIS2_PLACEMENT_3D('',#41413,#33561,#33562);
#30918=AXIS2_PLACEMENT_3D('',#41414,#33563,#33564);
#30919=AXIS2_PLACEMENT_3D('',#41416,#33565,#33566);
#30920=AXIS2_PLACEMENT_3D('',#41417,#33567,#33568);
#30921=AXIS2_PLACEMENT_3D('',#41419,#33569,#33570);
#30922=AXIS2_PLACEMENT_3D('',#41422,#33572,#33573);
#30923=AXIS2_PLACEMENT_3D('',#41423,#33574,#33575);
#30924=AXIS2_PLACEMENT_3D('',#41426,#33577,#33578);
#30925=AXIS2_PLACEMENT_3D('',#41427,#33579,#33580);
#30926=AXIS2_PLACEMENT_3D('',#41429,#33581,#33582);
#30927=AXIS2_PLACEMENT_3D('',#41430,#33583,#33584);
#30928=AXIS2_PLACEMENT_3D('',#41432,#33585,#33586);
#30929=AXIS2_PLACEMENT_3D('',#41435,#33588,#33589);
#30930=AXIS2_PLACEMENT_3D('',#41436,#33590,#33591);
#30931=AXIS2_PLACEMENT_3D('',#41439,#33593,#33594);
#30932=AXIS2_PLACEMENT_3D('',#41440,#33595,#33596);
#30933=AXIS2_PLACEMENT_3D('',#41442,#33597,#33598);
#30934=AXIS2_PLACEMENT_3D('',#41443,#33599,#33600);
#30935=AXIS2_PLACEMENT_3D('',#41445,#33601,#33602);
#30936=AXIS2_PLACEMENT_3D('',#41448,#33604,#33605);
#30937=AXIS2_PLACEMENT_3D('',#41449,#33606,#33607);
#30938=AXIS2_PLACEMENT_3D('',#41452,#33609,#33610);
#30939=AXIS2_PLACEMENT_3D('',#41453,#33611,#33612);
#30940=AXIS2_PLACEMENT_3D('',#41455,#33613,#33614);
#30941=AXIS2_PLACEMENT_3D('',#41456,#33615,#33616);
#30942=AXIS2_PLACEMENT_3D('',#41460,#33619,#33620);
#30943=AXIS2_PLACEMENT_3D('',#41465,#33624,#33625);
#30944=AXIS2_PLACEMENT_3D('',#41469,#33628,#33629);
#30945=AXIS2_PLACEMENT_3D('',#41475,#33633,#33634);
#30946=AXIS2_PLACEMENT_3D('',#41482,#33638,#33639);
#30947=AXIS2_PLACEMENT_3D('',#41488,#33643,#33644);
#30948=AXIS2_PLACEMENT_3D('',#41491,#33647,#33648);
#30949=AXIS2_PLACEMENT_3D('',#41493,#33650,#33651);
#30950=AXIS2_PLACEMENT_3D('',#41495,#33653,#33654);
#30951=AXIS2_PLACEMENT_3D('',#41498,#33657,#33658);
#30952=AXIS2_PLACEMENT_3D('',#41501,#33661,#33662);
#30953=AXIS2_PLACEMENT_3D('',#41503,#33664,#33665);
#30954=AXIS2_PLACEMENT_3D('',#41506,#33668,#33669);
#30955=AXIS2_PLACEMENT_3D('',#41507,#33670,#33671);
#30956=AXIS2_PLACEMENT_3D('',#41509,#33672,#33673);
#30957=AXIS2_PLACEMENT_3D('',#41511,#33674,#33675);
#30958=AXIS2_PLACEMENT_3D('',#41513,#33676,#33677);
#30959=AXIS2_PLACEMENT_3D('',#41515,#33678,#33679);
#30960=AXIS2_PLACEMENT_3D('',#41517,#33680,#33681);
#30961=AXIS2_PLACEMENT_3D('',#41519,#33682,#33683);
#30962=AXIS2_PLACEMENT_3D('',#41521,#33684,#33685);
#30963=AXIS2_PLACEMENT_3D('',#41523,#33686,#33687);
#30964=AXIS2_PLACEMENT_3D('',#41525,#33688,#33689);
#30965=AXIS2_PLACEMENT_3D('',#41527,#33690,#33691);
#30966=AXIS2_PLACEMENT_3D('',#41529,#33692,#33693);
#30967=AXIS2_PLACEMENT_3D('',#41531,#33694,#33695);
#30968=AXIS2_PLACEMENT_3D('',#41533,#33696,#33697);
#30969=AXIS2_PLACEMENT_3D('',#41535,#33698,#33699);
#30970=AXIS2_PLACEMENT_3D('',#41537,#33700,#33701);
#30971=AXIS2_PLACEMENT_3D('',#41539,#33702,#33703);
#30972=AXIS2_PLACEMENT_3D('',#41541,#33704,#33705);
#30973=AXIS2_PLACEMENT_3D('',#41542,#33706,#33707);
#30974=AXIS2_PLACEMENT_3D('',#41543,#33708,#33709);
#30975=AXIS2_PLACEMENT_3D('',#41545,#33710,#33711);
#30976=AXIS2_PLACEMENT_3D('',#41547,#33712,#33713);
#30977=AXIS2_PLACEMENT_3D('',#41549,#33714,#33715);
#30978=AXIS2_PLACEMENT_3D('',#41551,#33716,#33717);
#30979=AXIS2_PLACEMENT_3D('',#41553,#33718,#33719);
#30980=AXIS2_PLACEMENT_3D('',#41554,#33720,#33721);
#30981=AXIS2_PLACEMENT_3D('',#41560,#33725,#33726);
#30982=AXIS2_PLACEMENT_3D('',#41564,#33729,#33730);
#30983=AXIS2_PLACEMENT_3D('',#41568,#33733,#33734);
#30984=AXIS2_PLACEMENT_3D('',#41572,#33737,#33738);
#30985=AXIS2_PLACEMENT_3D('',#41576,#33741,#33742);
#30986=AXIS2_PLACEMENT_3D('',#41580,#33745,#33746);
#30987=AXIS2_PLACEMENT_3D('',#41584,#33749,#33750);
#30988=AXIS2_PLACEMENT_3D('',#41588,#33753,#33754);
#30989=AXIS2_PLACEMENT_3D('',#41592,#33757,#33758);
#30990=AXIS2_PLACEMENT_3D('',#41596,#33761,#33762);
#30991=AXIS2_PLACEMENT_3D('',#41600,#33765,#33766);
#30992=AXIS2_PLACEMENT_3D('',#41602,#33768,#33769);
#30993=AXIS2_PLACEMENT_3D('',#41603,#33770,#33771);
#30994=AXIS2_PLACEMENT_3D('',#41653,#33779,#33780);
#30995=AXIS2_PLACEMENT_3D('',#41657,#33783,#33784);
#30996=AXIS2_PLACEMENT_3D('',#41661,#33787,#33788);
#30997=AXIS2_PLACEMENT_3D('',#41742,#33798,#33799);
#30998=AXIS2_PLACEMENT_3D('',#41746,#33802,#33803);
#30999=AXIS2_PLACEMENT_3D('',#41750,#33806,#33807);
#31000=AXIS2_PLACEMENT_3D('',#41754,#33810,#33811);
#31001=AXIS2_PLACEMENT_3D('',#41756,#33813,#33814);
#31002=AXIS2_PLACEMENT_3D('',#41757,#33815,#33816);
#31003=AXIS2_PLACEMENT_3D('',#41763,#33820,#33821);
#31004=AXIS2_PLACEMENT_3D('',#41767,#33824,#33825);
#31005=AXIS2_PLACEMENT_3D('',#41771,#33828,#33829);
#31006=AXIS2_PLACEMENT_3D('',#41775,#33832,#33833);
#31007=AXIS2_PLACEMENT_3D('',#41779,#33836,#33837);
#31008=AXIS2_PLACEMENT_3D('',#41783,#33840,#33841);
#31009=AXIS2_PLACEMENT_3D('',#41787,#33844,#33845);
#31010=AXIS2_PLACEMENT_3D('',#41791,#33848,#33849);
#31011=AXIS2_PLACEMENT_3D('',#41795,#33852,#33853);
#31012=AXIS2_PLACEMENT_3D('',#41799,#33856,#33857);
#31013=AXIS2_PLACEMENT_3D('',#41803,#33860,#33861);
#31014=AXIS2_PLACEMENT_3D('',#41805,#33863,#33864);
#31015=AXIS2_PLACEMENT_3D('',#41830,#33868,#33869);
#31016=AXIS2_PLACEMENT_3D('',#41867,#33875,#33876);
#31017=AXIS2_PLACEMENT_3D('',#41871,#33879,#33880);
#31018=AXIS2_PLACEMENT_3D('',#41875,#33883,#33884);
#31019=AXIS2_PLACEMENT_3D('',#41879,#33887,#33888);
#31020=AXIS2_PLACEMENT_3D('',#41892,#33891,#33892);
#31021=AXIS2_PLACEMENT_3D('',#42038,#33907,#33908);
#31022=AXIS2_PLACEMENT_3D('',#42240,#33929,#33930);
#31023=AXIS2_PLACEMENT_3D('',#42264,#33934,#33935);
#31024=AXIS2_PLACEMENT_3D('',#42388,#33948,#33949);
#31025=AXIS2_PLACEMENT_3D('',#42469,#33959,#33960);
#31026=AXIS2_PLACEMENT_3D('',#42550,#33970,#33971);
#31027=AXIS2_PLACEMENT_3D('',#42574,#33975,#33976);
#31028=AXIS2_PLACEMENT_3D('',#42575,#33977,#33978);
#31029=AXIS2_PLACEMENT_3D('',#42581,#33982,#33983);
#31030=AXIS2_PLACEMENT_3D('',#42585,#33986,#33987);
#31031=AXIS2_PLACEMENT_3D('',#42589,#33990,#33991);
#31032=AXIS2_PLACEMENT_3D('',#42591,#33993,#33994);
#31033=AXIS2_PLACEMENT_3D('',#42737,#34009,#34010);
#31034=AXIS2_PLACEMENT_3D('',#42939,#34031,#34032);
#31035=AXIS2_PLACEMENT_3D('',#42963,#34036,#34037);
#31036=AXIS2_PLACEMENT_3D('',#42964,#34038,#34039);
#31037=AXIS2_PLACEMENT_3D('',#42967,#34041,#34042);
#31038=AXIS2_PLACEMENT_3D('',#42968,#34043,#34044);
#31039=AXIS2_PLACEMENT_3D('',#42970,#34045,#34046);
#31040=AXIS2_PLACEMENT_3D('',#42972,#34048,#34049);
#31041=AXIS2_PLACEMENT_3D('',#42975,#34051,#34052);
#31042=AXIS2_PLACEMENT_3D('',#42976,#34053,#34054);
#31043=AXIS2_PLACEMENT_3D('',#42979,#34056,#34057);
#31044=AXIS2_PLACEMENT_3D('',#42980,#34058,#34059);
#31045=AXIS2_PLACEMENT_3D('',#42983,#34061,#34062);
#31046=AXIS2_PLACEMENT_3D('',#42984,#34063,#34064);
#31047=AXIS2_PLACEMENT_3D('',#42987,#34066,#34067);
#31048=AXIS2_PLACEMENT_3D('',#42988,#34068,#34069);
#31049=AXIS2_PLACEMENT_3D('',#42991,#34071,#34072);
#31050=AXIS2_PLACEMENT_3D('',#42992,#34073,#34074);
#31051=AXIS2_PLACEMENT_3D('',#42995,#34076,#34077);
#31052=AXIS2_PLACEMENT_3D('',#42996,#34078,#34079);
#31053=AXIS2_PLACEMENT_3D('',#42999,#34081,#34082);
#31054=AXIS2_PLACEMENT_3D('',#43000,#34083,#34084);
#31055=AXIS2_PLACEMENT_3D('',#43003,#34086,#34087);
#31056=AXIS2_PLACEMENT_3D('',#43004,#34088,#34089);
#31057=AXIS2_PLACEMENT_3D('',#43007,#34091,#34092);
#31058=AXIS2_PLACEMENT_3D('',#43008,#34093,#34094);
#31059=AXIS2_PLACEMENT_3D('',#43011,#34096,#34097);
#31060=AXIS2_PLACEMENT_3D('',#43012,#34098,#34099);
#31061=AXIS2_PLACEMENT_3D('',#43015,#34101,#34102);
#31062=AXIS2_PLACEMENT_3D('',#43016,#34103,#34104);
#31063=AXIS2_PLACEMENT_3D('',#43019,#34106,#34107);
#31064=AXIS2_PLACEMENT_3D('',#43020,#34108,#34109);
#31065=AXIS2_PLACEMENT_3D('',#43023,#34111,#34112);
#31066=AXIS2_PLACEMENT_3D('',#43024,#34113,#34114);
#31067=AXIS2_PLACEMENT_3D('',#43027,#34116,#34117);
#31068=AXIS2_PLACEMENT_3D('',#43028,#34118,#34119);
#31069=AXIS2_PLACEMENT_3D('',#43031,#34121,#34122);
#31070=AXIS2_PLACEMENT_3D('',#43032,#34123,#34124);
#31071=AXIS2_PLACEMENT_3D('',#43035,#34126,#34127);
#31072=AXIS2_PLACEMENT_3D('',#43036,#34128,#34129);
#31073=AXIS2_PLACEMENT_3D('',#43039,#34131,#34132);
#31074=AXIS2_PLACEMENT_3D('',#43040,#34133,#34134);
#31075=AXIS2_PLACEMENT_3D('',#43043,#34136,#34137);
#31076=AXIS2_PLACEMENT_3D('',#43044,#34138,#34139);
#31077=AXIS2_PLACEMENT_3D('',#43047,#34141,#34142);
#31078=AXIS2_PLACEMENT_3D('',#43048,#34143,#34144);
#31079=AXIS2_PLACEMENT_3D('',#43051,#34146,#34147);
#31080=AXIS2_PLACEMENT_3D('',#43052,#34148,#34149);
#31081=AXIS2_PLACEMENT_3D('',#43055,#34151,#34152);
#31082=AXIS2_PLACEMENT_3D('',#43056,#34153,#34154);
#31083=AXIS2_PLACEMENT_3D('',#43059,#34156,#34157);
#31084=AXIS2_PLACEMENT_3D('',#43060,#34158,#34159);
#31085=AXIS2_PLACEMENT_3D('',#43063,#34161,#34162);
#31086=AXIS2_PLACEMENT_3D('',#43064,#34163,#34164);
#31087=AXIS2_PLACEMENT_3D('',#43067,#34166,#34167);
#31088=AXIS2_PLACEMENT_3D('',#43068,#34168,#34169);
#31089=AXIS2_PLACEMENT_3D('',#43071,#34171,#34172);
#31090=AXIS2_PLACEMENT_3D('',#43072,#34173,#34174);
#31091=AXIS2_PLACEMENT_3D('',#43074,#34176,#34177);
#31092=AXIS2_PLACEMENT_3D('',#43077,#34179,#34180);
#31093=AXIS2_PLACEMENT_3D('',#43078,#34181,#34182);
#31094=AXIS2_PLACEMENT_3D('',#43080,#34184,#34185);
#31095=AXIS2_PLACEMENT_3D('',#43083,#34187,#34188);
#31096=AXIS2_PLACEMENT_3D('',#43084,#34189,#34190);
#31097=AXIS2_PLACEMENT_3D('',#43086,#34192,#34193);
#31098=AXIS2_PLACEMENT_3D('',#43089,#34195,#34196);
#31099=AXIS2_PLACEMENT_3D('',#43090,#34197,#34198);
#31100=AXIS2_PLACEMENT_3D('',#43092,#34200,#34201);
#31101=AXIS2_PLACEMENT_3D('',#43094,#34203,#34204);
#31102=AXIS2_PLACEMENT_3D('',#43096,#34206,#34207);
#31103=AXIS2_PLACEMENT_3D('',#43098,#34209,#34210);
#31104=AXIS2_PLACEMENT_3D('',#43100,#34212,#34213);
#31105=AXIS2_PLACEMENT_3D('',#43101,#34214,#34215);
#31106=AXIS2_PLACEMENT_3D('',#43102,#34216,#34217);
#31107=AXIS2_PLACEMENT_3D('',#43103,#34218,#34219);
#31108=AXIS2_PLACEMENT_3D('',#43104,#34220,#34221);
#31109=AXIS2_PLACEMENT_3D('',#43105,#34222,#34223);
#31110=AXIS2_PLACEMENT_3D('',#43106,#34224,#34225);
#31111=AXIS2_PLACEMENT_3D('',#43107,#34226,#34227);
#31112=AXIS2_PLACEMENT_3D('',#43108,#34228,#34229);
#31113=AXIS2_PLACEMENT_3D('',#43109,#34230,#34231);
#31114=AXIS2_PLACEMENT_3D('',#43110,#34232,#34233);
#31115=AXIS2_PLACEMENT_3D('',#43111,#34234,#34235);
#31116=AXIS2_PLACEMENT_3D('',#43112,#34236,#34237);
#31117=AXIS2_PLACEMENT_3D('',#43113,#34238,#34239);
#31118=AXIS2_PLACEMENT_3D('',#43114,#34240,#34241);
#31119=AXIS2_PLACEMENT_3D('',#43117,#34243,#34244);
#31120=AXIS2_PLACEMENT_3D('',#43118,#34245,#34246);
#31121=AXIS2_PLACEMENT_3D('',#43119,#34247,#34248);
#31122=AXIS2_PLACEMENT_3D('',#43120,#34249,#34250);
#31123=AXIS2_PLACEMENT_3D('',#43121,#34251,#34252);
#31124=AXIS2_PLACEMENT_3D('',#43123,#34253,#34254);
#31125=AXIS2_PLACEMENT_3D('',#43126,#34256,#34257);
#31126=AXIS2_PLACEMENT_3D('',#43127,#34258,#34259);
#31127=AXIS2_PLACEMENT_3D('',#43134,#34262,#34263);
#31128=AXIS2_PLACEMENT_3D('',#43138,#34265,#34266);
#31129=AXIS2_PLACEMENT_3D('',#43142,#34268,#34269);
#31130=AXIS2_PLACEMENT_3D('',#43146,#34271,#34272);
#31131=AXIS2_PLACEMENT_3D('',#43150,#34274,#34275);
#31132=AXIS2_PLACEMENT_3D('',#43154,#34277,#34278);
#31133=AXIS2_PLACEMENT_3D('',#43158,#34280,#34281);
#31134=AXIS2_PLACEMENT_3D('',#43162,#34283,#34284);
#31135=AXIS2_PLACEMENT_3D('',#43166,#34286,#34287);
#31136=AXIS2_PLACEMENT_3D('',#43170,#34289,#34290);
#31137=AXIS2_PLACEMENT_3D('',#43174,#34292,#34293);
#31138=AXIS2_PLACEMENT_3D('',#43177,#34295,#34296);
#31139=AXIS2_PLACEMENT_3D('',#43179,#34297,#34298);
#31140=AXIS2_PLACEMENT_3D('',#43181,#34299,#34300);
#31141=AXIS2_PLACEMENT_3D('',#43183,#34301,#34302);
#31142=AXIS2_PLACEMENT_3D('',#43185,#34303,#34304);
#31143=AXIS2_PLACEMENT_3D('',#43187,#34305,#34306);
#31144=AXIS2_PLACEMENT_3D('',#43189,#34307,#34308);
#31145=AXIS2_PLACEMENT_3D('',#43191,#34309,#34310);
#31146=AXIS2_PLACEMENT_3D('',#43193,#34311,#34312);
#31147=AXIS2_PLACEMENT_3D('',#43195,#34313,#34314);
#31148=AXIS2_PLACEMENT_3D('',#43196,#34315,#34316);
#31149=AXIS2_PLACEMENT_3D('',#43199,#34318,#34319);
#31150=AXIS2_PLACEMENT_3D('',#43200,#34320,#34321);
#31151=AXIS2_PLACEMENT_3D('',#43203,#34323,#34324);
#31152=AXIS2_PLACEMENT_3D('',#43204,#34325,#34326);
#31153=AXIS2_PLACEMENT_3D('',#43207,#34328,#34329);
#31154=AXIS2_PLACEMENT_3D('',#43208,#34330,#34331);
#31155=AXIS2_PLACEMENT_3D('',#43214,#34335,#34336);
#31156=AXIS2_PLACEMENT_3D('',#43216,#34337,#34338);
#31157=AXIS2_PLACEMENT_3D('',#43218,#34340,#34341);
#31158=AXIS2_PLACEMENT_3D('',#43222,#34344,#34345);
#31159=AXIS2_PLACEMENT_3D('',#43224,#34346,#34347);
#31160=AXIS2_PLACEMENT_3D('',#43226,#34349,#34350);
#31161=AXIS2_PLACEMENT_3D('',#43234,#34353,#34354);
#31162=AXIS2_PLACEMENT_3D('',#43240,#34355,#34356);
#31163=AXIS2_PLACEMENT_3D('',#43249,#34357,#34358);
#31164=AXIS2_PLACEMENT_3D('',#43255,#34362,#34363);
#31165=AXIS2_PLACEMENT_3D('',#43261,#34365,#34366);
#31166=AXIS2_PLACEMENT_3D('',#43270,#34371,#34372);
#31167=AXIS2_PLACEMENT_3D('',#43274,#34374,#34375);
#31168=AXIS2_PLACEMENT_3D('',#43275,#34376,#34377);
#31169=AXIS2_PLACEMENT_3D('',#43276,#34378,#34379);
#31170=AXIS2_PLACEMENT_3D('',#43282,#34383,#34384);
#31171=AXIS2_PLACEMENT_3D('',#43286,#34386,#34387);
#31172=AXIS2_PLACEMENT_3D('',#43287,#34388,#34389);
#31173=AXIS2_PLACEMENT_3D('',#43288,#34390,#34391);
#31174=AXIS2_PLACEMENT_3D('',#43291,#34394,#34395);
#31175=AXIS2_PLACEMENT_3D('',#43297,#34396,#34397);
#31176=AXIS2_PLACEMENT_3D('',#43299,#34398,#34399);
#31177=AXIS2_PLACEMENT_3D('',#43303,#34400,#34401);
#31178=AXIS2_PLACEMENT_3D('',#43306,#34404,#34405);
#31179=AXIS2_PLACEMENT_3D('',#43308,#34407,#34408);
#31180=AXIS2_PLACEMENT_3D('',#43309,#34409,#34410);
#31181=AXIS2_PLACEMENT_3D('',#43311,#34412,#34413);
#31182=AXIS2_PLACEMENT_3D('',#43317,#34417,#34418);
#31183=AXIS2_PLACEMENT_3D('',#43323,#34422,#34423);
#31184=AXIS2_PLACEMENT_3D('',#43325,#34424,#34425);
#31185=AXIS2_PLACEMENT_3D('',#43328,#34427,#34428);
#31186=AXIS2_PLACEMENT_3D('',#43329,#34429,#34430);
#31187=AXIS2_PLACEMENT_3D('',#43333,#34432,#34433);
#31188=AXIS2_PLACEMENT_3D('',#43337,#34435,#34436);
#31189=AXIS2_PLACEMENT_3D('',#43341,#34438,#34439);
#31190=AXIS2_PLACEMENT_3D('',#43345,#34441,#34442);
#31191=AXIS2_PLACEMENT_3D('',#43349,#34444,#34445);
#31192=AXIS2_PLACEMENT_3D('',#43353,#34447,#34448);
#31193=AXIS2_PLACEMENT_3D('',#43356,#34450,#34451);
#31194=AXIS2_PLACEMENT_3D('',#43358,#34452,#34453);
#31195=AXIS2_PLACEMENT_3D('',#43360,#34454,#34455);
#31196=AXIS2_PLACEMENT_3D('',#43362,#34456,#34457);
#31197=AXIS2_PLACEMENT_3D('',#43363,#34458,#34459);
#31198=AXIS2_PLACEMENT_3D('',#43365,#34460,#34461);
#31199=AXIS2_PLACEMENT_3D('',#43367,#34463,#34464);
#31200=AXIS2_PLACEMENT_3D('',#43370,#34466,#34467);
#31201=AXIS2_PLACEMENT_3D('',#43371,#34468,#34469);
#31202=AXIS2_PLACEMENT_3D('',#43373,#34470,#34471);
#31203=AXIS2_PLACEMENT_3D('',#43375,#34473,#34474);
#31204=AXIS2_PLACEMENT_3D('',#43378,#34476,#34477);
#31205=AXIS2_PLACEMENT_3D('',#43379,#34478,#34479);
#31206=AXIS2_PLACEMENT_3D('',#43381,#34480,#34481);
#31207=AXIS2_PLACEMENT_3D('',#43383,#34483,#34484);
#31208=AXIS2_PLACEMENT_3D('',#43386,#34486,#34487);
#31209=AXIS2_PLACEMENT_3D('',#43387,#34488,#34489);
#31210=AXIS2_PLACEMENT_3D('',#43391,#34492,#34493);
#31211=AXIS2_PLACEMENT_3D('',#43394,#34495,#34496);
#31212=AXIS2_PLACEMENT_3D('',#43395,#34497,#34498);
#31213=AXIS2_PLACEMENT_3D('',#43399,#34501,#34502);
#31214=AXIS2_PLACEMENT_3D('',#43402,#34504,#34505);
#31215=AXIS2_PLACEMENT_3D('',#43403,#34506,#34507);
#31216=AXIS2_PLACEMENT_3D('',#43407,#34510,#34511);
#31217=AXIS2_PLACEMENT_3D('',#43410,#34513,#34514);
#31218=AXIS2_PLACEMENT_3D('',#43411,#34515,#34516);
#31219=AXIS2_PLACEMENT_3D('',#43415,#34519,#34520);
#31220=AXIS2_PLACEMENT_3D('',#43418,#34522,#34523);
#31221=AXIS2_PLACEMENT_3D('',#43419,#34524,#34525);
#31222=AXIS2_PLACEMENT_3D('',#43423,#34528,#34529);
#31223=AXIS2_PLACEMENT_3D('',#43428,#34530,#34531);
#31224=AXIS2_PLACEMENT_3D('',#43429,#34532,#34533);
#31225=AXIS2_PLACEMENT_3D('',#43433,#34536,#34537);
#31226=AXIS2_PLACEMENT_3D('',#43442,#34542,#34543);
#31227=AXIS2_PLACEMENT_3D('',#43446,#34545,#34546);
#31228=AXIS2_PLACEMENT_3D('',#43447,#34547,#34548);
#31229=AXIS2_PLACEMENT_3D('',#43448,#34549,#34550);
#31230=AXIS2_PLACEMENT_3D('',#43454,#34554,#34555);
#31231=AXIS2_PLACEMENT_3D('',#43458,#34557,#34558);
#31232=AXIS2_PLACEMENT_3D('',#43459,#34559,#34560);
#31233=AXIS2_PLACEMENT_3D('',#43460,#34561,#34562);
#31234=AXIS2_PLACEMENT_3D('',#43466,#34566,#34567);
#31235=AXIS2_PLACEMENT_3D('',#43470,#34569,#34570);
#31236=AXIS2_PLACEMENT_3D('',#43471,#34571,#34572);
#31237=AXIS2_PLACEMENT_3D('',#43472,#34573,#34574);
#31238=AXIS2_PLACEMENT_3D('',#43478,#34578,#34579);
#31239=AXIS2_PLACEMENT_3D('',#43479,#34580,#34581);
#31240=AXIS2_PLACEMENT_3D('',#43480,#34582,#34583);
#31241=AXIS2_PLACEMENT_3D('',#43481,#34584,#34585);
#31242=AXIS2_PLACEMENT_3D('',#43485,#34587,#34588);
#31243=AXIS2_PLACEMENT_3D('',#43487,#34590,#34591);
#31244=AXIS2_PLACEMENT_3D('',#43491,#34594,#34595);
#31245=AXIS2_PLACEMENT_3D('',#43507,#34598,#34599);
#31246=AXIS2_PLACEMENT_3D('',#43508,#34600,#34601);
#31247=AXIS2_PLACEMENT_3D('',#43513,#34605,#34606);
#31248=AXIS2_PLACEMENT_3D('',#43514,#34607,#34608);
#31249=AXIS2_PLACEMENT_3D('',#43516,#34609,#34610);
#31250=AXIS2_PLACEMENT_3D('',#43517,#34611,#34612);
#31251=AXIS2_PLACEMENT_3D('',#43518,#34613,#34614);
#31252=AXIS2_PLACEMENT_3D('',#43520,#34615,#34616);
#31253=AXIS2_PLACEMENT_3D('',#43522,#34618,#34619);
#31254=AXIS2_PLACEMENT_3D('',#43526,#34622,#34623);
#31255=AXIS2_PLACEMENT_3D('',#43528,#34624,#34625);
#31256=AXIS2_PLACEMENT_3D('',#43530,#34627,#34628);
#31257=AXIS2_PLACEMENT_3D('',#43534,#34631,#34632);
#31258=AXIS2_PLACEMENT_3D('',#43536,#34633,#34634);
#31259=AXIS2_PLACEMENT_3D('',#43538,#34636,#34637);
#31260=AXIS2_PLACEMENT_3D('',#43542,#34640,#34641);
#31261=AXIS2_PLACEMENT_3D('',#43544,#34642,#34643);
#31262=AXIS2_PLACEMENT_3D('',#43546,#34645,#34646);
#31263=AXIS2_PLACEMENT_3D('',#43550,#34649,#34650);
#31264=AXIS2_PLACEMENT_3D('',#43552,#34651,#34652);
#31265=AXIS2_PLACEMENT_3D('',#43554,#34654,#34655);
#31266=AXIS2_PLACEMENT_3D('',#43558,#34658,#34659);
#31267=AXIS2_PLACEMENT_3D('',#43560,#34660,#34661);
#31268=AXIS2_PLACEMENT_3D('',#43562,#34663,#34664);
#31269=AXIS2_PLACEMENT_3D('',#43566,#34667,#34668);
#31270=AXIS2_PLACEMENT_3D('',#43568,#34669,#34670);
#31271=AXIS2_PLACEMENT_3D('',#43570,#34672,#34673);
#31272=AXIS2_PLACEMENT_3D('',#43573,#34676,#34677);
#31273=AXIS2_PLACEMENT_3D('',#43575,#34679,#34680);
#31274=AXIS2_PLACEMENT_3D('',#43577,#34682,#34683);
#31275=AXIS2_PLACEMENT_3D('',#43579,#34685,#34686);
#31276=AXIS2_PLACEMENT_3D('',#43580,#34687,#34688);
#31277=AXIS2_PLACEMENT_3D('',#43582,#34690,#34691);
#31278=AXIS2_PLACEMENT_3D('',#43584,#34693,#34694);
#31279=AXIS2_PLACEMENT_3D('',#43587,#34697,#34698);
#31280=AXIS2_PLACEMENT_3D('',#43589,#34700,#34701);
#31281=AXIS2_PLACEMENT_3D('',#43591,#34703,#34704);
#31282=AXIS2_PLACEMENT_3D('',#43593,#34706,#34707);
#31283=AXIS2_PLACEMENT_3D('',#43595,#34709,#34710);
#31284=AXIS2_PLACEMENT_3D('',#43597,#34712,#34713);
#31285=AXIS2_PLACEMENT_3D('',#43599,#34715,#34716);
#31286=AXIS2_PLACEMENT_3D('',#43601,#34718,#34719);
#31287=AXIS2_PLACEMENT_3D('',#43603,#34721,#34722);
#31288=AXIS2_PLACEMENT_3D('',#43605,#34724,#34725);
#31289=AXIS2_PLACEMENT_3D('',#43607,#34727,#34728);
#31290=AXIS2_PLACEMENT_3D('',#43609,#34730,#34731);
#31291=AXIS2_PLACEMENT_3D('',#43610,#34732,#34733);
#31292=AXIS2_PLACEMENT_3D('',#43612,#34735,#34736);
#31293=AXIS2_PLACEMENT_3D('',#43614,#34738,#34739);
#31294=AXIS2_PLACEMENT_3D('',#43616,#34741,#34742);
#31295=AXIS2_PLACEMENT_3D('',#43619,#34744,#34745);
#31296=AXIS2_PLACEMENT_3D('',#43620,#34746,#34747);
#31297=AXIS2_PLACEMENT_3D('',#43622,#34749,#34750);
#31298=AXIS2_PLACEMENT_3D('',#43665,#34752,#34753);
#31299=AXIS2_PLACEMENT_3D('',#43706,#34755,#34756);
#31300=AXIS2_PLACEMENT_3D('',#43707,#34757,#34758);
#31301=AXIS2_PLACEMENT_3D('',#43708,#34759,#34760);
#31302=AXIS2_PLACEMENT_3D('',#43712,#34763,#34764);
#31303=AXIS2_PLACEMENT_3D('',#43713,#34765,#34766);
#31304=AXIS2_PLACEMENT_3D('',#43714,#34767,#34768);
#31305=AXIS2_PLACEMENT_3D('',#43717,#34770,#34771);
#31306=AXIS2_PLACEMENT_3D('',#43718,#34772,#34773);
#31307=AXIS2_PLACEMENT_3D('',#43719,#34774,#34775);
#31308=AXIS2_PLACEMENT_3D('',#43720,#34776,#34777);
#31309=AXIS2_PLACEMENT_3D('',#43721,#34778,#34779);
#31310=AXIS2_PLACEMENT_3D('',#43724,#34781,#34782);
#31311=AXIS2_PLACEMENT_3D('',#43725,#34783,#34784);
#31312=AXIS2_PLACEMENT_3D('',#43726,#34785,#34786);
#31313=AXIS2_PLACEMENT_3D('',#43729,#34788,#34789);
#31314=AXIS2_PLACEMENT_3D('',#43730,#34790,#34791);
#31315=AXIS2_PLACEMENT_3D('',#43731,#34792,#34793);
#31316=AXIS2_PLACEMENT_3D('',#43734,#34795,#34796);
#31317=AXIS2_PLACEMENT_3D('',#43735,#34797,#34798);
#31318=AXIS2_PLACEMENT_3D('',#43736,#34799,#34800);
#31319=AXIS2_PLACEMENT_3D('',#43738,#34802,#34803);
#31320=AXIS2_PLACEMENT_3D('',#43739,#34804,#34805);
#31321=AXIS2_PLACEMENT_3D('',#43740,#34806,#34807);
#31322=AXIS2_PLACEMENT_3D('',#43741,#34808,#34809);
#31323=AXIS2_PLACEMENT_3D('',#43743,#34810,#34811);
#31324=AXIS2_PLACEMENT_3D('',#43746,#34813,#34814);
#31325=AXIS2_PLACEMENT_3D('',#43747,#34815,#34816);
#31326=AXIS2_PLACEMENT_3D('',#43750,#34818,#34819);
#31327=AXIS2_PLACEMENT_3D('',#43751,#34820,#34821);
#31328=AXIS2_PLACEMENT_3D('',#43753,#34822,#34823);
#31329=AXIS2_PLACEMENT_3D('',#43754,#34824,#34825);
#31330=AXIS2_PLACEMENT_3D('',#43756,#34826,#34827);
#31331=AXIS2_PLACEMENT_3D('',#43759,#34829,#34830);
#31332=AXIS2_PLACEMENT_3D('',#43760,#34831,#34832);
#31333=AXIS2_PLACEMENT_3D('',#43763,#34834,#34835);
#31334=AXIS2_PLACEMENT_3D('',#43764,#34836,#34837);
#31335=AXIS2_PLACEMENT_3D('',#43766,#34838,#34839);
#31336=AXIS2_PLACEMENT_3D('',#43767,#34840,#34841);
#31337=AXIS2_PLACEMENT_3D('',#43769,#34842,#34843);
#31338=AXIS2_PLACEMENT_3D('',#43772,#34845,#34846);
#31339=AXIS2_PLACEMENT_3D('',#43773,#34847,#34848);
#31340=AXIS2_PLACEMENT_3D('',#43776,#34850,#34851);
#31341=AXIS2_PLACEMENT_3D('',#43777,#34852,#34853);
#31342=AXIS2_PLACEMENT_3D('',#43779,#34854,#34855);
#31343=AXIS2_PLACEMENT_3D('',#43780,#34856,#34857);
#31344=AXIS2_PLACEMENT_3D('',#43782,#34858,#34859);
#31345=AXIS2_PLACEMENT_3D('',#43785,#34861,#34862);
#31346=AXIS2_PLACEMENT_3D('',#43786,#34863,#34864);
#31347=AXIS2_PLACEMENT_3D('',#43789,#34866,#34867);
#31348=AXIS2_PLACEMENT_3D('',#43790,#34868,#34869);
#31349=AXIS2_PLACEMENT_3D('',#43792,#34870,#34871);
#31350=AXIS2_PLACEMENT_3D('',#43793,#34872,#34873);
#31351=AXIS2_PLACEMENT_3D('',#43795,#34874,#34875);
#31352=AXIS2_PLACEMENT_3D('',#43798,#34877,#34878);
#31353=AXIS2_PLACEMENT_3D('',#43799,#34879,#34880);
#31354=AXIS2_PLACEMENT_3D('',#43802,#34882,#34883);
#31355=AXIS2_PLACEMENT_3D('',#43803,#34884,#34885);
#31356=AXIS2_PLACEMENT_3D('',#43805,#34886,#34887);
#31357=AXIS2_PLACEMENT_3D('',#43806,#34888,#34889);
#31358=AXIS2_PLACEMENT_3D('',#43808,#34890,#34891);
#31359=AXIS2_PLACEMENT_3D('',#43811,#34893,#34894);
#31360=AXIS2_PLACEMENT_3D('',#43812,#34895,#34896);
#31361=AXIS2_PLACEMENT_3D('',#43815,#34898,#34899);
#31362=AXIS2_PLACEMENT_3D('',#43816,#34900,#34901);
#31363=AXIS2_PLACEMENT_3D('',#43818,#34902,#34903);
#31364=AXIS2_PLACEMENT_3D('',#43819,#34904,#34905);
#31365=AXIS2_PLACEMENT_3D('',#43821,#34906,#34907);
#31366=AXIS2_PLACEMENT_3D('',#43824,#34909,#34910);
#31367=AXIS2_PLACEMENT_3D('',#43825,#34911,#34912);
#31368=AXIS2_PLACEMENT_3D('',#43828,#34914,#34915);
#31369=AXIS2_PLACEMENT_3D('',#43829,#34916,#34917);
#31370=AXIS2_PLACEMENT_3D('',#43831,#34918,#34919);
#31371=AXIS2_PLACEMENT_3D('',#43832,#34920,#34921);
#31372=AXIS2_PLACEMENT_3D('',#43834,#34922,#34923);
#31373=AXIS2_PLACEMENT_3D('',#43837,#34925,#34926);
#31374=AXIS2_PLACEMENT_3D('',#43838,#34927,#34928);
#31375=AXIS2_PLACEMENT_3D('',#43841,#34930,#34931);
#31376=AXIS2_PLACEMENT_3D('',#43842,#34932,#34933);
#31377=AXIS2_PLACEMENT_3D('',#43844,#34934,#34935);
#31378=AXIS2_PLACEMENT_3D('',#43845,#34936,#34937);
#31379=AXIS2_PLACEMENT_3D('',#43847,#34938,#34939);
#31380=AXIS2_PLACEMENT_3D('',#43850,#34941,#34942);
#31381=AXIS2_PLACEMENT_3D('',#43851,#34943,#34944);
#31382=AXIS2_PLACEMENT_3D('',#43853,#34945,#34946);
#31383=AXIS2_PLACEMENT_3D('',#43855,#34948,#34949);
#31384=AXIS2_PLACEMENT_3D('',#43857,#34950,#34951);
#31385=AXIS2_PLACEMENT_3D('',#43858,#34952,#34953);
#31386=AXIS2_PLACEMENT_3D('',#43871,#34960,#34961);
#31387=AXIS2_PLACEMENT_3D('',#43881,#34967,#34968);
#31388=AXIS2_PLACEMENT_3D('',#43885,#34971,#34972);
#31389=AXIS2_PLACEMENT_3D('',#43893,#34977,#34978);
#31390=AXIS2_PLACEMENT_3D('',#43895,#34979,#34980);
#31391=AXIS2_PLACEMENT_3D('',#43898,#34982,#34983);
#31392=AXIS2_PLACEMENT_3D('',#43899,#34984,#34985);
#31393=AXIS2_PLACEMENT_3D('',#43902,#34987,#34988);
#31394=AXIS2_PLACEMENT_3D('',#43903,#34989,#34990);
#31395=AXIS2_PLACEMENT_3D('',#43905,#34991,#34992);
#31396=AXIS2_PLACEMENT_3D('',#43906,#34993,#34994);
#31397=AXIS2_PLACEMENT_3D('',#43908,#34995,#34996);
#31398=AXIS2_PLACEMENT_3D('',#43911,#34998,#34999);
#31399=AXIS2_PLACEMENT_3D('',#43912,#35000,#35001);
#31400=AXIS2_PLACEMENT_3D('',#43915,#35003,#35004);
#31401=AXIS2_PLACEMENT_3D('',#43916,#35005,#35006);
#31402=AXIS2_PLACEMENT_3D('',#43918,#35007,#35008);
#31403=AXIS2_PLACEMENT_3D('',#43919,#35009,#35010);
#31404=AXIS2_PLACEMENT_3D('',#43932,#35017,#35018);
#31405=AXIS2_PLACEMENT_3D('',#43942,#35024,#35025);
#31406=AXIS2_PLACEMENT_3D('',#43946,#35028,#35029);
#31407=AXIS2_PLACEMENT_3D('',#43954,#35034,#35035);
#31408=AXIS2_PLACEMENT_3D('',#43960,#35039,#35040);
#31409=AXIS2_PLACEMENT_3D('',#43966,#35044,#35045);
#31410=AXIS2_PLACEMENT_3D('',#43968,#35046,#35047);
#31411=AXIS2_PLACEMENT_3D('',#43971,#35049,#35050);
#31412=AXIS2_PLACEMENT_3D('',#43972,#35051,#35052);
#31413=AXIS2_PLACEMENT_3D('',#43975,#35054,#35055);
#31414=AXIS2_PLACEMENT_3D('',#43976,#35056,#35057);
#31415=AXIS2_PLACEMENT_3D('',#43978,#35058,#35059);
#31416=AXIS2_PLACEMENT_3D('',#43979,#35060,#35061);
#31417=AXIS2_PLACEMENT_3D('',#43981,#35062,#35063);
#31418=AXIS2_PLACEMENT_3D('',#43984,#35065,#35066);
#31419=AXIS2_PLACEMENT_3D('',#43985,#35067,#35068);
#31420=AXIS2_PLACEMENT_3D('',#43988,#35070,#35071);
#31421=AXIS2_PLACEMENT_3D('',#43989,#35072,#35073);
#31422=AXIS2_PLACEMENT_3D('',#43991,#35074,#35075);
#31423=AXIS2_PLACEMENT_3D('',#43992,#35076,#35077);
#31424=AXIS2_PLACEMENT_3D('',#43994,#35078,#35079);
#31425=AXIS2_PLACEMENT_3D('',#43996,#35081,#35082);
#31426=AXIS2_PLACEMENT_3D('',#44000,#35085,#35086);
#31427=AXIS2_PLACEMENT_3D('',#44002,#35087,#35088);
#31428=AXIS2_PLACEMENT_3D('',#44004,#35089,#35090);
#31429=AXIS2_PLACEMENT_3D('',#44006,#35091,#35092);
#31430=AXIS2_PLACEMENT_3D('',#44008,#35093,#35094);
#31431=AXIS2_PLACEMENT_3D('',#44010,#35095,#35096);
#31432=AXIS2_PLACEMENT_3D('',#44012,#35097,#35098);
#31433=AXIS2_PLACEMENT_3D('',#44014,#35099,#35100);
#31434=AXIS2_PLACEMENT_3D('',#44016,#35101,#35102);
#31435=AXIS2_PLACEMENT_3D('',#44018,#35103,#35104);
#31436=AXIS2_PLACEMENT_3D('',#44020,#35105,#35106);
#31437=AXIS2_PLACEMENT_3D('',#44022,#35107,#35108);
#31438=AXIS2_PLACEMENT_3D('',#44024,#35109,#35110);
#31439=AXIS2_PLACEMENT_3D('',#44026,#35111,#35112);
#31440=AXIS2_PLACEMENT_3D('',#44028,#35113,#35114);
#31441=AXIS2_PLACEMENT_3D('',#44030,#35115,#35116);
#31442=AXIS2_PLACEMENT_3D('',#44032,#35117,#35118);
#31443=AXIS2_PLACEMENT_3D('',#44034,#35119,#35120);
#31444=AXIS2_PLACEMENT_3D('',#44036,#35121,#35122);
#31445=AXIS2_PLACEMENT_3D('',#44038,#35123,#35124);
#31446=AXIS2_PLACEMENT_3D('',#44040,#35125,#35126);
#31447=AXIS2_PLACEMENT_3D('',#44042,#35127,#35128);
#31448=AXIS2_PLACEMENT_3D('',#44044,#35129,#35130);
#31449=AXIS2_PLACEMENT_3D('',#44046,#35131,#35132);
#31450=AXIS2_PLACEMENT_3D('',#44048,#35133,#35134);
#31451=AXIS2_PLACEMENT_3D('',#44050,#35135,#35136);
#31452=AXIS2_PLACEMENT_3D('',#44052,#35137,#35138);
#31453=AXIS2_PLACEMENT_3D('',#44054,#35139,#35140);
#31454=AXIS2_PLACEMENT_3D('',#44056,#35141,#35142);
#31455=AXIS2_PLACEMENT_3D('',#44058,#35143,#35144);
#31456=AXIS2_PLACEMENT_3D('',#44060,#35145,#35146);
#31457=AXIS2_PLACEMENT_3D('',#44062,#35147,#35148);
#31458=AXIS2_PLACEMENT_3D('',#44064,#35149,#35150);
#31459=AXIS2_PLACEMENT_3D('',#44066,#35151,#35152);
#31460=AXIS2_PLACEMENT_3D('',#44068,#35153,#35154);
#31461=AXIS2_PLACEMENT_3D('',#44070,#35155,#35156);
#31462=AXIS2_PLACEMENT_3D('',#44072,#35157,#35158);
#31463=AXIS2_PLACEMENT_3D('',#44074,#35159,#35160);
#31464=AXIS2_PLACEMENT_3D('',#44076,#35161,#35162);
#31465=AXIS2_PLACEMENT_3D('',#44078,#35163,#35164);
#31466=AXIS2_PLACEMENT_3D('',#44080,#35165,#35166);
#31467=AXIS2_PLACEMENT_3D('',#44081,#35167,#35168);
#31468=AXIS2_PLACEMENT_3D('',#44083,#35170,#35171);
#31469=AXIS2_PLACEMENT_3D('',#44085,#35173,#35174);
#31470=AXIS2_PLACEMENT_3D('',#44087,#35176,#35177);
#31471=AXIS2_PLACEMENT_3D('',#44089,#35179,#35180);
#31472=AXIS2_PLACEMENT_3D('',#44091,#35182,#35183);
#31473=AXIS2_PLACEMENT_3D('',#44093,#35185,#35186);
#31474=AXIS2_PLACEMENT_3D('',#44095,#35188,#35189);
#31475=AXIS2_PLACEMENT_3D('',#44098,#35191,#35192);
#31476=AXIS2_PLACEMENT_3D('',#44099,#35193,#35194);
#31477=AXIS2_PLACEMENT_3D('',#44101,#35195,#35196);
#31478=AXIS2_PLACEMENT_3D('',#44103,#35198,#35199);
#31479=AXIS2_PLACEMENT_3D('',#44106,#35201,#35202);
#31480=AXIS2_PLACEMENT_3D('',#44107,#35203,#35204);
#31481=AXIS2_PLACEMENT_3D('',#44109,#35205,#35206);
#31482=AXIS2_PLACEMENT_3D('',#44111,#35208,#35209);
#31483=AXIS2_PLACEMENT_3D('',#44113,#35211,#35212);
#31484=AXIS2_PLACEMENT_3D('',#44115,#35214,#35215);
#31485=AXIS2_PLACEMENT_3D('',#44117,#35217,#35218);
#31486=AXIS2_PLACEMENT_3D('',#44119,#35220,#35221);
#31487=AXIS2_PLACEMENT_3D('',#44121,#35223,#35224);
#31488=AXIS2_PLACEMENT_3D('',#44124,#35226,#35227);
#31489=AXIS2_PLACEMENT_3D('',#44125,#35228,#35229);
#31490=AXIS2_PLACEMENT_3D('',#44127,#35230,#35231);
#31491=AXIS2_PLACEMENT_3D('',#44129,#35233,#35234);
#31492=AXIS2_PLACEMENT_3D('',#44132,#35236,#35237);
#31493=AXIS2_PLACEMENT_3D('',#44133,#35238,#35239);
#31494=AXIS2_PLACEMENT_3D('',#44135,#35240,#35241);
#31495=AXIS2_PLACEMENT_3D('',#44137,#35243,#35244);
#31496=AXIS2_PLACEMENT_3D('',#44140,#35246,#35247);
#31497=AXIS2_PLACEMENT_3D('',#44141,#35248,#35249);
#31498=AXIS2_PLACEMENT_3D('',#44143,#35250,#35251);
#31499=AXIS2_PLACEMENT_3D('',#44145,#35253,#35254);
#31500=AXIS2_PLACEMENT_3D('',#44148,#35256,#35257);
#31501=AXIS2_PLACEMENT_3D('',#44149,#35258,#35259);
#31502=AXIS2_PLACEMENT_3D('',#44151,#35260,#35261);
#31503=AXIS2_PLACEMENT_3D('',#44153,#35263,#35264);
#31504=AXIS2_PLACEMENT_3D('',#44156,#35266,#35267);
#31505=AXIS2_PLACEMENT_3D('',#44157,#35268,#35269);
#31506=AXIS2_PLACEMENT_3D('',#44159,#35270,#35271);
#31507=AXIS2_PLACEMENT_3D('',#44161,#35273,#35274);
#31508=AXIS2_PLACEMENT_3D('',#44164,#35276,#35277);
#31509=AXIS2_PLACEMENT_3D('',#44165,#35278,#35279);
#31510=AXIS2_PLACEMENT_3D('',#44167,#35280,#35281);
#31511=AXIS2_PLACEMENT_3D('',#44169,#35283,#35284);
#31512=AXIS2_PLACEMENT_3D('',#44172,#35286,#35287);
#31513=AXIS2_PLACEMENT_3D('',#44173,#35288,#35289);
#31514=AXIS2_PLACEMENT_3D('',#44175,#35290,#35291);
#31515=AXIS2_PLACEMENT_3D('',#44177,#35293,#35294);
#31516=AXIS2_PLACEMENT_3D('',#44180,#35296,#35297);
#31517=AXIS2_PLACEMENT_3D('',#44181,#35298,#35299);
#31518=AXIS2_PLACEMENT_3D('',#44183,#35300,#35301);
#31519=AXIS2_PLACEMENT_3D('',#44185,#35303,#35304);
#31520=AXIS2_PLACEMENT_3D('',#44188,#35306,#35307);
#31521=AXIS2_PLACEMENT_3D('',#44189,#35308,#35309);
#31522=AXIS2_PLACEMENT_3D('',#44191,#35310,#35311);
#31523=AXIS2_PLACEMENT_3D('',#44193,#35313,#35314);
#31524=AXIS2_PLACEMENT_3D('',#44196,#35316,#35317);
#31525=AXIS2_PLACEMENT_3D('',#44197,#35318,#35319);
#31526=AXIS2_PLACEMENT_3D('',#44199,#35320,#35321);
#31527=AXIS2_PLACEMENT_3D('',#44201,#35323,#35324);
#31528=AXIS2_PLACEMENT_3D('',#44204,#35326,#35327);
#31529=AXIS2_PLACEMENT_3D('',#44205,#35328,#35329);
#31530=AXIS2_PLACEMENT_3D('',#44207,#35330,#35331);
#31531=AXIS2_PLACEMENT_3D('',#44209,#35333,#35334);
#31532=AXIS2_PLACEMENT_3D('',#44212,#35336,#35337);
#31533=AXIS2_PLACEMENT_3D('',#44213,#35338,#35339);
#31534=AXIS2_PLACEMENT_3D('',#44215,#35340,#35341);
#31535=AXIS2_PLACEMENT_3D('',#44217,#35343,#35344);
#31536=AXIS2_PLACEMENT_3D('',#44219,#35346,#35347);
#31537=AXIS2_PLACEMENT_3D('',#44221,#35349,#35350);
#31538=AXIS2_PLACEMENT_3D('',#44224,#35352,#35353);
#31539=AXIS2_PLACEMENT_3D('',#44225,#35354,#35355);
#31540=AXIS2_PLACEMENT_3D('',#44227,#35356,#35357);
#31541=AXIS2_PLACEMENT_3D('',#44229,#35359,#35360);
#31542=AXIS2_PLACEMENT_3D('',#44232,#35362,#35363);
#31543=AXIS2_PLACEMENT_3D('',#44233,#35364,#35365);
#31544=AXIS2_PLACEMENT_3D('',#44235,#35366,#35367);
#31545=AXIS2_PLACEMENT_3D('',#44237,#35369,#35370);
#31546=AXIS2_PLACEMENT_3D('',#44240,#35372,#35373);
#31547=AXIS2_PLACEMENT_3D('',#44241,#35374,#35375);
#31548=AXIS2_PLACEMENT_3D('',#44243,#35376,#35377);
#31549=AXIS2_PLACEMENT_3D('',#44245,#35379,#35380);
#31550=AXIS2_PLACEMENT_3D('',#44248,#35382,#35383);
#31551=AXIS2_PLACEMENT_3D('',#44249,#35384,#35385);
#31552=AXIS2_PLACEMENT_3D('',#44251,#35386,#35387);
#31553=AXIS2_PLACEMENT_3D('',#44253,#35389,#35390);
#31554=AXIS2_PLACEMENT_3D('',#44256,#35392,#35393);
#31555=AXIS2_PLACEMENT_3D('',#44257,#35394,#35395);
#31556=AXIS2_PLACEMENT_3D('',#44259,#35396,#35397);
#31557=AXIS2_PLACEMENT_3D('',#44261,#35399,#35400);
#31558=AXIS2_PLACEMENT_3D('',#44264,#35402,#35403);
#31559=AXIS2_PLACEMENT_3D('',#44265,#35404,#35405);
#31560=AXIS2_PLACEMENT_3D('',#44267,#35406,#35407);
#31561=AXIS2_PLACEMENT_3D('',#44269,#35409,#35410);
#31562=AXIS2_PLACEMENT_3D('',#44272,#35412,#35413);
#31563=AXIS2_PLACEMENT_3D('',#44273,#35414,#35415);
#31564=AXIS2_PLACEMENT_3D('',#44275,#35416,#35417);
#31565=AXIS2_PLACEMENT_3D('',#44277,#35419,#35420);
#31566=AXIS2_PLACEMENT_3D('',#44280,#35422,#35423);
#31567=AXIS2_PLACEMENT_3D('',#44281,#35424,#35425);
#31568=AXIS2_PLACEMENT_3D('',#44283,#35426,#35427);
#31569=AXIS2_PLACEMENT_3D('',#44285,#35429,#35430);
#31570=AXIS2_PLACEMENT_3D('',#44288,#35432,#35433);
#31571=AXIS2_PLACEMENT_3D('',#44289,#35434,#35435);
#31572=AXIS2_PLACEMENT_3D('',#44291,#35436,#35437);
#31573=AXIS2_PLACEMENT_3D('',#44293,#35439,#35440);
#31574=AXIS2_PLACEMENT_3D('',#44296,#35442,#35443);
#31575=AXIS2_PLACEMENT_3D('',#44297,#35444,#35445);
#31576=AXIS2_PLACEMENT_3D('',#44299,#35446,#35447);
#31577=AXIS2_PLACEMENT_3D('',#44301,#35449,#35450);
#31578=AXIS2_PLACEMENT_3D('',#44304,#35452,#35453);
#31579=AXIS2_PLACEMENT_3D('',#44305,#35454,#35455);
#31580=AXIS2_PLACEMENT_3D('',#44307,#35456,#35457);
#31581=AXIS2_PLACEMENT_3D('',#44309,#35459,#35460);
#31582=AXIS2_PLACEMENT_3D('',#44312,#35462,#35463);
#31583=AXIS2_PLACEMENT_3D('',#44313,#35464,#35465);
#31584=AXIS2_PLACEMENT_3D('',#44315,#35466,#35467);
#31585=AXIS2_PLACEMENT_3D('',#44317,#35469,#35470);
#31586=AXIS2_PLACEMENT_3D('',#44320,#35472,#35473);
#31587=AXIS2_PLACEMENT_3D('',#44321,#35474,#35475);
#31588=AXIS2_PLACEMENT_3D('',#44323,#35476,#35477);
#31589=AXIS2_PLACEMENT_3D('',#44325,#35479,#35480);
#31590=AXIS2_PLACEMENT_3D('',#44328,#35482,#35483);
#31591=AXIS2_PLACEMENT_3D('',#44329,#35484,#35485);
#31592=AXIS2_PLACEMENT_3D('',#44331,#35486,#35487);
#31593=AXIS2_PLACEMENT_3D('',#44333,#35489,#35490);
#31594=AXIS2_PLACEMENT_3D('',#44336,#35492,#35493);
#31595=AXIS2_PLACEMENT_3D('',#44337,#35494,#35495);
#31596=AXIS2_PLACEMENT_3D('',#44339,#35496,#35497);
#31597=AXIS2_PLACEMENT_3D('',#44341,#35499,#35500);
#31598=AXIS2_PLACEMENT_3D('',#44344,#35503,#35504);
#31599=AXIS2_PLACEMENT_3D('',#44346,#35506,#35507);
#31600=AXIS2_PLACEMENT_3D('',#44348,#35508,#35509);
#31601=AXIS2_PLACEMENT_3D('',#44350,#35510,#35511);
#31602=AXIS2_PLACEMENT_3D('',#44352,#35512,#35513);
#31603=AXIS2_PLACEMENT_3D('',#44354,#35514,#35515);
#31604=AXIS2_PLACEMENT_3D('',#44356,#35516,#35517);
#31605=AXIS2_PLACEMENT_3D('',#44358,#35518,#35519);
#31606=AXIS2_PLACEMENT_3D('',#44360,#35520,#35521);
#31607=AXIS2_PLACEMENT_3D('',#44362,#35522,#35523);
#31608=AXIS2_PLACEMENT_3D('',#44364,#35524,#35525);
#31609=AXIS2_PLACEMENT_3D('',#44366,#35526,#35527);
#31610=AXIS2_PLACEMENT_3D('',#44368,#35528,#35529);
#31611=AXIS2_PLACEMENT_3D('',#44370,#35530,#35531);
#31612=AXIS2_PLACEMENT_3D('',#44372,#35532,#35533);
#31613=AXIS2_PLACEMENT_3D('',#44374,#35534,#35535);
#31614=AXIS2_PLACEMENT_3D('',#44376,#35536,#35537);
#31615=AXIS2_PLACEMENT_3D('',#44378,#35538,#35539);
#31616=AXIS2_PLACEMENT_3D('',#44380,#35540,#35541);
#31617=AXIS2_PLACEMENT_3D('',#44382,#35542,#35543);
#31618=AXIS2_PLACEMENT_3D('',#44384,#35544,#35545);
#31619=AXIS2_PLACEMENT_3D('',#44386,#35546,#35547);
#31620=AXIS2_PLACEMENT_3D('',#44388,#35548,#35549);
#31621=AXIS2_PLACEMENT_3D('',#44390,#35550,#35551);
#31622=AXIS2_PLACEMENT_3D('',#44392,#35552,#35553);
#31623=AXIS2_PLACEMENT_3D('',#44394,#35554,#35555);
#31624=AXIS2_PLACEMENT_3D('',#44396,#35556,#35557);
#31625=AXIS2_PLACEMENT_3D('',#44398,#35558,#35559);
#31626=AXIS2_PLACEMENT_3D('',#44400,#35560,#35561);
#31627=AXIS2_PLACEMENT_3D('',#44402,#35562,#35563);
#31628=AXIS2_PLACEMENT_3D('',#44404,#35564,#35565);
#31629=AXIS2_PLACEMENT_3D('',#44406,#35566,#35567);
#31630=AXIS2_PLACEMENT_3D('',#44408,#35568,#35569);
#31631=AXIS2_PLACEMENT_3D('',#44410,#35570,#35571);
#31632=AXIS2_PLACEMENT_3D('',#44412,#35572,#35573);
#31633=AXIS2_PLACEMENT_3D('',#44414,#35574,#35575);
#31634=AXIS2_PLACEMENT_3D('',#44416,#35576,#35577);
#31635=AXIS2_PLACEMENT_3D('',#44418,#35578,#35579);
#31636=AXIS2_PLACEMENT_3D('',#44420,#35580,#35581);
#31637=AXIS2_PLACEMENT_3D('',#44422,#35582,#35583);
#31638=AXIS2_PLACEMENT_3D('',#44424,#35584,#35585);
#31639=AXIS2_PLACEMENT_3D('',#44426,#35586,#35587);
#31640=AXIS2_PLACEMENT_3D('',#44428,#35588,#35589);
#31641=AXIS2_PLACEMENT_3D('',#44430,#35590,#35591);
#31642=AXIS2_PLACEMENT_3D('',#44431,#35592,#35593);
#31643=AXIS2_PLACEMENT_3D('',#44433,#35595,#35596);
#31644=AXIS2_PLACEMENT_3D('',#44435,#35598,#35599);
#31645=AXIS2_PLACEMENT_3D('',#44437,#35601,#35602);
#31646=AXIS2_PLACEMENT_3D('',#44439,#35604,#35605);
#31647=AXIS2_PLACEMENT_3D('',#44441,#35607,#35608);
#31648=AXIS2_PLACEMENT_3D('',#44443,#35610,#35611);
#31649=AXIS2_PLACEMENT_3D('',#44445,#35613,#35614);
#31650=AXIS2_PLACEMENT_3D('',#44447,#35616,#35617);
#31651=AXIS2_PLACEMENT_3D('',#44450,#35619,#35620);
#31652=AXIS2_PLACEMENT_3D('',#44451,#35621,#35622);
#31653=AXIS2_PLACEMENT_3D('',#44453,#35624,#35625);
#31654=AXIS2_PLACEMENT_3D('',#44456,#35627,#35628);
#31655=AXIS2_PLACEMENT_3D('',#44457,#35629,#35630);
#31656=AXIS2_PLACEMENT_3D('',#44459,#35632,#35633);
#31657=AXIS2_PLACEMENT_3D('',#44462,#35635,#35636);
#31658=AXIS2_PLACEMENT_3D('',#44463,#35637,#35638);
#31659=AXIS2_PLACEMENT_3D('',#44465,#35640,#35641);
#31660=AXIS2_PLACEMENT_3D('',#44468,#35643,#35644);
#31661=AXIS2_PLACEMENT_3D('',#44469,#35645,#35646);
#31662=AXIS2_PLACEMENT_3D('',#44471,#35648,#35649);
#31663=AXIS2_PLACEMENT_3D('',#44474,#35651,#35652);
#31664=AXIS2_PLACEMENT_3D('',#44475,#35653,#35654);
#31665=AXIS2_PLACEMENT_3D('',#44477,#35656,#35657);
#31666=AXIS2_PLACEMENT_3D('',#44480,#35659,#35660);
#31667=AXIS2_PLACEMENT_3D('',#44481,#35661,#35662);
#31668=AXIS2_PLACEMENT_3D('',#44483,#35664,#35665);
#31669=AXIS2_PLACEMENT_3D('',#44486,#35667,#35668);
#31670=AXIS2_PLACEMENT_3D('',#44487,#35669,#35670);
#31671=AXIS2_PLACEMENT_3D('',#44489,#35672,#35673);
#31672=AXIS2_PLACEMENT_3D('',#44492,#35675,#35676);
#31673=AXIS2_PLACEMENT_3D('',#44493,#35677,#35678);
#31674=AXIS2_PLACEMENT_3D('',#44495,#35680,#35681);
#31675=AXIS2_PLACEMENT_3D('',#44498,#35683,#35684);
#31676=AXIS2_PLACEMENT_3D('',#44499,#35685,#35686);
#31677=AXIS2_PLACEMENT_3D('',#44501,#35688,#35689);
#31678=AXIS2_PLACEMENT_3D('',#44504,#35691,#35692);
#31679=AXIS2_PLACEMENT_3D('',#44505,#35693,#35694);
#31680=AXIS2_PLACEMENT_3D('',#44507,#35696,#35697);
#31681=AXIS2_PLACEMENT_3D('',#44509,#35699,#35700);
#31682=AXIS2_PLACEMENT_3D('',#44511,#35702,#35703);
#31683=AXIS2_PLACEMENT_3D('',#44513,#35705,#35706);
#31684=AXIS2_PLACEMENT_3D('',#44515,#35708,#35709);
#31685=AXIS2_PLACEMENT_3D('',#44517,#35711,#35712);
#31686=AXIS2_PLACEMENT_3D('',#44519,#35714,#35715);
#31687=AXIS2_PLACEMENT_3D('',#44521,#35717,#35718);
#31688=AXIS2_PLACEMENT_3D('',#44523,#35720,#35721);
#31689=AXIS2_PLACEMENT_3D('',#44525,#35723,#35724);
#31690=AXIS2_PLACEMENT_3D('',#44527,#35726,#35727);
#31691=AXIS2_PLACEMENT_3D('',#44529,#35729,#35730);
#31692=AXIS2_PLACEMENT_3D('',#44531,#35732,#35733);
#31693=AXIS2_PLACEMENT_3D('',#44533,#35735,#35736);
#31694=AXIS2_PLACEMENT_3D('',#44535,#35738,#35739);
#31695=AXIS2_PLACEMENT_3D('',#44537,#35741,#35742);
#31696=AXIS2_PLACEMENT_3D('',#44539,#35744,#35745);
#31697=AXIS2_PLACEMENT_3D('',#44541,#35747,#35748);
#31698=AXIS2_PLACEMENT_3D('',#44543,#35750,#35751);
#31699=AXIS2_PLACEMENT_3D('',#44545,#35753,#35754);
#31700=AXIS2_PLACEMENT_3D('',#44547,#35756,#35757);
#31701=AXIS2_PLACEMENT_3D('',#44549,#35759,#35760);
#31702=AXIS2_PLACEMENT_3D('',#44551,#35762,#35763);
#31703=AXIS2_PLACEMENT_3D('',#44554,#35765,#35766);
#31704=AXIS2_PLACEMENT_3D('',#44555,#35767,#35768);
#31705=AXIS2_PLACEMENT_3D('',#44557,#35770,#35771);
#31706=AXIS2_PLACEMENT_3D('',#44560,#35773,#35774);
#31707=AXIS2_PLACEMENT_3D('',#44561,#35775,#35776);
#31708=AXIS2_PLACEMENT_3D('',#44563,#35778,#35779);
#31709=AXIS2_PLACEMENT_3D('',#44565,#35781,#35782);
#31710=AXIS2_PLACEMENT_3D('',#44566,#35783,#35784);
#31711=AXIS2_PLACEMENT_3D('',#44567,#35785,#35786);
#31712=AXIS2_PLACEMENT_3D('',#44577,#35787,#35788);
#31713=AXIS2_PLACEMENT_3D('',#44580,#35790,#35791);
#31714=AXIS2_PLACEMENT_3D('',#44581,#35792,#35793);
#31715=AXIS2_PLACEMENT_3D('',#44582,#35794,#35795);
#31716=AXIS2_PLACEMENT_3D('',#44584,#35796,#35797);
#31717=AXIS2_PLACEMENT_3D('',#44587,#35799,#35800);
#31718=AXIS2_PLACEMENT_3D('',#44589,#35801,#35802);
#31719=AXIS2_PLACEMENT_3D('',#44594,#35803,#35804);
#31720=AXIS2_PLACEMENT_3D('',#44595,#35805,#35806);
#31721=AXIS2_PLACEMENT_3D('',#44598,#35808,#35809);
#31722=AXIS2_PLACEMENT_3D('',#44599,#35810,#35811);
#31723=AXIS2_PLACEMENT_3D('',#44611,#35818,#35819);
#31724=AXIS2_PLACEMENT_3D('',#44614,#35821,#35822);
#31725=AXIS2_PLACEMENT_3D('',#44615,#35823,#35824);
#31726=AXIS2_PLACEMENT_3D('',#44619,#35827,#35828);
#31727=AXIS2_PLACEMENT_3D('',#44626,#35832,#35833);
#31728=AXIS2_PLACEMENT_3D('',#44629,#35836,#35837);
#31729=AXIS2_PLACEMENT_3D('',#44637,#35842,#35843);
#31730=AXIS2_PLACEMENT_3D('',#44644,#35847,#35848);
#31731=AXIS2_PLACEMENT_3D('',#44649,#35852,#35853);
#31732=AXIS2_PLACEMENT_3D('',#44652,#35856,#35857);
#31733=AXIS2_PLACEMENT_3D('',#44660,#35862,#35863);
#31734=AXIS2_PLACEMENT_3D('',#44668,#35868,#35869);
#31735=AXIS2_PLACEMENT_3D('',#44671,#35871,#35872);
#31736=AXIS2_PLACEMENT_3D('',#44673,#35873,#35874);
#31737=AXIS2_PLACEMENT_3D('',#44674,#35875,#35876);
#31738=AXIS2_PLACEMENT_3D('',#44677,#35878,#35879);
#31739=AXIS2_PLACEMENT_3D('',#44679,#35880,#35881);
#31740=AXIS2_PLACEMENT_3D('',#44680,#35882,#35883);
#31741=AXIS2_PLACEMENT_3D('',#44686,#35887,#35888);
#31742=AXIS2_PLACEMENT_3D('',#44692,#35892,#35893);
#31743=AXIS2_PLACEMENT_3D('',#44693,#35894,#35895);
#31744=AXIS2_PLACEMENT_3D('',#44697,#35898,#35899);
#31745=AXIS2_PLACEMENT_3D('',#44700,#35902,#35903);
#31746=AXIS2_PLACEMENT_3D('',#44704,#35906,#35907);
#31747=AXIS2_PLACEMENT_3D('',#44707,#35910,#35911);
#31748=AXIS2_PLACEMENT_3D('',#44709,#35912,#35913);
#31749=AXIS2_PLACEMENT_3D('',#44710,#35914,#35915);
#31750=AXIS2_PLACEMENT_3D('',#44712,#35916,#35917);
#31751=AXIS2_PLACEMENT_3D('',#44713,#35918,#35919);
#31752=AXIS2_PLACEMENT_3D('',#44715,#35920,#35921);
#31753=AXIS2_PLACEMENT_3D('',#44716,#35922,#35923);
#31754=AXIS2_PLACEMENT_3D('',#44718,#35924,#35925);
#31755=AXIS2_PLACEMENT_3D('',#44719,#35926,#35927);
#31756=AXIS2_PLACEMENT_3D('',#44721,#35929,#35930);
#31757=AXIS2_PLACEMENT_3D('',#44723,#35932,#35933);
#31758=AXIS2_PLACEMENT_3D('',#44766,#35935,#35936);
#31759=AXIS2_PLACEMENT_3D('',#44807,#35938,#35939);
#31760=AXIS2_PLACEMENT_3D('',#44808,#35940,#35941);
#31761=AXIS2_PLACEMENT_3D('',#44809,#35942,#35943);
#31762=AXIS2_PLACEMENT_3D('',#44813,#35946,#35947);
#31763=AXIS2_PLACEMENT_3D('',#44814,#35948,#35949);
#31764=AXIS2_PLACEMENT_3D('',#44815,#35950,#35951);
#31765=AXIS2_PLACEMENT_3D('',#44817,#35953,#35954);
#31766=AXIS2_PLACEMENT_3D('',#44818,#35955,#35956);
#31767=AXIS2_PLACEMENT_3D('',#44819,#35957,#35958);
#31768=AXIS2_PLACEMENT_3D('',#44850,#35959,#35960);
#31769=AXIS2_PLACEMENT_3D('',#44906,#35962,#35963);
#31770=AXIS2_PLACEMENT_3D('',#44907,#35964,#35965);
#31771=AXIS2_PLACEMENT_3D('',#44909,#35967,#35968);
#31772=AXIS2_PLACEMENT_3D('',#44911,#35969,#35970);
#31773=AXIS2_PLACEMENT_3D('',#44912,#35971,#35972);
#31774=AXIS2_PLACEMENT_3D('',#44913,#35973,#35974);
#31775=AXIS2_PLACEMENT_3D('',#44914,#35975,#35976);
#31776=AXIS2_PLACEMENT_3D('',#44915,#35977,#35978);
#31777=AXIS2_PLACEMENT_3D('',#44938,#35979,#35980);
#31778=AXIS2_PLACEMENT_3D('',#45008,#35982,#35983);
#31779=AXIS2_PLACEMENT_3D('',#45010,#35985,#35986);
#31780=AXIS2_PLACEMENT_3D('',#45012,#35987,#35988);
#31781=AXIS2_PLACEMENT_3D('',#45013,#35989,#35990);
#31782=AXIS2_PLACEMENT_3D('',#45014,#35991,#35992);
#31783=AXIS2_PLACEMENT_3D('',#45015,#35993,#35994);
#31784=AXIS2_PLACEMENT_3D('',#46413,#35995,#35996);
#31785=AXIS2_PLACEMENT_3D('',#46414,#35997,#35998);
#31786=AXIS2_PLACEMENT_3D('',#46430,#36000,#36001);
#31787=AXIS2_PLACEMENT_3D('',#46438,#36002,#36003);
#31788=AXIS2_PLACEMENT_3D('',#46486,#36005,#36006);
#31789=AXIS2_PLACEMENT_3D('',#46534,#36008,#36009);
#31790=AXIS2_PLACEMENT_3D('',#46582,#36011,#36012);
#31791=AXIS2_PLACEMENT_3D('',#46636,#36014,#36015);
#31792=AXIS2_PLACEMENT_3D('',#46684,#36017,#36018);
#31793=AXIS2_PLACEMENT_3D('',#46732,#36020,#36021);
#31794=AXIS2_PLACEMENT_3D('',#46786,#36023,#36024);
#31795=AXIS2_PLACEMENT_3D('',#46834,#36026,#36027);
#31796=AXIS2_PLACEMENT_3D('',#46882,#36029,#36030);
#31797=AXIS2_PLACEMENT_3D('',#46893,#36032,#36033);
#31798=AXIS2_PLACEMENT_3D('',#46898,#36034,#36035);
#31799=AXIS2_PLACEMENT_3D('',#46922,#36037,#36038);
#31800=AXIS2_PLACEMENT_3D('',#46946,#36040,#36041);
#31801=AXIS2_PLACEMENT_3D('',#46971,#36043,#36044);
#31802=AXIS2_PLACEMENT_3D('',#46996,#36046,#36047);
#31803=AXIS2_PLACEMENT_3D('',#47020,#36049,#36050);
#31804=AXIS2_PLACEMENT_3D('',#47045,#36052,#36053);
#31805=AXIS2_PLACEMENT_3D('',#47070,#36055,#36056);
#31806=AXIS2_PLACEMENT_3D('',#47094,#36058,#36059);
#31807=AXIS2_PLACEMENT_3D('',#47118,#36061,#36062);
#31808=AXIS2_PLACEMENT_3D('',#47218,#36063,#36064);
#31809=AXIS2_PLACEMENT_3D('',#47220,#36065,#36066);
#31810=AXIS2_PLACEMENT_3D('',#47709,#36067,#36068);
#31811=AXIS2_PLACEMENT_3D('',#47711,#36069,#36070);
#31812=AXIS2_PLACEMENT_3D('',#47712,#36071,#36072);
#31813=AXIS2_PLACEMENT_3D('',#47811,#36073,#36074);
#31814=AXIS2_PLACEMENT_3D('',#47812,#36075,#36076);
#31815=AXIS2_PLACEMENT_3D('',#48102,#36077,#36078);
#31816=AXIS2_PLACEMENT_3D('',#48111,#36083,#36084);
#31817=AXIS2_PLACEMENT_3D('',#48113,#36085,#36086);
#31818=AXIS2_PLACEMENT_3D('',#48115,#36088,#36089);
#31819=AXIS2_PLACEMENT_3D('',#48119,#36092,#36093);
#31820=AXIS2_PLACEMENT_3D('',#48120,#36094,#36095);
#31821=AXIS2_PLACEMENT_3D('',#48121,#36096,#36097);
#31822=AXIS2_PLACEMENT_3D('',#48130,#36102,#36103);
#31823=AXIS2_PLACEMENT_3D('',#48132,#36104,#36105);
#31824=AXIS2_PLACEMENT_3D('',#48134,#36107,#36108);
#31825=AXIS2_PLACEMENT_3D('',#48138,#36111,#36112);
#31826=AXIS2_PLACEMENT_3D('',#48139,#36113,#36114);
#31827=AXIS2_PLACEMENT_3D('',#48140,#36115,#36116);
#31828=AXIS2_PLACEMENT_3D('',#48149,#36121,#36122);
#31829=AXIS2_PLACEMENT_3D('',#48151,#36123,#36124);
#31830=AXIS2_PLACEMENT_3D('',#48153,#36126,#36127);
#31831=AXIS2_PLACEMENT_3D('',#48157,#36130,#36131);
#31832=AXIS2_PLACEMENT_3D('',#48158,#36132,#36133);
#31833=AXIS2_PLACEMENT_3D('',#48159,#36134,#36135);
#31834=AXIS2_PLACEMENT_3D('',#48168,#36140,#36141);
#31835=AXIS2_PLACEMENT_3D('',#48170,#36142,#36143);
#31836=AXIS2_PLACEMENT_3D('',#48172,#36145,#36146);
#31837=AXIS2_PLACEMENT_3D('',#48176,#36149,#36150);
#31838=AXIS2_PLACEMENT_3D('',#48177,#36151,#36152);
#31839=AXIS2_PLACEMENT_3D('',#48178,#36153,#36154);
#31840=AXIS2_PLACEMENT_3D('',#48187,#36159,#36160);
#31841=AXIS2_PLACEMENT_3D('',#48189,#36161,#36162);
#31842=AXIS2_PLACEMENT_3D('',#48191,#36164,#36165);
#31843=AXIS2_PLACEMENT_3D('',#48195,#36168,#36169);
#31844=AXIS2_PLACEMENT_3D('',#48196,#36170,#36171);
#31845=AXIS2_PLACEMENT_3D('',#48197,#36172,#36173);
#31846=AXIS2_PLACEMENT_3D('',#48206,#36178,#36179);
#31847=AXIS2_PLACEMENT_3D('',#48208,#36180,#36181);
#31848=AXIS2_PLACEMENT_3D('',#48210,#36183,#36184);
#31849=AXIS2_PLACEMENT_3D('',#48214,#36187,#36188);
#31850=AXIS2_PLACEMENT_3D('',#48215,#36189,#36190);
#31851=AXIS2_PLACEMENT_3D('',#48216,#36191,#36192);
#31852=AXIS2_PLACEMENT_3D('',#48225,#36197,#36198);
#31853=AXIS2_PLACEMENT_3D('',#48227,#36199,#36200);
#31854=AXIS2_PLACEMENT_3D('',#48229,#36202,#36203);
#31855=AXIS2_PLACEMENT_3D('',#48233,#36206,#36207);
#31856=AXIS2_PLACEMENT_3D('',#48234,#36208,#36209);
#31857=AXIS2_PLACEMENT_3D('',#48235,#36210,#36211);
#31858=AXIS2_PLACEMENT_3D('',#48244,#36216,#36217);
#31859=AXIS2_PLACEMENT_3D('',#48246,#36218,#36219);
#31860=AXIS2_PLACEMENT_3D('',#48248,#36221,#36222);
#31861=AXIS2_PLACEMENT_3D('',#48252,#36225,#36226);
#31862=AXIS2_PLACEMENT_3D('',#48253,#36227,#36228);
#31863=AXIS2_PLACEMENT_3D('',#48254,#36229,#36230);
#31864=AXIS2_PLACEMENT_3D('',#48263,#36235,#36236);
#31865=AXIS2_PLACEMENT_3D('',#48265,#36237,#36238);
#31866=AXIS2_PLACEMENT_3D('',#48267,#36240,#36241);
#31867=AXIS2_PLACEMENT_3D('',#48271,#36244,#36245);
#31868=AXIS2_PLACEMENT_3D('',#48272,#36246,#36247);
#31869=AXIS2_PLACEMENT_3D('',#48273,#36248,#36249);
#31870=AXIS2_PLACEMENT_3D('',#48282,#36254,#36255);
#31871=AXIS2_PLACEMENT_3D('',#48284,#36256,#36257);
#31872=AXIS2_PLACEMENT_3D('',#48286,#36259,#36260);
#31873=AXIS2_PLACEMENT_3D('',#48290,#36263,#36264);
#31874=AXIS2_PLACEMENT_3D('',#48291,#36265,#36266);
#31875=AXIS2_PLACEMENT_3D('',#48292,#36267,#36268);
#31876=AXIS2_PLACEMENT_3D('',#48301,#36273,#36274);
#31877=AXIS2_PLACEMENT_3D('',#48303,#36275,#36276);
#31878=AXIS2_PLACEMENT_3D('',#48305,#36278,#36279);
#31879=AXIS2_PLACEMENT_3D('',#48309,#36282,#36283);
#31880=AXIS2_PLACEMENT_3D('',#48310,#36284,#36285);
#31881=AXIS2_PLACEMENT_3D('',#48311,#36286,#36287);
#31882=AXIS2_PLACEMENT_3D('',#48320,#36292,#36293);
#31883=AXIS2_PLACEMENT_3D('',#48322,#36294,#36295);
#31884=AXIS2_PLACEMENT_3D('',#48324,#36297,#36298);
#31885=AXIS2_PLACEMENT_3D('',#48328,#36301,#36302);
#31886=AXIS2_PLACEMENT_3D('',#48329,#36303,#36304);
#31887=AXIS2_PLACEMENT_3D('',#48330,#36305,#36306);
#31888=AXIS2_PLACEMENT_3D('',#48339,#36311,#36312);
#31889=AXIS2_PLACEMENT_3D('',#48341,#36313,#36314);
#31890=AXIS2_PLACEMENT_3D('',#48343,#36316,#36317);
#31891=AXIS2_PLACEMENT_3D('',#48347,#36320,#36321);
#31892=AXIS2_PLACEMENT_3D('',#48348,#36322,#36323);
#31893=AXIS2_PLACEMENT_3D('',#48349,#36324,#36325);
#31894=AXIS2_PLACEMENT_3D('',#48358,#36330,#36331);
#31895=AXIS2_PLACEMENT_3D('',#48360,#36332,#36333);
#31896=AXIS2_PLACEMENT_3D('',#48362,#36335,#36336);
#31897=AXIS2_PLACEMENT_3D('',#48366,#36339,#36340);
#31898=AXIS2_PLACEMENT_3D('',#48367,#36341,#36342);
#31899=AXIS2_PLACEMENT_3D('',#48368,#36343,#36344);
#31900=AXIS2_PLACEMENT_3D('',#48377,#36349,#36350);
#31901=AXIS2_PLACEMENT_3D('',#48379,#36351,#36352);
#31902=AXIS2_PLACEMENT_3D('',#48381,#36354,#36355);
#31903=AXIS2_PLACEMENT_3D('',#48385,#36358,#36359);
#31904=AXIS2_PLACEMENT_3D('',#48386,#36360,#36361);
#31905=AXIS2_PLACEMENT_3D('',#48387,#36362,#36363);
#31906=AXIS2_PLACEMENT_3D('',#48396,#36368,#36369);
#31907=AXIS2_PLACEMENT_3D('',#48398,#36370,#36371);
#31908=AXIS2_PLACEMENT_3D('',#48400,#36373,#36374);
#31909=AXIS2_PLACEMENT_3D('',#48404,#36377,#36378);
#31910=AXIS2_PLACEMENT_3D('',#48405,#36379,#36380);
#31911=AXIS2_PLACEMENT_3D('',#48406,#36381,#36382);
#31912=AXIS2_PLACEMENT_3D('',#48415,#36387,#36388);
#31913=AXIS2_PLACEMENT_3D('',#48417,#36389,#36390);
#31914=AXIS2_PLACEMENT_3D('',#48419,#36392,#36393);
#31915=AXIS2_PLACEMENT_3D('',#48423,#36396,#36397);
#31916=AXIS2_PLACEMENT_3D('',#48424,#36398,#36399);
#31917=AXIS2_PLACEMENT_3D('',#48425,#36400,#36401);
#31918=AXIS2_PLACEMENT_3D('',#48434,#36406,#36407);
#31919=AXIS2_PLACEMENT_3D('',#48436,#36408,#36409);
#31920=AXIS2_PLACEMENT_3D('',#48439,#36411,#36412);
#31921=AXIS2_PLACEMENT_3D('',#48440,#36413,#36414);
#31922=AXIS2_PLACEMENT_3D('',#48444,#36417,#36418);
#31923=AXIS2_PLACEMENT_3D('',#48446,#36419,#36420);
#31924=AXIS2_PLACEMENT_3D('',#48447,#36421,#36422);
#31925=AXIS2_PLACEMENT_3D('',#48448,#36423,#36424);
#31926=AXIS2_PLACEMENT_3D('',#48457,#36429,#36430);
#31927=AXIS2_PLACEMENT_3D('',#48459,#36431,#36432);
#31928=AXIS2_PLACEMENT_3D('',#48461,#36434,#36435);
#31929=AXIS2_PLACEMENT_3D('',#48465,#36438,#36439);
#31930=AXIS2_PLACEMENT_3D('',#48466,#36440,#36441);
#31931=AXIS2_PLACEMENT_3D('',#48467,#36442,#36443);
#31932=AXIS2_PLACEMENT_3D('',#48476,#36448,#36449);
#31933=AXIS2_PLACEMENT_3D('',#48478,#36450,#36451);
#31934=AXIS2_PLACEMENT_3D('',#48480,#36453,#36454);
#31935=AXIS2_PLACEMENT_3D('',#48484,#36457,#36458);
#31936=AXIS2_PLACEMENT_3D('',#48485,#36459,#36460);
#31937=AXIS2_PLACEMENT_3D('',#48486,#36461,#36462);
#31938=AXIS2_PLACEMENT_3D('',#48495,#36467,#36468);
#31939=AXIS2_PLACEMENT_3D('',#48497,#36469,#36470);
#31940=AXIS2_PLACEMENT_3D('',#48499,#36472,#36473);
#31941=AXIS2_PLACEMENT_3D('',#48503,#36476,#36477);
#31942=AXIS2_PLACEMENT_3D('',#48504,#36478,#36479);
#31943=AXIS2_PLACEMENT_3D('',#48505,#36480,#36481);
#31944=AXIS2_PLACEMENT_3D('',#48514,#36486,#36487);
#31945=AXIS2_PLACEMENT_3D('',#48516,#36488,#36489);
#31946=AXIS2_PLACEMENT_3D('',#48518,#36491,#36492);
#31947=AXIS2_PLACEMENT_3D('',#48522,#36495,#36496);
#31948=AXIS2_PLACEMENT_3D('',#48523,#36497,#36498);
#31949=AXIS2_PLACEMENT_3D('',#48524,#36499,#36500);
#31950=AXIS2_PLACEMENT_3D('',#48533,#36505,#36506);
#31951=AXIS2_PLACEMENT_3D('',#48535,#36507,#36508);
#31952=AXIS2_PLACEMENT_3D('',#48537,#36510,#36511);
#31953=AXIS2_PLACEMENT_3D('',#48541,#36514,#36515);
#31954=AXIS2_PLACEMENT_3D('',#48542,#36516,#36517);
#31955=AXIS2_PLACEMENT_3D('',#48543,#36518,#36519);
#31956=AXIS2_PLACEMENT_3D('',#48552,#36524,#36525);
#31957=AXIS2_PLACEMENT_3D('',#48554,#36526,#36527);
#31958=AXIS2_PLACEMENT_3D('',#48556,#36529,#36530);
#31959=AXIS2_PLACEMENT_3D('',#48560,#36533,#36534);
#31960=AXIS2_PLACEMENT_3D('',#48561,#36535,#36536);
#31961=AXIS2_PLACEMENT_3D('',#48562,#36537,#36538);
#31962=AXIS2_PLACEMENT_3D('',#48571,#36543,#36544);
#31963=AXIS2_PLACEMENT_3D('',#48573,#36545,#36546);
#31964=AXIS2_PLACEMENT_3D('',#48575,#36548,#36549);
#31965=AXIS2_PLACEMENT_3D('',#48579,#36552,#36553);
#31966=AXIS2_PLACEMENT_3D('',#48580,#36554,#36555);
#31967=AXIS2_PLACEMENT_3D('',#48581,#36556,#36557);
#31968=AXIS2_PLACEMENT_3D('',#48590,#36562,#36563);
#31969=AXIS2_PLACEMENT_3D('',#48592,#36564,#36565);
#31970=AXIS2_PLACEMENT_3D('',#48594,#36567,#36568);
#31971=AXIS2_PLACEMENT_3D('',#48598,#36571,#36572);
#31972=AXIS2_PLACEMENT_3D('',#48599,#36573,#36574);
#31973=AXIS2_PLACEMENT_3D('',#48600,#36575,#36576);
#31974=AXIS2_PLACEMENT_3D('',#48609,#36581,#36582);
#31975=AXIS2_PLACEMENT_3D('',#48611,#36583,#36584);
#31976=AXIS2_PLACEMENT_3D('',#48613,#36586,#36587);
#31977=AXIS2_PLACEMENT_3D('',#48617,#36590,#36591);
#31978=AXIS2_PLACEMENT_3D('',#48618,#36592,#36593);
#31979=AXIS2_PLACEMENT_3D('',#48619,#36594,#36595);
#31980=AXIS2_PLACEMENT_3D('',#48628,#36600,#36601);
#31981=AXIS2_PLACEMENT_3D('',#48630,#36602,#36603);
#31982=AXIS2_PLACEMENT_3D('',#48632,#36605,#36606);
#31983=AXIS2_PLACEMENT_3D('',#48636,#36609,#36610);
#31984=AXIS2_PLACEMENT_3D('',#48637,#36611,#36612);
#31985=AXIS2_PLACEMENT_3D('',#48638,#36613,#36614);
#31986=AXIS2_PLACEMENT_3D('',#48647,#36619,#36620);
#31987=AXIS2_PLACEMENT_3D('',#48649,#36621,#36622);
#31988=AXIS2_PLACEMENT_3D('',#48651,#36624,#36625);
#31989=AXIS2_PLACEMENT_3D('',#48655,#36628,#36629);
#31990=AXIS2_PLACEMENT_3D('',#48656,#36630,#36631);
#31991=AXIS2_PLACEMENT_3D('',#48657,#36632,#36633);
#31992=AXIS2_PLACEMENT_3D('',#48666,#36638,#36639);
#31993=AXIS2_PLACEMENT_3D('',#48668,#36640,#36641);
#31994=AXIS2_PLACEMENT_3D('',#48670,#36643,#36644);
#31995=AXIS2_PLACEMENT_3D('',#48674,#36647,#36648);
#31996=AXIS2_PLACEMENT_3D('',#48675,#36649,#36650);
#31997=AXIS2_PLACEMENT_3D('',#48676,#36651,#36652);
#31998=AXIS2_PLACEMENT_3D('',#48685,#36657,#36658);
#31999=AXIS2_PLACEMENT_3D('',#48687,#36659,#36660);
#32000=AXIS2_PLACEMENT_3D('',#48689,#36662,#36663);
#32001=AXIS2_PLACEMENT_3D('',#48693,#36666,#36667);
#32002=AXIS2_PLACEMENT_3D('',#48694,#36668,#36669);
#32003=AXIS2_PLACEMENT_3D('',#48695,#36670,#36671);
#32004=AXIS2_PLACEMENT_3D('',#48704,#36676,#36677);
#32005=AXIS2_PLACEMENT_3D('',#48706,#36678,#36679);
#32006=AXIS2_PLACEMENT_3D('',#48708,#36681,#36682);
#32007=AXIS2_PLACEMENT_3D('',#48712,#36685,#36686);
#32008=AXIS2_PLACEMENT_3D('',#48713,#36687,#36688);
#32009=AXIS2_PLACEMENT_3D('',#48714,#36689,#36690);
#32010=AXIS2_PLACEMENT_3D('',#48723,#36695,#36696);
#32011=AXIS2_PLACEMENT_3D('',#48725,#36697,#36698);
#32012=AXIS2_PLACEMENT_3D('',#48727,#36700,#36701);
#32013=AXIS2_PLACEMENT_3D('',#48731,#36704,#36705);
#32014=AXIS2_PLACEMENT_3D('',#48732,#36706,#36707);
#32015=AXIS2_PLACEMENT_3D('',#48733,#36708,#36709);
#32016=AXIS2_PLACEMENT_3D('',#48742,#36714,#36715);
#32017=AXIS2_PLACEMENT_3D('',#48744,#36716,#36717);
#32018=AXIS2_PLACEMENT_3D('',#48746,#36719,#36720);
#32019=AXIS2_PLACEMENT_3D('',#48750,#36723,#36724);
#32020=AXIS2_PLACEMENT_3D('',#48751,#36725,#36726);
#32021=AXIS2_PLACEMENT_3D('',#48752,#36727,#36728);
#32022=AXIS2_PLACEMENT_3D('',#48761,#36733,#36734);
#32023=AXIS2_PLACEMENT_3D('',#48763,#36735,#36736);
#32024=AXIS2_PLACEMENT_3D('',#48765,#36738,#36739);
#32025=AXIS2_PLACEMENT_3D('',#48769,#36742,#36743);
#32026=AXIS2_PLACEMENT_3D('',#48770,#36744,#36745);
#32027=AXIS2_PLACEMENT_3D('',#48771,#36746,#36747);
#32028=AXIS2_PLACEMENT_3D('',#48780,#36752,#36753);
#32029=AXIS2_PLACEMENT_3D('',#48782,#36754,#36755);
#32030=AXIS2_PLACEMENT_3D('',#48784,#36757,#36758);
#32031=AXIS2_PLACEMENT_3D('',#48788,#36761,#36762);
#32032=AXIS2_PLACEMENT_3D('',#48789,#36763,#36764);
#32033=AXIS2_PLACEMENT_3D('',#48790,#36765,#36766);
#32034=AXIS2_PLACEMENT_3D('',#48794,#36768,#36769);
#32035=AXIS2_PLACEMENT_3D('',#48795,#36770,#36771);
#32036=AXIS2_PLACEMENT_3D('',#48804,#36776,#36777);
#32037=AXIS2_PLACEMENT_3D('',#48810,#36781,#36782);
#32038=AXIS2_PLACEMENT_3D('',#48816,#36786,#36787);
#32039=AXIS2_PLACEMENT_3D('',#48822,#36791,#36792);
#32040=AXIS2_PLACEMENT_3D('',#48828,#36796,#36797);
#32041=AXIS2_PLACEMENT_3D('',#48831,#36800,#36801);
#32042=AXIS2_PLACEMENT_3D('',#48832,#36802,#36803);
#32043=AXIS2_PLACEMENT_3D('',#48835,#36804,#36805);
#32044=AXIS2_PLACEMENT_3D('',#48837,#36806,#36807);
#32045=AXIS2_PLACEMENT_3D('',#48838,#36808,#36809);
#32046=AXIS2_PLACEMENT_3D('',#48839,#36810,#36811);
#32047=AXIS2_PLACEMENT_3D('',#48840,#36812,#36813);
#32048=AXIS2_PLACEMENT_3D('',#48843,#36815,#36816);
#32049=AXIS2_PLACEMENT_3D('',#48844,#36817,#36818);
#32050=AXIS2_PLACEMENT_3D('',#48846,#36819,#36820);
#32051=AXIS2_PLACEMENT_3D('',#48847,#36821,#36822);
#32052=AXIS2_PLACEMENT_3D('',#48849,#36823,#36824);
#32053=AXIS2_PLACEMENT_3D('',#48850,#36825,#36826);
#32054=AXIS2_PLACEMENT_3D('',#48852,#36828,#36829);
#32055=AXIS2_PLACEMENT_3D('',#48853,#36830,#36831);
#32056=AXIS2_PLACEMENT_3D('',#48854,#36832,#36833);
#32057=AXIS2_PLACEMENT_3D('',#48856,#36834,#36835);
#32058=AXIS2_PLACEMENT_3D('',#48858,#36837,#36838);
#32059=AXIS2_PLACEMENT_3D('',#48860,#36839,#36840);
#32060=AXIS2_PLACEMENT_3D('',#48862,#36842,#36843);
#32061=AXIS2_PLACEMENT_3D('',#48863,#36844,#36845);
#32062=AXIS2_PLACEMENT_3D('',#48865,#36846,#36847);
#32063=AXIS2_PLACEMENT_3D('',#48868,#36850,#36851);
#32064=AXIS2_PLACEMENT_3D('',#48870,#36852,#36853);
#32065=AXIS2_PLACEMENT_3D('',#48872,#36855,#36856);
#32066=AXIS2_PLACEMENT_3D('',#48873,#36857,#36858);
#32067=AXIS2_PLACEMENT_3D('',#48874,#36859,#36860);
#32068=AXIS2_PLACEMENT_3D('',#48876,#36861,#36862);
#32069=AXIS2_PLACEMENT_3D('',#48879,#36864,#36865);
#32070=AXIS2_PLACEMENT_3D('',#48880,#36866,#36867);
#32071=AXIS2_PLACEMENT_3D('',#48882,#36868,#36869);
#32072=AXIS2_PLACEMENT_3D('',#48883,#36870,#36871);
#32073=AXIS2_PLACEMENT_3D('',#48885,#36872,#36873);
#32074=AXIS2_PLACEMENT_3D('',#48887,#36875,#36876);
#32075=AXIS2_PLACEMENT_3D('',#48888,#36877,#36878);
#32076=AXIS2_PLACEMENT_3D('',#48889,#36879,#36880);
#32077=AXIS2_PLACEMENT_3D('',#48892,#36881,#36882);
#32078=AXIS2_PLACEMENT_3D('',#48893,#36883,#36884);
#32079=AXIS2_PLACEMENT_3D('',#48894,#36885,#36886);
#32080=AXIS2_PLACEMENT_3D('',#48896,#36887,#36888);
#32081=AXIS2_PLACEMENT_3D('',#48897,#36889,#36890);
#32082=AXIS2_PLACEMENT_3D('',#48899,#36891,#36892);
#32083=AXIS2_PLACEMENT_3D('',#48901,#36894,#36895);
#32084=AXIS2_PLACEMENT_3D('',#48903,#36896,#36897);
#32085=AXIS2_PLACEMENT_3D('',#48905,#36899,#36900);
#32086=AXIS2_PLACEMENT_3D('',#48907,#36901,#36902);
#32087=AXIS2_PLACEMENT_3D('',#48909,#36904,#36905);
#32088=AXIS2_PLACEMENT_3D('',#48910,#36906,#36907);
#32089=AXIS2_PLACEMENT_3D('',#49482,#36908,#36909);
#32090=AXIS2_PLACEMENT_3D('',#49541,#36910,#36911);
#32091=AXIS2_PLACEMENT_3D('',#49542,#36912,#36913);
#32092=AXIS2_PLACEMENT_3D('',#49543,#36914,#36915);
#32093=AXIS2_PLACEMENT_3D('',#49544,#36916,#36917);
#32094=AXIS2_PLACEMENT_3D('',#49545,#36918,#36919);
#32095=AXIS2_PLACEMENT_3D('',#49547,#36920,#36921);
#32096=AXIS2_PLACEMENT_3D('',#49551,#36923,#36924);
#32097=AXIS2_PLACEMENT_3D('',#49552,#36925,#36926);
#32098=AXIS2_PLACEMENT_3D('',#49553,#36927,#36928);
#32099=AXIS2_PLACEMENT_3D('',#49556,#36930,#36931);
#32100=AXIS2_PLACEMENT_3D('',#49557,#36932,#36933);
#32101=AXIS2_PLACEMENT_3D('',#49559,#36934,#36935);
#32102=AXIS2_PLACEMENT_3D('',#49560,#36936,#36937);
#32103=AXIS2_PLACEMENT_3D('',#49563,#36939,#36940);
#32104=AXIS2_PLACEMENT_3D('',#49564,#36941,#36942);
#32105=AXIS2_PLACEMENT_3D('',#49566,#36943,#36944);
#32106=AXIS2_PLACEMENT_3D('',#49567,#36945,#36946);
#32107=AXIS2_PLACEMENT_3D('',#49569,#36948,#36949);
#32108=AXIS2_PLACEMENT_3D('',#49570,#36950,#36951);
#32109=AXIS2_PLACEMENT_3D('',#49586,#36953,#36954);
#32110=AXIS2_PLACEMENT_3D('',#49594,#36955,#36956);
#32111=AXIS2_PLACEMENT_3D('',#49642,#36958,#36959);
#32112=AXIS2_PLACEMENT_3D('',#49690,#36961,#36962);
#32113=AXIS2_PLACEMENT_3D('',#49741,#36964,#36965);
#32114=AXIS2_PLACEMENT_3D('',#49792,#36967,#36968);
#32115=AXIS2_PLACEMENT_3D('',#49840,#36970,#36971);
#32116=AXIS2_PLACEMENT_3D('',#49888,#36973,#36974);
#32117=AXIS2_PLACEMENT_3D('',#49942,#36976,#36977);
#32118=AXIS2_PLACEMENT_3D('',#49990,#36979,#36980);
#32119=AXIS2_PLACEMENT_3D('',#50038,#36982,#36983);
#32120=AXIS2_PLACEMENT_3D('',#50092,#36985,#36986);
#32121=AXIS2_PLACEMENT_3D('',#50140,#36988,#36989);
#32122=AXIS2_PLACEMENT_3D('',#50188,#36991,#36992);
#32123=AXIS2_PLACEMENT_3D('',#50236,#36994,#36995);
#32124=AXIS2_PLACEMENT_3D('',#50290,#36997,#36998);
#32125=AXIS2_PLACEMENT_3D('',#50338,#37000,#37001);
#32126=AXIS2_PLACEMENT_3D('',#50386,#37003,#37004);
#32127=AXIS2_PLACEMENT_3D('',#50440,#37006,#37007);
#32128=AXIS2_PLACEMENT_3D('',#50488,#37009,#37010);
#32129=AXIS2_PLACEMENT_3D('',#50536,#37012,#37013);
#32130=AXIS2_PLACEMENT_3D('',#50590,#37015,#37016);
#32131=AXIS2_PLACEMENT_3D('',#50638,#37018,#37019);
#32132=AXIS2_PLACEMENT_3D('',#50686,#37021,#37022);
#32133=AXIS2_PLACEMENT_3D('',#50734,#37024,#37025);
#32134=AXIS2_PLACEMENT_3D('',#50788,#37027,#37028);
#32135=AXIS2_PLACEMENT_3D('',#50836,#37030,#37031);
#32136=AXIS2_PLACEMENT_3D('',#50884,#37033,#37034);
#32137=AXIS2_PLACEMENT_3D('',#50938,#37036,#37037);
#32138=AXIS2_PLACEMENT_3D('',#50986,#37039,#37040);
#32139=AXIS2_PLACEMENT_3D('',#51034,#37042,#37043);
#32140=AXIS2_PLACEMENT_3D('',#51088,#37045,#37046);
#32141=AXIS2_PLACEMENT_3D('',#51136,#37048,#37049);
#32142=AXIS2_PLACEMENT_3D('',#51184,#37051,#37052);
#32143=AXIS2_PLACEMENT_3D('',#51232,#37054,#37055);
#32144=AXIS2_PLACEMENT_3D('',#51286,#37057,#37058);
#32145=AXIS2_PLACEMENT_3D('',#51334,#37060,#37061);
#32146=AXIS2_PLACEMENT_3D('',#51382,#37063,#37064);
#32147=AXIS2_PLACEMENT_3D('',#51436,#37066,#37067);
#32148=AXIS2_PLACEMENT_3D('',#51484,#37069,#37070);
#32149=AXIS2_PLACEMENT_3D('',#51532,#37072,#37073);
#32150=AXIS2_PLACEMENT_3D('',#51586,#37075,#37076);
#32151=AXIS2_PLACEMENT_3D('',#51634,#37078,#37079);
#32152=AXIS2_PLACEMENT_3D('',#51646,#37081,#37082);
#32153=AXIS2_PLACEMENT_3D('',#51652,#37083,#37084);
#32154=AXIS2_PLACEMENT_3D('',#51676,#37086,#37087);
#32155=AXIS2_PLACEMENT_3D('',#51701,#37089,#37090);
#32156=AXIS2_PLACEMENT_3D('',#51726,#37092,#37093);
#32157=AXIS2_PLACEMENT_3D('',#51750,#37095,#37096);
#32158=AXIS2_PLACEMENT_3D('',#51775,#37098,#37099);
#32159=AXIS2_PLACEMENT_3D('',#51800,#37101,#37102);
#32160=AXIS2_PLACEMENT_3D('',#51824,#37104,#37105);
#32161=AXIS2_PLACEMENT_3D('',#51849,#37107,#37108);
#32162=AXIS2_PLACEMENT_3D('',#51874,#37110,#37111);
#32163=AXIS2_PLACEMENT_3D('',#51898,#37113,#37114);
#32164=AXIS2_PLACEMENT_3D('',#51922,#37116,#37117);
#32165=AXIS2_PLACEMENT_3D('',#51947,#37119,#37120);
#32166=AXIS2_PLACEMENT_3D('',#51972,#37122,#37123);
#32167=AXIS2_PLACEMENT_3D('',#51996,#37125,#37126);
#32168=AXIS2_PLACEMENT_3D('',#52021,#37128,#37129);
#32169=AXIS2_PLACEMENT_3D('',#52046,#37131,#37132);
#32170=AXIS2_PLACEMENT_3D('',#52070,#37134,#37135);
#32171=AXIS2_PLACEMENT_3D('',#52095,#37137,#37138);
#32172=AXIS2_PLACEMENT_3D('',#52120,#37140,#37141);
#32173=AXIS2_PLACEMENT_3D('',#52144,#37143,#37144);
#32174=AXIS2_PLACEMENT_3D('',#52168,#37146,#37147);
#32175=AXIS2_PLACEMENT_3D('',#52193,#37149,#37150);
#32176=AXIS2_PLACEMENT_3D('',#52218,#37152,#37153);
#32177=AXIS2_PLACEMENT_3D('',#52242,#37155,#37156);
#32178=AXIS2_PLACEMENT_3D('',#52267,#37158,#37159);
#32179=AXIS2_PLACEMENT_3D('',#52292,#37161,#37162);
#32180=AXIS2_PLACEMENT_3D('',#52316,#37164,#37165);
#32181=AXIS2_PLACEMENT_3D('',#52341,#37167,#37168);
#32182=AXIS2_PLACEMENT_3D('',#52366,#37170,#37171);
#32183=AXIS2_PLACEMENT_3D('',#52390,#37173,#37174);
#32184=AXIS2_PLACEMENT_3D('',#52414,#37176,#37177);
#32185=AXIS2_PLACEMENT_3D('',#52439,#37179,#37180);
#32186=AXIS2_PLACEMENT_3D('',#52464,#37182,#37183);
#32187=AXIS2_PLACEMENT_3D('',#52488,#37185,#37186);
#32188=AXIS2_PLACEMENT_3D('',#52513,#37188,#37189);
#32189=AXIS2_PLACEMENT_3D('',#52538,#37191,#37192);
#32190=AXIS2_PLACEMENT_3D('',#52562,#37194,#37195);
#32191=AXIS2_PLACEMENT_3D('',#52587,#37197,#37198);
#32192=AXIS2_PLACEMENT_3D('',#52611,#37200,#37201);
#32193=AXIS2_PLACEMENT_3D('',#52636,#37203,#37204);
#32194=AXIS2_PLACEMENT_3D('',#52660,#37206,#37207);
#32195=AXIS2_PLACEMENT_3D('',#52748,#37208,#37209);
#32196=AXIS2_PLACEMENT_3D('',#54028,#37210,#37211);
#32197=AXIS2_PLACEMENT_3D('',#54030,#37212,#37213);
#32198=AXIS2_PLACEMENT_3D('',#54031,#37214,#37215);
#32199=AXIS2_PLACEMENT_3D('',#54118,#37216,#37217);
#32200=AXIS2_PLACEMENT_3D('',#54119,#37218,#37219);
#32201=AXIS2_PLACEMENT_3D('',#55224,#37220,#37221);
#32202=AXIS2_PLACEMENT_3D('',#55226,#37222,#37223);
#32203=AXIS2_PLACEMENT_3D('',#55228,#37224,#37225);
#32204=AXIS2_PLACEMENT_3D('',#55229,#37226,#37227);
#32205=AXIS2_PLACEMENT_3D('',#55230,#37228,#37229);
#32206=AXIS2_PLACEMENT_3D('',#55231,#37230,#37231);
#32207=AXIS2_PLACEMENT_3D('',#55232,#37232,#37233);
#32208=AXIS2_PLACEMENT_3D('',#55234,#37234,#37235);
#32209=AXIS2_PLACEMENT_3D('',#55235,#37236,#37237);
#32210=AXIS2_PLACEMENT_3D('',#55244,#37242,#37243);
#32211=AXIS2_PLACEMENT_3D('',#55246,#37244,#37245);
#32212=AXIS2_PLACEMENT_3D('',#55248,#37247,#37248);
#32213=AXIS2_PLACEMENT_3D('',#55252,#37251,#37252);
#32214=AXIS2_PLACEMENT_3D('',#55253,#37253,#37254);
#32215=AXIS2_PLACEMENT_3D('',#55254,#37255,#37256);
#32216=AXIS2_PLACEMENT_3D('',#55263,#37261,#37262);
#32217=AXIS2_PLACEMENT_3D('',#55265,#37263,#37264);
#32218=AXIS2_PLACEMENT_3D('',#55267,#37266,#37267);
#32219=AXIS2_PLACEMENT_3D('',#55271,#37270,#37271);
#32220=AXIS2_PLACEMENT_3D('',#55272,#37272,#37273);
#32221=AXIS2_PLACEMENT_3D('',#55273,#37274,#37275);
#32222=AXIS2_PLACEMENT_3D('',#55282,#37280,#37281);
#32223=AXIS2_PLACEMENT_3D('',#55284,#37282,#37283);
#32224=AXIS2_PLACEMENT_3D('',#55286,#37285,#37286);
#32225=AXIS2_PLACEMENT_3D('',#55290,#37289,#37290);
#32226=AXIS2_PLACEMENT_3D('',#55291,#37291,#37292);
#32227=AXIS2_PLACEMENT_3D('',#55292,#37293,#37294);
#32228=AXIS2_PLACEMENT_3D('',#55301,#37299,#37300);
#32229=AXIS2_PLACEMENT_3D('',#55303,#37301,#37302);
#32230=AXIS2_PLACEMENT_3D('',#55305,#37304,#37305);
#32231=AXIS2_PLACEMENT_3D('',#55309,#37308,#37309);
#32232=AXIS2_PLACEMENT_3D('',#55310,#37310,#37311);
#32233=AXIS2_PLACEMENT_3D('',#55311,#37312,#37313);
#32234=AXIS2_PLACEMENT_3D('',#55320,#37318,#37319);
#32235=AXIS2_PLACEMENT_3D('',#55322,#37320,#37321);
#32236=AXIS2_PLACEMENT_3D('',#55324,#37323,#37324);
#32237=AXIS2_PLACEMENT_3D('',#55328,#37327,#37328);
#32238=AXIS2_PLACEMENT_3D('',#55329,#37329,#37330);
#32239=AXIS2_PLACEMENT_3D('',#55330,#37331,#37332);
#32240=AXIS2_PLACEMENT_3D('',#55339,#37337,#37338);
#32241=AXIS2_PLACEMENT_3D('',#55341,#37339,#37340);
#32242=AXIS2_PLACEMENT_3D('',#55343,#37342,#37343);
#32243=AXIS2_PLACEMENT_3D('',#55347,#37346,#37347);
#32244=AXIS2_PLACEMENT_3D('',#55348,#37348,#37349);
#32245=AXIS2_PLACEMENT_3D('',#55349,#37350,#37351);
#32246=AXIS2_PLACEMENT_3D('',#55358,#37356,#37357);
#32247=AXIS2_PLACEMENT_3D('',#55360,#37358,#37359);
#32248=AXIS2_PLACEMENT_3D('',#55362,#37361,#37362);
#32249=AXIS2_PLACEMENT_3D('',#55366,#37365,#37366);
#32250=AXIS2_PLACEMENT_3D('',#55367,#37367,#37368);
#32251=AXIS2_PLACEMENT_3D('',#55368,#37369,#37370);
#32252=AXIS2_PLACEMENT_3D('',#55377,#37375,#37376);
#32253=AXIS2_PLACEMENT_3D('',#55379,#37377,#37378);
#32254=AXIS2_PLACEMENT_3D('',#55381,#37380,#37381);
#32255=AXIS2_PLACEMENT_3D('',#55385,#37384,#37385);
#32256=AXIS2_PLACEMENT_3D('',#55386,#37386,#37387);
#32257=AXIS2_PLACEMENT_3D('',#55387,#37388,#37389);
#32258=AXIS2_PLACEMENT_3D('',#55396,#37394,#37395);
#32259=AXIS2_PLACEMENT_3D('',#55398,#37396,#37397);
#32260=AXIS2_PLACEMENT_3D('',#55400,#37399,#37400);
#32261=AXIS2_PLACEMENT_3D('',#55404,#37403,#37404);
#32262=AXIS2_PLACEMENT_3D('',#55405,#37405,#37406);
#32263=AXIS2_PLACEMENT_3D('',#55406,#37407,#37408);
#32264=AXIS2_PLACEMENT_3D('',#55415,#37413,#37414);
#32265=AXIS2_PLACEMENT_3D('',#55417,#37415,#37416);
#32266=AXIS2_PLACEMENT_3D('',#55419,#37418,#37419);
#32267=AXIS2_PLACEMENT_3D('',#55423,#37422,#37423);
#32268=AXIS2_PLACEMENT_3D('',#55424,#37424,#37425);
#32269=AXIS2_PLACEMENT_3D('',#55425,#37426,#37427);
#32270=AXIS2_PLACEMENT_3D('',#55434,#37432,#37433);
#32271=AXIS2_PLACEMENT_3D('',#55436,#37434,#37435);
#32272=AXIS2_PLACEMENT_3D('',#55438,#37437,#37438);
#32273=AXIS2_PLACEMENT_3D('',#55442,#37441,#37442);
#32274=AXIS2_PLACEMENT_3D('',#55443,#37443,#37444);
#32275=AXIS2_PLACEMENT_3D('',#55444,#37445,#37446);
#32276=AXIS2_PLACEMENT_3D('',#55453,#37451,#37452);
#32277=AXIS2_PLACEMENT_3D('',#55455,#37453,#37454);
#32278=AXIS2_PLACEMENT_3D('',#55457,#37456,#37457);
#32279=AXIS2_PLACEMENT_3D('',#55461,#37460,#37461);
#32280=AXIS2_PLACEMENT_3D('',#55462,#37462,#37463);
#32281=AXIS2_PLACEMENT_3D('',#55463,#37464,#37465);
#32282=AXIS2_PLACEMENT_3D('',#55472,#37470,#37471);
#32283=AXIS2_PLACEMENT_3D('',#55474,#37472,#37473);
#32284=AXIS2_PLACEMENT_3D('',#55476,#37475,#37476);
#32285=AXIS2_PLACEMENT_3D('',#55480,#37479,#37480);
#32286=AXIS2_PLACEMENT_3D('',#55481,#37481,#37482);
#32287=AXIS2_PLACEMENT_3D('',#55482,#37483,#37484);
#32288=AXIS2_PLACEMENT_3D('',#55491,#37489,#37490);
#32289=AXIS2_PLACEMENT_3D('',#55493,#37491,#37492);
#32290=AXIS2_PLACEMENT_3D('',#55495,#37494,#37495);
#32291=AXIS2_PLACEMENT_3D('',#55499,#37498,#37499);
#32292=AXIS2_PLACEMENT_3D('',#55500,#37500,#37501);
#32293=AXIS2_PLACEMENT_3D('',#55501,#37502,#37503);
#32294=AXIS2_PLACEMENT_3D('',#55510,#37508,#37509);
#32295=AXIS2_PLACEMENT_3D('',#55512,#37510,#37511);
#32296=AXIS2_PLACEMENT_3D('',#55514,#37513,#37514);
#32297=AXIS2_PLACEMENT_3D('',#55518,#37517,#37518);
#32298=AXIS2_PLACEMENT_3D('',#55519,#37519,#37520);
#32299=AXIS2_PLACEMENT_3D('',#55520,#37521,#37522);
#32300=AXIS2_PLACEMENT_3D('',#55529,#37527,#37528);
#32301=AXIS2_PLACEMENT_3D('',#55531,#37529,#37530);
#32302=AXIS2_PLACEMENT_3D('',#55533,#37532,#37533);
#32303=AXIS2_PLACEMENT_3D('',#55537,#37536,#37537);
#32304=AXIS2_PLACEMENT_3D('',#55538,#37538,#37539);
#32305=AXIS2_PLACEMENT_3D('',#55539,#37540,#37541);
#32306=AXIS2_PLACEMENT_3D('',#55548,#37546,#37547);
#32307=AXIS2_PLACEMENT_3D('',#55550,#37548,#37549);
#32308=AXIS2_PLACEMENT_3D('',#55552,#37551,#37552);
#32309=AXIS2_PLACEMENT_3D('',#55556,#37555,#37556);
#32310=AXIS2_PLACEMENT_3D('',#55557,#37557,#37558);
#32311=AXIS2_PLACEMENT_3D('',#55558,#37559,#37560);
#32312=AXIS2_PLACEMENT_3D('',#55567,#37565,#37566);
#32313=AXIS2_PLACEMENT_3D('',#55569,#37567,#37568);
#32314=AXIS2_PLACEMENT_3D('',#55572,#37570,#37571);
#32315=AXIS2_PLACEMENT_3D('',#55573,#37572,#37573);
#32316=AXIS2_PLACEMENT_3D('',#55577,#37576,#37577);
#32317=AXIS2_PLACEMENT_3D('',#55579,#37578,#37579);
#32318=AXIS2_PLACEMENT_3D('',#55580,#37580,#37581);
#32319=AXIS2_PLACEMENT_3D('',#55581,#37582,#37583);
#32320=AXIS2_PLACEMENT_3D('',#55590,#37588,#37589);
#32321=AXIS2_PLACEMENT_3D('',#55592,#37590,#37591);
#32322=AXIS2_PLACEMENT_3D('',#55594,#37593,#37594);
#32323=AXIS2_PLACEMENT_3D('',#55598,#37597,#37598);
#32324=AXIS2_PLACEMENT_3D('',#55599,#37599,#37600);
#32325=AXIS2_PLACEMENT_3D('',#55600,#37601,#37602);
#32326=AXIS2_PLACEMENT_3D('',#55609,#37607,#37608);
#32327=AXIS2_PLACEMENT_3D('',#55611,#37609,#37610);
#32328=AXIS2_PLACEMENT_3D('',#55613,#37612,#37613);
#32329=AXIS2_PLACEMENT_3D('',#55617,#37616,#37617);
#32330=AXIS2_PLACEMENT_3D('',#55618,#37618,#37619);
#32331=AXIS2_PLACEMENT_3D('',#55619,#37620,#37621);
#32332=AXIS2_PLACEMENT_3D('',#55628,#37626,#37627);
#32333=AXIS2_PLACEMENT_3D('',#55630,#37628,#37629);
#32334=AXIS2_PLACEMENT_3D('',#55632,#37631,#37632);
#32335=AXIS2_PLACEMENT_3D('',#55636,#37635,#37636);
#32336=AXIS2_PLACEMENT_3D('',#55637,#37637,#37638);
#32337=AXIS2_PLACEMENT_3D('',#55638,#37639,#37640);
#32338=AXIS2_PLACEMENT_3D('',#55647,#37645,#37646);
#32339=AXIS2_PLACEMENT_3D('',#55649,#37647,#37648);
#32340=AXIS2_PLACEMENT_3D('',#55651,#37650,#37651);
#32341=AXIS2_PLACEMENT_3D('',#55655,#37654,#37655);
#32342=AXIS2_PLACEMENT_3D('',#55656,#37656,#37657);
#32343=AXIS2_PLACEMENT_3D('',#55657,#37658,#37659);
#32344=AXIS2_PLACEMENT_3D('',#55666,#37664,#37665);
#32345=AXIS2_PLACEMENT_3D('',#55668,#37666,#37667);
#32346=AXIS2_PLACEMENT_3D('',#55670,#37669,#37670);
#32347=AXIS2_PLACEMENT_3D('',#55674,#37673,#37674);
#32348=AXIS2_PLACEMENT_3D('',#55675,#37675,#37676);
#32349=AXIS2_PLACEMENT_3D('',#55676,#37677,#37678);
#32350=AXIS2_PLACEMENT_3D('',#55685,#37683,#37684);
#32351=AXIS2_PLACEMENT_3D('',#55687,#37685,#37686);
#32352=AXIS2_PLACEMENT_3D('',#55689,#37688,#37689);
#32353=AXIS2_PLACEMENT_3D('',#55693,#37692,#37693);
#32354=AXIS2_PLACEMENT_3D('',#55694,#37694,#37695);
#32355=AXIS2_PLACEMENT_3D('',#55695,#37696,#37697);
#32356=AXIS2_PLACEMENT_3D('',#55704,#37702,#37703);
#32357=AXIS2_PLACEMENT_3D('',#55706,#37704,#37705);
#32358=AXIS2_PLACEMENT_3D('',#55708,#37707,#37708);
#32359=AXIS2_PLACEMENT_3D('',#55712,#37711,#37712);
#32360=AXIS2_PLACEMENT_3D('',#55713,#37713,#37714);
#32361=AXIS2_PLACEMENT_3D('',#55714,#37715,#37716);
#32362=AXIS2_PLACEMENT_3D('',#55723,#37721,#37722);
#32363=AXIS2_PLACEMENT_3D('',#55725,#37723,#37724);
#32364=AXIS2_PLACEMENT_3D('',#55727,#37726,#37727);
#32365=AXIS2_PLACEMENT_3D('',#55731,#37730,#37731);
#32366=AXIS2_PLACEMENT_3D('',#55732,#37732,#37733);
#32367=AXIS2_PLACEMENT_3D('',#55733,#37734,#37735);
#32368=AXIS2_PLACEMENT_3D('',#55742,#37740,#37741);
#32369=AXIS2_PLACEMENT_3D('',#55744,#37742,#37743);
#32370=AXIS2_PLACEMENT_3D('',#55746,#37745,#37746);
#32371=AXIS2_PLACEMENT_3D('',#55750,#37749,#37750);
#32372=AXIS2_PLACEMENT_3D('',#55751,#37751,#37752);
#32373=AXIS2_PLACEMENT_3D('',#55752,#37753,#37754);
#32374=AXIS2_PLACEMENT_3D('',#55761,#37759,#37760);
#32375=AXIS2_PLACEMENT_3D('',#55763,#37761,#37762);
#32376=AXIS2_PLACEMENT_3D('',#55765,#37764,#37765);
#32377=AXIS2_PLACEMENT_3D('',#55769,#37768,#37769);
#32378=AXIS2_PLACEMENT_3D('',#55770,#37770,#37771);
#32379=AXIS2_PLACEMENT_3D('',#55771,#37772,#37773);
#32380=AXIS2_PLACEMENT_3D('',#55780,#37778,#37779);
#32381=AXIS2_PLACEMENT_3D('',#55782,#37780,#37781);
#32382=AXIS2_PLACEMENT_3D('',#55784,#37783,#37784);
#32383=AXIS2_PLACEMENT_3D('',#55788,#37787,#37788);
#32384=AXIS2_PLACEMENT_3D('',#55789,#37789,#37790);
#32385=AXIS2_PLACEMENT_3D('',#55790,#37791,#37792);
#32386=AXIS2_PLACEMENT_3D('',#55799,#37797,#37798);
#32387=AXIS2_PLACEMENT_3D('',#55801,#37799,#37800);
#32388=AXIS2_PLACEMENT_3D('',#55803,#37802,#37803);
#32389=AXIS2_PLACEMENT_3D('',#55807,#37806,#37807);
#32390=AXIS2_PLACEMENT_3D('',#55808,#37808,#37809);
#32391=AXIS2_PLACEMENT_3D('',#55809,#37810,#37811);
#32392=AXIS2_PLACEMENT_3D('',#55818,#37816,#37817);
#32393=AXIS2_PLACEMENT_3D('',#55820,#37818,#37819);
#32394=AXIS2_PLACEMENT_3D('',#55822,#37821,#37822);
#32395=AXIS2_PLACEMENT_3D('',#55826,#37825,#37826);
#32396=AXIS2_PLACEMENT_3D('',#55827,#37827,#37828);
#32397=AXIS2_PLACEMENT_3D('',#55828,#37829,#37830);
#32398=AXIS2_PLACEMENT_3D('',#55837,#37835,#37836);
#32399=AXIS2_PLACEMENT_3D('',#55839,#37837,#37838);
#32400=AXIS2_PLACEMENT_3D('',#55841,#37840,#37841);
#32401=AXIS2_PLACEMENT_3D('',#55845,#37844,#37845);
#32402=AXIS2_PLACEMENT_3D('',#55846,#37846,#37847);
#32403=AXIS2_PLACEMENT_3D('',#55847,#37848,#37849);
#32404=AXIS2_PLACEMENT_3D('',#55856,#37854,#37855);
#32405=AXIS2_PLACEMENT_3D('',#55858,#37856,#37857);
#32406=AXIS2_PLACEMENT_3D('',#55860,#37859,#37860);
#32407=AXIS2_PLACEMENT_3D('',#55864,#37863,#37864);
#32408=AXIS2_PLACEMENT_3D('',#55865,#37865,#37866);
#32409=AXIS2_PLACEMENT_3D('',#55866,#37867,#37868);
#32410=AXIS2_PLACEMENT_3D('',#55875,#37873,#37874);
#32411=AXIS2_PLACEMENT_3D('',#55877,#37875,#37876);
#32412=AXIS2_PLACEMENT_3D('',#55879,#37878,#37879);
#32413=AXIS2_PLACEMENT_3D('',#55883,#37882,#37883);
#32414=AXIS2_PLACEMENT_3D('',#55884,#37884,#37885);
#32415=AXIS2_PLACEMENT_3D('',#55885,#37886,#37887);
#32416=AXIS2_PLACEMENT_3D('',#55894,#37892,#37893);
#32417=AXIS2_PLACEMENT_3D('',#55896,#37894,#37895);
#32418=AXIS2_PLACEMENT_3D('',#55898,#37897,#37898);
#32419=AXIS2_PLACEMENT_3D('',#55902,#37901,#37902);
#32420=AXIS2_PLACEMENT_3D('',#55903,#37903,#37904);
#32421=AXIS2_PLACEMENT_3D('',#55904,#37905,#37906);
#32422=AXIS2_PLACEMENT_3D('',#55913,#37911,#37912);
#32423=AXIS2_PLACEMENT_3D('',#55915,#37913,#37914);
#32424=AXIS2_PLACEMENT_3D('',#55917,#37916,#37917);
#32425=AXIS2_PLACEMENT_3D('',#55921,#37920,#37921);
#32426=AXIS2_PLACEMENT_3D('',#55922,#37922,#37923);
#32427=AXIS2_PLACEMENT_3D('',#55923,#37924,#37925);
#32428=AXIS2_PLACEMENT_3D('',#55927,#37927,#37928);
#32429=AXIS2_PLACEMENT_3D('',#55928,#37929,#37930);
#32430=AXIS2_PLACEMENT_3D('',#55937,#37935,#37936);
#32431=AXIS2_PLACEMENT_3D('',#55943,#37940,#37941);
#32432=AXIS2_PLACEMENT_3D('',#55949,#37945,#37946);
#32433=AXIS2_PLACEMENT_3D('',#55955,#37950,#37951);
#32434=AXIS2_PLACEMENT_3D('',#55961,#37955,#37956);
#32435=AXIS2_PLACEMENT_3D('',#55964,#37959,#37960);
#32436=AXIS2_PLACEMENT_3D('',#55965,#37961,#37962);
#32437=AXIS2_PLACEMENT_3D('',#55967,#37963,#37964);
#32438=AXIS2_PLACEMENT_3D('',#55968,#37965,#37966);
#32439=AXIS2_PLACEMENT_3D('',#55970,#37968,#37969);
#32440=AXIS2_PLACEMENT_3D('',#55972,#37970,#37971);
#32441=AXIS2_PLACEMENT_3D('',#55975,#37974,#37975);
#32442=AXIS2_PLACEMENT_3D('',#55977,#37976,#37977);
#32443=AXIS2_PLACEMENT_3D('',#55979,#37979,#37980);
#32444=AXIS2_PLACEMENT_3D('',#55980,#37981,#37982);
#32445=AXIS2_PLACEMENT_3D('',#55981,#37983,#37984);
#32446=AXIS2_PLACEMENT_3D('',#55983,#37985,#37986);
#32447=AXIS2_PLACEMENT_3D('',#55984,#37987,#37988);
#32448=AXIS2_PLACEMENT_3D('',#55986,#37989,#37990);
#32449=AXIS2_PLACEMENT_3D('',#55988,#37992,#37993);
#32450=AXIS2_PLACEMENT_3D('',#55990,#37994,#37995);
#32451=AXIS2_PLACEMENT_3D('',#55992,#37997,#37998);
#32452=AXIS2_PLACEMENT_3D('',#55994,#37999,#38000);
#32453=AXIS2_PLACEMENT_3D('',#55996,#38002,#38003);
#32454=AXIS2_PLACEMENT_3D('',#55997,#38004,#38005);
#32455=AXIS2_PLACEMENT_3D('',#55998,#38006,#38007);
#32456=AXIS2_PLACEMENT_3D('',#56014,#38009,#38010);
#32457=AXIS2_PLACEMENT_3D('',#56022,#38011,#38012);
#32458=AXIS2_PLACEMENT_3D('',#56070,#38014,#38015);
#32459=AXIS2_PLACEMENT_3D('',#56118,#38017,#38018);
#32460=AXIS2_PLACEMENT_3D('',#56166,#38020,#38021);
#32461=AXIS2_PLACEMENT_3D('',#56220,#38023,#38024);
#32462=AXIS2_PLACEMENT_3D('',#56268,#38026,#38027);
#32463=AXIS2_PLACEMENT_3D('',#56316,#38029,#38030);
#32464=AXIS2_PLACEMENT_3D('',#56370,#38032,#38033);
#32465=AXIS2_PLACEMENT_3D('',#56418,#38035,#38036);
#32466=AXIS2_PLACEMENT_3D('',#56466,#38038,#38039);
#32467=AXIS2_PLACEMENT_3D('',#56514,#38041,#38042);
#32468=AXIS2_PLACEMENT_3D('',#56568,#38044,#38045);
#32469=AXIS2_PLACEMENT_3D('',#56616,#38047,#38048);
#32470=AXIS2_PLACEMENT_3D('',#56664,#38050,#38051);
#32471=AXIS2_PLACEMENT_3D('',#56718,#38053,#38054);
#32472=AXIS2_PLACEMENT_3D('',#56766,#38056,#38057);
#32473=AXIS2_PLACEMENT_3D('',#56814,#38059,#38060);
#32474=AXIS2_PLACEMENT_3D('',#56862,#38062,#38063);
#32475=AXIS2_PLACEMENT_3D('',#56916,#38065,#38066);
#32476=AXIS2_PLACEMENT_3D('',#56964,#38068,#38069);
#32477=AXIS2_PLACEMENT_3D('',#57012,#38071,#38072);
#32478=AXIS2_PLACEMENT_3D('',#57066,#38074,#38075);
#32479=AXIS2_PLACEMENT_3D('',#57114,#38077,#38078);
#32480=AXIS2_PLACEMENT_3D('',#57162,#38080,#38081);
#32481=AXIS2_PLACEMENT_3D('',#57210,#38083,#38084);
#32482=AXIS2_PLACEMENT_3D('',#57264,#38086,#38087);
#32483=AXIS2_PLACEMENT_3D('',#57312,#38089,#38090);
#32484=AXIS2_PLACEMENT_3D('',#57360,#38092,#38093);
#32485=AXIS2_PLACEMENT_3D('',#57414,#38095,#38096);
#32486=AXIS2_PLACEMENT_3D('',#57462,#38098,#38099);
#32487=AXIS2_PLACEMENT_3D('',#57510,#38101,#38102);
#32488=AXIS2_PLACEMENT_3D('',#57558,#38104,#38105);
#32489=AXIS2_PLACEMENT_3D('',#57612,#38107,#38108);
#32490=AXIS2_PLACEMENT_3D('',#57660,#38110,#38111);
#32491=AXIS2_PLACEMENT_3D('',#57708,#38113,#38114);
#32492=AXIS2_PLACEMENT_3D('',#57762,#38116,#38117);
#32493=AXIS2_PLACEMENT_3D('',#57810,#38119,#38120);
#32494=AXIS2_PLACEMENT_3D('',#57858,#38122,#38123);
#32495=AXIS2_PLACEMENT_3D('',#57906,#38125,#38126);
#32496=AXIS2_PLACEMENT_3D('',#57960,#38128,#38129);
#32497=AXIS2_PLACEMENT_3D('',#58008,#38131,#38132);
#32498=AXIS2_PLACEMENT_3D('',#58056,#38134,#38135);
#32499=AXIS2_PLACEMENT_3D('',#58110,#38137,#38138);
#32500=AXIS2_PLACEMENT_3D('',#58158,#38140,#38141);
#32501=AXIS2_PLACEMENT_3D('',#58206,#38143,#38144);
#32502=AXIS2_PLACEMENT_3D('',#58254,#38146,#38147);
#32503=AXIS2_PLACEMENT_3D('',#58308,#38149,#38150);
#32504=AXIS2_PLACEMENT_3D('',#58356,#38152,#38153);
#32505=AXIS2_PLACEMENT_3D('',#58404,#38155,#38156);
#32506=AXIS2_PLACEMENT_3D('',#58458,#38158,#38159);
#32507=AXIS2_PLACEMENT_3D('',#58506,#38161,#38162);
#32508=AXIS2_PLACEMENT_3D('',#58554,#38164,#38165);
#32509=AXIS2_PLACEMENT_3D('',#58602,#38167,#38168);
#32510=AXIS2_PLACEMENT_3D('',#58656,#38170,#38171);
#32511=AXIS2_PLACEMENT_3D('',#58704,#38173,#38174);
#32512=AXIS2_PLACEMENT_3D('',#58752,#38176,#38177);
#32513=AXIS2_PLACEMENT_3D('',#58806,#38179,#38180);
#32514=AXIS2_PLACEMENT_3D('',#58854,#38182,#38183);
#32515=AXIS2_PLACEMENT_3D('',#58902,#38185,#38186);
#32516=AXIS2_PLACEMENT_3D('',#58950,#38188,#38189);
#32517=AXIS2_PLACEMENT_3D('',#59004,#38191,#38192);
#32518=AXIS2_PLACEMENT_3D('',#59052,#38194,#38195);
#32519=AXIS2_PLACEMENT_3D('',#59100,#38197,#38198);
#32520=AXIS2_PLACEMENT_3D('',#59154,#38200,#38201);
#32521=AXIS2_PLACEMENT_3D('',#59202,#38203,#38204);
#32522=AXIS2_PLACEMENT_3D('',#59250,#38206,#38207);
#32523=AXIS2_PLACEMENT_3D('',#59298,#38209,#38210);
#32524=AXIS2_PLACEMENT_3D('',#59352,#38212,#38213);
#32525=AXIS2_PLACEMENT_3D('',#59400,#38215,#38216);
#32526=AXIS2_PLACEMENT_3D('',#59411,#38218,#38219);
#32527=AXIS2_PLACEMENT_3D('',#59416,#38220,#38221);
#32528=AXIS2_PLACEMENT_3D('',#59440,#38223,#38224);
#32529=AXIS2_PLACEMENT_3D('',#59465,#38226,#38227);
#32530=AXIS2_PLACEMENT_3D('',#59490,#38229,#38230);
#32531=AXIS2_PLACEMENT_3D('',#59514,#38232,#38233);
#32532=AXIS2_PLACEMENT_3D('',#59538,#38235,#38236);
#32533=AXIS2_PLACEMENT_3D('',#59563,#38238,#38239);
#32534=AXIS2_PLACEMENT_3D('',#59588,#38241,#38242);
#32535=AXIS2_PLACEMENT_3D('',#59612,#38244,#38245);
#32536=AXIS2_PLACEMENT_3D('',#59637,#38247,#38248);
#32537=AXIS2_PLACEMENT_3D('',#59662,#38250,#38251);
#32538=AXIS2_PLACEMENT_3D('',#59686,#38253,#38254);
#32539=AXIS2_PLACEMENT_3D('',#59710,#38256,#38257);
#32540=AXIS2_PLACEMENT_3D('',#59735,#38259,#38260);
#32541=AXIS2_PLACEMENT_3D('',#59760,#38262,#38263);
#32542=AXIS2_PLACEMENT_3D('',#59784,#38265,#38266);
#32543=AXIS2_PLACEMENT_3D('',#59809,#38268,#38269);
#32544=AXIS2_PLACEMENT_3D('',#59834,#38271,#38272);
#32545=AXIS2_PLACEMENT_3D('',#59858,#38274,#38275);
#32546=AXIS2_PLACEMENT_3D('',#59882,#38277,#38278);
#32547=AXIS2_PLACEMENT_3D('',#59907,#38280,#38281);
#32548=AXIS2_PLACEMENT_3D('',#59932,#38283,#38284);
#32549=AXIS2_PLACEMENT_3D('',#59956,#38286,#38287);
#32550=AXIS2_PLACEMENT_3D('',#59981,#38289,#38290);
#32551=AXIS2_PLACEMENT_3D('',#60006,#38292,#38293);
#32552=AXIS2_PLACEMENT_3D('',#60030,#38295,#38296);
#32553=AXIS2_PLACEMENT_3D('',#60054,#38298,#38299);
#32554=AXIS2_PLACEMENT_3D('',#60079,#38301,#38302);
#32555=AXIS2_PLACEMENT_3D('',#60104,#38304,#38305);
#32556=AXIS2_PLACEMENT_3D('',#60128,#38307,#38308);
#32557=AXIS2_PLACEMENT_3D('',#60153,#38310,#38311);
#32558=AXIS2_PLACEMENT_3D('',#60178,#38313,#38314);
#32559=AXIS2_PLACEMENT_3D('',#60202,#38316,#38317);
#32560=AXIS2_PLACEMENT_3D('',#60226,#38319,#38320);
#32561=AXIS2_PLACEMENT_3D('',#60251,#38322,#38323);
#32562=AXIS2_PLACEMENT_3D('',#60276,#38325,#38326);
#32563=AXIS2_PLACEMENT_3D('',#60300,#38328,#38329);
#32564=AXIS2_PLACEMENT_3D('',#60325,#38331,#38332);
#32565=AXIS2_PLACEMENT_3D('',#60350,#38334,#38335);
#32566=AXIS2_PLACEMENT_3D('',#60374,#38337,#38338);
#32567=AXIS2_PLACEMENT_3D('',#60398,#38340,#38341);
#32568=AXIS2_PLACEMENT_3D('',#60423,#38343,#38344);
#32569=AXIS2_PLACEMENT_3D('',#60448,#38346,#38347);
#32570=AXIS2_PLACEMENT_3D('',#60472,#38349,#38350);
#32571=AXIS2_PLACEMENT_3D('',#60497,#38352,#38353);
#32572=AXIS2_PLACEMENT_3D('',#60522,#38355,#38356);
#32573=AXIS2_PLACEMENT_3D('',#60546,#38358,#38359);
#32574=AXIS2_PLACEMENT_3D('',#60570,#38361,#38362);
#32575=AXIS2_PLACEMENT_3D('',#60595,#38364,#38365);
#32576=AXIS2_PLACEMENT_3D('',#60620,#38367,#38368);
#32577=AXIS2_PLACEMENT_3D('',#60644,#38370,#38371);
#32578=AXIS2_PLACEMENT_3D('',#60669,#38373,#38374);
#32579=AXIS2_PLACEMENT_3D('',#60694,#38376,#38377);
#32580=AXIS2_PLACEMENT_3D('',#60718,#38379,#38380);
#32581=AXIS2_PLACEMENT_3D('',#60742,#38382,#38383);
#32582=AXIS2_PLACEMENT_3D('',#60767,#38385,#38386);
#32583=AXIS2_PLACEMENT_3D('',#60792,#38388,#38389);
#32584=AXIS2_PLACEMENT_3D('',#60816,#38391,#38392);
#32585=AXIS2_PLACEMENT_3D('',#60841,#38394,#38395);
#32586=AXIS2_PLACEMENT_3D('',#60866,#38397,#38398);
#32587=AXIS2_PLACEMENT_3D('',#60890,#38400,#38401);
#32588=AXIS2_PLACEMENT_3D('',#60914,#38403,#38404);
#32589=AXIS2_PLACEMENT_3D('',#60939,#38406,#38407);
#32590=AXIS2_PLACEMENT_3D('',#60964,#38409,#38410);
#32591=AXIS2_PLACEMENT_3D('',#60988,#38412,#38413);
#32592=AXIS2_PLACEMENT_3D('',#61013,#38415,#38416);
#32593=AXIS2_PLACEMENT_3D('',#61038,#38418,#38419);
#32594=AXIS2_PLACEMENT_3D('',#61062,#38421,#38422);
#32595=AXIS2_PLACEMENT_3D('',#61086,#38424,#38425);
#32596=AXIS2_PLACEMENT_3D('',#61174,#38426,#38427);
#32597=AXIS2_PLACEMENT_3D('',#61176,#38428,#38429);
#32598=AXIS2_PLACEMENT_3D('',#63122,#38430,#38431);
#32599=AXIS2_PLACEMENT_3D('',#63124,#38432,#38433);
#32600=AXIS2_PLACEMENT_3D('',#63125,#38434,#38435);
#32601=AXIS2_PLACEMENT_3D('',#63209,#38436,#38437);
#32602=AXIS2_PLACEMENT_3D('',#63210,#38438,#38439);
#32603=AXIS2_PLACEMENT_3D('',#64984,#38440,#38441);
#32604=AXIS2_PLACEMENT_3D('',#64986,#38442,#38443);
#32605=AXIS2_PLACEMENT_3D('',#64987,#38444,#38445);
#32606=AXIS2_PLACEMENT_3D('',#64988,#38446,#38447);
#32607=AXIS2_PLACEMENT_3D('',#64989,#38448,#38449);
#32608=AXIS2_PLACEMENT_3D('',#64990,#38450,#38451);
#32609=AXIS2_PLACEMENT_3D('',#64992,#38452,#38453);
#32610=AXIS2_PLACEMENT_3D('',#64993,#38454,#38455);
#32611=AXIS2_PLACEMENT_3D('',#65002,#38460,#38461);
#32612=AXIS2_PLACEMENT_3D('',#65004,#38462,#38463);
#32613=AXIS2_PLACEMENT_3D('',#65006,#38465,#38466);
#32614=AXIS2_PLACEMENT_3D('',#65010,#38469,#38470);
#32615=AXIS2_PLACEMENT_3D('',#65011,#38471,#38472);
#32616=AXIS2_PLACEMENT_3D('',#65012,#38473,#38474);
#32617=AXIS2_PLACEMENT_3D('',#65021,#38479,#38480);
#32618=AXIS2_PLACEMENT_3D('',#65023,#38481,#38482);
#32619=AXIS2_PLACEMENT_3D('',#65025,#38484,#38485);
#32620=AXIS2_PLACEMENT_3D('',#65029,#38488,#38489);
#32621=AXIS2_PLACEMENT_3D('',#65030,#38490,#38491);
#32622=AXIS2_PLACEMENT_3D('',#65031,#38492,#38493);
#32623=AXIS2_PLACEMENT_3D('',#65040,#38498,#38499);
#32624=AXIS2_PLACEMENT_3D('',#65042,#38500,#38501);
#32625=AXIS2_PLACEMENT_3D('',#65044,#38503,#38504);
#32626=AXIS2_PLACEMENT_3D('',#65048,#38507,#38508);
#32627=AXIS2_PLACEMENT_3D('',#65049,#38509,#38510);
#32628=AXIS2_PLACEMENT_3D('',#65050,#38511,#38512);
#32629=AXIS2_PLACEMENT_3D('',#65059,#38517,#38518);
#32630=AXIS2_PLACEMENT_3D('',#65061,#38519,#38520);
#32631=AXIS2_PLACEMENT_3D('',#65063,#38522,#38523);
#32632=AXIS2_PLACEMENT_3D('',#65067,#38526,#38527);
#32633=AXIS2_PLACEMENT_3D('',#65068,#38528,#38529);
#32634=AXIS2_PLACEMENT_3D('',#65069,#38530,#38531);
#32635=AXIS2_PLACEMENT_3D('',#65078,#38536,#38537);
#32636=AXIS2_PLACEMENT_3D('',#65080,#38538,#38539);
#32637=AXIS2_PLACEMENT_3D('',#65082,#38541,#38542);
#32638=AXIS2_PLACEMENT_3D('',#65086,#38545,#38546);
#32639=AXIS2_PLACEMENT_3D('',#65087,#38547,#38548);
#32640=AXIS2_PLACEMENT_3D('',#65088,#38549,#38550);
#32641=AXIS2_PLACEMENT_3D('',#65097,#38555,#38556);
#32642=AXIS2_PLACEMENT_3D('',#65099,#38557,#38558);
#32643=AXIS2_PLACEMENT_3D('',#65101,#38560,#38561);
#32644=AXIS2_PLACEMENT_3D('',#65105,#38564,#38565);
#32645=AXIS2_PLACEMENT_3D('',#65106,#38566,#38567);
#32646=AXIS2_PLACEMENT_3D('',#65107,#38568,#38569);
#32647=AXIS2_PLACEMENT_3D('',#65116,#38574,#38575);
#32648=AXIS2_PLACEMENT_3D('',#65118,#38576,#38577);
#32649=AXIS2_PLACEMENT_3D('',#65120,#38579,#38580);
#32650=AXIS2_PLACEMENT_3D('',#65124,#38583,#38584);
#32651=AXIS2_PLACEMENT_3D('',#65125,#38585,#38586);
#32652=AXIS2_PLACEMENT_3D('',#65126,#38587,#38588);
#32653=AXIS2_PLACEMENT_3D('',#65135,#38593,#38594);
#32654=AXIS2_PLACEMENT_3D('',#65137,#38595,#38596);
#32655=AXIS2_PLACEMENT_3D('',#65139,#38598,#38599);
#32656=AXIS2_PLACEMENT_3D('',#65143,#38602,#38603);
#32657=AXIS2_PLACEMENT_3D('',#65144,#38604,#38605);
#32658=AXIS2_PLACEMENT_3D('',#65145,#38606,#38607);
#32659=AXIS2_PLACEMENT_3D('',#65154,#38612,#38613);
#32660=AXIS2_PLACEMENT_3D('',#65156,#38614,#38615);
#32661=AXIS2_PLACEMENT_3D('',#65158,#38617,#38618);
#32662=AXIS2_PLACEMENT_3D('',#65162,#38621,#38622);
#32663=AXIS2_PLACEMENT_3D('',#65163,#38623,#38624);
#32664=AXIS2_PLACEMENT_3D('',#65164,#38625,#38626);
#32665=AXIS2_PLACEMENT_3D('',#65173,#38631,#38632);
#32666=AXIS2_PLACEMENT_3D('',#65175,#38633,#38634);
#32667=AXIS2_PLACEMENT_3D('',#65177,#38636,#38637);
#32668=AXIS2_PLACEMENT_3D('',#65181,#38640,#38641);
#32669=AXIS2_PLACEMENT_3D('',#65182,#38642,#38643);
#32670=AXIS2_PLACEMENT_3D('',#65183,#38644,#38645);
#32671=AXIS2_PLACEMENT_3D('',#65192,#38650,#38651);
#32672=AXIS2_PLACEMENT_3D('',#65194,#38652,#38653);
#32673=AXIS2_PLACEMENT_3D('',#65196,#38655,#38656);
#32674=AXIS2_PLACEMENT_3D('',#65200,#38659,#38660);
#32675=AXIS2_PLACEMENT_3D('',#65201,#38661,#38662);
#32676=AXIS2_PLACEMENT_3D('',#65202,#38663,#38664);
#32677=AXIS2_PLACEMENT_3D('',#65211,#38669,#38670);
#32678=AXIS2_PLACEMENT_3D('',#65213,#38671,#38672);
#32679=AXIS2_PLACEMENT_3D('',#65215,#38674,#38675);
#32680=AXIS2_PLACEMENT_3D('',#65219,#38678,#38679);
#32681=AXIS2_PLACEMENT_3D('',#65220,#38680,#38681);
#32682=AXIS2_PLACEMENT_3D('',#65221,#38682,#38683);
#32683=AXIS2_PLACEMENT_3D('',#65230,#38688,#38689);
#32684=AXIS2_PLACEMENT_3D('',#65232,#38690,#38691);
#32685=AXIS2_PLACEMENT_3D('',#65234,#38693,#38694);
#32686=AXIS2_PLACEMENT_3D('',#65238,#38697,#38698);
#32687=AXIS2_PLACEMENT_3D('',#65239,#38699,#38700);
#32688=AXIS2_PLACEMENT_3D('',#65240,#38701,#38702);
#32689=AXIS2_PLACEMENT_3D('',#65249,#38707,#38708);
#32690=AXIS2_PLACEMENT_3D('',#65251,#38709,#38710);
#32691=AXIS2_PLACEMENT_3D('',#65253,#38712,#38713);
#32692=AXIS2_PLACEMENT_3D('',#65257,#38716,#38717);
#32693=AXIS2_PLACEMENT_3D('',#65258,#38718,#38719);
#32694=AXIS2_PLACEMENT_3D('',#65259,#38720,#38721);
#32695=AXIS2_PLACEMENT_3D('',#65268,#38726,#38727);
#32696=AXIS2_PLACEMENT_3D('',#65270,#38728,#38729);
#32697=AXIS2_PLACEMENT_3D('',#65272,#38731,#38732);
#32698=AXIS2_PLACEMENT_3D('',#65276,#38735,#38736);
#32699=AXIS2_PLACEMENT_3D('',#65277,#38737,#38738);
#32700=AXIS2_PLACEMENT_3D('',#65278,#38739,#38740);
#32701=AXIS2_PLACEMENT_3D('',#65287,#38745,#38746);
#32702=AXIS2_PLACEMENT_3D('',#65289,#38747,#38748);
#32703=AXIS2_PLACEMENT_3D('',#65291,#38750,#38751);
#32704=AXIS2_PLACEMENT_3D('',#65295,#38754,#38755);
#32705=AXIS2_PLACEMENT_3D('',#65296,#38756,#38757);
#32706=AXIS2_PLACEMENT_3D('',#65297,#38758,#38759);
#32707=AXIS2_PLACEMENT_3D('',#65306,#38764,#38765);
#32708=AXIS2_PLACEMENT_3D('',#65308,#38766,#38767);
#32709=AXIS2_PLACEMENT_3D('',#65310,#38769,#38770);
#32710=AXIS2_PLACEMENT_3D('',#65314,#38773,#38774);
#32711=AXIS2_PLACEMENT_3D('',#65315,#38775,#38776);
#32712=AXIS2_PLACEMENT_3D('',#65316,#38777,#38778);
#32713=AXIS2_PLACEMENT_3D('',#65325,#38783,#38784);
#32714=AXIS2_PLACEMENT_3D('',#65327,#38785,#38786);
#32715=AXIS2_PLACEMENT_3D('',#65330,#38788,#38789);
#32716=AXIS2_PLACEMENT_3D('',#65331,#38790,#38791);
#32717=AXIS2_PLACEMENT_3D('',#65335,#38794,#38795);
#32718=AXIS2_PLACEMENT_3D('',#65337,#38796,#38797);
#32719=AXIS2_PLACEMENT_3D('',#65338,#38798,#38799);
#32720=AXIS2_PLACEMENT_3D('',#65339,#38800,#38801);
#32721=AXIS2_PLACEMENT_3D('',#65348,#38806,#38807);
#32722=AXIS2_PLACEMENT_3D('',#65350,#38808,#38809);
#32723=AXIS2_PLACEMENT_3D('',#65352,#38811,#38812);
#32724=AXIS2_PLACEMENT_3D('',#65356,#38815,#38816);
#32725=AXIS2_PLACEMENT_3D('',#65357,#38817,#38818);
#32726=AXIS2_PLACEMENT_3D('',#65358,#38819,#38820);
#32727=AXIS2_PLACEMENT_3D('',#65367,#38825,#38826);
#32728=AXIS2_PLACEMENT_3D('',#65369,#38827,#38828);
#32729=AXIS2_PLACEMENT_3D('',#65371,#38830,#38831);
#32730=AXIS2_PLACEMENT_3D('',#65375,#38834,#38835);
#32731=AXIS2_PLACEMENT_3D('',#65376,#38836,#38837);
#32732=AXIS2_PLACEMENT_3D('',#65377,#38838,#38839);
#32733=AXIS2_PLACEMENT_3D('',#65386,#38844,#38845);
#32734=AXIS2_PLACEMENT_3D('',#65388,#38846,#38847);
#32735=AXIS2_PLACEMENT_3D('',#65390,#38849,#38850);
#32736=AXIS2_PLACEMENT_3D('',#65394,#38853,#38854);
#32737=AXIS2_PLACEMENT_3D('',#65395,#38855,#38856);
#32738=AXIS2_PLACEMENT_3D('',#65396,#38857,#38858);
#32739=AXIS2_PLACEMENT_3D('',#65405,#38863,#38864);
#32740=AXIS2_PLACEMENT_3D('',#65407,#38865,#38866);
#32741=AXIS2_PLACEMENT_3D('',#65409,#38868,#38869);
#32742=AXIS2_PLACEMENT_3D('',#65413,#38872,#38873);
#32743=AXIS2_PLACEMENT_3D('',#65414,#38874,#38875);
#32744=AXIS2_PLACEMENT_3D('',#65415,#38876,#38877);
#32745=AXIS2_PLACEMENT_3D('',#65424,#38882,#38883);
#32746=AXIS2_PLACEMENT_3D('',#65426,#38884,#38885);
#32747=AXIS2_PLACEMENT_3D('',#65428,#38887,#38888);
#32748=AXIS2_PLACEMENT_3D('',#65432,#38891,#38892);
#32749=AXIS2_PLACEMENT_3D('',#65433,#38893,#38894);
#32750=AXIS2_PLACEMENT_3D('',#65434,#38895,#38896);
#32751=AXIS2_PLACEMENT_3D('',#65443,#38901,#38902);
#32752=AXIS2_PLACEMENT_3D('',#65445,#38903,#38904);
#32753=AXIS2_PLACEMENT_3D('',#65447,#38906,#38907);
#32754=AXIS2_PLACEMENT_3D('',#65451,#38910,#38911);
#32755=AXIS2_PLACEMENT_3D('',#65452,#38912,#38913);
#32756=AXIS2_PLACEMENT_3D('',#65453,#38914,#38915);
#32757=AXIS2_PLACEMENT_3D('',#65462,#38920,#38921);
#32758=AXIS2_PLACEMENT_3D('',#65464,#38922,#38923);
#32759=AXIS2_PLACEMENT_3D('',#65466,#38925,#38926);
#32760=AXIS2_PLACEMENT_3D('',#65470,#38929,#38930);
#32761=AXIS2_PLACEMENT_3D('',#65471,#38931,#38932);
#32762=AXIS2_PLACEMENT_3D('',#65472,#38933,#38934);
#32763=AXIS2_PLACEMENT_3D('',#65481,#38939,#38940);
#32764=AXIS2_PLACEMENT_3D('',#65483,#38941,#38942);
#32765=AXIS2_PLACEMENT_3D('',#65485,#38944,#38945);
#32766=AXIS2_PLACEMENT_3D('',#65489,#38948,#38949);
#32767=AXIS2_PLACEMENT_3D('',#65490,#38950,#38951);
#32768=AXIS2_PLACEMENT_3D('',#65491,#38952,#38953);
#32769=AXIS2_PLACEMENT_3D('',#65500,#38958,#38959);
#32770=AXIS2_PLACEMENT_3D('',#65502,#38960,#38961);
#32771=AXIS2_PLACEMENT_3D('',#65504,#38963,#38964);
#32772=AXIS2_PLACEMENT_3D('',#65508,#38967,#38968);
#32773=AXIS2_PLACEMENT_3D('',#65509,#38969,#38970);
#32774=AXIS2_PLACEMENT_3D('',#65510,#38971,#38972);
#32775=AXIS2_PLACEMENT_3D('',#65519,#38977,#38978);
#32776=AXIS2_PLACEMENT_3D('',#65521,#38979,#38980);
#32777=AXIS2_PLACEMENT_3D('',#65523,#38982,#38983);
#32778=AXIS2_PLACEMENT_3D('',#65527,#38986,#38987);
#32779=AXIS2_PLACEMENT_3D('',#65528,#38988,#38989);
#32780=AXIS2_PLACEMENT_3D('',#65529,#38990,#38991);
#32781=AXIS2_PLACEMENT_3D('',#65538,#38996,#38997);
#32782=AXIS2_PLACEMENT_3D('',#65540,#38998,#38999);
#32783=AXIS2_PLACEMENT_3D('',#65542,#39001,#39002);
#32784=AXIS2_PLACEMENT_3D('',#65546,#39005,#39006);
#32785=AXIS2_PLACEMENT_3D('',#65547,#39007,#39008);
#32786=AXIS2_PLACEMENT_3D('',#65548,#39009,#39010);
#32787=AXIS2_PLACEMENT_3D('',#65557,#39015,#39016);
#32788=AXIS2_PLACEMENT_3D('',#65559,#39017,#39018);
#32789=AXIS2_PLACEMENT_3D('',#65561,#39020,#39021);
#32790=AXIS2_PLACEMENT_3D('',#65565,#39024,#39025);
#32791=AXIS2_PLACEMENT_3D('',#65566,#39026,#39027);
#32792=AXIS2_PLACEMENT_3D('',#65567,#39028,#39029);
#32793=AXIS2_PLACEMENT_3D('',#65576,#39034,#39035);
#32794=AXIS2_PLACEMENT_3D('',#65578,#39036,#39037);
#32795=AXIS2_PLACEMENT_3D('',#65580,#39039,#39040);
#32796=AXIS2_PLACEMENT_3D('',#65584,#39043,#39044);
#32797=AXIS2_PLACEMENT_3D('',#65585,#39045,#39046);
#32798=AXIS2_PLACEMENT_3D('',#65586,#39047,#39048);
#32799=AXIS2_PLACEMENT_3D('',#65595,#39053,#39054);
#32800=AXIS2_PLACEMENT_3D('',#65597,#39055,#39056);
#32801=AXIS2_PLACEMENT_3D('',#65599,#39058,#39059);
#32802=AXIS2_PLACEMENT_3D('',#65603,#39062,#39063);
#32803=AXIS2_PLACEMENT_3D('',#65604,#39064,#39065);
#32804=AXIS2_PLACEMENT_3D('',#65605,#39066,#39067);
#32805=AXIS2_PLACEMENT_3D('',#65614,#39072,#39073);
#32806=AXIS2_PLACEMENT_3D('',#65616,#39074,#39075);
#32807=AXIS2_PLACEMENT_3D('',#65618,#39077,#39078);
#32808=AXIS2_PLACEMENT_3D('',#65622,#39081,#39082);
#32809=AXIS2_PLACEMENT_3D('',#65623,#39083,#39084);
#32810=AXIS2_PLACEMENT_3D('',#65624,#39085,#39086);
#32811=AXIS2_PLACEMENT_3D('',#65633,#39091,#39092);
#32812=AXIS2_PLACEMENT_3D('',#65635,#39093,#39094);
#32813=AXIS2_PLACEMENT_3D('',#65637,#39096,#39097);
#32814=AXIS2_PLACEMENT_3D('',#65641,#39100,#39101);
#32815=AXIS2_PLACEMENT_3D('',#65642,#39102,#39103);
#32816=AXIS2_PLACEMENT_3D('',#65643,#39104,#39105);
#32817=AXIS2_PLACEMENT_3D('',#65652,#39110,#39111);
#32818=AXIS2_PLACEMENT_3D('',#65654,#39112,#39113);
#32819=AXIS2_PLACEMENT_3D('',#65656,#39115,#39116);
#32820=AXIS2_PLACEMENT_3D('',#65660,#39119,#39120);
#32821=AXIS2_PLACEMENT_3D('',#65661,#39121,#39122);
#32822=AXIS2_PLACEMENT_3D('',#65662,#39123,#39124);
#32823=AXIS2_PLACEMENT_3D('',#65671,#39129,#39130);
#32824=AXIS2_PLACEMENT_3D('',#65673,#39131,#39132);
#32825=AXIS2_PLACEMENT_3D('',#65675,#39134,#39135);
#32826=AXIS2_PLACEMENT_3D('',#65679,#39138,#39139);
#32827=AXIS2_PLACEMENT_3D('',#65680,#39140,#39141);
#32828=AXIS2_PLACEMENT_3D('',#65681,#39142,#39143);
#32829=AXIS2_PLACEMENT_3D('',#65685,#39145,#39146);
#32830=AXIS2_PLACEMENT_3D('',#65686,#39147,#39148);
#32831=AXIS2_PLACEMENT_3D('',#65695,#39153,#39154);
#32832=AXIS2_PLACEMENT_3D('',#65701,#39158,#39159);
#32833=AXIS2_PLACEMENT_3D('',#65707,#39163,#39164);
#32834=AXIS2_PLACEMENT_3D('',#65713,#39168,#39169);
#32835=AXIS2_PLACEMENT_3D('',#65719,#39173,#39174);
#32836=AXIS2_PLACEMENT_3D('',#65722,#39177,#39178);
#32837=AXIS2_PLACEMENT_3D('',#65723,#39179,#39180);
#32838=AXIS2_PLACEMENT_3D('',#65725,#39181,#39182);
#32839=AXIS2_PLACEMENT_3D('',#65726,#39183,#39184);
#32840=AXIS2_PLACEMENT_3D('',#65728,#39186,#39187);
#32841=AXIS2_PLACEMENT_3D('',#65730,#39188,#39189);
#32842=AXIS2_PLACEMENT_3D('',#65733,#39192,#39193);
#32843=AXIS2_PLACEMENT_3D('',#65735,#39194,#39195);
#32844=AXIS2_PLACEMENT_3D('',#65737,#39197,#39198);
#32845=AXIS2_PLACEMENT_3D('',#65738,#39199,#39200);
#32846=AXIS2_PLACEMENT_3D('',#65739,#39201,#39202);
#32847=AXIS2_PLACEMENT_3D('',#65748,#39207,#39208);
#32848=AXIS2_PLACEMENT_3D('',#65754,#39212,#39213);
#32849=AXIS2_PLACEMENT_3D('',#65767,#39216,#39217);
#32850=AXIS2_PLACEMENT_3D('',#65769,#39218,#39219);
#32851=AXIS2_PLACEMENT_3D('',#65772,#39221,#39222);
#32852=AXIS2_PLACEMENT_3D('',#65773,#39223,#39224);
#32853=AXIS2_PLACEMENT_3D('',#65779,#39225,#39226);
#32854=AXIS2_PLACEMENT_3D('',#65787,#39227,#39228);
#32855=AXIS2_PLACEMENT_3D('',#65800,#39231,#39232);
#32856=AXIS2_PLACEMENT_3D('',#65813,#39236,#39237);
#32857=AXIS2_PLACEMENT_3D('',#65815,#39238,#39239);
#32858=AXIS2_PLACEMENT_3D('',#65824,#39240,#39241);
#32859=AXIS2_PLACEMENT_3D('',#65825,#39242,#39243);
#32860=AXIS2_PLACEMENT_3D('',#65834,#39248,#39249);
#32861=AXIS2_PLACEMENT_3D('',#65840,#39253,#39254);
#32862=AXIS2_PLACEMENT_3D('',#65848,#39257,#39258);
#32863=AXIS2_PLACEMENT_3D('',#65857,#39262,#39263);
#32864=AXIS2_PLACEMENT_3D('',#65870,#39266,#39267);
#32865=AXIS2_PLACEMENT_3D('',#65872,#39268,#39269);
#32866=AXIS2_PLACEMENT_3D('',#65875,#39271,#39272);
#32867=AXIS2_PLACEMENT_3D('',#65876,#39273,#39274);
#32868=AXIS2_PLACEMENT_3D('',#65882,#39275,#39276);
#32869=AXIS2_PLACEMENT_3D('',#65890,#39277,#39278);
#32870=AXIS2_PLACEMENT_3D('',#65899,#39283,#39284);
#32871=AXIS2_PLACEMENT_3D('',#65905,#39288,#39289);
#32872=AXIS2_PLACEMENT_3D('',#65911,#39291,#39292);
#32873=AXIS2_PLACEMENT_3D('',#65917,#39293,#39294);
#32874=AXIS2_PLACEMENT_3D('',#65921,#39295,#39296);
#32875=AXIS2_PLACEMENT_3D('',#65926,#39300,#39301);
#32876=AXIS2_PLACEMENT_3D('',#65939,#39304,#39305);
#32877=AXIS2_PLACEMENT_3D('',#65941,#39306,#39307);
#32878=AXIS2_PLACEMENT_3D('',#65944,#39309,#39310);
#32879=AXIS2_PLACEMENT_3D('',#65945,#39311,#39312);
#32880=AXIS2_PLACEMENT_3D('',#65951,#39313,#39314);
#32881=AXIS2_PLACEMENT_3D('',#65959,#39315,#39316);
#32882=AXIS2_PLACEMENT_3D('',#65963,#39319,#39320);
#32883=AXIS2_PLACEMENT_3D('',#65967,#39323,#39324);
#32884=AXIS2_PLACEMENT_3D('',#65971,#39327,#39328);
#32885=AXIS2_PLACEMENT_3D('',#65980,#39333,#39334);
#32886=AXIS2_PLACEMENT_3D('',#65986,#39338,#39339);
#32887=AXIS2_PLACEMENT_3D('',#65992,#39343,#39344);
#32888=AXIS2_PLACEMENT_3D('',#65998,#39346,#39347);
#32889=AXIS2_PLACEMENT_3D('',#66004,#39348,#39349);
#32890=AXIS2_PLACEMENT_3D('',#66008,#39350,#39351);
#32891=AXIS2_PLACEMENT_3D('',#66011,#39354,#39355);
#32892=AXIS2_PLACEMENT_3D('',#66017,#39357,#39358);
#32893=AXIS2_PLACEMENT_3D('',#66023,#39359,#39360);
#32894=AXIS2_PLACEMENT_3D('',#66027,#39361,#39362);
#32895=AXIS2_PLACEMENT_3D('',#66030,#39365,#39366);
#32896=AXIS2_PLACEMENT_3D('',#66034,#39370,#39371);
#32897=AXIS2_PLACEMENT_3D('',#66036,#39372,#39373);
#32898=AXIS2_PLACEMENT_3D('',#66037,#39374,#39375);
#32899=AXIS2_PLACEMENT_3D('',#66039,#39377,#39378);
#32900=AXIS2_PLACEMENT_3D('',#66041,#39380,#39381);
#32901=AXIS2_PLACEMENT_3D('',#66042,#39382,#39383);
#32902=AXIS2_PLACEMENT_3D('',#66043,#39384,#39385);
#32903=AXIS2_PLACEMENT_3D('',#66044,#39386,#39387);
#32904=AXIS2_PLACEMENT_3D('',#66046,#39389,#39390);
#32905=AXIS2_PLACEMENT_3D('',#66048,#39391,#39392);
#32906=AXIS2_PLACEMENT_3D('',#66050,#39394,#39395);
#32907=AXIS2_PLACEMENT_3D('',#66051,#39396,#39397);
#32908=AXIS2_PLACEMENT_3D('',#66052,#39398,#39399);
#32909=AXIS2_PLACEMENT_3D('',#66074,#39401,#39402);
#32910=AXIS2_PLACEMENT_3D('',#66085,#39403,#39404);
#32911=AXIS2_PLACEMENT_3D('',#66169,#39406,#39407);
#32912=AXIS2_PLACEMENT_3D('',#66259,#39409,#39410);
#32913=AXIS2_PLACEMENT_3D('',#66349,#39412,#39413);
#32914=AXIS2_PLACEMENT_3D('',#66433,#39415,#39416);
#32915=AXIS2_PLACEMENT_3D('',#66523,#39418,#39419);
#32916=AXIS2_PLACEMENT_3D('',#66607,#39421,#39422);
#32917=AXIS2_PLACEMENT_3D('',#66697,#39424,#39425);
#32918=AXIS2_PLACEMENT_3D('',#66787,#39427,#39428);
#32919=AXIS2_PLACEMENT_3D('',#66871,#39430,#39431);
#32920=AXIS2_PLACEMENT_3D('',#66961,#39433,#39434);
#32921=AXIS2_PLACEMENT_3D('',#67045,#39436,#39437);
#32922=AXIS2_PLACEMENT_3D('',#67135,#39439,#39440);
#32923=AXIS2_PLACEMENT_3D('',#67225,#39442,#39443);
#32924=AXIS2_PLACEMENT_3D('',#67309,#39445,#39446);
#32925=AXIS2_PLACEMENT_3D('',#67399,#39448,#39449);
#32926=AXIS2_PLACEMENT_3D('',#67408,#39451,#39452);
#32927=AXIS2_PLACEMENT_3D('',#67409,#39453,#39454);
#32928=AXIS2_PLACEMENT_3D('',#67431,#39456,#39457);
#32929=AXIS2_PLACEMENT_3D('',#67446,#39458,#39459);
#32930=AXIS2_PLACEMENT_3D('',#67483,#39461,#39462);
#32931=AXIS2_PLACEMENT_3D('',#67520,#39464,#39465);
#32932=AXIS2_PLACEMENT_3D('',#67558,#39467,#39468);
#32933=AXIS2_PLACEMENT_3D('',#67595,#39470,#39471);
#32934=AXIS2_PLACEMENT_3D('',#67632,#39473,#39474);
#32935=AXIS2_PLACEMENT_3D('',#67669,#39476,#39477);
#32936=AXIS2_PLACEMENT_3D('',#67706,#39479,#39480);
#32937=AXIS2_PLACEMENT_3D('',#67744,#39482,#39483);
#32938=AXIS2_PLACEMENT_3D('',#67781,#39485,#39486);
#32939=AXIS2_PLACEMENT_3D('',#67818,#39488,#39489);
#32940=AXIS2_PLACEMENT_3D('',#67855,#39491,#39492);
#32941=AXIS2_PLACEMENT_3D('',#67892,#39494,#39495);
#32942=AXIS2_PLACEMENT_3D('',#67930,#39497,#39498);
#32943=AXIS2_PLACEMENT_3D('',#67967,#39500,#39501);
#32944=AXIS2_PLACEMENT_3D('',#67969,#39502,#39503);
#32945=AXIS2_PLACEMENT_3D('',#67973,#39505,#39506);
#32946=AXIS2_PLACEMENT_3D('',#67974,#39507,#39508);
#32947=AXIS2_PLACEMENT_3D('',#67975,#39509,#39510);
#32948=AXIS2_PLACEMENT_3D('',#67978,#39511,#39512);
#32949=AXIS2_PLACEMENT_3D('',#67979,#39513,#39514);
#32950=AXIS2_PLACEMENT_3D('',#68010,#39518,#39519);
#32951=AXIS2_PLACEMENT_3D('',#68012,#39520,#39521);
#32952=AXIS2_PLACEMENT_3D('',#68013,#39522,#39523);
#32953=AXIS2_PLACEMENT_3D('',#68016,#39525,#39526);
#32954=AXIS2_PLACEMENT_3D('',#68017,#39527,#39528);
#32955=AXIS2_PLACEMENT_3D('',#68019,#39529,#39530);
#32956=AXIS2_PLACEMENT_3D('',#68189,#39532,#39533);
#32957=AXIS2_PLACEMENT_3D('',#68191,#39535,#39536);
#32958=AXIS2_PLACEMENT_3D('',#68192,#39537,#39538);
#32959=AXIS2_PLACEMENT_3D('',#68193,#39539,#39540);
#32960=AXIS2_PLACEMENT_3D('',#68195,#39541,#39542);
#32961=AXIS2_PLACEMENT_3D('',#68198,#39544,#39545);
#32962=AXIS2_PLACEMENT_3D('',#69284,#39546,#39547);
#32963=AXIS2_PLACEMENT_3D('',#69286,#39548,#39549);
#32964=AXIS2_PLACEMENT_3D('',#69287,#39550,#39551);
#32965=AXIS2_PLACEMENT_3D('',#69404,#39552,#39553);
#32966=AXIS2_PLACEMENT_3D('',#69405,#39554,#39555);
#32967=AXIS2_PLACEMENT_3D('',#70367,#39556,#39557);
#32968=AXIS2_PLACEMENT_3D('',#70368,#39558,#39559);
#32969=AXIS2_PLACEMENT_3D('',#70369,#39560,#39561);
#32970=AXIS2_PLACEMENT_3D('',#70371,#39563,#39564);
#32971=AXIS2_PLACEMENT_3D('',#70372,#39565,#39566);
#32972=AXIS2_PLACEMENT_3D('',#70373,#39567,#39568);
#32973=AXIS2_PLACEMENT_3D('',#70375,#39569,#39570);
#32974=AXIS2_PLACEMENT_3D('',#70376,#39571,#39572);
#32975=AXIS2_PLACEMENT_3D('',#70378,#39574,#39575);
#32976=AXIS2_PLACEMENT_3D('',#70380,#39576,#39577);
#32977=AXIS2_PLACEMENT_3D('',#70382,#39579,#39580);
#32978=AXIS2_PLACEMENT_3D('',#70384,#39581,#39582);
#32979=AXIS2_PLACEMENT_3D('',#70385,#39583,#39584);
#32980=AXIS2_PLACEMENT_3D('',#70387,#39585,#39586);
#32981=AXIS2_PLACEMENT_3D('',#70389,#39588,#39589);
#32982=AXIS2_PLACEMENT_3D('',#70391,#39591,#39592);
#32983=AXIS2_PLACEMENT_3D('',#70392,#39593,#39594);
#32984=AXIS2_PLACEMENT_3D('',#70408,#39596,#39597);
#32985=AXIS2_PLACEMENT_3D('',#70419,#39598,#39599);
#32986=AXIS2_PLACEMENT_3D('',#70467,#39601,#39602);
#32987=AXIS2_PLACEMENT_3D('',#70515,#39604,#39605);
#32988=AXIS2_PLACEMENT_3D('',#70563,#39607,#39608);
#32989=AXIS2_PLACEMENT_3D('',#70617,#39610,#39611);
#32990=AXIS2_PLACEMENT_3D('',#70665,#39613,#39614);
#32991=AXIS2_PLACEMENT_3D('',#70713,#39616,#39617);
#32992=AXIS2_PLACEMENT_3D('',#70767,#39619,#39620);
#32993=AXIS2_PLACEMENT_3D('',#70815,#39622,#39623);
#32994=AXIS2_PLACEMENT_3D('',#70863,#39625,#39626);
#32995=AXIS2_PLACEMENT_3D('',#70914,#39628,#39629);
#32996=AXIS2_PLACEMENT_3D('',#70965,#39631,#39632);
#32997=AXIS2_PLACEMENT_3D('',#71013,#39634,#39635);
#32998=AXIS2_PLACEMENT_3D('',#71061,#39637,#39638);
#32999=AXIS2_PLACEMENT_3D('',#71115,#39640,#39641);
#33000=AXIS2_PLACEMENT_3D('',#71163,#39643,#39644);
#33001=AXIS2_PLACEMENT_3D('',#71211,#39646,#39647);
#33002=AXIS2_PLACEMENT_3D('',#71262,#39649,#39650);
#33003=AXIS2_PLACEMENT_3D('',#71310,#39652,#39653);
#33004=AXIS2_PLACEMENT_3D('',#71358,#39655,#39656);
#33005=AXIS2_PLACEMENT_3D('',#71406,#39658,#39659);
#33006=AXIS2_PLACEMENT_3D('',#71460,#39661,#39662);
#33007=AXIS2_PLACEMENT_3D('',#71508,#39664,#39665);
#33008=AXIS2_PLACEMENT_3D('',#71556,#39667,#39668);
#33009=AXIS2_PLACEMENT_3D('',#71610,#39670,#39671);
#33010=AXIS2_PLACEMENT_3D('',#71658,#39673,#39674);
#33011=AXIS2_PLACEMENT_3D('',#71706,#39676,#39677);
#33012=AXIS2_PLACEMENT_3D('',#71754,#39679,#39680);
#33013=AXIS2_PLACEMENT_3D('',#71808,#39682,#39683);
#33014=AXIS2_PLACEMENT_3D('',#71856,#39685,#39686);
#33015=AXIS2_PLACEMENT_3D('',#71904,#39688,#39689);
#33016=AXIS2_PLACEMENT_3D('',#71958,#39691,#39692);
#33017=AXIS2_PLACEMENT_3D('',#72006,#39694,#39695);
#33018=AXIS2_PLACEMENT_3D('',#72054,#39697,#39698);
#33019=AXIS2_PLACEMENT_3D('',#72102,#39700,#39701);
#33020=AXIS2_PLACEMENT_3D('',#72156,#39703,#39704);
#33021=AXIS2_PLACEMENT_3D('',#72204,#39706,#39707);
#33022=AXIS2_PLACEMENT_3D('',#72252,#39709,#39710);
#33023=AXIS2_PLACEMENT_3D('',#72306,#39712,#39713);
#33024=AXIS2_PLACEMENT_3D('',#72354,#39715,#39716);
#33025=AXIS2_PLACEMENT_3D('',#72402,#39718,#39719);
#33026=AXIS2_PLACEMENT_3D('',#72450,#39721,#39722);
#33027=AXIS2_PLACEMENT_3D('',#72504,#39724,#39725);
#33028=AXIS2_PLACEMENT_3D('',#72552,#39727,#39728);
#33029=AXIS2_PLACEMENT_3D('',#72600,#39730,#39731);
#33030=AXIS2_PLACEMENT_3D('',#72654,#39733,#39734);
#33031=AXIS2_PLACEMENT_3D('',#72702,#39736,#39737);
#33032=AXIS2_PLACEMENT_3D('',#72750,#39739,#39740);
#33033=AXIS2_PLACEMENT_3D('',#72798,#39742,#39743);
#33034=AXIS2_PLACEMENT_3D('',#72852,#39745,#39746);
#33035=AXIS2_PLACEMENT_3D('',#72900,#39748,#39749);
#33036=AXIS2_PLACEMENT_3D('',#72948,#39751,#39752);
#33037=AXIS2_PLACEMENT_3D('',#73002,#39754,#39755);
#33038=AXIS2_PLACEMENT_3D('',#73050,#39757,#39758);
#33039=AXIS2_PLACEMENT_3D('',#73098,#39760,#39761);
#33040=AXIS2_PLACEMENT_3D('',#73146,#39763,#39764);
#33041=AXIS2_PLACEMENT_3D('',#73200,#39766,#39767);
#33042=AXIS2_PLACEMENT_3D('',#73248,#39769,#39770);
#33043=AXIS2_PLACEMENT_3D('',#73296,#39772,#39773);
#33044=AXIS2_PLACEMENT_3D('',#73350,#39775,#39776);
#33045=AXIS2_PLACEMENT_3D('',#73398,#39778,#39779);
#33046=AXIS2_PLACEMENT_3D('',#73446,#39781,#39782);
#33047=AXIS2_PLACEMENT_3D('',#73497,#39784,#39785);
#33048=AXIS2_PLACEMENT_3D('',#73548,#39787,#39788);
#33049=AXIS2_PLACEMENT_3D('',#73596,#39790,#39791);
#33050=AXIS2_PLACEMENT_3D('',#73644,#39793,#39794);
#33051=AXIS2_PLACEMENT_3D('',#73698,#39796,#39797);
#33052=AXIS2_PLACEMENT_3D('',#73746,#39799,#39800);
#33053=AXIS2_PLACEMENT_3D('',#73794,#39802,#39803);
#33054=AXIS2_PLACEMENT_3D('',#73845,#39805,#39806);
#33055=AXIS2_PLACEMENT_3D('',#73893,#39808,#39809);
#33056=AXIS2_PLACEMENT_3D('',#73941,#39811,#39812);
#33057=AXIS2_PLACEMENT_3D('',#73989,#39814,#39815);
#33058=AXIS2_PLACEMENT_3D('',#74043,#39817,#39818);
#33059=AXIS2_PLACEMENT_3D('',#74091,#39820,#39821);
#33060=AXIS2_PLACEMENT_3D('',#74102,#39823,#39824);
#33061=AXIS2_PLACEMENT_3D('',#74107,#39825,#39826);
#33062=AXIS2_PLACEMENT_3D('',#74132,#39828,#39829);
#33063=AXIS2_PLACEMENT_3D('',#74157,#39831,#39832);
#33064=AXIS2_PLACEMENT_3D('',#74182,#39834,#39835);
#33065=AXIS2_PLACEMENT_3D('',#74206,#39837,#39838);
#33066=AXIS2_PLACEMENT_3D('',#74230,#39840,#39841);
#33067=AXIS2_PLACEMENT_3D('',#74255,#39843,#39844);
#33068=AXIS2_PLACEMENT_3D('',#74280,#39846,#39847);
#33069=AXIS2_PLACEMENT_3D('',#74304,#39849,#39850);
#33070=AXIS2_PLACEMENT_3D('',#74329,#39852,#39853);
#33071=AXIS2_PLACEMENT_3D('',#74354,#39855,#39856);
#33072=AXIS2_PLACEMENT_3D('',#74378,#39858,#39859);
#33073=AXIS2_PLACEMENT_3D('',#74403,#39861,#39862);
#33074=AXIS2_PLACEMENT_3D('',#74427,#39864,#39865);
#33075=AXIS2_PLACEMENT_3D('',#74452,#39867,#39868);
#33076=AXIS2_PLACEMENT_3D('',#74476,#39870,#39871);
#33077=AXIS2_PLACEMENT_3D('',#74501,#39873,#39874);
#33078=AXIS2_PLACEMENT_3D('',#74526,#39876,#39877);
#33079=AXIS2_PLACEMENT_3D('',#74550,#39879,#39880);
#33080=AXIS2_PLACEMENT_3D('',#74575,#39882,#39883);
#33081=AXIS2_PLACEMENT_3D('',#74600,#39885,#39886);
#33082=AXIS2_PLACEMENT_3D('',#74624,#39888,#39889);
#33083=AXIS2_PLACEMENT_3D('',#74648,#39891,#39892);
#33084=AXIS2_PLACEMENT_3D('',#74673,#39894,#39895);
#33085=AXIS2_PLACEMENT_3D('',#74698,#39897,#39898);
#33086=AXIS2_PLACEMENT_3D('',#74722,#39900,#39901);
#33087=AXIS2_PLACEMENT_3D('',#74747,#39903,#39904);
#33088=AXIS2_PLACEMENT_3D('',#74772,#39906,#39907);
#33089=AXIS2_PLACEMENT_3D('',#74796,#39909,#39910);
#33090=AXIS2_PLACEMENT_3D('',#74820,#39912,#39913);
#33091=AXIS2_PLACEMENT_3D('',#74845,#39915,#39916);
#33092=AXIS2_PLACEMENT_3D('',#74870,#39918,#39919);
#33093=AXIS2_PLACEMENT_3D('',#74894,#39921,#39922);
#33094=AXIS2_PLACEMENT_3D('',#74919,#39924,#39925);
#33095=AXIS2_PLACEMENT_3D('',#74944,#39927,#39928);
#33096=AXIS2_PLACEMENT_3D('',#74968,#39930,#39931);
#33097=AXIS2_PLACEMENT_3D('',#74992,#39933,#39934);
#33098=AXIS2_PLACEMENT_3D('',#75017,#39936,#39937);
#33099=AXIS2_PLACEMENT_3D('',#75042,#39939,#39940);
#33100=AXIS2_PLACEMENT_3D('',#75066,#39942,#39943);
#33101=AXIS2_PLACEMENT_3D('',#75091,#39945,#39946);
#33102=AXIS2_PLACEMENT_3D('',#75116,#39948,#39949);
#33103=AXIS2_PLACEMENT_3D('',#75140,#39951,#39952);
#33104=AXIS2_PLACEMENT_3D('',#75164,#39954,#39955);
#33105=AXIS2_PLACEMENT_3D('',#75189,#39957,#39958);
#33106=AXIS2_PLACEMENT_3D('',#75214,#39960,#39961);
#33107=AXIS2_PLACEMENT_3D('',#75238,#39963,#39964);
#33108=AXIS2_PLACEMENT_3D('',#75263,#39966,#39967);
#33109=AXIS2_PLACEMENT_3D('',#75288,#39969,#39970);
#33110=AXIS2_PLACEMENT_3D('',#75312,#39972,#39973);
#33111=AXIS2_PLACEMENT_3D('',#75336,#39975,#39976);
#33112=AXIS2_PLACEMENT_3D('',#75361,#39978,#39979);
#33113=AXIS2_PLACEMENT_3D('',#75386,#39981,#39982);
#33114=AXIS2_PLACEMENT_3D('',#75410,#39984,#39985);
#33115=AXIS2_PLACEMENT_3D('',#75435,#39987,#39988);
#33116=AXIS2_PLACEMENT_3D('',#75460,#39990,#39991);
#33117=AXIS2_PLACEMENT_3D('',#75484,#39993,#39994);
#33118=AXIS2_PLACEMENT_3D('',#75508,#39996,#39997);
#33119=AXIS2_PLACEMENT_3D('',#75533,#39999,#40000);
#33120=AXIS2_PLACEMENT_3D('',#75558,#40002,#40003);
#33121=AXIS2_PLACEMENT_3D('',#75582,#40005,#40006);
#33122=AXIS2_PLACEMENT_3D('',#75607,#40008,#40009);
#33123=AXIS2_PLACEMENT_3D('',#75632,#40011,#40012);
#33124=AXIS2_PLACEMENT_3D('',#75656,#40014,#40015);
#33125=AXIS2_PLACEMENT_3D('',#75681,#40017,#40018);
#33126=AXIS2_PLACEMENT_3D('',#75705,#40020,#40021);
#33127=AXIS2_PLACEMENT_3D('',#75730,#40023,#40024);
#33128=AXIS2_PLACEMENT_3D('',#75754,#40026,#40027);
#33129=AXIS2_PLACEMENT_3D('',#75779,#40029,#40030);
#33130=AXIS2_PLACEMENT_3D('',#75804,#40032,#40033);
#33131=AXIS2_PLACEMENT_3D('',#75828,#40035,#40036);
#33132=AXIS2_PLACEMENT_3D('',#75853,#40038,#40039);
#33133=AXIS2_PLACEMENT_3D('',#75878,#40041,#40042);
#33134=AXIS2_PLACEMENT_3D('',#75902,#40044,#40045);
#33135=AXIS2_PLACEMENT_3D('',#75926,#40047,#40048);
#33136=AXIS2_PLACEMENT_3D('',#76035,#40049,#40050);
#33137=AXIS2_PLACEMENT_3D('',#76037,#40051,#40052);
#33138=AXIS2_PLACEMENT_3D('',#78191,#40053,#40054);
#33139=AXIS2_PLACEMENT_3D('',#78193,#40055,#40056);
#33140=AXIS2_PLACEMENT_3D('',#78194,#40057,#40058);
#33141=AXIS2_PLACEMENT_3D('',#78305,#40059,#40060);
#33142=AXIS2_PLACEMENT_3D('',#78306,#40061,#40062);
#33143=AXIS2_PLACEMENT_3D('',#80244,#40063,#40064);
#33144=AXIS2_PLACEMENT_3D('',#80246,#40065,#40066);
#33145=AXIS2_PLACEMENT_3D('',#80249,#40068,#40069);
#33146=AXIS2_PLACEMENT_3D('',#80250,#40070,#40071);
#33147=AXIS2_PLACEMENT_3D('',#80252,#40073,#40074);
#33148=AXIS2_PLACEMENT_3D('',#80253,#40075,#40076);
#33149=AXIS2_PLACEMENT_3D('',#80254,#40077,#40078);
#33150=AXIS2_PLACEMENT_3D('',#80256,#40079,#40080);
#33151=AXIS2_PLACEMENT_3D('',#80258,#40082,#40083);
#33152=AXIS2_PLACEMENT_3D('',#80259,#40084,#40085);
#33153=AXIS2_PLACEMENT_3D('',#80262,#40086,#40087);
#33154=AXIS2_PLACEMENT_3D('',#80263,#40088,#40089);
#33155=AXIS2_PLACEMENT_3D('',#80264,#40090,#40091);
#33156=AXIS2_PLACEMENT_3D('',#80266,#40092,#40093);
#33157=AXIS2_PLACEMENT_3D('',#80270,#40095,#40096);
#33158=AXIS2_PLACEMENT_3D('',#80271,#40097,#40098);
#33159=AXIS2_PLACEMENT_3D('',#80272,#40099,#40100);
#33160=AXIS2_PLACEMENT_3D('',#80274,#40101,#40102);
#33161=AXIS2_PLACEMENT_3D('',#80276,#40104,#40105);
#33162=AXIS2_PLACEMENT_3D('',#80278,#40106,#40107);
#33163=AXIS2_PLACEMENT_3D('',#80279,#40108,#40109);
#33164=AXIS2_PLACEMENT_3D('',#80290,#40113,#40114);
#33165=AXIS2_PLACEMENT_3D('',#80292,#40115,#40116);
#33166=AXIS2_PLACEMENT_3D('',#80303,#40118,#40119);
#33167=AXIS2_PLACEMENT_3D('',#80310,#40120,#40121);
#33168=AXIS2_PLACEMENT_3D('',#80318,#40124,#40125);
#33169=AXIS2_PLACEMENT_3D('',#80320,#40126,#40127);
#33170=AXIS2_PLACEMENT_3D('',#80332,#40128,#40129);
#33171=AXIS2_PLACEMENT_3D('',#80333,#40130,#40131);
#33172=AXIS2_PLACEMENT_3D('',#80335,#40132,#40133);
#33173=AXIS2_PLACEMENT_3D('',#80339,#40135,#40136);
#33174=AXIS2_PLACEMENT_3D('',#80343,#40138,#40139);
#33175=AXIS2_PLACEMENT_3D('',#80347,#40141,#40142);
#33176=AXIS2_PLACEMENT_3D('',#80351,#40144,#40145);
#33177=AXIS2_PLACEMENT_3D('',#80355,#40147,#40148);
#33178=AXIS2_PLACEMENT_3D('',#80359,#40150,#40151);
#33179=AXIS2_PLACEMENT_3D('',#80363,#40153,#40154);
#33180=AXIS2_PLACEMENT_3D('',#80367,#40156,#40157);
#33181=AXIS2_PLACEMENT_3D('',#80371,#40159,#40160);
#33182=AXIS2_PLACEMENT_3D('',#80375,#40162,#40163);
#33183=AXIS2_PLACEMENT_3D('',#80379,#40165,#40166);
#33184=AXIS2_PLACEMENT_3D('',#80383,#40168,#40169);
#33185=AXIS2_PLACEMENT_3D('',#80387,#40171,#40172);
#33186=AXIS2_PLACEMENT_3D('',#80391,#40174,#40175);
#33187=AXIS2_PLACEMENT_3D('',#80394,#40177,#40178);
#33188=AXIS2_PLACEMENT_3D('',#80396,#40179,#40180);
#33189=AXIS2_PLACEMENT_3D('',#80400,#40182,#40183);
#33190=AXIS2_PLACEMENT_3D('',#80404,#40185,#40186);
#33191=AXIS2_PLACEMENT_3D('',#80408,#40188,#40189);
#33192=AXIS2_PLACEMENT_3D('',#80412,#40191,#40192);
#33193=AXIS2_PLACEMENT_3D('',#80416,#40194,#40195);
#33194=AXIS2_PLACEMENT_3D('',#80420,#40197,#40198);
#33195=AXIS2_PLACEMENT_3D('',#80424,#40200,#40201);
#33196=AXIS2_PLACEMENT_3D('',#80428,#40203,#40204);
#33197=AXIS2_PLACEMENT_3D('',#80432,#40206,#40207);
#33198=AXIS2_PLACEMENT_3D('',#80436,#40209,#40210);
#33199=AXIS2_PLACEMENT_3D('',#80440,#40212,#40213);
#33200=AXIS2_PLACEMENT_3D('',#80444,#40215,#40216);
#33201=AXIS2_PLACEMENT_3D('',#80448,#40218,#40219);
#33202=AXIS2_PLACEMENT_3D('',#80450,#40221,#40222);
#33203=AXIS2_PLACEMENT_3D('',#80451,#40223,#40224);
#33204=AXIS2_PLACEMENT_3D('',#80455,#40227,#40228);
#33205=AXIS2_PLACEMENT_3D('',#80457,#40229,#40230);
#33206=AXIS2_PLACEMENT_3D('',#80467,#40232,#40233);
#33207=AXIS2_PLACEMENT_3D('',#80468,#40234,#40235);
#33208=AXIS2_PLACEMENT_3D('',#80473,#40237,#40238);
#33209=AXIS2_PLACEMENT_3D('',#80485,#40239,#40240);
#33210=AXIS2_PLACEMENT_3D('',#80486,#40241,#40242);
#33211=AXIS2_PLACEMENT_3D('',#80490,#40245,#40246);
#33212=AXIS2_PLACEMENT_3D('',#80492,#40247,#40248);
#33213=AXIS2_PLACEMENT_3D('',#80502,#40250,#40251);
#33214=AXIS2_PLACEMENT_3D('',#80503,#40252,#40253);
#33215=AXIS2_PLACEMENT_3D('',#80508,#40255,#40256);
#33216=AXIS2_PLACEMENT_3D('',#80520,#40257,#40258);
#33217=AXIS2_PLACEMENT_3D('',#80521,#40259,#40260);
#33218=AXIS2_PLACEMENT_3D('',#80525,#40263,#40264);
#33219=AXIS2_PLACEMENT_3D('',#80527,#40265,#40266);
#33220=AXIS2_PLACEMENT_3D('',#80537,#40268,#40269);
#33221=AXIS2_PLACEMENT_3D('',#80538,#40270,#40271);
#33222=AXIS2_PLACEMENT_3D('',#80543,#40273,#40274);
#33223=AXIS2_PLACEMENT_3D('',#80555,#40275,#40276);
#33224=AXIS2_PLACEMENT_3D('',#80556,#40277,#40278);
#33225=AXIS2_PLACEMENT_3D('',#80560,#40281,#40282);
#33226=AXIS2_PLACEMENT_3D('',#80562,#40283,#40284);
#33227=AXIS2_PLACEMENT_3D('',#80572,#40286,#40287);
#33228=AXIS2_PLACEMENT_3D('',#80573,#40288,#40289);
#33229=AXIS2_PLACEMENT_3D('',#80578,#40291,#40292);
#33230=AXIS2_PLACEMENT_3D('',#80590,#40293,#40294);
#33231=AXIS2_PLACEMENT_3D('',#80591,#40295,#40296);
#33232=AXIS2_PLACEMENT_3D('',#80595,#40299,#40300);
#33233=AXIS2_PLACEMENT_3D('',#80597,#40301,#40302);
#33234=AXIS2_PLACEMENT_3D('',#80607,#40304,#40305);
#33235=AXIS2_PLACEMENT_3D('',#80608,#40306,#40307);
#33236=AXIS2_PLACEMENT_3D('',#80613,#40309,#40310);
#33237=AXIS2_PLACEMENT_3D('',#80625,#40311,#40312);
#33238=AXIS2_PLACEMENT_3D('',#80626,#40313,#40314);
#33239=AXIS2_PLACEMENT_3D('',#80630,#40317,#40318);
#33240=AXIS2_PLACEMENT_3D('',#80632,#40319,#40320);
#33241=AXIS2_PLACEMENT_3D('',#80642,#40322,#40323);
#33242=AXIS2_PLACEMENT_3D('',#80643,#40324,#40325);
#33243=AXIS2_PLACEMENT_3D('',#80648,#40327,#40328);
#33244=AXIS2_PLACEMENT_3D('',#80660,#40329,#40330);
#33245=AXIS2_PLACEMENT_3D('',#80661,#40331,#40332);
#33246=AXIS2_PLACEMENT_3D('',#80665,#40335,#40336);
#33247=AXIS2_PLACEMENT_3D('',#80667,#40337,#40338);
#33248=AXIS2_PLACEMENT_3D('',#80677,#40340,#40341);
#33249=AXIS2_PLACEMENT_3D('',#80678,#40342,#40343);
#33250=AXIS2_PLACEMENT_3D('',#80683,#40345,#40346);
#33251=AXIS2_PLACEMENT_3D('',#80695,#40347,#40348);
#33252=AXIS2_PLACEMENT_3D('',#80696,#40349,#40350);
#33253=AXIS2_PLACEMENT_3D('',#80700,#40353,#40354);
#33254=AXIS2_PLACEMENT_3D('',#80702,#40355,#40356);
#33255=AXIS2_PLACEMENT_3D('',#80712,#40358,#40359);
#33256=AXIS2_PLACEMENT_3D('',#80713,#40360,#40361);
#33257=AXIS2_PLACEMENT_3D('',#80718,#40363,#40364);
#33258=AXIS2_PLACEMENT_3D('',#80730,#40365,#40366);
#33259=AXIS2_PLACEMENT_3D('',#80731,#40367,#40368);
#33260=AXIS2_PLACEMENT_3D('',#80735,#40371,#40372);
#33261=AXIS2_PLACEMENT_3D('',#80737,#40373,#40374);
#33262=AXIS2_PLACEMENT_3D('',#80747,#40376,#40377);
#33263=AXIS2_PLACEMENT_3D('',#80748,#40378,#40379);
#33264=AXIS2_PLACEMENT_3D('',#80753,#40381,#40382);
#33265=AXIS2_PLACEMENT_3D('',#80765,#40383,#40384);
#33266=AXIS2_PLACEMENT_3D('',#80766,#40385,#40386);
#33267=AXIS2_PLACEMENT_3D('',#80770,#40389,#40390);
#33268=AXIS2_PLACEMENT_3D('',#80772,#40391,#40392);
#33269=AXIS2_PLACEMENT_3D('',#80782,#40394,#40395);
#33270=AXIS2_PLACEMENT_3D('',#80783,#40396,#40397);
#33271=AXIS2_PLACEMENT_3D('',#80788,#40399,#40400);
#33272=AXIS2_PLACEMENT_3D('',#80800,#40401,#40402);
#33273=AXIS2_PLACEMENT_3D('',#80801,#40403,#40404);
#33274=AXIS2_PLACEMENT_3D('',#80805,#40407,#40408);
#33275=AXIS2_PLACEMENT_3D('',#80807,#40409,#40410);
#33276=AXIS2_PLACEMENT_3D('',#80817,#40412,#40413);
#33277=AXIS2_PLACEMENT_3D('',#80818,#40414,#40415);
#33278=AXIS2_PLACEMENT_3D('',#80823,#40417,#40418);
#33279=AXIS2_PLACEMENT_3D('',#80835,#40419,#40420);
#33280=AXIS2_PLACEMENT_3D('',#80836,#40421,#40422);
#33281=AXIS2_PLACEMENT_3D('',#80840,#40425,#40426);
#33282=AXIS2_PLACEMENT_3D('',#80842,#40427,#40428);
#33283=AXIS2_PLACEMENT_3D('',#80852,#40430,#40431);
#33284=AXIS2_PLACEMENT_3D('',#80853,#40432,#40433);
#33285=AXIS2_PLACEMENT_3D('',#80858,#40435,#40436);
#33286=AXIS2_PLACEMENT_3D('',#80870,#40437,#40438);
#33287=AXIS2_PLACEMENT_3D('',#80871,#40439,#40440);
#33288=AXIS2_PLACEMENT_3D('',#80875,#40443,#40444);
#33289=AXIS2_PLACEMENT_3D('',#80877,#40445,#40446);
#33290=AXIS2_PLACEMENT_3D('',#80887,#40448,#40449);
#33291=AXIS2_PLACEMENT_3D('',#80888,#40450,#40451);
#33292=AXIS2_PLACEMENT_3D('',#80893,#40453,#40454);
#33293=AXIS2_PLACEMENT_3D('',#80905,#40455,#40456);
#33294=AXIS2_PLACEMENT_3D('',#80906,#40457,#40458);
#33295=AXIS2_PLACEMENT_3D('',#80910,#40461,#40462);
#33296=AXIS2_PLACEMENT_3D('',#80912,#40463,#40464);
#33297=AXIS2_PLACEMENT_3D('',#80922,#40466,#40467);
#33298=AXIS2_PLACEMENT_3D('',#80923,#40468,#40469);
#33299=AXIS2_PLACEMENT_3D('',#80928,#40471,#40472);
#33300=AXIS2_PLACEMENT_3D('',#80937,#40477,#40478);
#33301=AXIS2_PLACEMENT_3D('',#80943,#40482,#40483);
#33302=AXIS2_PLACEMENT_3D('',#80952,#40488,#40489);
#33303=AXIS2_PLACEMENT_3D('',#80958,#40493,#40494);
#33304=AXIS2_PLACEMENT_3D('',#80961,#40497,#40498);
#33305=AXIS2_PLACEMENT_3D('',#80964,#40501,#40502);
#33306=AXIS2_PLACEMENT_3D('',#80970,#40506,#40507);
#33307=AXIS2_PLACEMENT_3D('',#80974,#40510,#40511);
#33308=AXIS2_PLACEMENT_3D('',#80978,#40514,#40515);
#33309=AXIS2_PLACEMENT_3D('',#80979,#40516,#40517);
#33310=AXIS2_PLACEMENT_3D('',#80980,#40518,#40519);
#33311=AXIS2_PLACEMENT_3D('',#80984,#40522,#40523);
#33312=AXIS2_PLACEMENT_3D('',#80988,#40526,#40527);
#33313=AXIS2_PLACEMENT_3D('',#80990,#40529,#40530);
#33314=AXIS2_PLACEMENT_3D('',#80991,#40531,#40532);
#33315=AXIS2_PLACEMENT_3D('',#80992,#40533,#40534);
#33316=AXIS2_PLACEMENT_3D('',#80993,#40535,#40536);
#33317=AXIS2_PLACEMENT_3D('',#80994,#40537,#40538);
#33318=AXIS2_PLACEMENT_3D('',#80995,#40539,#40540);
#33319=AXIS2_PLACEMENT_3D('',#80996,#40541,#40542);
#33320=AXIS2_PLACEMENT_3D('',#80997,#40543,#40544);
#33321=AXIS2_PLACEMENT_3D('',#80998,#40545,#40546);
#33322=AXIS2_PLACEMENT_3D('',#80999,#40547,#40548);
#33323=AXIS2_PLACEMENT_3D('',#81000,#40549,#40550);
#33324=AXIS2_PLACEMENT_3D('',#81001,#40551,#40552);
#33325=AXIS2_PLACEMENT_3D('',#81002,#40553,#40554);
#33326=AXIS2_PLACEMENT_3D('',#81003,#40555,#40556);
#33327=AXIS2_PLACEMENT_3D('',#81004,#40557,#40558);
#33328=AXIS2_PLACEMENT_3D('',#81005,#40559,#40560);
#33329=AXIS2_PLACEMENT_3D('',#81006,#40561,#40562);
#33330=AXIS2_PLACEMENT_3D('',#81007,#40563,#40564);
#33331=AXIS2_PLACEMENT_3D('',#81009,#40565,#40566);
#33332=AXIS2_PLACEMENT_3D('',#81011,#40568,#40569);
#33333=AXIS2_PLACEMENT_3D('',#81013,#40570,#40571);
#33334=AXIS2_PLACEMENT_3D('',#81015,#40573,#40574);
#33335=AXIS2_PLACEMENT_3D('',#81017,#40575,#40576);
#33336=AXIS2_PLACEMENT_3D('',#81018,#40577,#40578);
#33337=AXIS2_PLACEMENT_3D('',#81020,#40580,#40581);
#33338=AXIS2_PLACEMENT_3D('',#81021,#40582,#40583);
#33339=AXIS2_PLACEMENT_3D('',#81022,#40584,#40585);
#33340=AXIS2_PLACEMENT_3D('',#81038,#40587,#40588);
#33341=AXIS2_PLACEMENT_3D('',#81046,#40589,#40590);
#33342=AXIS2_PLACEMENT_3D('',#81094,#40592,#40593);
#33343=AXIS2_PLACEMENT_3D('',#81142,#40595,#40596);
#33344=AXIS2_PLACEMENT_3D('',#81196,#40598,#40599);
#33345=AXIS2_PLACEMENT_3D('',#81244,#40601,#40602);
#33346=AXIS2_PLACEMENT_3D('',#81292,#40604,#40605);
#33347=AXIS2_PLACEMENT_3D('',#81340,#40607,#40608);
#33348=AXIS2_PLACEMENT_3D('',#81356,#40610,#40611);
#33349=AXIS2_PLACEMENT_3D('',#81366,#40612,#40613);
#33350=AXIS2_PLACEMENT_3D('',#81390,#40615,#40616);
#33351=AXIS2_PLACEMENT_3D('',#81414,#40618,#40619);
#33352=AXIS2_PLACEMENT_3D('',#81439,#40621,#40622);
#33353=AXIS2_PLACEMENT_3D('',#81464,#40624,#40625);
#33354=AXIS2_PLACEMENT_3D('',#81488,#40627,#40628);
#33355=AXIS2_PLACEMENT_3D('',#81576,#40629,#40630);
#33356=AXIS2_PLACEMENT_3D('',#81578,#40631,#40632);
#33357=AXIS2_PLACEMENT_3D('',#81960,#40633,#40634);
#33358=AXIS2_PLACEMENT_3D('',#81962,#40635,#40636);
#33359=AXIS2_PLACEMENT_3D('',#81963,#40637,#40638);
#33360=AXIS2_PLACEMENT_3D('',#82050,#40639,#40640);
#33361=AXIS2_PLACEMENT_3D('',#82051,#40641,#40642);
#33362=AXIS2_PLACEMENT_3D('',#82258,#40643,#40644);
#33363=AXIS2_PLACEMENT_3D('',#82267,#40649,#40650);
#33364=AXIS2_PLACEMENT_3D('',#82273,#40654,#40655);
#33365=AXIS2_PLACEMENT_3D('',#82279,#40659,#40660);
#33366=AXIS2_PLACEMENT_3D('',#82285,#40664,#40665);
#33367=AXIS2_PLACEMENT_3D('',#82291,#40669,#40670);
#33368=AXIS2_PLACEMENT_3D('',#82294,#40673,#40674);
#33369=AXIS2_PLACEMENT_3D('',#82295,#40675,#40676);
#33370=AXIS2_PLACEMENT_3D('',#82297,#40677,#40678);
#33371=AXIS2_PLACEMENT_3D('',#82298,#40679,#40680);
#33372=AXIS2_PLACEMENT_3D('',#82300,#40682,#40683);
#33373=AXIS2_PLACEMENT_3D('',#82301,#40684,#40685);
#33374=AXIS2_PLACEMENT_3D('',#82302,#40686,#40687);
#33375=AXIS2_PLACEMENT_3D('',#82304,#40688,#40689);
#33376=AXIS2_PLACEMENT_3D('',#82306,#40691,#40692);
#33377=AXIS2_PLACEMENT_3D('',#82307,#40693,#40694);
#33378=AXIS2_PLACEMENT_3D('',#82308,#40695,#40696);
#33379=AXIS2_PLACEMENT_3D('',#82309,#40697,#40698);
#33380=AXIS2_PLACEMENT_3D('',#82310,#40699,#40700);
#33381=AXIS2_PLACEMENT_3D('',#82311,#40701,#40702);
#33382=AXIS2_PLACEMENT_3D('',#82312,#40703,#40704);
#33383=AXIS2_PLACEMENT_3D('',#82313,#40705,#40706);
#33384=AXIS2_PLACEMENT_3D('',#82314,#40707,#40708);
#33385=AXIS2_PLACEMENT_3D('',#82315,#40709,#40710);
#33386=AXIS2_PLACEMENT_3D('',#82316,#40711,#40712);
#33387=AXIS2_PLACEMENT_3D('',#82317,#40713,#40714);
#33388=AXIS2_PLACEMENT_3D('',#82318,#40715,#40716);
#33389=AXIS2_PLACEMENT_3D('',#82319,#40717,#40718);
#33390=AXIS2_PLACEMENT_3D('',#82320,#40719,#40720);
#33391=AXIS2_PLACEMENT_3D('',#82321,#40721,#40722);
#33392=AXIS2_PLACEMENT_3D('',#82322,#40723,#40724);
#33393=AXIS2_PLACEMENT_3D('',#82323,#40725,#40726);
#33394=AXIS2_PLACEMENT_3D('',#82324,#40727,#40728);
#33395=AXIS2_PLACEMENT_3D('',#82325,#40729,#40730);
#33396=AXIS2_PLACEMENT_3D('',#82326,#40731,#40732);
#33397=AXIS2_PLACEMENT_3D('',#82327,#40733,#40734);
#33398=AXIS2_PLACEMENT_3D('',#82328,#40735,#40736);
#33399=AXIS2_PLACEMENT_3D('',#82329,#40737,#40738);
#33400=AXIS2_PLACEMENT_3D('',#82330,#40739,#40740);
#33401=AXIS2_PLACEMENT_3D('',#82331,#40741,#40742);
#33402=AXIS2_PLACEMENT_3D('',#82332,#40743,#40744);
#33403=AXIS2_PLACEMENT_3D('',#82333,#40745,#40746);
#33404=AXIS2_PLACEMENT_3D('',#82334,#40747,#40748);
#33405=AXIS2_PLACEMENT_3D('',#82335,#40749,#40750);
#33406=AXIS2_PLACEMENT_3D('',#82336,#40751,#40752);
#33407=AXIS2_PLACEMENT_3D('',#82337,#40753,#40754);
#33408=AXIS2_PLACEMENT_3D('',#82338,#40755,#40756);
#33409=AXIS2_PLACEMENT_3D('',#82339,#40757,#40758);
#33410=AXIS2_PLACEMENT_3D('',#82340,#40759,#40760);
#33411=AXIS2_PLACEMENT_3D('',#82341,#40761,#40762);
#33412=AXIS2_PLACEMENT_3D('',#82342,#40763,#40764);
#33413=DIRECTION('axis',(0.,0.,1.));
#33414=DIRECTION('refdir',(1.,0.,0.));
#33415=DIRECTION('axis',(0.,0.,1.));
#33416=DIRECTION('refdir',(1.,0.,0.));
#33417=DIRECTION('center_axis',(0.707106781186548,0.707106781186548,0.));
#33418=DIRECTION('ref_axis',(0.,0.,-1.));
#33419=DIRECTION('',(0.577350269189628,-0.577350269189628,-0.577350269189621));
#33420=DIRECTION('',(0.,0.,-1.));
#33421=DIRECTION('',(-0.577350269189629,0.577350269189629,-0.57735026918962));
#33422=DIRECTION('',(-0.577350269189629,0.577350269189629,0.57735026918962));
#33423=DIRECTION('',(0.,0.,1.));
#33424=DIRECTION('',(0.577350269189628,-0.577350269189628,0.577350269189621));
#33425=DIRECTION('center_axis',(1.,0.,0.));
#33426=DIRECTION('ref_axis',(0.,1.,0.));
#33427=DIRECTION('',(0.,1.,0.));
#33428=DIRECTION('',(0.,0.,1.));
#33429=DIRECTION('',(0.,-1.,0.));
#33430=DIRECTION('center_axis',(0.707106781186543,0.,0.707106781186552));
#33431=DIRECTION('ref_axis',(0.707106781186552,0.,-0.707106781186543));
#33432=DIRECTION('',(0.577350269189635,0.577350269189615,-0.577350269189628));
#33433=DIRECTION('',(0.,-1.,0.));
#33434=DIRECTION('',(0.577350269189628,-0.577350269189628,-0.577350269189621));
#33435=DIRECTION('',(-0.577350269189628,-0.577350269189628,0.577350269189621));
#33436=DIRECTION('center_axis',(0.,0.707106781186543,0.707106781186552));
#33437=DIRECTION('ref_axis',(1.,0.,0.));
#33438=DIRECTION('',(-1.,0.,0.));
#33439=DIRECTION('',(0.,-0.707106781186552,0.707106781186543));
#33440=DIRECTION('',(1.,0.,0.));
#33441=DIRECTION('center_axis',(0.707106781186548,-0.707106781186548,0.));
#33442=DIRECTION('ref_axis',(0.,0.,-1.));
#33443=DIRECTION('',(-0.577350269189628,-0.577350269189628,-0.577350269189621));
#33444=DIRECTION('',(0.,0.,-1.));
#33445=DIRECTION('',(0.577350269189629,0.577350269189629,-0.57735026918962));
#33446=DIRECTION('',(0.577350269189629,0.577350269189629,0.57735026918962));
#33447=DIRECTION('center_axis',(0.707106781186543,0.,-0.707106781186553));
#33448=DIRECTION('ref_axis',(-0.707106781186553,0.,-0.707106781186543));
#33449=DIRECTION('',(0.577350269189629,-0.577350269189629,0.57735026918962));
#33450=DIRECTION('',(0.,1.,0.));
#33451=DIRECTION('',(0.577350269189629,0.577350269189629,0.57735026918962));
#33452=DIRECTION('center_axis',(0.,-0.707106781186543,-0.707106781186553));
#33453=DIRECTION('ref_axis',(-1.,0.,0.));
#33454=DIRECTION('',(-1.,0.,0.));
#33455=DIRECTION('',(0.577350269189629,-0.577350269189629,0.57735026918962));
#33456=DIRECTION('',(-0.577350269189622,-0.577350269189632,0.577350269189624));
#33457=DIRECTION('',(1.,0.,0.));
#33458=DIRECTION('center_axis',(0.,-1.,0.));
#33459=DIRECTION('ref_axis',(1.,0.,0.));
#33460=DIRECTION('',(1.,0.,0.));
#33461=DIRECTION('',(0.,0.,1.));
#33462=DIRECTION('',(1.,0.,0.));
#33463=DIRECTION('',(0.,0.,-1.));
#33464=DIRECTION('',(-1.,0.,0.));
#33465=DIRECTION('',(0.,0.,1.));
#33466=DIRECTION('',(1.,0.,0.));
#33467=DIRECTION('',(0.,0.,-1.));
#33468=DIRECTION('',(-1.,0.,0.));
#33469=DIRECTION('',(0.,0.,-1.));
#33470=DIRECTION('',(1.,0.,0.));
#33471=DIRECTION('',(0.,0.,-1.));
#33472=DIRECTION('',(-1.,0.,0.));
#33473=DIRECTION('',(0.,0.,-1.));
#33474=DIRECTION('',(-1.,0.,0.));
#33475=DIRECTION('',(0.,0.,-1.));
#33476=DIRECTION('',(-1.,0.,0.));
#33477=DIRECTION('',(0.,0.,1.));
#33478=DIRECTION('',(1.,0.,0.));
#33479=DIRECTION('',(0.538514489852619,0.,-0.842616249676431));
#33480=DIRECTION('',(-1.,0.,0.));
#33481=DIRECTION('',(-0.536696608221845,0.,0.843775296345637));
#33482=DIRECTION('',(1.,0.,0.));
#33483=DIRECTION('',(0.,0.,-1.));
#33484=DIRECTION('',(-1.,0.,0.));
#33485=DIRECTION('',(0.,0.,1.));
#33486=DIRECTION('',(1.,0.,0.));
#33487=DIRECTION('',(0.,0.,-1.));
#33488=DIRECTION('',(-1.,0.,0.));
#33489=DIRECTION('',(0.,0.,-1.));
#33490=DIRECTION('',(1.,0.,0.));
#33491=DIRECTION('',(0.,0.,-1.));
#33492=DIRECTION('',(-1.,0.,0.));
#33493=DIRECTION('',(0.,0.,-1.));
#33494=DIRECTION('',(-1.,0.,0.));
#33495=DIRECTION('',(0.,0.,1.));
#33496=DIRECTION('',(1.,0.,0.));
#33497=DIRECTION('',(0.,0.,-1.));
#33498=DIRECTION('',(-1.,0.,0.));
#33499=DIRECTION('',(0.996199647084823,0.,0.0870991569883124));
#33500=DIRECTION('',(-0.997179320834183,0.,-0.0750559931030013));
#33501=DIRECTION('',(0.991227966055039,0.,0.132163229797056));
#33502=DIRECTION('',(0.125580368698037,0.,0.992083449613824));
#33503=DIRECTION('',(-0.984562438638901,0.,0.175033723668955));
#33504=DIRECTION('',(1.,0.,0.));
#33505=DIRECTION('',(0.,0.,-1.));
#33506=DIRECTION('',(-1.,0.,0.));
#33507=DIRECTION('',(0.,0.,1.));
#33508=DIRECTION('',(0.996199663122956,0.,0.0870989735514131));
#33509=DIRECTION('',(-0.997179320834183,0.,-0.0750559931030013));
#33510=DIRECTION('center_axis',(-0.707106781186548,-0.707106781186548,0.));
#33511=DIRECTION('ref_axis',(0.,0.,1.));
#33512=DIRECTION('',(-0.577350269189625,0.577350269189625,-0.577350269189627));
#33513=DIRECTION('',(0.,0.,-1.));
#33514=DIRECTION('',(0.577350269189625,-0.577350269189625,-0.577350269189627));
#33515=DIRECTION('',(-0.577350269189628,0.577350269189628,0.577350269189621));
#33516=DIRECTION('center_axis',(-0.707106781186549,0.,-0.707106781186546));
#33517=DIRECTION('ref_axis',(-0.707106781186546,0.,0.707106781186549));
#33518=DIRECTION('',(0.,1.,0.));
#33519=DIRECTION('',(0.577350269189625,0.577350269189625,-0.577350269189627));
#33520=DIRECTION('',(0.,-1.,0.));
#33521=DIRECTION('center_axis',(0.,-1.,0.));
#33522=DIRECTION('ref_axis',(1.,0.,0.));
#33523=DIRECTION('center_axis',(0.,-1.,0.));
#33524=DIRECTION('ref_axis',(1.,0.,0.));
#33525=DIRECTION('',(0.707106781186547,0.707106781186547,8.65956056235493E-17));
#33526=DIRECTION('center_axis',(0.,1.,0.));
#33527=DIRECTION('ref_axis',(1.,0.,0.));
#33528=DIRECTION('center_axis',(0.,-1.,0.));
#33529=DIRECTION('ref_axis',(1.,0.,0.));
#33530=DIRECTION('',(1.,0.,0.));
#33531=DIRECTION('',(0.,0.,1.));
#33532=DIRECTION('',(-1.,0.,0.));
#33533=DIRECTION('',(0.,0.,1.));
#33534=DIRECTION('center_axis',(0.,-1.,0.));
#33535=DIRECTION('ref_axis',(1.,0.,0.));
#33536=DIRECTION('center_axis',(0.,1.,0.));
#33537=DIRECTION('ref_axis',(1.,0.,0.));
#33538=DIRECTION('',(0.,1.,0.));
#33539=DIRECTION('center_axis',(0.,1.,0.));
#33540=DIRECTION('ref_axis',(1.,0.,0.));
#33541=DIRECTION('center_axis',(0.,-1.,0.));
#33542=DIRECTION('ref_axis',(1.,0.,0.));
#33543=DIRECTION('',(0.707106781186547,0.707106781186547,8.65956056235493E-17));
#33544=DIRECTION('center_axis',(0.,1.,0.));
#33545=DIRECTION('ref_axis',(1.,0.,0.));
#33546=DIRECTION('center_axis',(0.,1.,0.));
#33547=DIRECTION('ref_axis',(1.,0.,0.));
#33548=DIRECTION('',(0.,1.,0.));
#33549=DIRECTION('center_axis',(0.,1.,0.));
#33550=DIRECTION('ref_axis',(1.,0.,0.));
#33551=DIRECTION('center_axis',(0.,0.,1.));
#33552=DIRECTION('ref_axis',(1.,0.,0.));
#33553=DIRECTION('center_axis',(0.,0.,-1.));
#33554=DIRECTION('ref_axis',(1.,0.,0.));
#33555=DIRECTION('',(-0.707106781186547,8.65956056235493E-17,0.707106781186548));
#33556=DIRECTION('center_axis',(0.,0.,1.));
#33557=DIRECTION('ref_axis',(1.,0.,0.));
#33558=DIRECTION('center_axis',(0.,0.,-1.));
#33559=DIRECTION('ref_axis',(1.,0.,0.));
#33560=DIRECTION('',(0.,0.,-1.));
#33561=DIRECTION('center_axis',(0.,0.,1.));
#33562=DIRECTION('ref_axis',(1.,0.,0.));
#33563=DIRECTION('center_axis',(0.,0.,1.));
#33564=DIRECTION('ref_axis',(1.,0.,0.));
#33565=DIRECTION('center_axis',(0.,0.,-1.));
#33566=DIRECTION('ref_axis',(1.,0.,0.));
#33567=DIRECTION('center_axis',(0.,0.,1.));
#33568=DIRECTION('ref_axis',(1.,0.,0.));
#33569=DIRECTION('center_axis',(0.,0.,-1.));
#33570=DIRECTION('ref_axis',(1.,0.,0.));
#33571=DIRECTION('',(-0.707106781186546,8.65956056235491E-17,0.707106781186549));
#33572=DIRECTION('center_axis',(0.,0.,1.));
#33573=DIRECTION('ref_axis',(1.,0.,0.));
#33574=DIRECTION('center_axis',(0.,0.,-1.));
#33575=DIRECTION('ref_axis',(1.,0.,0.));
#33576=DIRECTION('',(0.,0.,-1.));
#33577=DIRECTION('center_axis',(0.,0.,1.));
#33578=DIRECTION('ref_axis',(1.,0.,0.));
#33579=DIRECTION('center_axis',(0.,0.,1.));
#33580=DIRECTION('ref_axis',(1.,0.,0.));
#33581=DIRECTION('center_axis',(0.,0.,-1.));
#33582=DIRECTION('ref_axis',(1.,0.,0.));
#33583=DIRECTION('center_axis',(0.,0.,1.));
#33584=DIRECTION('ref_axis',(1.,0.,0.));
#33585=DIRECTION('center_axis',(0.,0.,-1.));
#33586=DIRECTION('ref_axis',(1.,0.,0.));
#33587=DIRECTION('',(-0.707106781186546,8.65956056235491E-17,0.707106781186549));
#33588=DIRECTION('center_axis',(0.,0.,1.));
#33589=DIRECTION('ref_axis',(1.,0.,0.));
#33590=DIRECTION('center_axis',(0.,0.,-1.));
#33591=DIRECTION('ref_axis',(1.,0.,0.));
#33592=DIRECTION('',(0.,0.,-1.));
#33593=DIRECTION('center_axis',(0.,0.,1.));
#33594=DIRECTION('ref_axis',(1.,0.,0.));
#33595=DIRECTION('center_axis',(0.,0.,1.));
#33596=DIRECTION('ref_axis',(1.,0.,0.));
#33597=DIRECTION('center_axis',(0.,0.,-1.));
#33598=DIRECTION('ref_axis',(1.,0.,0.));
#33599=DIRECTION('center_axis',(0.,0.,1.));
#33600=DIRECTION('ref_axis',(1.,0.,0.));
#33601=DIRECTION('center_axis',(0.,0.,-1.));
#33602=DIRECTION('ref_axis',(1.,0.,0.));
#33603=DIRECTION('',(-0.707106781186547,8.65956056235493E-17,0.707106781186548));
#33604=DIRECTION('center_axis',(0.,0.,1.));
#33605=DIRECTION('ref_axis',(1.,0.,0.));
#33606=DIRECTION('center_axis',(0.,0.,-1.));
#33607=DIRECTION('ref_axis',(1.,0.,0.));
#33608=DIRECTION('',(0.,0.,-1.));
#33609=DIRECTION('center_axis',(0.,0.,1.));
#33610=DIRECTION('ref_axis',(1.,0.,0.));
#33611=DIRECTION('center_axis',(0.,0.,1.));
#33612=DIRECTION('ref_axis',(1.,0.,0.));
#33613=DIRECTION('center_axis',(0.,0.,-1.));
#33614=DIRECTION('ref_axis',(1.,0.,0.));
#33615=DIRECTION('center_axis',(0.,-0.707106781186543,0.707106781186552));
#33616=DIRECTION('ref_axis',(1.,0.,0.));
#33617=DIRECTION('',(-1.,0.,0.));
#33618=DIRECTION('',(-0.577350269189622,-0.577350269189632,-0.577350269189624));
#33619=DIRECTION('center_axis',(-0.707106781186549,0.,0.707106781186546));
#33620=DIRECTION('ref_axis',(0.707106781186546,0.,0.707106781186549));
#33621=DIRECTION('',(0.,1.,0.));
#33622=DIRECTION('',(-0.577350269189625,-0.577350269189625,-0.577350269189628));
#33623=DIRECTION('',(0.,-1.,0.));
#33624=DIRECTION('center_axis',(-0.577350269189623,0.577350269189623,0.577350269189631));
#33625=DIRECTION('ref_axis',(0.707106781186552,0.,0.707106781186543));
#33626=DIRECTION('',(0.707106781186547,0.707106781186547,0.));
#33627=DIRECTION('',(-0.707106781186552,0.,-0.707106781186543));
#33628=DIRECTION('center_axis',(-0.57735026918962,-0.57735026918963,0.577350269189628));
#33629=DIRECTION('ref_axis',(0.707106781186552,0.,0.707106781186543));
#33630=DIRECTION('',(0.707106781186552,0.,0.707106781186543));
#33631=DIRECTION('',(-0.707106781186554,0.707106781186541,0.));
#33632=DIRECTION('',(0.,-0.707106781186546,-0.707106781186549));
#33633=DIRECTION('center_axis',(-0.577350269189623,0.577350269189623,-0.577350269189631));
#33634=DIRECTION('ref_axis',(-0.707106781186553,0.,0.707106781186543));
#33635=DIRECTION('',(-0.707106781186547,-0.707106781186547,0.));
#33636=DIRECTION('',(0.,0.707106781186552,0.707106781186542));
#33637=DIRECTION('',(0.707106781186552,0.,-0.707106781186542));
#33638=DIRECTION('center_axis',(-0.57735026918962,-0.57735026918963,-0.577350269189628));
#33639=DIRECTION('ref_axis',(-0.707106781186553,0.,0.707106781186543));
#33640=DIRECTION('',(0.707106781186554,-0.707106781186541,0.));
#33641=DIRECTION('',(-0.707106781186552,0.,0.707106781186542));
#33642=DIRECTION('',(0.,0.707106781186546,-0.707106781186549));
#33643=DIRECTION('center_axis',(-0.707106781186543,0.,-0.707106781186553));
#33644=DIRECTION('ref_axis',(-0.707106781186553,0.,0.707106781186543));
#33645=DIRECTION('',(0.,1.,0.));
#33646=DIRECTION('',(0.,-1.,0.));
#33647=DIRECTION('center_axis',(0.,-0.707106781186549,-0.707106781186546));
#33648=DIRECTION('ref_axis',(-1.,0.,0.));
#33649=DIRECTION('',(1.,0.,0.));
#33650=DIRECTION('center_axis',(-0.707106781186541,-0.707106781186554,0.));
#33651=DIRECTION('ref_axis',(0.,0.,1.));
#33652=DIRECTION('',(0.,0.,-1.));
#33653=DIRECTION('center_axis',(0.,0.707106781186543,-0.707106781186553));
#33654=DIRECTION('ref_axis',(-1.,0.,0.));
#33655=DIRECTION('',(-1.,0.,0.));
#33656=DIRECTION('',(1.,0.,0.));
#33657=DIRECTION('center_axis',(-0.707106781186548,0.707106781186548,0.));
#33658=DIRECTION('ref_axis',(0.,0.,1.));
#33659=DIRECTION('',(0.,0.,-1.));
#33660=DIRECTION('',(0.,0.,1.));
#33661=DIRECTION('center_axis',(0.,-0.707106781186549,0.707106781186546));
#33662=DIRECTION('ref_axis',(1.,0.,0.));
#33663=DIRECTION('',(-1.,0.,0.));
#33664=DIRECTION('center_axis',(-0.707106781186543,0.,0.707106781186552));
#33665=DIRECTION('ref_axis',(0.707106781186552,0.,0.707106781186543));
#33666=DIRECTION('',(0.,1.,0.));
#33667=DIRECTION('',(0.,-1.,0.));
#33668=DIRECTION('center_axis',(-1.,0.,0.));
#33669=DIRECTION('ref_axis',(0.,-1.,0.));
#33670=DIRECTION('center_axis',(0.,0.,1.));
#33671=DIRECTION('ref_axis',(1.,0.,0.));
#33672=DIRECTION('center_axis',(0.,0.,1.));
#33673=DIRECTION('ref_axis',(1.,0.,0.));
#33674=DIRECTION('center_axis',(0.,0.,1.));
#33675=DIRECTION('ref_axis',(1.,0.,0.));
#33676=DIRECTION('center_axis',(0.,0.,1.));
#33677=DIRECTION('ref_axis',(1.,0.,0.));
#33678=DIRECTION('center_axis',(0.,0.,1.));
#33679=DIRECTION('ref_axis',(1.,0.,0.));
#33680=DIRECTION('center_axis',(0.,0.,1.));
#33681=DIRECTION('ref_axis',(1.,0.,0.));
#33682=DIRECTION('center_axis',(0.,0.,1.));
#33683=DIRECTION('ref_axis',(1.,0.,0.));
#33684=DIRECTION('center_axis',(0.,0.,1.));
#33685=DIRECTION('ref_axis',(1.,0.,0.));
#33686=DIRECTION('center_axis',(0.,0.,1.));
#33687=DIRECTION('ref_axis',(1.,0.,0.));
#33688=DIRECTION('center_axis',(0.,0.,-1.));
#33689=DIRECTION('ref_axis',(1.,0.,0.));
#33690=DIRECTION('center_axis',(0.,0.,1.));
#33691=DIRECTION('ref_axis',(1.,0.,0.));
#33692=DIRECTION('center_axis',(0.,0.,1.));
#33693=DIRECTION('ref_axis',(1.,0.,0.));
#33694=DIRECTION('center_axis',(0.,0.,1.));
#33695=DIRECTION('ref_axis',(1.,0.,0.));
#33696=DIRECTION('center_axis',(0.,0.,1.));
#33697=DIRECTION('ref_axis',(1.,0.,0.));
#33698=DIRECTION('center_axis',(0.,0.,1.));
#33699=DIRECTION('ref_axis',(1.,0.,0.));
#33700=DIRECTION('center_axis',(0.,0.,1.));
#33701=DIRECTION('ref_axis',(1.,0.,0.));
#33702=DIRECTION('center_axis',(0.,0.,1.));
#33703=DIRECTION('ref_axis',(1.,0.,0.));
#33704=DIRECTION('center_axis',(0.,0.,1.));
#33705=DIRECTION('ref_axis',(1.,0.,0.));
#33706=DIRECTION('center_axis',(-1.,0.,0.));
#33707=DIRECTION('ref_axis',(0.,-1.,0.));
#33708=DIRECTION('center_axis',(0.,0.,1.));
#33709=DIRECTION('ref_axis',(1.,0.,0.));
#33710=DIRECTION('center_axis',(0.,0.,-1.));
#33711=DIRECTION('ref_axis',(1.,0.,0.));
#33712=DIRECTION('center_axis',(0.,0.,-1.));
#33713=DIRECTION('ref_axis',(1.,0.,0.));
#33714=DIRECTION('center_axis',(0.,0.,-1.));
#33715=DIRECTION('ref_axis',(1.,0.,0.));
#33716=DIRECTION('center_axis',(0.,0.,-1.));
#33717=DIRECTION('ref_axis',(1.,0.,0.));
#33718=DIRECTION('center_axis',(0.,0.,-1.));
#33719=DIRECTION('ref_axis',(1.,0.,0.));
#33720=DIRECTION('center_axis',(0.,0.,1.));
#33721=DIRECTION('ref_axis',(1.,0.,0.));
#33722=DIRECTION('',(0.,1.,0.));
#33723=DIRECTION('',(1.,0.,0.));
#33724=DIRECTION('',(0.,1.,0.));
#33725=DIRECTION('center_axis',(1.,0.,0.));
#33726=DIRECTION('ref_axis',(0.,0.,-1.));
#33727=DIRECTION('',(0.,1.,0.));
#33728=DIRECTION('',(0.,0.,-1.));
#33729=DIRECTION('center_axis',(0.,0.,-1.));
#33730=DIRECTION('ref_axis',(-1.,0.,0.));
#33731=DIRECTION('',(0.,1.,0.));
#33732=DIRECTION('',(-1.,0.,0.));
#33733=DIRECTION('center_axis',(1.,0.,0.));
#33734=DIRECTION('ref_axis',(0.,0.,-1.));
#33735=DIRECTION('',(0.,1.,0.));
#33736=DIRECTION('',(0.,0.,-1.));
#33737=DIRECTION('center_axis',(0.,0.,1.));
#33738=DIRECTION('ref_axis',(1.,0.,0.));
#33739=DIRECTION('',(0.,1.,0.));
#33740=DIRECTION('',(1.,0.,0.));
#33741=DIRECTION('center_axis',(1.,0.,0.));
#33742=DIRECTION('ref_axis',(0.,0.,-1.));
#33743=DIRECTION('',(0.,1.,0.));
#33744=DIRECTION('',(0.,0.,-1.));
#33745=DIRECTION('center_axis',(0.,0.,-1.));
#33746=DIRECTION('ref_axis',(-1.,0.,0.));
#33747=DIRECTION('',(0.,1.,0.));
#33748=DIRECTION('',(-1.,0.,0.));
#33749=DIRECTION('center_axis',(1.,0.,0.));
#33750=DIRECTION('ref_axis',(0.,0.,-1.));
#33751=DIRECTION('',(0.,1.,0.));
#33752=DIRECTION('',(0.,0.,-1.));
#33753=DIRECTION('center_axis',(0.,0.,1.));
#33754=DIRECTION('ref_axis',(1.,0.,0.));
#33755=DIRECTION('',(0.,1.,0.));
#33756=DIRECTION('',(1.,0.,0.));
#33757=DIRECTION('center_axis',(-1.,0.,0.));
#33758=DIRECTION('ref_axis',(0.,0.,1.));
#33759=DIRECTION('',(0.,1.,0.));
#33760=DIRECTION('',(0.,0.,1.));
#33761=DIRECTION('center_axis',(0.,0.,-1.));
#33762=DIRECTION('ref_axis',(-1.,0.,0.));
#33763=DIRECTION('',(0.,1.,0.));
#33764=DIRECTION('',(-1.,0.,0.));
#33765=DIRECTION('center_axis',(1.,0.,0.));
#33766=DIRECTION('ref_axis',(0.,0.,-1.));
#33767=DIRECTION('',(0.,0.,-1.));
#33768=DIRECTION('center_axis',(0.,1.,0.));
#33769=DIRECTION('ref_axis',(0.,0.,1.));
#33770=DIRECTION('center_axis',(0.,0.,-1.));
#33771=DIRECTION('ref_axis',(-1.,0.,0.));
#33772=DIRECTION('',(0.,1.,0.));
#33773=DIRECTION('',(-1.,0.,0.));
#33774=DIRECTION('',(0.,1.,0.));
#33775=DIRECTION('',(0.,1.,0.));
#33776=DIRECTION('',(0.,1.,0.));
#33777=DIRECTION('',(0.,1.,0.));
#33778=DIRECTION('',(0.,1.,0.));
#33779=DIRECTION('center_axis',(-0.843775296345637,0.,-0.536696608221845));
#33780=DIRECTION('ref_axis',(-0.536696608221845,0.,0.843775296345637));
#33781=DIRECTION('',(0.,1.,0.));
#33782=DIRECTION('',(-0.536696608221845,0.,0.843775296345637));
#33783=DIRECTION('center_axis',(0.,0.,-1.));
#33784=DIRECTION('ref_axis',(-1.,0.,0.));
#33785=DIRECTION('',(0.,1.,0.));
#33786=DIRECTION('',(-1.,0.,0.));
#33787=DIRECTION('center_axis',(0.842616249676431,0.,0.538514489852619));
#33788=DIRECTION('ref_axis',(0.538514489852619,0.,-0.842616249676431));
#33789=DIRECTION('',(0.,1.,0.));
#33790=DIRECTION('',(0.538514489852619,0.,-0.842616249676431));
#33791=DIRECTION('',(0.,1.,0.));
#33792=DIRECTION('',(0.,1.,0.));
#33793=DIRECTION('',(0.,1.,0.));
#33794=DIRECTION('',(0.,1.,0.));
#33795=DIRECTION('',(0.,1.,0.));
#33796=DIRECTION('',(0.,1.,0.));
#33797=DIRECTION('',(0.,1.,0.));
#33798=DIRECTION('center_axis',(0.,0.,1.));
#33799=DIRECTION('ref_axis',(1.,0.,0.));
#33800=DIRECTION('',(0.,1.,0.));
#33801=DIRECTION('',(1.,0.,0.));
#33802=DIRECTION('center_axis',(-1.,0.,0.));
#33803=DIRECTION('ref_axis',(0.,0.,1.));
#33804=DIRECTION('',(0.,1.,0.));
#33805=DIRECTION('',(0.,0.,1.));
#33806=DIRECTION('center_axis',(0.,0.,-1.));
#33807=DIRECTION('ref_axis',(-1.,0.,0.));
#33808=DIRECTION('',(0.,1.,0.));
#33809=DIRECTION('',(-1.,0.,0.));
#33810=DIRECTION('center_axis',(1.,0.,0.));
#33811=DIRECTION('ref_axis',(0.,0.,-1.));
#33812=DIRECTION('',(0.,0.,-1.));
#33813=DIRECTION('center_axis',(0.,-1.,0.));
#33814=DIRECTION('ref_axis',(1.,0.,0.));
#33815=DIRECTION('center_axis',(0.,0.,1.));
#33816=DIRECTION('ref_axis',(1.,0.,0.));
#33817=DIRECTION('',(0.,1.,0.));
#33818=DIRECTION('',(1.,0.,0.));
#33819=DIRECTION('',(0.,1.,0.));
#33820=DIRECTION('center_axis',(1.,0.,0.));
#33821=DIRECTION('ref_axis',(0.,0.,-1.));
#33822=DIRECTION('',(0.,1.,0.));
#33823=DIRECTION('',(0.,0.,-1.));
#33824=DIRECTION('center_axis',(0.,0.,-1.));
#33825=DIRECTION('ref_axis',(-1.,0.,0.));
#33826=DIRECTION('',(0.,1.,0.));
#33827=DIRECTION('',(-1.,0.,0.));
#33828=DIRECTION('center_axis',(1.,0.,0.));
#33829=DIRECTION('ref_axis',(0.,0.,-1.));
#33830=DIRECTION('',(0.,1.,0.));
#33831=DIRECTION('',(0.,0.,-1.));
#33832=DIRECTION('center_axis',(0.,0.,1.));
#33833=DIRECTION('ref_axis',(1.,0.,0.));
#33834=DIRECTION('',(0.,1.,0.));
#33835=DIRECTION('',(1.,0.,0.));
#33836=DIRECTION('center_axis',(1.,0.,0.));
#33837=DIRECTION('ref_axis',(0.,0.,-1.));
#33838=DIRECTION('',(0.,1.,0.));
#33839=DIRECTION('',(0.,0.,-1.));
#33840=DIRECTION('center_axis',(0.,0.,-1.));
#33841=DIRECTION('ref_axis',(-1.,0.,0.));
#33842=DIRECTION('',(0.,1.,0.));
#33843=DIRECTION('',(-1.,0.,0.));
#33844=DIRECTION('center_axis',(1.,0.,0.));
#33845=DIRECTION('ref_axis',(0.,0.,-1.));
#33846=DIRECTION('',(0.,1.,0.));
#33847=DIRECTION('',(0.,0.,-1.));
#33848=DIRECTION('center_axis',(0.,0.,1.));
#33849=DIRECTION('ref_axis',(1.,0.,0.));
#33850=DIRECTION('',(0.,1.,0.));
#33851=DIRECTION('',(1.,0.,0.));
#33852=DIRECTION('center_axis',(-1.,0.,0.));
#33853=DIRECTION('ref_axis',(0.,0.,1.));
#33854=DIRECTION('',(0.,1.,0.));
#33855=DIRECTION('',(0.,0.,1.));
#33856=DIRECTION('center_axis',(0.,0.,-1.));
#33857=DIRECTION('ref_axis',(-1.,0.,0.));
#33858=DIRECTION('',(0.,1.,0.));
#33859=DIRECTION('',(-1.,0.,0.));
#33860=DIRECTION('center_axis',(1.,0.,0.));
#33861=DIRECTION('ref_axis',(0.,0.,-1.));
#33862=DIRECTION('',(0.,0.,-1.));
#33863=DIRECTION('center_axis',(0.,1.,0.));
#33864=DIRECTION('ref_axis',(0.,0.,1.));
#33865=DIRECTION('',(0.,1.,0.));
#33866=DIRECTION('',(0.,1.,0.));
#33867=DIRECTION('',(0.,1.,0.));
#33868=DIRECTION('center_axis',(0.,0.,-1.));
#33869=DIRECTION('ref_axis',(-1.,0.,0.));
#33870=DIRECTION('',(0.,1.,0.));
#33871=DIRECTION('',(-1.,0.,0.));
#33872=DIRECTION('',(0.,1.,0.));
#33873=DIRECTION('',(0.,1.,0.));
#33874=DIRECTION('',(0.,1.,0.));
#33875=DIRECTION('center_axis',(1.,0.,0.));
#33876=DIRECTION('ref_axis',(0.,0.,-1.));
#33877=DIRECTION('',(0.,1.,0.));
#33878=DIRECTION('',(0.,0.,-1.));
#33879=DIRECTION('center_axis',(0.,0.,1.));
#33880=DIRECTION('ref_axis',(1.,0.,0.));
#33881=DIRECTION('',(0.,1.,0.));
#33882=DIRECTION('',(1.,0.,0.));
#33883=DIRECTION('center_axis',(-1.,0.,0.));
#33884=DIRECTION('ref_axis',(0.,0.,1.));
#33885=DIRECTION('',(0.,1.,0.));
#33886=DIRECTION('',(0.,0.,1.));
#33887=DIRECTION('center_axis',(0.,0.,-1.));
#33888=DIRECTION('ref_axis',(-1.,0.,0.));
#33889=DIRECTION('',(0.,1.,0.));
#33890=DIRECTION('',(-1.,0.,0.));
#33891=DIRECTION('center_axis',(0.,-1.,0.));
#33892=DIRECTION('ref_axis',(1.,0.,0.));
#33893=DIRECTION('',(0.,1.,0.));
#33894=DIRECTION('',(0.,1.,0.));
#33895=DIRECTION('',(0.,1.,0.));
#33896=DIRECTION('',(0.,1.,0.));
#33897=DIRECTION('',(0.,1.,0.));
#33898=DIRECTION('',(0.,1.,0.));
#33899=DIRECTION('',(0.,1.,0.));
#33900=DIRECTION('',(0.,1.,0.));
#33901=DIRECTION('',(0.,1.,0.));
#33902=DIRECTION('',(0.,1.,0.));
#33903=DIRECTION('',(0.,1.,0.));
#33904=DIRECTION('',(0.,1.,0.));
#33905=DIRECTION('',(0.,1.,0.));
#33906=DIRECTION('',(0.,1.,0.));
#33907=DIRECTION('center_axis',(0.0750559931030013,0.,-0.997179320834183));
#33908=DIRECTION('ref_axis',(-0.997179320834183,0.,-0.0750559931030013));
#33909=DIRECTION('',(0.,1.,0.));
#33910=DIRECTION('',(-0.997179320834183,0.,-0.0750559931030013));
#33911=DIRECTION('',(0.,1.,0.));
#33912=DIRECTION('',(0.,1.,0.));
#33913=DIRECTION('',(0.,1.,0.));
#33914=DIRECTION('',(0.,1.,0.));
#33915=DIRECTION('',(0.,1.,0.));
#33916=DIRECTION('',(0.,1.,0.));
#33917=DIRECTION('',(0.,1.,0.));
#33918=DIRECTION('',(0.,1.,0.));
#33919=DIRECTION('',(0.,1.,0.));
#33920=DIRECTION('',(0.,1.,0.));
#33921=DIRECTION('',(0.,1.,0.));
#33922=DIRECTION('',(0.,1.,0.));
#33923=DIRECTION('',(0.,1.,0.));
#33924=DIRECTION('',(0.,1.,0.));
#33925=DIRECTION('',(0.,1.,0.));
#33926=DIRECTION('',(0.,1.,0.));
#33927=DIRECTION('',(0.,1.,0.));
#33928=DIRECTION('',(0.,1.,0.));
#33929=DIRECTION('center_axis',(-0.0870991569883124,0.,0.996199647084823));
#33930=DIRECTION('ref_axis',(0.996199647084823,0.,0.0870991569883124));
#33931=DIRECTION('',(0.,1.,0.));
#33932=DIRECTION('',(0.996199647084823,0.,0.0870991569883124));
#33933=DIRECTION('',(0.,1.,0.));
#33934=DIRECTION('center_axis',(0.,-1.,0.));
#33935=DIRECTION('ref_axis',(1.,0.,0.));
#33936=DIRECTION('',(0.,1.,0.));
#33937=DIRECTION('',(0.,1.,0.));
#33938=DIRECTION('',(0.,1.,0.));
#33939=DIRECTION('',(0.,1.,0.));
#33940=DIRECTION('',(0.,1.,0.));
#33941=DIRECTION('',(0.,1.,0.));
#33942=DIRECTION('',(0.,1.,0.));
#33943=DIRECTION('',(0.,1.,0.));
#33944=DIRECTION('',(0.,1.,0.));
#33945=DIRECTION('',(0.,1.,0.));
#33946=DIRECTION('',(0.,1.,0.));
#33947=DIRECTION('',(0.,1.,0.));
#33948=DIRECTION('center_axis',(-0.175033723668955,0.,-0.984562438638901));
#33949=DIRECTION('ref_axis',(-0.984562438638901,0.,0.175033723668955));
#33950=DIRECTION('',(0.,1.,0.));
#33951=DIRECTION('',(-0.984562438638901,0.,0.175033723668955));
#33952=DIRECTION('',(0.,1.,0.));
#33953=DIRECTION('',(0.,1.,0.));
#33954=DIRECTION('',(0.,1.,0.));
#33955=DIRECTION('',(0.,1.,0.));
#33956=DIRECTION('',(0.,1.,0.));
#33957=DIRECTION('',(0.,1.,0.));
#33958=DIRECTION('',(0.,1.,0.));
#33959=DIRECTION('center_axis',(-0.992083449613824,0.,0.125580368698037));
#33960=DIRECTION('ref_axis',(0.125580368698037,0.,0.992083449613824));
#33961=DIRECTION('',(0.,1.,0.));
#33962=DIRECTION('',(0.125580368698037,0.,0.992083449613824));
#33963=DIRECTION('',(0.,1.,0.));
#33964=DIRECTION('',(0.,1.,0.));
#33965=DIRECTION('',(0.,1.,0.));
#33966=DIRECTION('',(0.,1.,0.));
#33967=DIRECTION('',(0.,1.,0.));
#33968=DIRECTION('',(0.,1.,0.));
#33969=DIRECTION('',(0.,1.,0.));
#33970=DIRECTION('center_axis',(-0.132163229797056,0.,0.99122796605504));
#33971=DIRECTION('ref_axis',(0.991227966055039,0.,0.132163229797056));
#33972=DIRECTION('',(0.,1.,0.));
#33973=DIRECTION('',(0.991227966055039,0.,0.132163229797056));
#33974=DIRECTION('',(0.,1.,0.));
#33975=DIRECTION('center_axis',(0.,-1.,0.));
#33976=DIRECTION('ref_axis',(1.,0.,0.));
#33977=DIRECTION('center_axis',(0.,0.,1.));
#33978=DIRECTION('ref_axis',(1.,0.,0.));
#33979=DIRECTION('',(0.,1.,0.));
#33980=DIRECTION('',(1.,0.,0.));
#33981=DIRECTION('',(0.,1.,0.));
#33982=DIRECTION('center_axis',(-1.,0.,0.));
#33983=DIRECTION('ref_axis',(0.,0.,1.));
#33984=DIRECTION('',(0.,1.,0.));
#33985=DIRECTION('',(0.,0.,1.));
#33986=DIRECTION('center_axis',(0.,0.,-1.));
#33987=DIRECTION('ref_axis',(-1.,0.,0.));
#33988=DIRECTION('',(0.,1.,0.));
#33989=DIRECTION('',(-1.,0.,0.));
#33990=DIRECTION('center_axis',(1.,0.,0.));
#33991=DIRECTION('ref_axis',(0.,0.,-1.));
#33992=DIRECTION('',(0.,0.,-1.));
#33993=DIRECTION('center_axis',(0.,1.,0.));
#33994=DIRECTION('ref_axis',(0.,0.,1.));
#33995=DIRECTION('',(0.,1.,0.));
#33996=DIRECTION('',(0.,1.,0.));
#33997=DIRECTION('',(0.,1.,0.));
#33998=DIRECTION('',(0.,1.,0.));
#33999=DIRECTION('',(0.,1.,0.));
#34000=DIRECTION('',(0.,1.,0.));
#34001=DIRECTION('',(0.,1.,0.));
#34002=DIRECTION('',(0.,1.,0.));
#34003=DIRECTION('',(0.,1.,0.));
#34004=DIRECTION('',(0.,1.,0.));
#34005=DIRECTION('',(0.,1.,0.));
#34006=DIRECTION('',(0.,1.,0.));
#34007=DIRECTION('',(0.,1.,0.));
#34008=DIRECTION('',(0.,1.,0.));
#34009=DIRECTION('center_axis',(0.0750559931030013,0.,-0.997179320834183));
#34010=DIRECTION('ref_axis',(-0.997179320834183,0.,-0.0750559931030013));
#34011=DIRECTION('',(0.,1.,0.));
#34012=DIRECTION('',(-0.997179320834183,0.,-0.0750559931030013));
#34013=DIRECTION('',(0.,1.,0.));
#34014=DIRECTION('',(0.,1.,0.));
#34015=DIRECTION('',(0.,1.,0.));
#34016=DIRECTION('',(0.,1.,0.));
#34017=DIRECTION('',(0.,1.,0.));
#34018=DIRECTION('',(0.,1.,0.));
#34019=DIRECTION('',(0.,1.,0.));
#34020=DIRECTION('',(0.,1.,0.));
#34021=DIRECTION('',(0.,1.,0.));
#34022=DIRECTION('',(0.,1.,0.));
#34023=DIRECTION('',(0.,1.,0.));
#34024=DIRECTION('',(0.,1.,0.));
#34025=DIRECTION('',(0.,1.,0.));
#34026=DIRECTION('',(0.,1.,0.));
#34027=DIRECTION('',(0.,1.,0.));
#34028=DIRECTION('',(0.,1.,0.));
#34029=DIRECTION('',(0.,1.,0.));
#34030=DIRECTION('',(0.,1.,0.));
#34031=DIRECTION('center_axis',(-0.0870989735514131,0.,0.996199663122956));
#34032=DIRECTION('ref_axis',(0.996199663122956,0.,0.0870989735514131));
#34033=DIRECTION('',(0.,1.,0.));
#34034=DIRECTION('',(0.996199663122956,0.,0.0870989735514131));
#34035=DIRECTION('',(0.,1.,0.));
#34036=DIRECTION('center_axis',(0.,-1.,0.));
#34037=DIRECTION('ref_axis',(1.,0.,0.));
#34038=DIRECTION('center_axis',(0.,0.,-1.));
#34039=DIRECTION('ref_axis',(1.,0.,0.));
#34040=DIRECTION('',(0.707106781186547,-8.65956056235493E-17,0.707106781186548));
#34041=DIRECTION('center_axis',(0.,0.,1.));
#34042=DIRECTION('ref_axis',(1.,0.,0.));
#34043=DIRECTION('center_axis',(0.,0.,-1.));
#34044=DIRECTION('ref_axis',(1.,0.,0.));
#34045=DIRECTION('center_axis',(0.,0.,1.));
#34046=DIRECTION('ref_axis',(1.,0.,0.));
#34047=DIRECTION('',(0.,0.,-1.));
#34048=DIRECTION('center_axis',(0.,0.,1.));
#34049=DIRECTION('ref_axis',(1.,0.,0.));
#34050=DIRECTION('',(0.707106781186548,8.65956056235493E-17,-0.707106781186548));
#34051=DIRECTION('center_axis',(0.,0.,-1.));
#34052=DIRECTION('ref_axis',(1.,0.,0.));
#34053=DIRECTION('center_axis',(0.,0.,-1.));
#34054=DIRECTION('ref_axis',(1.,0.,0.));
#34055=DIRECTION('',(0.,0.,-1.));
#34056=DIRECTION('center_axis',(0.,0.,-1.));
#34057=DIRECTION('ref_axis',(1.,0.,0.));
#34058=DIRECTION('center_axis',(0.,0.,1.));
#34059=DIRECTION('ref_axis',(1.,0.,0.));
#34060=DIRECTION('',(0.707106781186548,8.65956056235493E-17,-0.707106781186548));
#34061=DIRECTION('center_axis',(0.,0.,-1.));
#34062=DIRECTION('ref_axis',(1.,0.,0.));
#34063=DIRECTION('center_axis',(0.,0.,-1.));
#34064=DIRECTION('ref_axis',(1.,0.,0.));
#34065=DIRECTION('',(0.,0.,-1.));
#34066=DIRECTION('center_axis',(0.,0.,-1.));
#34067=DIRECTION('ref_axis',(1.,0.,0.));
#34068=DIRECTION('center_axis',(0.,0.,1.));
#34069=DIRECTION('ref_axis',(1.,0.,0.));
#34070=DIRECTION('',(0.707106781186548,8.65956056235493E-17,-0.707106781186548));
#34071=DIRECTION('center_axis',(0.,0.,-1.));
#34072=DIRECTION('ref_axis',(1.,0.,0.));
#34073=DIRECTION('center_axis',(0.,0.,-1.));
#34074=DIRECTION('ref_axis',(1.,0.,0.));
#34075=DIRECTION('',(0.,0.,-1.));
#34076=DIRECTION('center_axis',(0.,0.,-1.));
#34077=DIRECTION('ref_axis',(1.,0.,0.));
#34078=DIRECTION('center_axis',(0.,0.,1.));
#34079=DIRECTION('ref_axis',(1.,0.,0.));
#34080=DIRECTION('',(0.70710678118654,8.65956056235484E-17,-0.707106781186555));
#34081=DIRECTION('center_axis',(0.,0.,-1.));
#34082=DIRECTION('ref_axis',(1.,0.,0.));
#34083=DIRECTION('center_axis',(0.,0.,-1.));
#34084=DIRECTION('ref_axis',(1.,0.,0.));
#34085=DIRECTION('',(0.,0.,-1.));
#34086=DIRECTION('center_axis',(0.,0.,-1.));
#34087=DIRECTION('ref_axis',(1.,0.,0.));
#34088=DIRECTION('center_axis',(0.,0.,1.));
#34089=DIRECTION('ref_axis',(1.,0.,0.));
#34090=DIRECTION('',(0.707106781186547,8.65956056235493E-17,-0.707106781186547));
#34091=DIRECTION('center_axis',(0.,0.,-1.));
#34092=DIRECTION('ref_axis',(1.,0.,0.));
#34093=DIRECTION('center_axis',(0.,0.,-1.));
#34094=DIRECTION('ref_axis',(1.,0.,0.));
#34095=DIRECTION('',(0.,0.,-1.));
#34096=DIRECTION('center_axis',(0.,0.,-1.));
#34097=DIRECTION('ref_axis',(1.,0.,0.));
#34098=DIRECTION('center_axis',(0.,0.,1.));
#34099=DIRECTION('ref_axis',(1.,0.,0.));
#34100=DIRECTION('',(0.70710678118654,8.65956056235484E-17,-0.707106781186555));
#34101=DIRECTION('center_axis',(0.,0.,-1.));
#34102=DIRECTION('ref_axis',(1.,0.,0.));
#34103=DIRECTION('center_axis',(0.,0.,-1.));
#34104=DIRECTION('ref_axis',(1.,0.,0.));
#34105=DIRECTION('',(0.,0.,-1.));
#34106=DIRECTION('center_axis',(0.,0.,-1.));
#34107=DIRECTION('ref_axis',(1.,0.,0.));
#34108=DIRECTION('center_axis',(0.,0.,1.));
#34109=DIRECTION('ref_axis',(1.,0.,0.));
#34110=DIRECTION('',(0.707106781186548,8.65956056235493E-17,-0.707106781186548));
#34111=DIRECTION('center_axis',(0.,0.,-1.));
#34112=DIRECTION('ref_axis',(1.,0.,0.));
#34113=DIRECTION('center_axis',(0.,0.,-1.));
#34114=DIRECTION('ref_axis',(1.,0.,0.));
#34115=DIRECTION('',(0.,0.,-1.));
#34116=DIRECTION('center_axis',(0.,0.,-1.));
#34117=DIRECTION('ref_axis',(1.,0.,0.));
#34118=DIRECTION('center_axis',(0.,0.,1.));
#34119=DIRECTION('ref_axis',(1.,0.,0.));
#34120=DIRECTION('',(0.707106781186548,8.65956056235493E-17,-0.707106781186548));
#34121=DIRECTION('center_axis',(0.,0.,-1.));
#34122=DIRECTION('ref_axis',(1.,0.,0.));
#34123=DIRECTION('center_axis',(0.,0.,-1.));
#34124=DIRECTION('ref_axis',(1.,0.,0.));
#34125=DIRECTION('',(0.,0.,-1.));
#34126=DIRECTION('center_axis',(0.,0.,-1.));
#34127=DIRECTION('ref_axis',(1.,0.,0.));
#34128=DIRECTION('center_axis',(0.,0.,1.));
#34129=DIRECTION('ref_axis',(1.,0.,0.));
#34130=DIRECTION('',(0.70710678118654,8.65956056235484E-17,-0.707106781186555));
#34131=DIRECTION('center_axis',(0.,0.,-1.));
#34132=DIRECTION('ref_axis',(1.,0.,0.));
#34133=DIRECTION('center_axis',(0.,0.,-1.));
#34134=DIRECTION('ref_axis',(1.,0.,0.));
#34135=DIRECTION('',(0.,0.,-1.));
#34136=DIRECTION('center_axis',(0.,0.,-1.));
#34137=DIRECTION('ref_axis',(1.,0.,0.));
#34138=DIRECTION('center_axis',(0.,0.,1.));
#34139=DIRECTION('ref_axis',(1.,0.,0.));
#34140=DIRECTION('',(0.707106781186548,8.65956056235493E-17,-0.707106781186548));
#34141=DIRECTION('center_axis',(0.,0.,-1.));
#34142=DIRECTION('ref_axis',(1.,0.,0.));
#34143=DIRECTION('center_axis',(0.,0.,-1.));
#34144=DIRECTION('ref_axis',(1.,0.,0.));
#34145=DIRECTION('',(0.,0.,-1.));
#34146=DIRECTION('center_axis',(0.,0.,-1.));
#34147=DIRECTION('ref_axis',(1.,0.,0.));
#34148=DIRECTION('center_axis',(0.,0.,1.));
#34149=DIRECTION('ref_axis',(1.,0.,0.));
#34150=DIRECTION('',(0.70710678118654,8.65956056235484E-17,-0.707106781186555));
#34151=DIRECTION('center_axis',(0.,0.,-1.));
#34152=DIRECTION('ref_axis',(1.,0.,0.));
#34153=DIRECTION('center_axis',(0.,0.,-1.));
#34154=DIRECTION('ref_axis',(1.,0.,0.));
#34155=DIRECTION('',(0.,0.,-1.));
#34156=DIRECTION('center_axis',(0.,0.,-1.));
#34157=DIRECTION('ref_axis',(1.,0.,0.));
#34158=DIRECTION('center_axis',(0.,0.,1.));
#34159=DIRECTION('ref_axis',(1.,0.,0.));
#34160=DIRECTION('',(0.707106781186548,8.65956056235493E-17,-0.707106781186548));
#34161=DIRECTION('center_axis',(0.,0.,-1.));
#34162=DIRECTION('ref_axis',(1.,0.,0.));
#34163=DIRECTION('center_axis',(0.,0.,-1.));
#34164=DIRECTION('ref_axis',(1.,0.,0.));
#34165=DIRECTION('',(0.,0.,-1.));
#34166=DIRECTION('center_axis',(0.,0.,-1.));
#34167=DIRECTION('ref_axis',(1.,0.,0.));
#34168=DIRECTION('center_axis',(0.,0.,1.));
#34169=DIRECTION('ref_axis',(1.,0.,0.));
#34170=DIRECTION('',(0.707106781186547,8.65956056235493E-17,-0.707106781186547));
#34171=DIRECTION('center_axis',(0.,0.,-1.));
#34172=DIRECTION('ref_axis',(1.,0.,0.));
#34173=DIRECTION('center_axis',(0.,0.,-1.));
#34174=DIRECTION('ref_axis',(1.,0.,0.));
#34175=DIRECTION('',(0.,0.,-1.));
#34176=DIRECTION('center_axis',(0.,0.,1.));
#34177=DIRECTION('ref_axis',(1.,0.,0.));
#34178=DIRECTION('',(0.707106781186548,8.65956056235493E-17,-0.707106781186548));
#34179=DIRECTION('center_axis',(0.,0.,-1.));
#34180=DIRECTION('ref_axis',(1.,0.,0.));
#34181=DIRECTION('center_axis',(0.,0.,-1.));
#34182=DIRECTION('ref_axis',(1.,0.,0.));
#34183=DIRECTION('',(0.,0.,-1.));
#34184=DIRECTION('center_axis',(0.,0.,1.));
#34185=DIRECTION('ref_axis',(1.,0.,0.));
#34186=DIRECTION('',(0.707106781186548,8.65956056235493E-17,-0.707106781186548));
#34187=DIRECTION('center_axis',(0.,0.,-1.));
#34188=DIRECTION('ref_axis',(1.,0.,0.));
#34189=DIRECTION('center_axis',(0.,0.,-1.));
#34190=DIRECTION('ref_axis',(1.,0.,0.));
#34191=DIRECTION('',(0.,0.,-1.));
#34192=DIRECTION('center_axis',(0.,0.,1.));
#34193=DIRECTION('ref_axis',(1.,0.,0.));
#34194=DIRECTION('',(0.707106781186547,8.65956056235493E-17,-0.707106781186547));
#34195=DIRECTION('center_axis',(0.,0.,-1.));
#34196=DIRECTION('ref_axis',(1.,0.,0.));
#34197=DIRECTION('center_axis',(0.,0.,-1.));
#34198=DIRECTION('ref_axis',(1.,0.,0.));
#34199=DIRECTION('',(0.,0.,-1.));
#34200=DIRECTION('center_axis',(0.,0.,-1.));
#34201=DIRECTION('ref_axis',(1.,0.,0.));
#34202=DIRECTION('',(0.707106781186547,-8.65956056235493E-17,0.707106781186548));
#34203=DIRECTION('center_axis',(0.,0.,-1.));
#34204=DIRECTION('ref_axis',(1.,0.,0.));
#34205=DIRECTION('',(0.707106781186548,-8.65956056235493E-17,0.707106781186548));
#34206=DIRECTION('center_axis',(0.,0.,-1.));
#34207=DIRECTION('ref_axis',(1.,0.,0.));
#34208=DIRECTION('',(0.707106781186548,-8.65956056235493E-17,0.707106781186548));
#34209=DIRECTION('center_axis',(0.,0.,-1.));
#34210=DIRECTION('ref_axis',(1.,0.,0.));
#34211=DIRECTION('',(0.707106781186547,-8.65956056235493E-17,0.707106781186548));
#34212=DIRECTION('center_axis',(0.,1.,0.));
#34213=DIRECTION('ref_axis',(1.,0.,0.));
#34214=DIRECTION('center_axis',(0.,1.,0.));
#34215=DIRECTION('ref_axis',(1.,0.,0.));
#34216=DIRECTION('center_axis',(0.,0.,1.));
#34217=DIRECTION('ref_axis',(1.,0.,0.));
#34218=DIRECTION('center_axis',(0.,0.,1.));
#34219=DIRECTION('ref_axis',(1.,0.,0.));
#34220=DIRECTION('center_axis',(0.,0.,1.));
#34221=DIRECTION('ref_axis',(1.,0.,0.));
#34222=DIRECTION('center_axis',(0.,0.,1.));
#34223=DIRECTION('ref_axis',(1.,0.,0.));
#34224=DIRECTION('center_axis',(0.,0.,1.));
#34225=DIRECTION('ref_axis',(1.,0.,0.));
#34226=DIRECTION('center_axis',(0.,0.,1.));
#34227=DIRECTION('ref_axis',(1.,0.,0.));
#34228=DIRECTION('center_axis',(0.,0.,1.));
#34229=DIRECTION('ref_axis',(1.,0.,0.));
#34230=DIRECTION('center_axis',(0.,0.,1.));
#34231=DIRECTION('ref_axis',(1.,0.,0.));
#34232=DIRECTION('center_axis',(0.,0.,1.));
#34233=DIRECTION('ref_axis',(1.,0.,0.));
#34234=DIRECTION('center_axis',(0.,0.,1.));
#34235=DIRECTION('ref_axis',(1.,0.,0.));
#34236=DIRECTION('center_axis',(0.,0.,1.));
#34237=DIRECTION('ref_axis',(1.,0.,0.));
#34238=DIRECTION('center_axis',(0.,0.,1.));
#34239=DIRECTION('ref_axis',(1.,0.,0.));
#34240=DIRECTION('center_axis',(0.,0.,-1.));
#34241=DIRECTION('ref_axis',(1.,0.,0.));
#34242=DIRECTION('',(0.,0.,-1.));
#34243=DIRECTION('center_axis',(0.,0.,-1.));
#34244=DIRECTION('ref_axis',(1.,0.,0.));
#34245=DIRECTION('center_axis',(0.,0.,1.));
#34246=DIRECTION('ref_axis',(1.,0.,0.));
#34247=DIRECTION('center_axis',(0.,1.,0.));
#34248=DIRECTION('ref_axis',(-1.,0.,0.));
#34249=DIRECTION('axis',(0.,0.,1.));
#34250=DIRECTION('refdir',(1.,0.,0.));
#34251=DIRECTION('center_axis',(0.,0.,1.));
#34252=DIRECTION('ref_axis',(1.,0.,0.));
#34253=DIRECTION('center_axis',(0.,0.,1.));
#34254=DIRECTION('ref_axis',(1.,0.,0.));
#34255=DIRECTION('',(0.707106781186547,8.65956056235493E-17,-0.707106781186547));
#34256=DIRECTION('center_axis',(0.,0.,-1.));
#34257=DIRECTION('ref_axis',(1.,0.,0.));
#34258=DIRECTION('center_axis',(0.,0.,1.));
#34259=DIRECTION('ref_axis',(1.,0.,0.));
#34260=DIRECTION('',(0.,-1.,0.));
#34261=DIRECTION('',(-1.,0.,0.));
#34262=DIRECTION('center_axis',(0.,0.,-1.));
#34263=DIRECTION('ref_axis',(0.707106781186545,-0.70710678118655,0.));
#34264=DIRECTION('',(0.,-1.,0.));
#34265=DIRECTION('center_axis',(0.,0.,1.));
#34266=DIRECTION('ref_axis',(-0.70710678118655,0.707106781186545,0.));
#34267=DIRECTION('',(-1.,0.,0.));
#34268=DIRECTION('center_axis',(0.,0.,1.));
#34269=DIRECTION('ref_axis',(1.,0.,0.));
#34270=DIRECTION('',(-1.,0.,0.));
#34271=DIRECTION('center_axis',(0.,0.,1.));
#34272=DIRECTION('ref_axis',(0.707106781186547,0.707106781186547,0.));
#34273=DIRECTION('',(0.,1.,0.));
#34274=DIRECTION('center_axis',(0.,0.,-1.));
#34275=DIRECTION('ref_axis',(-0.70710678118655,-0.707106781186545,0.));
#34276=DIRECTION('',(-1.,0.,0.));
#34277=DIRECTION('center_axis',(0.,0.,-1.));
#34278=DIRECTION('ref_axis',(0.707106781186545,-0.70710678118655,0.));
#34279=DIRECTION('',(0.,-1.,0.));
#34280=DIRECTION('center_axis',(0.,0.,-1.));
#34281=DIRECTION('ref_axis',(0.707106781186548,0.707106781186548,0.));
#34282=DIRECTION('',(1.,0.,0.));
#34283=DIRECTION('center_axis',(0.,0.,-1.));
#34284=DIRECTION('ref_axis',(-0.707106781186548,0.707106781186548,0.));
#34285=DIRECTION('',(0.,1.,0.));
#34286=DIRECTION('center_axis',(0.,0.,1.));
#34287=DIRECTION('ref_axis',(0.707106781186547,-0.707106781186547,0.));
#34288=DIRECTION('',(1.,0.,0.));
#34289=DIRECTION('center_axis',(0.,0.,-1.));
#34290=DIRECTION('ref_axis',(-0.707106781186548,0.707106781186548,0.));
#34291=DIRECTION('',(0.,1.,0.));
#34292=DIRECTION('center_axis',(0.,0.,-1.));
#34293=DIRECTION('ref_axis',(-0.707106781186548,-0.707106781186548,0.));
#34294=DIRECTION('',(-1.,0.,0.));
#34295=DIRECTION('center_axis',(0.,0.,-1.));
#34296=DIRECTION('ref_axis',(0.707106781186545,-0.70710678118655,0.));
#34297=DIRECTION('center_axis',(0.,0.,1.));
#34298=DIRECTION('ref_axis',(1.,0.,0.));
#34299=DIRECTION('center_axis',(0.,0.,1.));
#34300=DIRECTION('ref_axis',(1.,0.,0.));
#34301=DIRECTION('center_axis',(0.,0.,1.));
#34302=DIRECTION('ref_axis',(1.,0.,0.));
#34303=DIRECTION('center_axis',(0.,0.,-1.));
#34304=DIRECTION('ref_axis',(1.,0.,0.));
#34305=DIRECTION('center_axis',(0.,0.,-1.));
#34306=DIRECTION('ref_axis',(1.,0.,0.));
#34307=DIRECTION('center_axis',(0.,0.,-1.));
#34308=DIRECTION('ref_axis',(1.,0.,0.));
#34309=DIRECTION('center_axis',(0.,0.,-1.));
#34310=DIRECTION('ref_axis',(1.,0.,0.));
#34311=DIRECTION('center_axis',(0.,0.,1.));
#34312=DIRECTION('ref_axis',(1.,0.,0.));
#34313=DIRECTION('center_axis',(0.,0.,1.));
#34314=DIRECTION('ref_axis',(1.,0.,0.));
#34315=DIRECTION('center_axis',(0.,0.,-1.));
#34316=DIRECTION('ref_axis',(1.,0.,0.));
#34317=DIRECTION('',(0.,0.,-1.));
#34318=DIRECTION('center_axis',(0.,0.,-1.));
#34319=DIRECTION('ref_axis',(1.,0.,0.));
#34320=DIRECTION('center_axis',(0.,0.,1.));
#34321=DIRECTION('ref_axis',(1.,0.,0.));
#34322=DIRECTION('',(0.707106781186549,8.65956056235495E-17,-0.707106781186546));
#34323=DIRECTION('center_axis',(0.,0.,-1.));
#34324=DIRECTION('ref_axis',(1.,0.,0.));
#34325=DIRECTION('center_axis',(0.,0.,-1.));
#34326=DIRECTION('ref_axis',(1.,0.,0.));
#34327=DIRECTION('',(0.,0.,-1.));
#34328=DIRECTION('center_axis',(0.,0.,-1.));
#34329=DIRECTION('ref_axis',(1.,0.,0.));
#34330=DIRECTION('center_axis',(0.,-0.707106781186548,0.707106781186548));
#34331=DIRECTION('ref_axis',(1.,0.,0.));
#34332=DIRECTION('',(-0.577350269189626,0.577350269189626,0.577350269189626));
#34333=DIRECTION('',(1.,0.,0.));
#34334=DIRECTION('',(0.,0.707106781186548,0.707106781186548));
#34335=DIRECTION('center_axis',(0.,0.,-1.));
#34336=DIRECTION('ref_axis',(0.707106781186545,-0.70710678118655,0.));
#34337=DIRECTION('center_axis',(0.,0.,1.));
#34338=DIRECTION('ref_axis',(0.707106781186545,-0.70710678118655,0.));
#34339=DIRECTION('',(-0.707106781186548,0.,0.707106781186548));
#34340=DIRECTION('center_axis',(0.707106781186548,0.,0.707106781186548));
#34341=DIRECTION('ref_axis',(0.707106781186548,0.,-0.707106781186548));
#34342=DIRECTION('',(-0.707106781186548,0.,0.707106781186548));
#34343=DIRECTION('',(0.,1.,0.));
#34344=DIRECTION('center_axis',(0.,0.,1.));
#34345=DIRECTION('ref_axis',(-0.70710678118655,0.707106781186545,0.));
#34346=DIRECTION('center_axis',(0.,0.,-1.));
#34347=DIRECTION('ref_axis',(-0.70710678118655,0.707106781186545,0.));
#34348=DIRECTION('',(0.,0.707106781186551,0.707106781186544));
#34349=DIRECTION('center_axis',(0.,-0.707106781186548,0.707106781186548));
#34350=DIRECTION('ref_axis',(1.,0.,0.));
#34351=DIRECTION('',(1.,0.,0.));
#34352=DIRECTION('',(0.504717559062642,0.610434347646759,0.610434347646759));
#34353=DIRECTION('center_axis',(0.,0.,1.));
#34354=DIRECTION('ref_axis',(-5.1924747385868E-12,1.,0.));
#34355=DIRECTION('center_axis',(0.,0.,-1.));
#34356=DIRECTION('ref_axis',(1.,0.,0.));
#34357=DIRECTION('center_axis',(0.770685380459105,-0.637215853809841,0.));
#34358=DIRECTION('ref_axis',(0.,0.,-1.));
#34359=DIRECTION('',(0.,0.,-1.));
#34360=DIRECTION('',(0.637215853809841,0.770685380459105,6.96921156614208E-15));
#34361=DIRECTION('',(0.,0.,1.));
#34362=DIRECTION('center_axis',(0.603317169232353,-0.498832954222525,-0.622233137249286));
#34363=DIRECTION('ref_axis',(-0.717935231561239,0.,-0.696109907473748));
#34364=DIRECTION('',(0.143139597747746,-0.699825355198214,0.699825355198214));
#34365=DIRECTION('center_axis',(0.,-0.707106781186548,-0.707106781186548));
#34366=DIRECTION('ref_axis',(-1.,0.,0.));
#34367=DIRECTION('',(0.,-0.707106781186548,0.707106781186548));
#34368=DIRECTION('',(1.,0.,0.));
#34369=DIRECTION('',(0.,-0.707106781186548,0.707106781186548));
#34370=DIRECTION('',(-1.,0.,0.));
#34371=DIRECTION('center_axis',(0.,0.,1.));
#34372=DIRECTION('ref_axis',(0.707106781186545,-0.70710678118655,0.));
#34373=DIRECTION('',(0.707106781186548,0.,0.707106781186548));
#34374=DIRECTION('center_axis',(0.,0.,-1.));
#34375=DIRECTION('ref_axis',(0.707106781186545,-0.70710678118655,0.));
#34376=DIRECTION('center_axis',(0.,0.,1.));
#34377=DIRECTION('ref_axis',(0.707106781186545,-0.70710678118655,0.));
#34378=DIRECTION('center_axis',(0.707106781186548,0.,-0.707106781186548));
#34379=DIRECTION('ref_axis',(-0.707106781186548,0.,-0.707106781186548));
#34380=DIRECTION('',(0.707106781186548,0.,0.707106781186548));
#34381=DIRECTION('',(0.,-1.,0.));
#34382=DIRECTION('',(0.,1.,0.));
#34383=DIRECTION('center_axis',(0.,0.,-1.));
#34384=DIRECTION('ref_axis',(-0.70710678118655,0.707106781186545,0.));
#34385=DIRECTION('',(0.,-0.707106781186551,0.707106781186544));
#34386=DIRECTION('center_axis',(0.,0.,1.));
#34387=DIRECTION('ref_axis',(-0.70710678118655,0.707106781186545,0.));
#34388=DIRECTION('center_axis',(0.,0.,-1.));
#34389=DIRECTION('ref_axis',(-0.70710678118655,0.707106781186545,0.));
#34390=DIRECTION('center_axis',(0.,-0.707106781186548,-0.707106781186548));
#34391=DIRECTION('ref_axis',(-1.,0.,0.));
#34392=DIRECTION('',(1.,0.,0.));
#34393=DIRECTION('',(-1.,0.,0.));
#34394=DIRECTION('center_axis',(0.,0.,-1.));
#34395=DIRECTION('ref_axis',(0.00854146177382261,0.999963521050026,0.));
#34396=DIRECTION('center_axis',(0.,0.,1.));
#34397=DIRECTION('ref_axis',(-1.,0.,0.));
#34398=DIRECTION('center_axis',(0.,0.,-1.));
#34399=DIRECTION('ref_axis',(-1.,0.,0.));
#34400=DIRECTION('center_axis',(1.,0.,0.));
#34401=DIRECTION('ref_axis',(0.,1.,0.));
#34402=DIRECTION('',(0.,0.,1.));
#34403=DIRECTION('',(0.,0.,-1.));
#34404=DIRECTION('center_axis',(0.,0.,1.));
#34405=DIRECTION('ref_axis',(-0.70710678118655,0.707106781186545,0.));
#34406=DIRECTION('',(0.,0.,1.));
#34407=DIRECTION('center_axis',(0.,-1.,0.));
#34408=DIRECTION('ref_axis',(1.,0.,0.));
#34409=DIRECTION('center_axis',(0.,0.,-1.));
#34410=DIRECTION('ref_axis',(-1.83697019872103E-16,1.,0.));
#34411=DIRECTION('',(0.,0.,-1.));
#34412=DIRECTION('center_axis',(-0.770685380459105,-0.637215853809841,0.));
#34413=DIRECTION('ref_axis',(0.,0.,1.));
#34414=DIRECTION('',(-0.504717559062642,0.610434347646759,-0.610434347646759));
#34415=DIRECTION('',(0.,0.,1.));
#34416=DIRECTION('',(-0.504717559062642,0.610434347646759,0.610434347646759));
#34417=DIRECTION('center_axis',(0.,-0.707106781186548,-0.707106781186548));
#34418=DIRECTION('ref_axis',(-1.,0.,0.));
#34419=DIRECTION('',(1.,0.,0.));
#34420=DIRECTION('',(0.,-0.707106781186548,0.707106781186548));
#34421=DIRECTION('',(-1.,0.,0.));
#34422=DIRECTION('center_axis',(0.,0.,-1.));
#34423=DIRECTION('ref_axis',(1.,0.,0.));
#34424=DIRECTION('center_axis',(0.,0.,-1.));
#34425=DIRECTION('ref_axis',(1.,0.,0.));
#34426=DIRECTION('',(0.707106781186549,-8.65956056235495E-17,0.707106781186546));
#34427=DIRECTION('center_axis',(0.,0.,1.));
#34428=DIRECTION('ref_axis',(1.,0.,0.));
#34429=DIRECTION('center_axis',(0.,0.,1.));
#34430=DIRECTION('ref_axis',(1.,0.,0.));
#34431=DIRECTION('',(0.,1.,0.));
#34432=DIRECTION('center_axis',(0.,0.,1.));
#34433=DIRECTION('ref_axis',(0.70710678118655,0.707106781186545,0.));
#34434=DIRECTION('',(-1.,0.,0.));
#34435=DIRECTION('center_axis',(0.,0.,-1.));
#34436=DIRECTION('ref_axis',(0.707106781186547,-0.707106781186547,0.));
#34437=DIRECTION('',(0.,-1.,0.));
#34438=DIRECTION('center_axis',(0.,0.,1.));
#34439=DIRECTION('ref_axis',(-0.707106781186548,0.707106781186548,0.));
#34440=DIRECTION('',(-1.,0.,0.));
#34441=DIRECTION('center_axis',(0.,0.,1.));
#34442=DIRECTION('ref_axis',(0.707106781186548,0.707106781186548,0.));
#34443=DIRECTION('',(0.,1.,0.));
#34444=DIRECTION('center_axis',(0.,0.,1.));
#34445=DIRECTION('ref_axis',(0.707106781186545,-0.70710678118655,0.));
#34446=DIRECTION('',(1.,0.,0.));
#34447=DIRECTION('center_axis',(0.,0.,1.));
#34448=DIRECTION('ref_axis',(-0.70710678118655,-0.707106781186545,0.));
#34449=DIRECTION('',(0.,-1.,0.));
#34450=DIRECTION('center_axis',(0.,0.,-1.));
#34451=DIRECTION('ref_axis',(0.707106781186547,0.707106781186547,0.));
#34452=DIRECTION('center_axis',(0.,0.,-1.));
#34453=DIRECTION('ref_axis',(1.,0.,0.));
#34454=DIRECTION('center_axis',(0.,0.,1.));
#34455=DIRECTION('ref_axis',(1.,0.,0.));
#34456=DIRECTION('center_axis',(0.,0.,-1.));
#34457=DIRECTION('ref_axis',(1.,0.,0.));
#34458=DIRECTION('center_axis',(0.,0.,-1.));
#34459=DIRECTION('ref_axis',(1.,0.,0.));
#34460=DIRECTION('center_axis',(0.,0.,-1.));
#34461=DIRECTION('ref_axis',(1.,0.,0.));
#34462=DIRECTION('',(0.,0.,-1.));
#34463=DIRECTION('center_axis',(0.,0.,-1.));
#34464=DIRECTION('ref_axis',(1.,0.,0.));
#34465=DIRECTION('',(0.707106781186548,-8.65956056235493E-17,0.707106781186548));
#34466=DIRECTION('center_axis',(0.,0.,1.));
#34467=DIRECTION('ref_axis',(1.,0.,0.));
#34468=DIRECTION('center_axis',(0.,0.,-1.));
#34469=DIRECTION('ref_axis',(1.,0.,0.));
#34470=DIRECTION('center_axis',(0.,0.,-1.));
#34471=DIRECTION('ref_axis',(1.,0.,0.));
#34472=DIRECTION('',(0.,0.,-1.));
#34473=DIRECTION('center_axis',(0.,0.,-1.));
#34474=DIRECTION('ref_axis',(1.,0.,0.));
#34475=DIRECTION('',(0.707106781186548,-8.65956056235493E-17,0.707106781186548));
#34476=DIRECTION('center_axis',(0.,0.,1.));
#34477=DIRECTION('ref_axis',(1.,0.,0.));
#34478=DIRECTION('center_axis',(0.,0.,-1.));
#34479=DIRECTION('ref_axis',(1.,0.,0.));
#34480=DIRECTION('center_axis',(0.,0.,-1.));
#34481=DIRECTION('ref_axis',(1.,0.,0.));
#34482=DIRECTION('',(0.,0.,-1.));
#34483=DIRECTION('center_axis',(0.,0.,-1.));
#34484=DIRECTION('ref_axis',(0.707106781186548,0.707106781186548,0.));
#34485=DIRECTION('',(-0.707106781186548,0.,0.707106781186548));
#34486=DIRECTION('center_axis',(0.,0.,1.));
#34487=DIRECTION('ref_axis',(0.707106781186548,0.707106781186548,0.));
#34488=DIRECTION('center_axis',(-0.707106781186548,0.,-0.707106781186548));
#34489=DIRECTION('ref_axis',(-0.707106781186548,0.,0.707106781186548));
#34490=DIRECTION('',(-0.707106781186548,0.,0.707106781186548));
#34491=DIRECTION('',(0.,1.,0.));
#34492=DIRECTION('center_axis',(0.,0.,1.));
#34493=DIRECTION('ref_axis',(-0.70710678118655,-0.707106781186545,0.));
#34494=DIRECTION('',(0.,-0.707106781186548,0.707106781186548));
#34495=DIRECTION('center_axis',(0.,0.,-1.));
#34496=DIRECTION('ref_axis',(-0.70710678118655,-0.707106781186545,0.));
#34497=DIRECTION('center_axis',(0.,-0.707106781186548,-0.707106781186548));
#34498=DIRECTION('ref_axis',(-1.,0.,0.));
#34499=DIRECTION('',(1.25607396694702E-14,-0.707106781186548,0.707106781186548));
#34500=DIRECTION('',(-1.,0.,0.));
#34501=DIRECTION('center_axis',(0.,0.,1.));
#34502=DIRECTION('ref_axis',(0.707106781186545,-0.70710678118655,0.));
#34503=DIRECTION('',(0.707106781186548,0.,0.707106781186548));
#34504=DIRECTION('center_axis',(0.,0.,-1.));
#34505=DIRECTION('ref_axis',(0.707106781186545,-0.70710678118655,0.));
#34506=DIRECTION('center_axis',(0.707106781186548,0.,-0.707106781186548));
#34507=DIRECTION('ref_axis',(-0.707106781186548,0.,-0.707106781186548));
#34508=DIRECTION('',(0.707106781186548,0.,0.707106781186548));
#34509=DIRECTION('',(0.,-1.,0.));
#34510=DIRECTION('center_axis',(0.,0.,1.));
#34511=DIRECTION('ref_axis',(0.707106781186547,0.707106781186547,0.));
#34512=DIRECTION('',(0.,0.707106781186554,0.707106781186541));
#34513=DIRECTION('center_axis',(0.,0.,-1.));
#34514=DIRECTION('ref_axis',(0.707106781186548,0.707106781186548,0.));
#34515=DIRECTION('center_axis',(0.,0.707106781186548,-0.707106781186548));
#34516=DIRECTION('ref_axis',(-1.,0.,0.));
#34517=DIRECTION('',(0.,0.707106781186548,0.707106781186548));
#34518=DIRECTION('',(1.,0.,0.));
#34519=DIRECTION('center_axis',(0.,0.,1.));
#34520=DIRECTION('ref_axis',(-0.707106781186547,0.707106781186547,0.));
#34521=DIRECTION('',(-0.707106781186554,0.,0.707106781186541));
#34522=DIRECTION('center_axis',(0.,0.,-1.));
#34523=DIRECTION('ref_axis',(-0.707106781186548,0.707106781186548,0.));
#34524=DIRECTION('center_axis',(-0.707106781186548,0.,-0.707106781186548));
#34525=DIRECTION('ref_axis',(-0.707106781186548,0.,0.707106781186548));
#34526=DIRECTION('',(-0.707106781186548,0.,0.707106781186548));
#34527=DIRECTION('',(0.,1.,0.));
#34528=DIRECTION('center_axis',(0.,0.,-1.));
#34529=DIRECTION('ref_axis',(0.707106781186548,-0.707106781186548,0.));
#34530=DIRECTION('center_axis',(0.,0.,1.));
#34531=DIRECTION('ref_axis',(0.707106781186548,-0.707106781186548,0.));
#34532=DIRECTION('center_axis',(0.,-0.707106781186548,0.707106781186548));
#34533=DIRECTION('ref_axis',(1.,0.,0.));
#34534=DIRECTION('',(1.,0.,0.));
#34535=DIRECTION('',(0.,0.707106781186548,0.707106781186548));
#34536=DIRECTION('center_axis',(0.707106781186543,0.,-0.707106781186552));
#34537=DIRECTION('ref_axis',(-0.707106781186552,0.,-0.707106781186543));
#34538=DIRECTION('',(0.707106781186552,0.,0.707106781186543));
#34539=DIRECTION('',(0.,-1.,0.));
#34540=DIRECTION('',(-0.707106781186552,0.,-0.707106781186543));
#34541=DIRECTION('',(0.,1.,0.));
#34542=DIRECTION('center_axis',(0.,0.,1.));
#34543=DIRECTION('ref_axis',(0.70710678118655,0.707106781186545,0.));
#34544=DIRECTION('',(0.,0.707106781186547,0.707106781186548));
#34545=DIRECTION('center_axis',(0.,0.,-1.));
#34546=DIRECTION('ref_axis',(0.70710678118655,0.707106781186545,0.));
#34547=DIRECTION('center_axis',(0.,0.,1.));
#34548=DIRECTION('ref_axis',(0.70710678118655,0.707106781186545,0.));
#34549=DIRECTION('center_axis',(0.,0.707106781186549,-0.707106781186546));
#34550=DIRECTION('ref_axis',(-1.,0.,0.));
#34551=DIRECTION('',(0.,0.707106781186546,0.707106781186549));
#34552=DIRECTION('',(1.,0.,0.));
#34553=DIRECTION('',(-1.,0.,0.));
#34554=DIRECTION('center_axis',(0.,0.,1.));
#34555=DIRECTION('ref_axis',(-0.707106781186547,0.707106781186547,0.));
#34556=DIRECTION('',(-0.707106781186552,0.,0.707106781186543));
#34557=DIRECTION('center_axis',(0.,0.,-1.));
#34558=DIRECTION('ref_axis',(-0.707106781186548,0.707106781186548,0.));
#34559=DIRECTION('center_axis',(0.,0.,1.));
#34560=DIRECTION('ref_axis',(-0.707106781186548,0.707106781186548,0.));
#34561=DIRECTION('center_axis',(-0.707106781186543,0.,-0.707106781186552));
#34562=DIRECTION('ref_axis',(-0.707106781186552,0.,0.707106781186543));
#34563=DIRECTION('',(-0.707106781186552,0.,0.707106781186543));
#34564=DIRECTION('',(0.,1.,0.));
#34565=DIRECTION('',(0.,-1.,0.));
#34566=DIRECTION('center_axis',(0.,0.,1.));
#34567=DIRECTION('ref_axis',(-0.707106781186547,-0.707106781186547,0.));
#34568=DIRECTION('',(0.,-0.707106781186552,0.707106781186543));
#34569=DIRECTION('center_axis',(0.,0.,-1.));
#34570=DIRECTION('ref_axis',(-0.707106781186548,-0.707106781186548,0.));
#34571=DIRECTION('center_axis',(0.,0.,1.));
#34572=DIRECTION('ref_axis',(-0.707106781186548,-0.707106781186548,0.));
#34573=DIRECTION('center_axis',(0.,-0.707106781186543,-0.707106781186552));
#34574=DIRECTION('ref_axis',(-1.,0.,0.));
#34575=DIRECTION('',(0.,-0.707106781186552,0.707106781186543));
#34576=DIRECTION('',(-1.,0.,0.));
#34577=DIRECTION('',(1.,0.,0.));
#34578=DIRECTION('center_axis',(0.,0.,1.));
#34579=DIRECTION('ref_axis',(0.707106781186545,-0.70710678118655,0.));
#34580=DIRECTION('center_axis',(0.,0.,-1.));
#34581=DIRECTION('ref_axis',(0.707106781186545,-0.70710678118655,0.));
#34582=DIRECTION('center_axis',(0.,0.,1.));
#34583=DIRECTION('ref_axis',(0.707106781186545,-0.70710678118655,0.));
#34584=DIRECTION('center_axis',(0.,0.,1.));
#34585=DIRECTION('ref_axis',(-0.707106781186548,-0.707106781186548,0.));
#34586=DIRECTION('',(0.,0.,1.));
#34587=DIRECTION('center_axis',(0.,0.,1.));
#34588=DIRECTION('ref_axis',(-0.707106781186548,-0.707106781186548,0.));
#34589=DIRECTION('',(0.,0.,-1.));
#34590=DIRECTION('center_axis',(0.,-1.,0.));
#34591=DIRECTION('ref_axis',(1.,0.,0.));
#34592=DIRECTION('',(0.,0.,-1.));
#34593=DIRECTION('',(1.,0.,0.));
#34594=DIRECTION('center_axis',(0.,0.,1.));
#34595=DIRECTION('ref_axis',(0.707106781186545,-0.70710678118655,0.));
#34596=DIRECTION('',(0.,0.,1.));
#34597=DIRECTION('',(0.,0.,1.));
#34598=DIRECTION('center_axis',(0.,0.,1.));
#34599=DIRECTION('ref_axis',(0.707106781186545,-0.70710678118655,0.));
#34600=DIRECTION('center_axis',(1.,0.,0.));
#34601=DIRECTION('ref_axis',(0.,1.,0.));
#34602=DIRECTION('',(0.,0.,-1.));
#34603=DIRECTION('',(0.,0.,1.));
#34604=DIRECTION('',(0.,1.,0.));
#34605=DIRECTION('center_axis',(-1.,0.,0.));
#34606=DIRECTION('ref_axis',(0.,0.,-1.));
#34607=DIRECTION('center_axis',(-1.,0.,0.));
#34608=DIRECTION('ref_axis',(0.,0.,-1.));
#34609=DIRECTION('center_axis',(-1.,0.,0.));
#34610=DIRECTION('ref_axis',(0.,0.,-1.));
#34611=DIRECTION('center_axis',(0.,0.,1.));
#34612=DIRECTION('ref_axis',(1.,0.,0.));
#34613=DIRECTION('center_axis',(0.,0.,1.));
#34614=DIRECTION('ref_axis',(0.707106781186548,0.707106781186548,0.));
#34615=DIRECTION('center_axis',(0.,0.,-1.));
#34616=DIRECTION('ref_axis',(0.707106781186548,0.707106781186548,0.));
#34617=DIRECTION('',(0.707106781186548,0.,0.707106781186548));
#34618=DIRECTION('center_axis',(-0.707106781186548,0.,0.707106781186548));
#34619=DIRECTION('ref_axis',(0.707106781186548,0.,0.707106781186548));
#34620=DIRECTION('',(0.707106781186548,0.,0.707106781186548));
#34621=DIRECTION('',(0.,-1.,0.));
#34622=DIRECTION('center_axis',(0.,0.,-1.));
#34623=DIRECTION('ref_axis',(-0.70710678118655,-0.707106781186545,0.));
#34624=DIRECTION('center_axis',(0.,0.,1.));
#34625=DIRECTION('ref_axis',(-0.70710678118655,-0.707106781186545,0.));
#34626=DIRECTION('',(0.,0.707106781186548,0.707106781186548));
#34627=DIRECTION('center_axis',(0.,-0.707106781186548,0.707106781186548));
#34628=DIRECTION('ref_axis',(1.,0.,0.));
#34629=DIRECTION('',(-1.25607396694702E-14,0.707106781186548,0.707106781186548));
#34630=DIRECTION('',(1.,0.,0.));
#34631=DIRECTION('center_axis',(0.,0.,-1.));
#34632=DIRECTION('ref_axis',(0.707106781186545,-0.70710678118655,0.));
#34633=DIRECTION('center_axis',(0.,0.,1.));
#34634=DIRECTION('ref_axis',(0.707106781186545,-0.70710678118655,0.));
#34635=DIRECTION('',(-0.707106781186548,0.,0.707106781186548));
#34636=DIRECTION('center_axis',(0.707106781186548,0.,0.707106781186548));
#34637=DIRECTION('ref_axis',(0.707106781186548,0.,-0.707106781186548));
#34638=DIRECTION('',(-0.707106781186548,0.,0.707106781186548));
#34639=DIRECTION('',(0.,1.,0.));
#34640=DIRECTION('center_axis',(0.,0.,-1.));
#34641=DIRECTION('ref_axis',(0.707106781186547,0.707106781186547,0.));
#34642=DIRECTION('center_axis',(0.,0.,1.));
#34643=DIRECTION('ref_axis',(0.707106781186548,0.707106781186548,0.));
#34644=DIRECTION('',(0.,-0.707106781186554,0.707106781186541));
#34645=DIRECTION('center_axis',(0.,0.707106781186548,0.707106781186548));
#34646=DIRECTION('ref_axis',(1.,0.,0.));
#34647=DIRECTION('',(0.,-0.707106781186548,0.707106781186548));
#34648=DIRECTION('',(-1.,0.,0.));
#34649=DIRECTION('center_axis',(0.,0.,-1.));
#34650=DIRECTION('ref_axis',(-0.707106781186547,0.707106781186547,0.));
#34651=DIRECTION('center_axis',(0.,0.,1.));
#34652=DIRECTION('ref_axis',(-0.707106781186548,0.707106781186548,0.));
#34653=DIRECTION('',(0.707106781186554,0.,0.707106781186541));
#34654=DIRECTION('center_axis',(-0.707106781186548,0.,0.707106781186548));
#34655=DIRECTION('ref_axis',(0.707106781186548,0.,0.707106781186548));
#34656=DIRECTION('',(0.707106781186548,0.,0.707106781186548));
#34657=DIRECTION('',(0.,-1.,0.));
#34658=DIRECTION('center_axis',(0.,0.,1.));
#34659=DIRECTION('ref_axis',(0.707106781186548,-0.707106781186548,0.));
#34660=DIRECTION('center_axis',(0.,0.,-1.));
#34661=DIRECTION('ref_axis',(0.707106781186548,-0.707106781186548,0.));
#34662=DIRECTION('',(0.,-0.707106781186554,0.707106781186541));
#34663=DIRECTION('center_axis',(0.,0.707106781186548,0.707106781186548));
#34664=DIRECTION('ref_axis',(1.,0.,0.));
#34665=DIRECTION('',(0.,-0.707106781186548,0.707106781186548));
#34666=DIRECTION('',(-1.,0.,0.));
#34667=DIRECTION('center_axis',(0.,0.,-1.));
#34668=DIRECTION('ref_axis',(-0.707106781186547,0.707106781186547,0.));
#34669=DIRECTION('center_axis',(0.,0.,1.));
#34670=DIRECTION('ref_axis',(-0.707106781186548,0.707106781186548,0.));
#34671=DIRECTION('',(0.707106781186554,0.,0.707106781186541));
#34672=DIRECTION('center_axis',(-0.707106781186541,0.,0.707106781186554));
#34673=DIRECTION('ref_axis',(0.707106781186554,0.,0.707106781186541));
#34674=DIRECTION('',(0.707106781186554,0.,0.707106781186541));
#34675=DIRECTION('',(0.,-1.,0.));
#34676=DIRECTION('center_axis',(0.,0.,-1.));
#34677=DIRECTION('ref_axis',(-0.707106781186547,-0.707106781186547,0.));
#34678=DIRECTION('',(0.,0.707106781186554,0.707106781186541));
#34679=DIRECTION('center_axis',(0.,-0.707106781186541,0.707106781186554));
#34680=DIRECTION('ref_axis',(1.,0.,0.));
#34681=DIRECTION('',(0.,0.707106781186554,0.707106781186541));
#34682=DIRECTION('center_axis',(0.,0.,-1.));
#34683=DIRECTION('ref_axis',(0.707106781186545,-0.70710678118655,0.));
#34684=DIRECTION('',(-0.707106781186541,0.,0.707106781186554));
#34685=DIRECTION('center_axis',(0.707106781186548,0.,0.707106781186548));
#34686=DIRECTION('ref_axis',(0.707106781186548,0.,-0.707106781186548));
#34687=DIRECTION('center_axis',(-1.,0.,0.));
#34688=DIRECTION('ref_axis',(0.,-1.,0.));
#34689=DIRECTION('',(0.,0.,1.));
#34690=DIRECTION('center_axis',(0.,0.,1.));
#34691=DIRECTION('ref_axis',(-0.707106781186548,0.707106781186548,0.));
#34692=DIRECTION('',(0.,0.,-1.));
#34693=DIRECTION('center_axis',(0.,1.,0.));
#34694=DIRECTION('ref_axis',(-1.,0.,0.));
#34695=DIRECTION('',(0.,0.,1.));
#34696=DIRECTION('',(0.,0.,1.));
#34697=DIRECTION('center_axis',(0.,0.,1.));
#34698=DIRECTION('ref_axis',(0.707106781186548,-0.707106781186548,0.));
#34699=DIRECTION('',(0.,0.,-1.));
#34700=DIRECTION('center_axis',(-1.,0.,0.));
#34701=DIRECTION('ref_axis',(0.,-1.,0.));
#34702=DIRECTION('',(0.,0.,1.));
#34703=DIRECTION('center_axis',(0.,0.,1.));
#34704=DIRECTION('ref_axis',(-0.707106781186548,0.707106781186548,0.));
#34705=DIRECTION('',(0.,0.,-1.));
#34706=DIRECTION('center_axis',(0.,1.,0.));
#34707=DIRECTION('ref_axis',(-1.,0.,0.));
#34708=DIRECTION('',(0.,0.,1.));
#34709=DIRECTION('center_axis',(0.,0.,1.));
#34710=DIRECTION('ref_axis',(0.707106781186548,0.707106781186548,0.));
#34711=DIRECTION('',(0.,0.,-1.));
#34712=DIRECTION('center_axis',(1.,0.,0.));
#34713=DIRECTION('ref_axis',(0.,1.,0.));
#34714=DIRECTION('',(0.,0.,1.));
#34715=DIRECTION('center_axis',(0.,0.,1.));
#34716=DIRECTION('ref_axis',(0.707106781186545,-0.70710678118655,0.));
#34717=DIRECTION('',(0.,0.,-1.));
#34718=DIRECTION('center_axis',(0.,-1.,0.));
#34719=DIRECTION('ref_axis',(1.,0.,0.));
#34720=DIRECTION('',(0.,0.,1.));
#34721=DIRECTION('center_axis',(0.,0.,1.));
#34722=DIRECTION('ref_axis',(-0.70710678118655,-0.707106781186545,0.));
#34723=DIRECTION('',(0.,0.,-1.));
#34724=DIRECTION('center_axis',(-1.,0.,0.));
#34725=DIRECTION('ref_axis',(0.,-1.,0.));
#34726=DIRECTION('',(0.,0.,1.));
#34727=DIRECTION('center_axis',(0.,0.,1.));
#34728=DIRECTION('ref_axis',(0.707106781186548,0.707106781186548,0.));
#34729=DIRECTION('',(0.,0.,-1.));
#34730=DIRECTION('center_axis',(0.,-1.,0.));
#34731=DIRECTION('ref_axis',(1.,0.,0.));
#34732=DIRECTION('center_axis',(0.,0.,1.));
#34733=DIRECTION('ref_axis',(1.,0.,0.));
#34734=DIRECTION('',(0.707106781186548,8.65956056235493E-17,-0.707106781186548));
#34735=DIRECTION('center_axis',(0.,0.,1.));
#34736=DIRECTION('ref_axis',(1.,0.,0.));
#34737=DIRECTION('',(0.707106781186548,8.65956056235493E-17,-0.707106781186548));
#34738=DIRECTION('center_axis',(0.,0.,1.));
#34739=DIRECTION('ref_axis',(1.,0.,0.));
#34740=DIRECTION('',(0.707106781186549,8.65956056235495E-17,-0.707106781186546));
#34741=DIRECTION('center_axis',(0.,0.,1.));
#34742=DIRECTION('ref_axis',(1.,0.,0.));
#34743=DIRECTION('',(0.707106781186547,8.65956056235492E-17,-0.707106781186548));
#34744=DIRECTION('center_axis',(0.,0.,-1.));
#34745=DIRECTION('ref_axis',(1.,0.,0.));
#34746=DIRECTION('center_axis',(0.,0.,-1.));
#34747=DIRECTION('ref_axis',(1.,0.,0.));
#34748=DIRECTION('',(0.,0.,-1.));
#34749=DIRECTION('center_axis',(0.,0.,-1.));
#34750=DIRECTION('ref_axis',(1.,0.,0.));
#34751=DIRECTION('',(0.,0.,-1.));
#34752=DIRECTION('center_axis',(0.,0.,-1.));
#34753=DIRECTION('ref_axis',(1.,0.,0.));
#34754=DIRECTION('',(0.,0.,-1.));
#34755=DIRECTION('center_axis',(0.,0.,-1.));
#34756=DIRECTION('ref_axis',(1.,0.,0.));
#34757=DIRECTION('center_axis',(0.,0.,1.));
#34758=DIRECTION('ref_axis',(1.,0.,0.));
#34759=DIRECTION('center_axis',(-1.,0.,0.));
#34760=DIRECTION('ref_axis',(0.,0.,-1.));
#34761=DIRECTION('',(-1.,0.,0.));
#34762=DIRECTION('',(-1.,0.,0.));
#34763=DIRECTION('center_axis',(-1.,0.,0.));
#34764=DIRECTION('ref_axis',(0.,0.,-1.));
#34765=DIRECTION('center_axis',(1.,0.,0.));
#34766=DIRECTION('ref_axis',(0.,0.,-1.));
#34767=DIRECTION('center_axis',(-1.,0.,0.));
#34768=DIRECTION('ref_axis',(0.,0.,-1.));
#34769=DIRECTION('',(-1.,0.,0.));
#34770=DIRECTION('center_axis',(-1.,0.,0.));
#34771=DIRECTION('ref_axis',(0.,0.,-1.));
#34772=DIRECTION('center_axis',(1.,0.,0.));
#34773=DIRECTION('ref_axis',(0.,0.,-1.));
#34774=DIRECTION('center_axis',(0.,0.,1.));
#34775=DIRECTION('ref_axis',(1.,0.,0.));
#34776=DIRECTION('center_axis',(0.,0.,1.));
#34777=DIRECTION('ref_axis',(1.,0.,0.));
#34778=DIRECTION('center_axis',(0.,0.,-1.));
#34779=DIRECTION('ref_axis',(1.,0.,0.));
#34780=DIRECTION('',(0.,0.,-1.));
#34781=DIRECTION('center_axis',(0.,0.,-1.));
#34782=DIRECTION('ref_axis',(1.,0.,0.));
#34783=DIRECTION('center_axis',(0.,0.,1.));
#34784=DIRECTION('ref_axis',(1.,0.,0.));
#34785=DIRECTION('center_axis',(0.,0.,-1.));
#34786=DIRECTION('ref_axis',(1.,0.,0.));
#34787=DIRECTION('',(0.,0.,-1.));
#34788=DIRECTION('center_axis',(0.,0.,-1.));
#34789=DIRECTION('ref_axis',(1.,0.,0.));
#34790=DIRECTION('center_axis',(0.,0.,1.));
#34791=DIRECTION('ref_axis',(1.,0.,0.));
#34792=DIRECTION('center_axis',(0.,0.,-1.));
#34793=DIRECTION('ref_axis',(1.,0.,0.));
#34794=DIRECTION('',(0.,0.,-1.));
#34795=DIRECTION('center_axis',(0.,0.,-1.));
#34796=DIRECTION('ref_axis',(1.,0.,0.));
#34797=DIRECTION('center_axis',(0.,0.,1.));
#34798=DIRECTION('ref_axis',(1.,0.,0.));
#34799=DIRECTION('center_axis',(0.,0.,1.));
#34800=DIRECTION('ref_axis',(0.707106781186545,-0.70710678118655,0.));
#34801=DIRECTION('',(0.,0.,-1.));
#34802=DIRECTION('center_axis',(0.,-1.,0.));
#34803=DIRECTION('ref_axis',(1.,0.,0.));
#34804=DIRECTION('center_axis',(0.,0.,1.));
#34805=DIRECTION('ref_axis',(0.70710678118655,0.707106781186545,0.));
#34806=DIRECTION('axis',(0.,0.,1.));
#34807=DIRECTION('refdir',(1.,0.,0.));
#34808=DIRECTION('center_axis',(0.,0.,1.));
#34809=DIRECTION('ref_axis',(1.,0.,0.));
#34810=DIRECTION('center_axis',(0.,0.,-1.));
#34811=DIRECTION('ref_axis',(1.,0.,0.));
#34812=DIRECTION('',(-0.707106781186547,8.65956056235493E-17,0.707106781186547));
#34813=DIRECTION('center_axis',(0.,0.,1.));
#34814=DIRECTION('ref_axis',(1.,0.,0.));
#34815=DIRECTION('center_axis',(0.,0.,-1.));
#34816=DIRECTION('ref_axis',(1.,0.,0.));
#34817=DIRECTION('',(0.,0.,-1.));
#34818=DIRECTION('center_axis',(0.,0.,1.));
#34819=DIRECTION('ref_axis',(1.,0.,0.));
#34820=DIRECTION('center_axis',(0.,0.,1.));
#34821=DIRECTION('ref_axis',(1.,0.,0.));
#34822=DIRECTION('center_axis',(0.,0.,-1.));
#34823=DIRECTION('ref_axis',(1.,0.,0.));
#34824=DIRECTION('center_axis',(0.,0.,1.));
#34825=DIRECTION('ref_axis',(1.,0.,0.));
#34826=DIRECTION('center_axis',(0.,0.,-1.));
#34827=DIRECTION('ref_axis',(1.,0.,0.));
#34828=DIRECTION('',(-0.707106781186547,8.65956056235493E-17,0.707106781186547));
#34829=DIRECTION('center_axis',(0.,0.,1.));
#34830=DIRECTION('ref_axis',(1.,0.,0.));
#34831=DIRECTION('center_axis',(0.,0.,-1.));
#34832=DIRECTION('ref_axis',(1.,0.,0.));
#34833=DIRECTION('',(0.,0.,-1.));
#34834=DIRECTION('center_axis',(0.,0.,1.));
#34835=DIRECTION('ref_axis',(1.,0.,0.));
#34836=DIRECTION('center_axis',(0.,0.,1.));
#34837=DIRECTION('ref_axis',(1.,0.,0.));
#34838=DIRECTION('center_axis',(0.,0.,-1.));
#34839=DIRECTION('ref_axis',(1.,0.,0.));
#34840=DIRECTION('center_axis',(0.,0.,1.));
#34841=DIRECTION('ref_axis',(1.,0.,0.));
#34842=DIRECTION('center_axis',(0.,0.,-1.));
#34843=DIRECTION('ref_axis',(1.,0.,0.));
#34844=DIRECTION('',(-0.707106781186549,8.65956056235495E-17,0.707106781186546));
#34845=DIRECTION('center_axis',(0.,0.,1.));
#34846=DIRECTION('ref_axis',(1.,0.,0.));
#34847=DIRECTION('center_axis',(0.,0.,-1.));
#34848=DIRECTION('ref_axis',(1.,0.,0.));
#34849=DIRECTION('',(0.,0.,-1.));
#34850=DIRECTION('center_axis',(0.,0.,1.));
#34851=DIRECTION('ref_axis',(1.,0.,0.));
#34852=DIRECTION('center_axis',(0.,0.,1.));
#34853=DIRECTION('ref_axis',(1.,0.,0.));
#34854=DIRECTION('center_axis',(0.,0.,-1.));
#34855=DIRECTION('ref_axis',(1.,0.,0.));
#34856=DIRECTION('center_axis',(0.,0.,1.));
#34857=DIRECTION('ref_axis',(1.,0.,0.));
#34858=DIRECTION('center_axis',(0.,0.,-1.));
#34859=DIRECTION('ref_axis',(1.,0.,0.));
#34860=DIRECTION('',(-0.707106781186549,8.65956056235495E-17,0.707106781186546));
#34861=DIRECTION('center_axis',(0.,0.,1.));
#34862=DIRECTION('ref_axis',(1.,0.,0.));
#34863=DIRECTION('center_axis',(0.,0.,-1.));
#34864=DIRECTION('ref_axis',(1.,0.,0.));
#34865=DIRECTION('',(0.,0.,-1.));
#34866=DIRECTION('center_axis',(0.,0.,1.));
#34867=DIRECTION('ref_axis',(1.,0.,0.));
#34868=DIRECTION('center_axis',(0.,0.,1.));
#34869=DIRECTION('ref_axis',(1.,0.,0.));
#34870=DIRECTION('center_axis',(0.,0.,-1.));
#34871=DIRECTION('ref_axis',(1.,0.,0.));
#34872=DIRECTION('center_axis',(0.,0.,1.));
#34873=DIRECTION('ref_axis',(1.,0.,0.));
#34874=DIRECTION('center_axis',(0.,0.,-1.));
#34875=DIRECTION('ref_axis',(1.,0.,0.));
#34876=DIRECTION('',(-0.707106781186549,8.65956056235495E-17,0.707106781186546));
#34877=DIRECTION('center_axis',(0.,0.,1.));
#34878=DIRECTION('ref_axis',(1.,0.,0.));
#34879=DIRECTION('center_axis',(0.,0.,-1.));
#34880=DIRECTION('ref_axis',(1.,0.,0.));
#34881=DIRECTION('',(0.,0.,-1.));
#34882=DIRECTION('center_axis',(0.,0.,1.));
#34883=DIRECTION('ref_axis',(1.,0.,0.));
#34884=DIRECTION('center_axis',(0.,0.,1.));
#34885=DIRECTION('ref_axis',(1.,0.,0.));
#34886=DIRECTION('center_axis',(0.,0.,-1.));
#34887=DIRECTION('ref_axis',(1.,0.,0.));
#34888=DIRECTION('center_axis',(0.,0.,1.));
#34889=DIRECTION('ref_axis',(1.,0.,0.));
#34890=DIRECTION('center_axis',(0.,0.,-1.));
#34891=DIRECTION('ref_axis',(1.,0.,0.));
#34892=DIRECTION('',(-0.707106781186547,8.65956056235493E-17,0.707106781186547));
#34893=DIRECTION('center_axis',(0.,0.,1.));
#34894=DIRECTION('ref_axis',(1.,0.,0.));
#34895=DIRECTION('center_axis',(0.,0.,-1.));
#34896=DIRECTION('ref_axis',(1.,0.,0.));
#34897=DIRECTION('',(0.,0.,-1.));
#34898=DIRECTION('center_axis',(0.,0.,1.));
#34899=DIRECTION('ref_axis',(1.,0.,0.));
#34900=DIRECTION('center_axis',(0.,0.,1.));
#34901=DIRECTION('ref_axis',(1.,0.,0.));
#34902=DIRECTION('center_axis',(0.,0.,-1.));
#34903=DIRECTION('ref_axis',(1.,0.,0.));
#34904=DIRECTION('center_axis',(0.,0.,1.));
#34905=DIRECTION('ref_axis',(1.,0.,0.));
#34906=DIRECTION('center_axis',(0.,0.,-1.));
#34907=DIRECTION('ref_axis',(1.,0.,0.));
#34908=DIRECTION('',(-0.707106781186547,8.65956056235493E-17,0.707106781186547));
#34909=DIRECTION('center_axis',(0.,0.,1.));
#34910=DIRECTION('ref_axis',(1.,0.,0.));
#34911=DIRECTION('center_axis',(0.,0.,-1.));
#34912=DIRECTION('ref_axis',(1.,0.,0.));
#34913=DIRECTION('',(0.,0.,-1.));
#34914=DIRECTION('center_axis',(0.,0.,1.));
#34915=DIRECTION('ref_axis',(1.,0.,0.));
#34916=DIRECTION('center_axis',(0.,0.,1.));
#34917=DIRECTION('ref_axis',(1.,0.,0.));
#34918=DIRECTION('center_axis',(0.,0.,-1.));
#34919=DIRECTION('ref_axis',(1.,0.,0.));
#34920=DIRECTION('center_axis',(0.,0.,1.));
#34921=DIRECTION('ref_axis',(1.,0.,0.));
#34922=DIRECTION('center_axis',(0.,0.,-1.));
#34923=DIRECTION('ref_axis',(1.,0.,0.));
#34924=DIRECTION('',(-0.707106781186547,8.65956056235493E-17,0.707106781186547));
#34925=DIRECTION('center_axis',(0.,0.,1.));
#34926=DIRECTION('ref_axis',(1.,0.,0.));
#34927=DIRECTION('center_axis',(0.,0.,-1.));
#34928=DIRECTION('ref_axis',(1.,0.,0.));
#34929=DIRECTION('',(0.,0.,-1.));
#34930=DIRECTION('center_axis',(0.,0.,1.));
#34931=DIRECTION('ref_axis',(1.,0.,0.));
#34932=DIRECTION('center_axis',(0.,0.,1.));
#34933=DIRECTION('ref_axis',(1.,0.,0.));
#34934=DIRECTION('center_axis',(0.,0.,-1.));
#34935=DIRECTION('ref_axis',(1.,0.,0.));
#34936=DIRECTION('center_axis',(0.,0.,-1.));
#34937=DIRECTION('ref_axis',(1.,0.,0.));
#34938=DIRECTION('center_axis',(0.,0.,1.));
#34939=DIRECTION('ref_axis',(1.,0.,0.));
#34940=DIRECTION('',(-0.707106781186547,-8.65956056235493E-17,-0.707106781186547));
#34941=DIRECTION('center_axis',(0.,0.,-1.));
#34942=DIRECTION('ref_axis',(1.,0.,0.));
#34943=DIRECTION('center_axis',(0.,0.,-1.));
#34944=DIRECTION('ref_axis',(1.,0.,0.));
#34945=DIRECTION('center_axis',(0.,0.,-1.));
#34946=DIRECTION('ref_axis',(1.,0.,0.));
#34947=DIRECTION('',(0.,0.,-1.));
#34948=DIRECTION('center_axis',(0.,0.,1.));
#34949=DIRECTION('ref_axis',(1.,0.,0.));
#34950=DIRECTION('center_axis',(0.,0.,1.));
#34951=DIRECTION('ref_axis',(1.,0.,0.));
#34952=DIRECTION('center_axis',(0.707106781186548,-0.707106781186548,0.));
#34953=DIRECTION('ref_axis',(0.,0.,-1.));
#34954=DIRECTION('',(-0.577350269189629,-0.577350269189629,-0.577350269189619));
#34955=DIRECTION('',(0.,0.,-1.));
#34956=DIRECTION('',(0.577350269189629,0.577350269189629,-0.577350269189619));
#34957=DIRECTION('',(0.577350269189629,0.577350269189629,0.577350269189619));
#34958=DIRECTION('',(0.,0.,1.));
#34959=DIRECTION('',(-0.577350269189629,-0.577350269189629,0.577350269189619));
#34960=DIRECTION('center_axis',(0.707106781186541,0.,0.707106781186554));
#34961=DIRECTION('ref_axis',(0.707106781186554,0.,-0.707106781186541));
#34962=DIRECTION('',(0.,1.,0.));
#34963=DIRECTION('',(0.577350269189629,-0.577350269189629,-0.577350269189619));
#34964=DIRECTION('',(0.577350269189636,0.577350269189616,-0.577350269189626));
#34965=DIRECTION('',(0.,-1.,0.));
#34966=DIRECTION('',(0.577350269189616,-0.577350269189636,-0.577350269189626));
#34967=DIRECTION('center_axis',(1.,0.,0.));
#34968=DIRECTION('ref_axis',(0.,1.,0.));
#34969=DIRECTION('',(0.,-1.,0.));
#34970=DIRECTION('',(0.,0.,-1.));
#34971=DIRECTION('center_axis',(0.707106781186541,0.,-0.707106781186554));
#34972=DIRECTION('ref_axis',(-0.707106781186554,0.,-0.707106781186541));
#34973=DIRECTION('',(0.577350269189629,-0.577350269189629,0.577350269189619));
#34974=DIRECTION('',(0.,1.,0.));
#34975=DIRECTION('',(0.577350269189629,0.577350269189629,0.577350269189619));
#34976=DIRECTION('',(-0.577350269189629,0.577350269189629,-0.577350269189619));
#34977=DIRECTION('center_axis',(0.,0.,1.));
#34978=DIRECTION('ref_axis',(1.,0.,0.));
#34979=DIRECTION('center_axis',(0.,0.,-1.));
#34980=DIRECTION('ref_axis',(1.,0.,0.));
#34981=DIRECTION('',(-0.707106781186549,8.65956056235495E-17,0.707106781186546));
#34982=DIRECTION('center_axis',(0.,0.,1.));
#34983=DIRECTION('ref_axis',(1.,0.,0.));
#34984=DIRECTION('center_axis',(0.,0.,-1.));
#34985=DIRECTION('ref_axis',(1.,0.,0.));
#34986=DIRECTION('',(0.,0.,-1.));
#34987=DIRECTION('center_axis',(0.,0.,1.));
#34988=DIRECTION('ref_axis',(1.,0.,0.));
#34989=DIRECTION('center_axis',(0.,0.,1.));
#34990=DIRECTION('ref_axis',(1.,0.,0.));
#34991=DIRECTION('center_axis',(0.,0.,-1.));
#34992=DIRECTION('ref_axis',(1.,0.,0.));
#34993=DIRECTION('center_axis',(0.,0.,1.));
#34994=DIRECTION('ref_axis',(1.,0.,0.));
#34995=DIRECTION('center_axis',(0.,0.,-1.));
#34996=DIRECTION('ref_axis',(1.,0.,0.));
#34997=DIRECTION('',(-0.707106781186548,8.65956056235493E-17,0.707106781186548));
#34998=DIRECTION('center_axis',(0.,0.,1.));
#34999=DIRECTION('ref_axis',(1.,0.,0.));
#35000=DIRECTION('center_axis',(0.,0.,-1.));
#35001=DIRECTION('ref_axis',(1.,0.,0.));
#35002=DIRECTION('',(0.,0.,-1.));
#35003=DIRECTION('center_axis',(0.,0.,1.));
#35004=DIRECTION('ref_axis',(1.,0.,0.));
#35005=DIRECTION('center_axis',(0.,0.,1.));
#35006=DIRECTION('ref_axis',(1.,0.,0.));
#35007=DIRECTION('center_axis',(0.,0.,-1.));
#35008=DIRECTION('ref_axis',(1.,0.,0.));
#35009=DIRECTION('center_axis',(-0.707106781186548,-0.707106781186548,0.));
#35010=DIRECTION('ref_axis',(0.,0.,1.));
#35011=DIRECTION('',(-0.577350269189629,0.577350269189629,-0.577350269189619));
#35012=DIRECTION('',(0.,0.,-1.));
#35013=DIRECTION('',(0.577350269189629,-0.577350269189629,-0.577350269189619));
#35014=DIRECTION('',(0.577350269189629,-0.577350269189629,0.577350269189619));
#35015=DIRECTION('',(0.,0.,1.));
#35016=DIRECTION('',(-0.577350269189629,0.577350269189629,0.577350269189619));
#35017=DIRECTION('center_axis',(-0.707106781186541,0.,-0.707106781186554));
#35018=DIRECTION('ref_axis',(-0.707106781186554,0.,0.707106781186541));
#35019=DIRECTION('',(0.,1.,0.));
#35020=DIRECTION('',(-0.577350269189629,-0.577350269189629,0.577350269189619));
#35021=DIRECTION('',(0.577350269189616,-0.577350269189636,-0.577350269189626));
#35022=DIRECTION('',(0.,-1.,0.));
#35023=DIRECTION('',(-0.577350269189629,-0.577350269189629,0.577350269189619));
#35024=DIRECTION('center_axis',(-1.,0.,0.));
#35025=DIRECTION('ref_axis',(0.,-1.,0.));
#35026=DIRECTION('',(0.,-1.,0.));
#35027=DIRECTION('',(0.,0.,1.));
#35028=DIRECTION('center_axis',(-0.707106781186541,0.,0.707106781186554));
#35029=DIRECTION('ref_axis',(0.707106781186554,0.,0.707106781186541));
#35030=DIRECTION('',(-0.577350269189636,-0.577350269189616,-0.577350269189626));
#35031=DIRECTION('',(0.,1.,0.));
#35032=DIRECTION('',(-0.577350269189616,0.577350269189636,-0.577350269189626));
#35033=DIRECTION('',(0.577350269189629,0.577350269189629,0.577350269189619));
#35034=DIRECTION('center_axis',(0.707106781186548,0.707106781186548,0.));
#35035=DIRECTION('ref_axis',(0.,0.,-1.));
#35036=DIRECTION('',(-0.577350269189629,0.577350269189629,0.577350269189619));
#35037=DIRECTION('',(0.,0.,1.));
#35038=DIRECTION('',(0.577350269189629,-0.577350269189629,0.577350269189619));
#35039=DIRECTION('center_axis',(-0.707106781186548,0.707106781186548,0.));
#35040=DIRECTION('ref_axis',(0.,0.,1.));
#35041=DIRECTION('',(0.577350269189629,0.577350269189629,-0.577350269189619));
#35042=DIRECTION('',(0.,0.,-1.));
#35043=DIRECTION('',(-0.577350269189629,-0.577350269189629,-0.577350269189619));
#35044=DIRECTION('center_axis',(0.,0.,1.));
#35045=DIRECTION('ref_axis',(1.,0.,0.));
#35046=DIRECTION('center_axis',(0.,0.,-1.));
#35047=DIRECTION('ref_axis',(1.,0.,0.));
#35048=DIRECTION('',(-0.707106781186547,8.65956056235493E-17,0.707106781186547));
#35049=DIRECTION('center_axis',(0.,0.,1.));
#35050=DIRECTION('ref_axis',(1.,0.,0.));
#35051=DIRECTION('center_axis',(0.,0.,-1.));
#35052=DIRECTION('ref_axis',(1.,0.,0.));
#35053=DIRECTION('',(0.,0.,-1.));
#35054=DIRECTION('center_axis',(0.,0.,1.));
#35055=DIRECTION('ref_axis',(1.,0.,0.));
#35056=DIRECTION('center_axis',(0.,0.,1.));
#35057=DIRECTION('ref_axis',(1.,0.,0.));
#35058=DIRECTION('center_axis',(0.,0.,-1.));
#35059=DIRECTION('ref_axis',(1.,0.,0.));
#35060=DIRECTION('center_axis',(0.,0.,1.));
#35061=DIRECTION('ref_axis',(1.,0.,0.));
#35062=DIRECTION('center_axis',(0.,0.,-1.));
#35063=DIRECTION('ref_axis',(1.,0.,0.));
#35064=DIRECTION('',(-0.707106781186547,8.65956056235493E-17,0.707106781186547));
#35065=DIRECTION('center_axis',(0.,0.,1.));
#35066=DIRECTION('ref_axis',(1.,0.,0.));
#35067=DIRECTION('center_axis',(0.,0.,-1.));
#35068=DIRECTION('ref_axis',(1.,0.,0.));
#35069=DIRECTION('',(0.,0.,-1.));
#35070=DIRECTION('center_axis',(0.,0.,1.));
#35071=DIRECTION('ref_axis',(1.,0.,0.));
#35072=DIRECTION('center_axis',(0.,0.,1.));
#35073=DIRECTION('ref_axis',(1.,0.,0.));
#35074=DIRECTION('center_axis',(0.,0.,-1.));
#35075=DIRECTION('ref_axis',(1.,0.,0.));
#35076=DIRECTION('center_axis',(0.,0.,-1.));
#35077=DIRECTION('ref_axis',(1.,0.,0.));
#35078=DIRECTION('center_axis',(0.,0.,-1.));
#35079=DIRECTION('ref_axis',(1.,0.,0.));
#35080=DIRECTION('',(0.707106781186547,-8.65956056235493E-17,0.707106781186547));
#35081=DIRECTION('center_axis',(0.,0.,1.));
#35082=DIRECTION('ref_axis',(1.,0.,0.));
#35083=DIRECTION('',(-1.,0.,0.));
#35084=DIRECTION('',(1.,0.,0.));
#35085=DIRECTION('center_axis',(0.,0.,-1.));
#35086=DIRECTION('ref_axis',(1.,0.,0.));
#35087=DIRECTION('center_axis',(0.,0.,-1.));
#35088=DIRECTION('ref_axis',(1.,0.,0.));
#35089=DIRECTION('center_axis',(0.,0.,-1.));
#35090=DIRECTION('ref_axis',(1.,0.,0.));
#35091=DIRECTION('center_axis',(0.,0.,-1.));
#35092=DIRECTION('ref_axis',(1.,0.,0.));
#35093=DIRECTION('center_axis',(0.,0.,-1.));
#35094=DIRECTION('ref_axis',(1.,0.,0.));
#35095=DIRECTION('center_axis',(0.,0.,-1.));
#35096=DIRECTION('ref_axis',(1.,0.,0.));
#35097=DIRECTION('center_axis',(0.,0.,-1.));
#35098=DIRECTION('ref_axis',(1.,0.,0.));
#35099=DIRECTION('center_axis',(0.,0.,-1.));
#35100=DIRECTION('ref_axis',(1.,0.,0.));
#35101=DIRECTION('center_axis',(0.,0.,-1.));
#35102=DIRECTION('ref_axis',(1.,0.,0.));
#35103=DIRECTION('center_axis',(0.,0.,-1.));
#35104=DIRECTION('ref_axis',(1.,0.,0.));
#35105=DIRECTION('center_axis',(0.,0.,-1.));
#35106=DIRECTION('ref_axis',(1.,0.,0.));
#35107=DIRECTION('center_axis',(0.,0.,-1.));
#35108=DIRECTION('ref_axis',(1.,0.,0.));
#35109=DIRECTION('center_axis',(0.,0.,-1.));
#35110=DIRECTION('ref_axis',(1.,0.,0.));
#35111=DIRECTION('center_axis',(0.,0.,-1.));
#35112=DIRECTION('ref_axis',(1.,0.,0.));
#35113=DIRECTION('center_axis',(0.,0.,-1.));
#35114=DIRECTION('ref_axis',(1.,0.,0.));
#35115=DIRECTION('center_axis',(0.,0.,-1.));
#35116=DIRECTION('ref_axis',(1.,0.,0.));
#35117=DIRECTION('center_axis',(0.,0.,-1.));
#35118=DIRECTION('ref_axis',(1.,0.,0.));
#35119=DIRECTION('center_axis',(0.,0.,-1.));
#35120=DIRECTION('ref_axis',(1.,0.,0.));
#35121=DIRECTION('center_axis',(0.,0.,-1.));
#35122=DIRECTION('ref_axis',(1.,0.,0.));
#35123=DIRECTION('center_axis',(0.,0.,-1.));
#35124=DIRECTION('ref_axis',(1.,0.,0.));
#35125=DIRECTION('center_axis',(0.,0.,-1.));
#35126=DIRECTION('ref_axis',(1.,0.,0.));
#35127=DIRECTION('center_axis',(0.,0.,1.));
#35128=DIRECTION('ref_axis',(1.,0.,0.));
#35129=DIRECTION('center_axis',(0.,0.,-1.));
#35130=DIRECTION('ref_axis',(1.,0.,0.));
#35131=DIRECTION('center_axis',(0.,0.,-1.));
#35132=DIRECTION('ref_axis',(1.,0.,0.));
#35133=DIRECTION('center_axis',(0.,0.,-1.));
#35134=DIRECTION('ref_axis',(1.,0.,0.));
#35135=DIRECTION('center_axis',(0.,0.,-1.));
#35136=DIRECTION('ref_axis',(1.,0.,0.));
#35137=DIRECTION('center_axis',(0.,0.,-1.));
#35138=DIRECTION('ref_axis',(1.,0.,0.));
#35139=DIRECTION('center_axis',(0.,0.,-1.));
#35140=DIRECTION('ref_axis',(1.,0.,0.));
#35141=DIRECTION('center_axis',(0.,0.,-1.));
#35142=DIRECTION('ref_axis',(1.,0.,0.));
#35143=DIRECTION('center_axis',(0.,0.,-1.));
#35144=DIRECTION('ref_axis',(1.,0.,0.));
#35145=DIRECTION('center_axis',(0.,0.,-1.));
#35146=DIRECTION('ref_axis',(1.,0.,0.));
#35147=DIRECTION('center_axis',(0.,0.,-1.));
#35148=DIRECTION('ref_axis',(1.,0.,0.));
#35149=DIRECTION('center_axis',(0.,0.,-1.));
#35150=DIRECTION('ref_axis',(1.,0.,0.));
#35151=DIRECTION('center_axis',(0.,0.,-1.));
#35152=DIRECTION('ref_axis',(1.,0.,0.));
#35153=DIRECTION('center_axis',(0.,0.,-1.));
#35154=DIRECTION('ref_axis',(1.,0.,0.));
#35155=DIRECTION('center_axis',(0.,0.,-1.));
#35156=DIRECTION('ref_axis',(1.,0.,0.));
#35157=DIRECTION('center_axis',(0.,0.,-1.));
#35158=DIRECTION('ref_axis',(1.,0.,0.));
#35159=DIRECTION('center_axis',(0.,0.,-1.));
#35160=DIRECTION('ref_axis',(1.,0.,0.));
#35161=DIRECTION('center_axis',(0.,0.,-1.));
#35162=DIRECTION('ref_axis',(1.,0.,0.));
#35163=DIRECTION('center_axis',(0.,0.,-1.));
#35164=DIRECTION('ref_axis',(1.,0.,0.));
#35165=DIRECTION('center_axis',(0.,0.,-1.));
#35166=DIRECTION('ref_axis',(1.,0.,0.));
#35167=DIRECTION('center_axis',(0.,0.,-1.));
#35168=DIRECTION('ref_axis',(1.,0.,0.));
#35169=DIRECTION('',(0.707106781186547,-8.65956056235493E-17,0.707106781186547));
#35170=DIRECTION('center_axis',(0.,0.,-1.));
#35171=DIRECTION('ref_axis',(1.,0.,0.));
#35172=DIRECTION('',(0.707106781186549,-8.65956056235495E-17,0.707106781186546));
#35173=DIRECTION('center_axis',(0.,0.,-1.));
#35174=DIRECTION('ref_axis',(1.,0.,0.));
#35175=DIRECTION('',(0.707106781186549,-8.65956056235495E-17,0.707106781186546));
#35176=DIRECTION('center_axis',(0.,0.,-1.));
#35177=DIRECTION('ref_axis',(1.,0.,0.));
#35178=DIRECTION('',(0.707106781186549,-8.65956056235495E-17,0.707106781186546));
#35179=DIRECTION('center_axis',(0.,0.,-1.));
#35180=DIRECTION('ref_axis',(1.,0.,0.));
#35181=DIRECTION('',(0.707106781186547,-8.65956056235493E-17,0.707106781186547));
#35182=DIRECTION('center_axis',(0.,0.,-1.));
#35183=DIRECTION('ref_axis',(1.,0.,0.));
#35184=DIRECTION('',(0.707106781186547,-8.65956056235493E-17,0.707106781186547));
#35185=DIRECTION('center_axis',(0.,0.,-1.));
#35186=DIRECTION('ref_axis',(1.,0.,0.));
#35187=DIRECTION('',(0.707106781186547,-8.65956056235493E-17,0.707106781186547));
#35188=DIRECTION('center_axis',(0.,0.,-1.));
#35189=DIRECTION('ref_axis',(1.,0.,0.));
#35190=DIRECTION('',(0.707106781186548,-8.65956056235493E-17,0.707106781186548));
#35191=DIRECTION('center_axis',(0.,0.,1.));
#35192=DIRECTION('ref_axis',(1.,0.,0.));
#35193=DIRECTION('center_axis',(0.,0.,-1.));
#35194=DIRECTION('ref_axis',(1.,0.,0.));
#35195=DIRECTION('center_axis',(0.,0.,-1.));
#35196=DIRECTION('ref_axis',(1.,0.,0.));
#35197=DIRECTION('',(0.,0.,-1.));
#35198=DIRECTION('center_axis',(0.,0.,-1.));
#35199=DIRECTION('ref_axis',(1.,0.,0.));
#35200=DIRECTION('',(0.707106781186548,-8.65956056235493E-17,0.707106781186548));
#35201=DIRECTION('center_axis',(0.,0.,1.));
#35202=DIRECTION('ref_axis',(1.,0.,0.));
#35203=DIRECTION('center_axis',(0.,0.,-1.));
#35204=DIRECTION('ref_axis',(1.,0.,0.));
#35205=DIRECTION('center_axis',(0.,0.,-1.));
#35206=DIRECTION('ref_axis',(1.,0.,0.));
#35207=DIRECTION('',(0.,0.,-1.));
#35208=DIRECTION('center_axis',(0.,0.,-1.));
#35209=DIRECTION('ref_axis',(1.,0.,0.));
#35210=DIRECTION('',(0.707106781186547,-8.65956056235493E-17,0.707106781186547));
#35211=DIRECTION('center_axis',(0.,0.,-1.));
#35212=DIRECTION('ref_axis',(1.,0.,0.));
#35213=DIRECTION('',(0.707106781186547,-8.65956056235493E-17,0.707106781186547));
#35214=DIRECTION('center_axis',(0.,0.707106781186541,-0.707106781186554));
#35215=DIRECTION('ref_axis',(-1.,0.,0.));
#35216=DIRECTION('',(1.,0.,0.));
#35217=DIRECTION('center_axis',(0.,-0.707106781186541,-0.707106781186554));
#35218=DIRECTION('ref_axis',(-1.,0.,0.));
#35219=DIRECTION('',(-1.,0.,0.));
#35220=DIRECTION('center_axis',(0.,1.,0.));
#35221=DIRECTION('ref_axis',(-1.,0.,0.));
#35222=DIRECTION('',(-1.,0.,0.));
#35223=DIRECTION('center_axis',(0.,0.,-1.));
#35224=DIRECTION('ref_axis',(1.,0.,0.));
#35225=DIRECTION('',(0.707106781186548,-8.65956056235493E-17,0.707106781186548));
#35226=DIRECTION('center_axis',(0.,0.,1.));
#35227=DIRECTION('ref_axis',(1.,0.,0.));
#35228=DIRECTION('center_axis',(0.,0.,-1.));
#35229=DIRECTION('ref_axis',(1.,0.,0.));
#35230=DIRECTION('center_axis',(0.,0.,-1.));
#35231=DIRECTION('ref_axis',(1.,0.,0.));
#35232=DIRECTION('',(0.,0.,-1.));
#35233=DIRECTION('center_axis',(0.,0.,-1.));
#35234=DIRECTION('ref_axis',(1.,0.,0.));
#35235=DIRECTION('',(0.707106781186548,-8.65956056235493E-17,0.707106781186548));
#35236=DIRECTION('center_axis',(0.,0.,1.));
#35237=DIRECTION('ref_axis',(1.,0.,0.));
#35238=DIRECTION('center_axis',(0.,0.,-1.));
#35239=DIRECTION('ref_axis',(1.,0.,0.));
#35240=DIRECTION('center_axis',(0.,0.,-1.));
#35241=DIRECTION('ref_axis',(1.,0.,0.));
#35242=DIRECTION('',(0.,0.,-1.));
#35243=DIRECTION('center_axis',(0.,0.,-1.));
#35244=DIRECTION('ref_axis',(1.,0.,0.));
#35245=DIRECTION('',(0.707106781186547,-8.65956056235493E-17,0.707106781186547));
#35246=DIRECTION('center_axis',(0.,0.,1.));
#35247=DIRECTION('ref_axis',(1.,0.,0.));
#35248=DIRECTION('center_axis',(0.,0.,-1.));
#35249=DIRECTION('ref_axis',(1.,0.,0.));
#35250=DIRECTION('center_axis',(0.,0.,-1.));
#35251=DIRECTION('ref_axis',(1.,0.,0.));
#35252=DIRECTION('',(0.,0.,-1.));
#35253=DIRECTION('center_axis',(0.,0.,-1.));
#35254=DIRECTION('ref_axis',(1.,0.,0.));
#35255=DIRECTION('',(0.707106781186548,-8.65956056235493E-17,0.707106781186548));
#35256=DIRECTION('center_axis',(0.,0.,1.));
#35257=DIRECTION('ref_axis',(1.,0.,0.));
#35258=DIRECTION('center_axis',(0.,0.,-1.));
#35259=DIRECTION('ref_axis',(1.,0.,0.));
#35260=DIRECTION('center_axis',(0.,0.,-1.));
#35261=DIRECTION('ref_axis',(1.,0.,0.));
#35262=DIRECTION('',(0.,0.,-1.));
#35263=DIRECTION('center_axis',(0.,0.,-1.));
#35264=DIRECTION('ref_axis',(1.,0.,0.));
#35265=DIRECTION('',(0.707106781186549,-8.65956056235495E-17,0.707106781186546));
#35266=DIRECTION('center_axis',(0.,0.,1.));
#35267=DIRECTION('ref_axis',(1.,0.,0.));
#35268=DIRECTION('center_axis',(0.,0.,-1.));
#35269=DIRECTION('ref_axis',(1.,0.,0.));
#35270=DIRECTION('center_axis',(0.,0.,-1.));
#35271=DIRECTION('ref_axis',(1.,0.,0.));
#35272=DIRECTION('',(0.,0.,-1.));
#35273=DIRECTION('center_axis',(0.,0.,-1.));
#35274=DIRECTION('ref_axis',(1.,0.,0.));
#35275=DIRECTION('',(0.707106781186549,-8.65956056235495E-17,0.707106781186546));
#35276=DIRECTION('center_axis',(0.,0.,1.));
#35277=DIRECTION('ref_axis',(1.,0.,0.));
#35278=DIRECTION('center_axis',(0.,0.,-1.));
#35279=DIRECTION('ref_axis',(1.,0.,0.));
#35280=DIRECTION('center_axis',(0.,0.,-1.));
#35281=DIRECTION('ref_axis',(1.,0.,0.));
#35282=DIRECTION('',(0.,0.,-1.));
#35283=DIRECTION('center_axis',(0.,0.,-1.));
#35284=DIRECTION('ref_axis',(1.,0.,0.));
#35285=DIRECTION('',(0.707106781186549,-8.65956056235495E-17,0.707106781186546));
#35286=DIRECTION('center_axis',(0.,0.,1.));
#35287=DIRECTION('ref_axis',(1.,0.,0.));
#35288=DIRECTION('center_axis',(0.,0.,-1.));
#35289=DIRECTION('ref_axis',(1.,0.,0.));
#35290=DIRECTION('center_axis',(0.,0.,-1.));
#35291=DIRECTION('ref_axis',(1.,0.,0.));
#35292=DIRECTION('',(0.,0.,-1.));
#35293=DIRECTION('center_axis',(0.,0.,-1.));
#35294=DIRECTION('ref_axis',(1.,0.,0.));
#35295=DIRECTION('',(0.707106781186549,-8.65956056235495E-17,0.707106781186546));
#35296=DIRECTION('center_axis',(0.,0.,1.));
#35297=DIRECTION('ref_axis',(1.,0.,0.));
#35298=DIRECTION('center_axis',(0.,0.,-1.));
#35299=DIRECTION('ref_axis',(1.,0.,0.));
#35300=DIRECTION('center_axis',(0.,0.,-1.));
#35301=DIRECTION('ref_axis',(1.,0.,0.));
#35302=DIRECTION('',(0.,0.,-1.));
#35303=DIRECTION('center_axis',(0.,0.,-1.));
#35304=DIRECTION('ref_axis',(1.,0.,0.));
#35305=DIRECTION('',(0.707106781186548,-8.65956056235493E-17,0.707106781186548));
#35306=DIRECTION('center_axis',(0.,0.,1.));
#35307=DIRECTION('ref_axis',(1.,0.,0.));
#35308=DIRECTION('center_axis',(0.,0.,-1.));
#35309=DIRECTION('ref_axis',(1.,0.,0.));
#35310=DIRECTION('center_axis',(0.,0.,-1.));
#35311=DIRECTION('ref_axis',(1.,0.,0.));
#35312=DIRECTION('',(0.,0.,-1.));
#35313=DIRECTION('center_axis',(0.,0.,-1.));
#35314=DIRECTION('ref_axis',(1.,0.,0.));
#35315=DIRECTION('',(0.707106781186548,-8.65956056235493E-17,0.707106781186548));
#35316=DIRECTION('center_axis',(0.,0.,1.));
#35317=DIRECTION('ref_axis',(1.,0.,0.));
#35318=DIRECTION('center_axis',(0.,0.,-1.));
#35319=DIRECTION('ref_axis',(1.,0.,0.));
#35320=DIRECTION('center_axis',(0.,0.,-1.));
#35321=DIRECTION('ref_axis',(1.,0.,0.));
#35322=DIRECTION('',(0.,0.,-1.));
#35323=DIRECTION('center_axis',(0.,0.,-1.));
#35324=DIRECTION('ref_axis',(1.,0.,0.));
#35325=DIRECTION('',(0.707106781186547,-8.65956056235493E-17,0.707106781186547));
#35326=DIRECTION('center_axis',(0.,0.,1.));
#35327=DIRECTION('ref_axis',(1.,0.,0.));
#35328=DIRECTION('center_axis',(0.,0.,-1.));
#35329=DIRECTION('ref_axis',(1.,0.,0.));
#35330=DIRECTION('center_axis',(0.,0.,-1.));
#35331=DIRECTION('ref_axis',(1.,0.,0.));
#35332=DIRECTION('',(0.,0.,-1.));
#35333=DIRECTION('center_axis',(0.,0.,-1.));
#35334=DIRECTION('ref_axis',(1.,0.,0.));
#35335=DIRECTION('',(0.707106781186547,-8.65956056235493E-17,0.707106781186547));
#35336=DIRECTION('center_axis',(0.,0.,1.));
#35337=DIRECTION('ref_axis',(1.,0.,0.));
#35338=DIRECTION('center_axis',(0.,0.,-1.));
#35339=DIRECTION('ref_axis',(1.,0.,0.));
#35340=DIRECTION('center_axis',(0.,0.,-1.));
#35341=DIRECTION('ref_axis',(1.,0.,0.));
#35342=DIRECTION('',(0.,0.,-1.));
#35343=DIRECTION('center_axis',(0.,0.,-1.));
#35344=DIRECTION('ref_axis',(1.,0.,0.));
#35345=DIRECTION('',(0.707106781186548,-8.65956056235493E-17,0.707106781186548));
#35346=DIRECTION('center_axis',(0.,0.,-1.));
#35347=DIRECTION('ref_axis',(1.,0.,0.));
#35348=DIRECTION('',(0.707106781186549,-8.65956056235495E-17,0.707106781186546));
#35349=DIRECTION('center_axis',(0.,0.,-1.));
#35350=DIRECTION('ref_axis',(1.,0.,0.));
#35351=DIRECTION('',(0.707106781186549,-8.65956056235495E-17,0.707106781186546));
#35352=DIRECTION('center_axis',(0.,0.,1.));
#35353=DIRECTION('ref_axis',(1.,0.,0.));
#35354=DIRECTION('center_axis',(0.,0.,-1.));
#35355=DIRECTION('ref_axis',(1.,0.,0.));
#35356=DIRECTION('center_axis',(0.,0.,-1.));
#35357=DIRECTION('ref_axis',(1.,0.,0.));
#35358=DIRECTION('',(0.,0.,-1.));
#35359=DIRECTION('center_axis',(0.,0.,-1.));
#35360=DIRECTION('ref_axis',(1.,0.,0.));
#35361=DIRECTION('',(0.707106781186549,-8.65956056235495E-17,0.707106781186546));
#35362=DIRECTION('center_axis',(0.,0.,1.));
#35363=DIRECTION('ref_axis',(1.,0.,0.));
#35364=DIRECTION('center_axis',(0.,0.,-1.));
#35365=DIRECTION('ref_axis',(1.,0.,0.));
#35366=DIRECTION('center_axis',(0.,0.,-1.));
#35367=DIRECTION('ref_axis',(1.,0.,0.));
#35368=DIRECTION('',(0.,0.,-1.));
#35369=DIRECTION('center_axis',(0.,0.,-1.));
#35370=DIRECTION('ref_axis',(1.,0.,0.));
#35371=DIRECTION('',(0.707106781186547,-8.65956056235493E-17,0.707106781186547));
#35372=DIRECTION('center_axis',(0.,0.,1.));
#35373=DIRECTION('ref_axis',(1.,0.,0.));
#35374=DIRECTION('center_axis',(0.,0.,-1.));
#35375=DIRECTION('ref_axis',(1.,0.,0.));
#35376=DIRECTION('center_axis',(0.,0.,-1.));
#35377=DIRECTION('ref_axis',(1.,0.,0.));
#35378=DIRECTION('',(0.,0.,-1.));
#35379=DIRECTION('center_axis',(0.,0.,-1.));
#35380=DIRECTION('ref_axis',(1.,0.,0.));
#35381=DIRECTION('',(0.707106781186549,-8.65956056235495E-17,0.707106781186546));
#35382=DIRECTION('center_axis',(0.,0.,1.));
#35383=DIRECTION('ref_axis',(1.,0.,0.));
#35384=DIRECTION('center_axis',(0.,0.,-1.));
#35385=DIRECTION('ref_axis',(1.,0.,0.));
#35386=DIRECTION('center_axis',(0.,0.,-1.));
#35387=DIRECTION('ref_axis',(1.,0.,0.));
#35388=DIRECTION('',(0.,0.,-1.));
#35389=DIRECTION('center_axis',(0.,0.,-1.));
#35390=DIRECTION('ref_axis',(1.,0.,0.));
#35391=DIRECTION('',(0.707106781186548,-8.65956056235493E-17,0.707106781186548));
#35392=DIRECTION('center_axis',(0.,0.,1.));
#35393=DIRECTION('ref_axis',(1.,0.,0.));
#35394=DIRECTION('center_axis',(0.,0.,-1.));
#35395=DIRECTION('ref_axis',(1.,0.,0.));
#35396=DIRECTION('center_axis',(0.,0.,-1.));
#35397=DIRECTION('ref_axis',(1.,0.,0.));
#35398=DIRECTION('',(0.,0.,-1.));
#35399=DIRECTION('center_axis',(0.,0.,-1.));
#35400=DIRECTION('ref_axis',(1.,0.,0.));
#35401=DIRECTION('',(0.707106781186547,-8.65956056235493E-17,0.707106781186547));
#35402=DIRECTION('center_axis',(0.,0.,1.));
#35403=DIRECTION('ref_axis',(1.,0.,0.));
#35404=DIRECTION('center_axis',(0.,0.,-1.));
#35405=DIRECTION('ref_axis',(1.,0.,0.));
#35406=DIRECTION('center_axis',(0.,0.,-1.));
#35407=DIRECTION('ref_axis',(1.,0.,0.));
#35408=DIRECTION('',(0.,0.,-1.));
#35409=DIRECTION('center_axis',(0.,0.,-1.));
#35410=DIRECTION('ref_axis',(1.,0.,0.));
#35411=DIRECTION('',(0.707106781186547,-8.65956056235493E-17,0.707106781186547));
#35412=DIRECTION('center_axis',(0.,0.,1.));
#35413=DIRECTION('ref_axis',(1.,0.,0.));
#35414=DIRECTION('center_axis',(0.,0.,-1.));
#35415=DIRECTION('ref_axis',(1.,0.,0.));
#35416=DIRECTION('center_axis',(0.,0.,-1.));
#35417=DIRECTION('ref_axis',(1.,0.,0.));
#35418=DIRECTION('',(0.,0.,-1.));
#35419=DIRECTION('center_axis',(0.,0.,-1.));
#35420=DIRECTION('ref_axis',(1.,0.,0.));
#35421=DIRECTION('',(0.707106781186547,-8.65956056235493E-17,0.707106781186547));
#35422=DIRECTION('center_axis',(0.,0.,1.));
#35423=DIRECTION('ref_axis',(1.,0.,0.));
#35424=DIRECTION('center_axis',(0.,0.,-1.));
#35425=DIRECTION('ref_axis',(1.,0.,0.));
#35426=DIRECTION('center_axis',(0.,0.,-1.));
#35427=DIRECTION('ref_axis',(1.,0.,0.));
#35428=DIRECTION('',(0.,0.,-1.));
#35429=DIRECTION('center_axis',(0.,0.,-1.));
#35430=DIRECTION('ref_axis',(1.,0.,0.));
#35431=DIRECTION('',(0.707106781186547,-8.65956056235493E-17,0.707106781186547));
#35432=DIRECTION('center_axis',(0.,0.,1.));
#35433=DIRECTION('ref_axis',(1.,0.,0.));
#35434=DIRECTION('center_axis',(0.,0.,-1.));
#35435=DIRECTION('ref_axis',(1.,0.,0.));
#35436=DIRECTION('center_axis',(0.,0.,-1.));
#35437=DIRECTION('ref_axis',(1.,0.,0.));
#35438=DIRECTION('',(0.,0.,-1.));
#35439=DIRECTION('center_axis',(0.,0.,-1.));
#35440=DIRECTION('ref_axis',(1.,0.,0.));
#35441=DIRECTION('',(0.707106781186547,-8.65956056235493E-17,0.707106781186547));
#35442=DIRECTION('center_axis',(0.,0.,1.));
#35443=DIRECTION('ref_axis',(1.,0.,0.));
#35444=DIRECTION('center_axis',(0.,0.,-1.));
#35445=DIRECTION('ref_axis',(1.,0.,0.));
#35446=DIRECTION('center_axis',(0.,0.,-1.));
#35447=DIRECTION('ref_axis',(1.,0.,0.));
#35448=DIRECTION('',(0.,0.,-1.));
#35449=DIRECTION('center_axis',(0.,0.,-1.));
#35450=DIRECTION('ref_axis',(1.,0.,0.));
#35451=DIRECTION('',(0.707106781186549,-8.65956056235495E-17,0.707106781186546));
#35452=DIRECTION('center_axis',(0.,0.,1.));
#35453=DIRECTION('ref_axis',(1.,0.,0.));
#35454=DIRECTION('center_axis',(0.,0.,-1.));
#35455=DIRECTION('ref_axis',(1.,0.,0.));
#35456=DIRECTION('center_axis',(0.,0.,-1.));
#35457=DIRECTION('ref_axis',(1.,0.,0.));
#35458=DIRECTION('',(0.,0.,-1.));
#35459=DIRECTION('center_axis',(0.,0.,-1.));
#35460=DIRECTION('ref_axis',(1.,0.,0.));
#35461=DIRECTION('',(0.707106781186547,-8.65956056235493E-17,0.707106781186547));
#35462=DIRECTION('center_axis',(0.,0.,1.));
#35463=DIRECTION('ref_axis',(1.,0.,0.));
#35464=DIRECTION('center_axis',(0.,0.,-1.));
#35465=DIRECTION('ref_axis',(1.,0.,0.));
#35466=DIRECTION('center_axis',(0.,0.,-1.));
#35467=DIRECTION('ref_axis',(1.,0.,0.));
#35468=DIRECTION('',(0.,0.,-1.));
#35469=DIRECTION('center_axis',(0.,0.,-1.));
#35470=DIRECTION('ref_axis',(1.,0.,0.));
#35471=DIRECTION('',(0.707106781186549,-8.65956056235495E-17,0.707106781186546));
#35472=DIRECTION('center_axis',(0.,0.,1.));
#35473=DIRECTION('ref_axis',(1.,0.,0.));
#35474=DIRECTION('center_axis',(0.,0.,-1.));
#35475=DIRECTION('ref_axis',(1.,0.,0.));
#35476=DIRECTION('center_axis',(0.,0.,-1.));
#35477=DIRECTION('ref_axis',(1.,0.,0.));
#35478=DIRECTION('',(0.,0.,-1.));
#35479=DIRECTION('center_axis',(0.,0.,-1.));
#35480=DIRECTION('ref_axis',(1.,0.,0.));
#35481=DIRECTION('',(0.707106781186549,-8.65956056235495E-17,0.707106781186546));
#35482=DIRECTION('center_axis',(0.,0.,1.));
#35483=DIRECTION('ref_axis',(1.,0.,0.));
#35484=DIRECTION('center_axis',(0.,0.,-1.));
#35485=DIRECTION('ref_axis',(1.,0.,0.));
#35486=DIRECTION('center_axis',(0.,0.,-1.));
#35487=DIRECTION('ref_axis',(1.,0.,0.));
#35488=DIRECTION('',(0.,0.,-1.));
#35489=DIRECTION('center_axis',(0.,0.,-1.));
#35490=DIRECTION('ref_axis',(1.,0.,0.));
#35491=DIRECTION('',(0.707106781186547,-8.65956056235493E-17,0.707106781186547));
#35492=DIRECTION('center_axis',(0.,0.,1.));
#35493=DIRECTION('ref_axis',(1.,0.,0.));
#35494=DIRECTION('center_axis',(0.,0.,-1.));
#35495=DIRECTION('ref_axis',(1.,0.,0.));
#35496=DIRECTION('center_axis',(0.,0.,-1.));
#35497=DIRECTION('ref_axis',(1.,0.,0.));
#35498=DIRECTION('',(0.,0.,-1.));
#35499=DIRECTION('center_axis',(0.,-0.707106781186541,0.707106781186554));
#35500=DIRECTION('ref_axis',(1.,0.,0.));
#35501=DIRECTION('',(-1.,0.,0.));
#35502=DIRECTION('',(1.,0.,0.));
#35503=DIRECTION('center_axis',(0.,0.707106781186541,0.707106781186554));
#35504=DIRECTION('ref_axis',(1.,0.,0.));
#35505=DIRECTION('',(1.,0.,0.));
#35506=DIRECTION('center_axis',(0.,0.,1.));
#35507=DIRECTION('ref_axis',(1.,0.,0.));
#35508=DIRECTION('center_axis',(0.,0.,1.));
#35509=DIRECTION('ref_axis',(1.,0.,0.));
#35510=DIRECTION('center_axis',(0.,0.,1.));
#35511=DIRECTION('ref_axis',(1.,0.,0.));
#35512=DIRECTION('center_axis',(0.,0.,1.));
#35513=DIRECTION('ref_axis',(1.,0.,0.));
#35514=DIRECTION('center_axis',(0.,0.,1.));
#35515=DIRECTION('ref_axis',(1.,0.,0.));
#35516=DIRECTION('center_axis',(0.,0.,1.));
#35517=DIRECTION('ref_axis',(1.,0.,0.));
#35518=DIRECTION('center_axis',(0.,0.,1.));
#35519=DIRECTION('ref_axis',(1.,0.,0.));
#35520=DIRECTION('center_axis',(0.,0.,1.));
#35521=DIRECTION('ref_axis',(1.,0.,0.));
#35522=DIRECTION('center_axis',(0.,0.,1.));
#35523=DIRECTION('ref_axis',(1.,0.,0.));
#35524=DIRECTION('center_axis',(0.,0.,1.));
#35525=DIRECTION('ref_axis',(1.,0.,0.));
#35526=DIRECTION('center_axis',(0.,0.,1.));
#35527=DIRECTION('ref_axis',(1.,0.,0.));
#35528=DIRECTION('center_axis',(0.,0.,1.));
#35529=DIRECTION('ref_axis',(1.,0.,0.));
#35530=DIRECTION('center_axis',(0.,0.,1.));
#35531=DIRECTION('ref_axis',(1.,0.,0.));
#35532=DIRECTION('center_axis',(0.,0.,1.));
#35533=DIRECTION('ref_axis',(1.,0.,0.));
#35534=DIRECTION('center_axis',(0.,0.,1.));
#35535=DIRECTION('ref_axis',(1.,0.,0.));
#35536=DIRECTION('center_axis',(0.,0.,1.));
#35537=DIRECTION('ref_axis',(1.,0.,0.));
#35538=DIRECTION('center_axis',(0.,0.,1.));
#35539=DIRECTION('ref_axis',(1.,0.,0.));
#35540=DIRECTION('center_axis',(0.,0.,1.));
#35541=DIRECTION('ref_axis',(1.,0.,0.));
#35542=DIRECTION('center_axis',(0.,0.,1.));
#35543=DIRECTION('ref_axis',(1.,0.,0.));
#35544=DIRECTION('center_axis',(0.,0.,1.));
#35545=DIRECTION('ref_axis',(1.,0.,0.));
#35546=DIRECTION('center_axis',(0.,0.,1.));
#35547=DIRECTION('ref_axis',(1.,0.,0.));
#35548=DIRECTION('center_axis',(0.,0.,1.));
#35549=DIRECTION('ref_axis',(1.,0.,0.));
#35550=DIRECTION('center_axis',(0.,0.,1.));
#35551=DIRECTION('ref_axis',(1.,0.,0.));
#35552=DIRECTION('center_axis',(0.,0.,1.));
#35553=DIRECTION('ref_axis',(1.,0.,0.));
#35554=DIRECTION('center_axis',(0.,0.,1.));
#35555=DIRECTION('ref_axis',(1.,0.,0.));
#35556=DIRECTION('center_axis',(0.,0.,1.));
#35557=DIRECTION('ref_axis',(1.,0.,0.));
#35558=DIRECTION('center_axis',(0.,0.,1.));
#35559=DIRECTION('ref_axis',(1.,0.,0.));
#35560=DIRECTION('center_axis',(0.,0.,1.));
#35561=DIRECTION('ref_axis',(1.,0.,0.));
#35562=DIRECTION('center_axis',(0.,0.,1.));
#35563=DIRECTION('ref_axis',(1.,0.,0.));
#35564=DIRECTION('center_axis',(0.,0.,1.));
#35565=DIRECTION('ref_axis',(1.,0.,0.));
#35566=DIRECTION('center_axis',(0.,0.,1.));
#35567=DIRECTION('ref_axis',(1.,0.,0.));
#35568=DIRECTION('center_axis',(0.,0.,1.));
#35569=DIRECTION('ref_axis',(1.,0.,0.));
#35570=DIRECTION('center_axis',(0.,0.,1.));
#35571=DIRECTION('ref_axis',(1.,0.,0.));
#35572=DIRECTION('center_axis',(0.,0.,1.));
#35573=DIRECTION('ref_axis',(1.,0.,0.));
#35574=DIRECTION('center_axis',(0.,0.,1.));
#35575=DIRECTION('ref_axis',(1.,0.,0.));
#35576=DIRECTION('center_axis',(0.,0.,1.));
#35577=DIRECTION('ref_axis',(1.,0.,0.));
#35578=DIRECTION('center_axis',(0.,0.,1.));
#35579=DIRECTION('ref_axis',(1.,0.,0.));
#35580=DIRECTION('center_axis',(0.,0.,1.));
#35581=DIRECTION('ref_axis',(1.,0.,0.));
#35582=DIRECTION('center_axis',(0.,0.,1.));
#35583=DIRECTION('ref_axis',(1.,0.,0.));
#35584=DIRECTION('center_axis',(0.,0.,1.));
#35585=DIRECTION('ref_axis',(1.,0.,0.));
#35586=DIRECTION('center_axis',(0.,0.,1.));
#35587=DIRECTION('ref_axis',(1.,0.,0.));
#35588=DIRECTION('center_axis',(0.,0.,1.));
#35589=DIRECTION('ref_axis',(1.,0.,0.));
#35590=DIRECTION('center_axis',(0.,0.,1.));
#35591=DIRECTION('ref_axis',(1.,0.,0.));
#35592=DIRECTION('center_axis',(0.,0.,1.));
#35593=DIRECTION('ref_axis',(1.,0.,0.));
#35594=DIRECTION('',(0.707106781186547,8.65956056235493E-17,-0.707106781186547));
#35595=DIRECTION('center_axis',(0.,0.,1.));
#35596=DIRECTION('ref_axis',(1.,0.,0.));
#35597=DIRECTION('',(0.707106781186547,8.65956056235493E-17,-0.707106781186547));
#35598=DIRECTION('center_axis',(0.,0.,1.));
#35599=DIRECTION('ref_axis',(1.,0.,0.));
#35600=DIRECTION('',(0.707106781186549,8.65956056235495E-17,-0.707106781186546));
#35601=DIRECTION('center_axis',(0.,0.,1.));
#35602=DIRECTION('ref_axis',(1.,0.,0.));
#35603=DIRECTION('',(0.707106781186549,8.65956056235495E-17,-0.707106781186546));
#35604=DIRECTION('center_axis',(0.,0.,1.));
#35605=DIRECTION('ref_axis',(1.,0.,0.));
#35606=DIRECTION('',(0.707106781186547,8.65956056235493E-17,-0.707106781186547));
#35607=DIRECTION('center_axis',(0.,0.,1.));
#35608=DIRECTION('ref_axis',(1.,0.,0.));
#35609=DIRECTION('',(0.707106781186549,8.65956056235495E-17,-0.707106781186546));
#35610=DIRECTION('center_axis',(0.,0.,1.));
#35611=DIRECTION('ref_axis',(1.,0.,0.));
#35612=DIRECTION('',(0.707106781186547,8.65956056235493E-17,-0.707106781186547));
#35613=DIRECTION('center_axis',(0.,0.,1.));
#35614=DIRECTION('ref_axis',(1.,0.,0.));
#35615=DIRECTION('',(0.707106781186547,8.65956056235493E-17,-0.707106781186547));
#35616=DIRECTION('center_axis',(0.,0.,1.));
#35617=DIRECTION('ref_axis',(1.,0.,0.));
#35618=DIRECTION('',(0.707106781186548,8.65956056235494E-17,-0.707106781186548));
#35619=DIRECTION('center_axis',(0.,0.,-1.));
#35620=DIRECTION('ref_axis',(1.,0.,0.));
#35621=DIRECTION('center_axis',(0.,0.,-1.));
#35622=DIRECTION('ref_axis',(1.,0.,0.));
#35623=DIRECTION('',(0.,0.,-1.));
#35624=DIRECTION('center_axis',(0.,0.,1.));
#35625=DIRECTION('ref_axis',(1.,0.,0.));
#35626=DIRECTION('',(0.707106781186548,8.65956056235494E-17,-0.707106781186548));
#35627=DIRECTION('center_axis',(0.,0.,-1.));
#35628=DIRECTION('ref_axis',(1.,0.,0.));
#35629=DIRECTION('center_axis',(0.,0.,-1.));
#35630=DIRECTION('ref_axis',(1.,0.,0.));
#35631=DIRECTION('',(0.,0.,-1.));
#35632=DIRECTION('center_axis',(0.,0.,1.));
#35633=DIRECTION('ref_axis',(1.,0.,0.));
#35634=DIRECTION('',(0.707106781186547,8.65956056235493E-17,-0.707106781186547));
#35635=DIRECTION('center_axis',(0.,0.,-1.));
#35636=DIRECTION('ref_axis',(1.,0.,0.));
#35637=DIRECTION('center_axis',(0.,0.,-1.));
#35638=DIRECTION('ref_axis',(1.,0.,0.));
#35639=DIRECTION('',(0.,0.,-1.));
#35640=DIRECTION('center_axis',(0.,0.,1.));
#35641=DIRECTION('ref_axis',(1.,0.,0.));
#35642=DIRECTION('',(0.707106781186548,8.65956056235494E-17,-0.707106781186548));
#35643=DIRECTION('center_axis',(0.,0.,-1.));
#35644=DIRECTION('ref_axis',(1.,0.,0.));
#35645=DIRECTION('center_axis',(0.,0.,-1.));
#35646=DIRECTION('ref_axis',(1.,0.,0.));
#35647=DIRECTION('',(0.,0.,-1.));
#35648=DIRECTION('center_axis',(0.,0.,1.));
#35649=DIRECTION('ref_axis',(1.,0.,0.));
#35650=DIRECTION('',(0.707106781186549,8.65956056235495E-17,-0.707106781186546));
#35651=DIRECTION('center_axis',(0.,0.,-1.));
#35652=DIRECTION('ref_axis',(1.,0.,0.));
#35653=DIRECTION('center_axis',(0.,0.,-1.));
#35654=DIRECTION('ref_axis',(1.,0.,0.));
#35655=DIRECTION('',(0.,0.,-1.));
#35656=DIRECTION('center_axis',(0.,0.,1.));
#35657=DIRECTION('ref_axis',(1.,0.,0.));
#35658=DIRECTION('',(0.707106781186549,8.65956056235495E-17,-0.707106781186546));
#35659=DIRECTION('center_axis',(0.,0.,-1.));
#35660=DIRECTION('ref_axis',(1.,0.,0.));
#35661=DIRECTION('center_axis',(0.,0.,-1.));
#35662=DIRECTION('ref_axis',(1.,0.,0.));
#35663=DIRECTION('',(0.,0.,-1.));
#35664=DIRECTION('center_axis',(0.,0.,1.));
#35665=DIRECTION('ref_axis',(1.,0.,0.));
#35666=DIRECTION('',(0.707106781186549,8.65956056235495E-17,-0.707106781186546));
#35667=DIRECTION('center_axis',(0.,0.,-1.));
#35668=DIRECTION('ref_axis',(1.,0.,0.));
#35669=DIRECTION('center_axis',(0.,0.,-1.));
#35670=DIRECTION('ref_axis',(1.,0.,0.));
#35671=DIRECTION('',(0.,0.,-1.));
#35672=DIRECTION('center_axis',(0.,0.,1.));
#35673=DIRECTION('ref_axis',(1.,0.,0.));
#35674=DIRECTION('',(0.707106781186548,8.65956056235494E-17,-0.707106781186548));
#35675=DIRECTION('center_axis',(0.,0.,-1.));
#35676=DIRECTION('ref_axis',(1.,0.,0.));
#35677=DIRECTION('center_axis',(0.,0.,-1.));
#35678=DIRECTION('ref_axis',(1.,0.,0.));
#35679=DIRECTION('',(0.,0.,-1.));
#35680=DIRECTION('center_axis',(0.,0.,1.));
#35681=DIRECTION('ref_axis',(1.,0.,0.));
#35682=DIRECTION('',(0.707106781186547,8.65956056235493E-17,-0.707106781186547));
#35683=DIRECTION('center_axis',(0.,0.,-1.));
#35684=DIRECTION('ref_axis',(1.,0.,0.));
#35685=DIRECTION('center_axis',(0.,0.,-1.));
#35686=DIRECTION('ref_axis',(1.,0.,0.));
#35687=DIRECTION('',(0.,0.,-1.));
#35688=DIRECTION('center_axis',(0.,0.,1.));
#35689=DIRECTION('ref_axis',(1.,0.,0.));
#35690=DIRECTION('',(0.707106781186548,8.65956056235494E-17,-0.707106781186548));
#35691=DIRECTION('center_axis',(0.,0.,-1.));
#35692=DIRECTION('ref_axis',(1.,0.,0.));
#35693=DIRECTION('center_axis',(0.,0.,-1.));
#35694=DIRECTION('ref_axis',(1.,0.,0.));
#35695=DIRECTION('',(0.,0.,-1.));
#35696=DIRECTION('center_axis',(0.,0.,1.));
#35697=DIRECTION('ref_axis',(1.,0.,0.));
#35698=DIRECTION('',(0.707106781186547,8.65956056235493E-17,-0.707106781186547));
#35699=DIRECTION('center_axis',(0.,0.,1.));
#35700=DIRECTION('ref_axis',(1.,0.,0.));
#35701=DIRECTION('',(0.707106781186547,8.65956056235493E-17,-0.707106781186547));
#35702=DIRECTION('center_axis',(0.,0.,1.));
#35703=DIRECTION('ref_axis',(1.,0.,0.));
#35704=DIRECTION('',(0.707106781186547,8.65956056235493E-17,-0.707106781186547));
#35705=DIRECTION('center_axis',(0.,0.,1.));
#35706=DIRECTION('ref_axis',(1.,0.,0.));
#35707=DIRECTION('',(0.707106781186548,8.65956056235493E-17,-0.707106781186548));
#35708=DIRECTION('center_axis',(0.,0.,1.));
#35709=DIRECTION('ref_axis',(1.,0.,0.));
#35710=DIRECTION('',(0.707106781186549,8.65956056235495E-17,-0.707106781186546));
#35711=DIRECTION('center_axis',(0.,0.,1.));
#35712=DIRECTION('ref_axis',(1.,0.,0.));
#35713=DIRECTION('',(0.707106781186547,8.65956056235493E-17,-0.707106781186547));
#35714=DIRECTION('center_axis',(0.,0.,1.));
#35715=DIRECTION('ref_axis',(1.,0.,0.));
#35716=DIRECTION('',(0.707106781186549,8.65956056235495E-17,-0.707106781186546));
#35717=DIRECTION('center_axis',(0.,0.,1.));
#35718=DIRECTION('ref_axis',(1.,0.,0.));
#35719=DIRECTION('',(0.707106781186549,8.65956056235495E-17,-0.707106781186546));
#35720=DIRECTION('center_axis',(0.,0.,1.));
#35721=DIRECTION('ref_axis',(1.,0.,0.));
#35722=DIRECTION('',(0.707106781186548,8.65956056235493E-17,-0.707106781186548));
#35723=DIRECTION('center_axis',(0.,0.,1.));
#35724=DIRECTION('ref_axis',(1.,0.,0.));
#35725=DIRECTION('',(0.707106781186548,8.65956056235493E-17,-0.707106781186548));
#35726=DIRECTION('center_axis',(0.,0.,1.));
#35727=DIRECTION('ref_axis',(1.,0.,0.));
#35728=DIRECTION('',(0.707106781186547,8.65956056235493E-17,-0.707106781186547));
#35729=DIRECTION('center_axis',(0.,0.,1.));
#35730=DIRECTION('ref_axis',(1.,0.,0.));
#35731=DIRECTION('',(0.707106781186548,8.65956056235493E-17,-0.707106781186548));
#35732=DIRECTION('center_axis',(0.,0.,1.));
#35733=DIRECTION('ref_axis',(1.,0.,0.));
#35734=DIRECTION('',(0.707106781186549,8.65956056235495E-17,-0.707106781186546));
#35735=DIRECTION('center_axis',(0.,0.,1.));
#35736=DIRECTION('ref_axis',(1.,0.,0.));
#35737=DIRECTION('',(0.707106781186549,8.65956056235495E-17,-0.707106781186546));
#35738=DIRECTION('center_axis',(0.,0.,1.));
#35739=DIRECTION('ref_axis',(1.,0.,0.));
#35740=DIRECTION('',(0.707106781186549,8.65956056235495E-17,-0.707106781186546));
#35741=DIRECTION('center_axis',(0.,0.,1.));
#35742=DIRECTION('ref_axis',(1.,0.,0.));
#35743=DIRECTION('',(0.707106781186549,8.65956056235495E-17,-0.707106781186546));
#35744=DIRECTION('center_axis',(0.,0.,1.));
#35745=DIRECTION('ref_axis',(1.,0.,0.));
#35746=DIRECTION('',(0.707106781186548,8.65956056235493E-17,-0.707106781186548));
#35747=DIRECTION('center_axis',(0.,0.,1.));
#35748=DIRECTION('ref_axis',(1.,0.,0.));
#35749=DIRECTION('',(0.707106781186548,8.65956056235493E-17,-0.707106781186548));
#35750=DIRECTION('center_axis',(0.,0.,1.));
#35751=DIRECTION('ref_axis',(1.,0.,0.));
#35752=DIRECTION('',(0.707106781186547,8.65956056235493E-17,-0.707106781186547));
#35753=DIRECTION('center_axis',(0.,0.,1.));
#35754=DIRECTION('ref_axis',(1.,0.,0.));
#35755=DIRECTION('',(0.707106781186547,8.65956056235493E-17,-0.707106781186547));
#35756=DIRECTION('center_axis',(0.,0.,1.));
#35757=DIRECTION('ref_axis',(1.,0.,0.));
#35758=DIRECTION('',(0.707106781186548,8.65956056235493E-17,-0.707106781186548));
#35759=DIRECTION('center_axis',(0.,0.,1.));
#35760=DIRECTION('ref_axis',(1.,0.,0.));
#35761=DIRECTION('',(0.707106781186548,8.65956056235493E-17,-0.707106781186548));
#35762=DIRECTION('center_axis',(0.,0.,1.));
#35763=DIRECTION('ref_axis',(1.,0.,0.));
#35764=DIRECTION('',(0.707106781186547,8.65956056235493E-17,-0.707106781186547));
#35765=DIRECTION('center_axis',(0.,0.,-1.));
#35766=DIRECTION('ref_axis',(1.,0.,0.));
#35767=DIRECTION('center_axis',(0.,0.,-1.));
#35768=DIRECTION('ref_axis',(1.,0.,0.));
#35769=DIRECTION('',(0.,0.,-1.));
#35770=DIRECTION('center_axis',(0.,0.,1.));
#35771=DIRECTION('ref_axis',(1.,0.,0.));
#35772=DIRECTION('',(0.707106781186549,8.65956056235495E-17,-0.707106781186546));
#35773=DIRECTION('center_axis',(0.,0.,-1.));
#35774=DIRECTION('ref_axis',(1.,0.,0.));
#35775=DIRECTION('center_axis',(0.,0.,-1.));
#35776=DIRECTION('ref_axis',(1.,0.,0.));
#35777=DIRECTION('',(0.,0.,-1.));
#35778=DIRECTION('center_axis',(0.,0.,1.));
#35779=DIRECTION('ref_axis',(1.,0.,0.));
#35780=DIRECTION('',(0.,0.,1.));
#35781=DIRECTION('center_axis',(0.,-1.,0.));
#35782=DIRECTION('ref_axis',(1.,0.,0.));
#35783=DIRECTION('axis',(0.,0.,1.));
#35784=DIRECTION('refdir',(1.,0.,0.));
#35785=DIRECTION('center_axis',(0.,-1.,0.));
#35786=DIRECTION('ref_axis',(1.,0.,0.));
#35787=DIRECTION('center_axis',(0.,-1.,0.));
#35788=DIRECTION('ref_axis',(1.,0.,0.));
#35789=DIRECTION('',(0.707106781186543,0.707106781186552,8.65956056235487E-17));
#35790=DIRECTION('center_axis',(0.,1.,0.));
#35791=DIRECTION('ref_axis',(1.,0.,0.));
#35792=DIRECTION('center_axis',(0.,-1.,0.));
#35793=DIRECTION('ref_axis',(1.,0.,0.));
#35794=DIRECTION('center_axis',(0.,-1.,0.));
#35795=DIRECTION('ref_axis',(1.,0.,0.));
#35796=DIRECTION('center_axis',(0.,-1.,0.));
#35797=DIRECTION('ref_axis',(1.,0.,0.));
#35798=DIRECTION('',(0.707106781186543,0.707106781186552,8.65956056235487E-17));
#35799=DIRECTION('center_axis',(0.,1.,0.));
#35800=DIRECTION('ref_axis',(1.,0.,0.));
#35801=DIRECTION('center_axis',(0.,-1.,0.));
#35802=DIRECTION('ref_axis',(1.,0.,0.));
#35803=DIRECTION('center_axis',(0.,-1.,0.));
#35804=DIRECTION('ref_axis',(1.,0.,0.));
#35805=DIRECTION('center_axis',(0.,1.,0.));
#35806=DIRECTION('ref_axis',(1.,0.,0.));
#35807=DIRECTION('',(0.,1.,0.));
#35808=DIRECTION('center_axis',(0.,1.,0.));
#35809=DIRECTION('ref_axis',(1.,0.,0.));
#35810=DIRECTION('center_axis',(0.,-0.707106781186543,-0.707106781186553));
#35811=DIRECTION('ref_axis',(-1.,0.,0.));
#35812=DIRECTION('',(-1.,0.,0.));
#35813=DIRECTION('',(-1.25607396694701E-14,0.707106781186552,-0.707106781186542));
#35814=DIRECTION('',(1.,0.,0.));
#35815=DIRECTION('',(-0.577350269189618,0.577350269189634,-0.577350269189625));
#35816=DIRECTION('',(-0.577350269189622,-0.577350269189632,0.577350269189624));
#35817=DIRECTION('',(-1.,0.,0.));
#35818=DIRECTION('center_axis',(0.,1.,0.));
#35819=DIRECTION('ref_axis',(1.,0.,0.));
#35820=DIRECTION('',(0.,1.,0.));
#35821=DIRECTION('center_axis',(0.,1.,0.));
#35822=DIRECTION('ref_axis',(1.,0.,0.));
#35823=DIRECTION('center_axis',(-0.577350269189627,-0.577350269189626,-0.577350269189624));
#35824=DIRECTION('ref_axis',(-0.707106781186546,0.,0.707106781186549));
#35825=DIRECTION('',(0.707106781186547,-0.707106781186547,0.));
#35826=DIRECTION('',(-0.707106781186546,0.,0.707106781186549));
#35827=DIRECTION('center_axis',(-0.577350269189627,0.577350269189627,-0.577350269189624));
#35828=DIRECTION('ref_axis',(-0.707106781186546,0.,0.707106781186549));
#35829=DIRECTION('',(0.,0.707106781186546,0.707106781186549));
#35830=DIRECTION('',(0.707106781186546,0.,-0.707106781186549));
#35831=DIRECTION('',(-0.707106781186548,-0.707106781186548,0.));
#35832=DIRECTION('center_axis',(-0.707106781186549,0.,-0.707106781186546));
#35833=DIRECTION('ref_axis',(-0.707106781186546,0.,0.707106781186549));
#35834=DIRECTION('',(0.,1.,0.));
#35835=DIRECTION('',(0.,-1.,0.));
#35836=DIRECTION('center_axis',(-0.707106781186548,0.707106781186548,0.));
#35837=DIRECTION('ref_axis',(0.,0.,1.));
#35838=DIRECTION('',(0.577350269189626,0.577350269189626,-0.577350269189626));
#35839=DIRECTION('',(0.,0.,-1.));
#35840=DIRECTION('',(0.,0.,1.));
#35841=DIRECTION('',(0.577350269189626,0.577350269189626,0.577350269189626));
#35842=DIRECTION('center_axis',(0.577350269189628,0.577350269189628,-0.577350269189621));
#35843=DIRECTION('ref_axis',(-0.707106781186543,0.,-0.707106781186552));
#35844=DIRECTION('',(-0.707106781186548,0.707106781186548,0.));
#35845=DIRECTION('',(0.707106781186543,0.,0.707106781186552));
#35846=DIRECTION('',(6.28036983473511E-15,-0.707106781186546,-0.707106781186549));
#35847=DIRECTION('center_axis',(0.707106781186552,0.,-0.707106781186543));
#35848=DIRECTION('ref_axis',(-0.707106781186543,0.,-0.707106781186552));
#35849=DIRECTION('',(0.,1.,0.));
#35850=DIRECTION('',(0.,-1.,0.));
#35851=DIRECTION('',(-0.57735026918962,-0.57735026918963,-0.577350269189627));
#35852=DIRECTION('center_axis',(0.,0.707106781186549,-0.707106781186546));
#35853=DIRECTION('ref_axis',(-1.,0.,0.));
#35854=DIRECTION('',(1.,0.,0.));
#35855=DIRECTION('',(-1.,0.,0.));
#35856=DIRECTION('center_axis',(0.707106781186548,0.707106781186548,0.));
#35857=DIRECTION('ref_axis',(0.,0.,-1.));
#35858=DIRECTION('',(0.577350269189626,-0.577350269189626,-0.577350269189626));
#35859=DIRECTION('',(0.,0.,-1.));
#35860=DIRECTION('',(0.,0.,1.));
#35861=DIRECTION('',(0.577350269189626,-0.577350269189626,0.577350269189626));
#35862=DIRECTION('center_axis',(-0.707106781186548,-0.707106781186548,0.));
#35863=DIRECTION('ref_axis',(0.,0.,1.));
#35864=DIRECTION('',(-0.577350269189626,0.577350269189626,-0.577350269189626));
#35865=DIRECTION('',(0.,0.,-1.));
#35866=DIRECTION('',(0.,0.,1.));
#35867=DIRECTION('',(-0.577350269189629,0.577350269189629,0.577350269189619));
#35868=DIRECTION('center_axis',(0.,1.,0.));
#35869=DIRECTION('ref_axis',(-1.,0.,0.));
#35870=DIRECTION('',(-1.,0.,0.));
#35871=DIRECTION('center_axis',(0.,-1.,0.));
#35872=DIRECTION('ref_axis',(1.,0.,0.));
#35873=DIRECTION('center_axis',(0.,-1.,0.));
#35874=DIRECTION('ref_axis',(1.,0.,0.));
#35875=DIRECTION('center_axis',(-1.,0.,0.));
#35876=DIRECTION('ref_axis',(0.,-1.,0.));
#35877=DIRECTION('',(0.,-1.,0.));
#35878=DIRECTION('center_axis',(1.,0.,0.));
#35879=DIRECTION('ref_axis',(0.,0.,-1.));
#35880=DIRECTION('center_axis',(1.,0.,0.));
#35881=DIRECTION('ref_axis',(0.,0.,-1.));
#35882=DIRECTION('center_axis',(-0.707106781186548,0.,0.707106781186548));
#35883=DIRECTION('ref_axis',(0.707106781186548,0.,0.707106781186548));
#35884=DIRECTION('',(-0.577350269189622,-0.577350269189633,-0.577350269189622));
#35885=DIRECTION('',(0.,1.,0.));
#35886=DIRECTION('',(-0.577350269189626,0.577350269189626,-0.577350269189626));
#35887=DIRECTION('center_axis',(0.,-0.707106781186541,0.707106781186554));
#35888=DIRECTION('ref_axis',(1.,0.,0.));
#35889=DIRECTION('',(1.,0.,0.));
#35890=DIRECTION('',(0.,0.707106781186554,0.707106781186541));
#35891=DIRECTION('',(-1.,0.,0.));
#35892=DIRECTION('center_axis',(0.,0.,1.));
#35893=DIRECTION('ref_axis',(1.,0.,0.));
#35894=DIRECTION('center_axis',(0.577350269189629,-0.577350269189619,0.577350269189629));
#35895=DIRECTION('ref_axis',(0.707106781186548,0.,-0.707106781186548));
#35896=DIRECTION('',(-0.707106781186541,-0.707106781186554,0.));
#35897=DIRECTION('',(0.707106781186548,0.,-0.707106781186548));
#35898=DIRECTION('center_axis',(0.707106781186554,-0.707106781186541,0.));
#35899=DIRECTION('ref_axis',(0.,0.,-1.));
#35900=DIRECTION('',(0.,0.,1.));
#35901=DIRECTION('',(0.,0.,-1.));
#35902=DIRECTION('center_axis',(0.,0.707106781186548,0.707106781186548));
#35903=DIRECTION('ref_axis',(1.,0.,0.));
#35904=DIRECTION('',(1.,0.,0.));
#35905=DIRECTION('',(0.577350269189626,0.577350269189626,-0.577350269189626));
#35906=DIRECTION('center_axis',(0.707106781186548,0.,0.707106781186548));
#35907=DIRECTION('ref_axis',(0.707106781186548,0.,-0.707106781186548));
#35908=DIRECTION('',(0.,-1.,0.));
#35909=DIRECTION('',(0.,1.,0.));
#35910=DIRECTION('center_axis',(1.,0.,0.));
#35911=DIRECTION('ref_axis',(0.,1.,0.));
#35912=DIRECTION('center_axis',(-1.,0.,0.));
#35913=DIRECTION('ref_axis',(0.,0.,-1.));
#35914=DIRECTION('center_axis',(0.,0.,1.));
#35915=DIRECTION('ref_axis',(1.,0.,0.));
#35916=DIRECTION('center_axis',(0.,0.,-1.));
#35917=DIRECTION('ref_axis',(1.,0.,0.));
#35918=DIRECTION('center_axis',(0.,1.,0.));
#35919=DIRECTION('ref_axis',(1.,0.,0.));
#35920=DIRECTION('center_axis',(0.,-1.,0.));
#35921=DIRECTION('ref_axis',(1.,0.,0.));
#35922=DIRECTION('center_axis',(0.,1.,0.));
#35923=DIRECTION('ref_axis',(1.,0.,0.));
#35924=DIRECTION('center_axis',(0.,-1.,0.));
#35925=DIRECTION('ref_axis',(1.,0.,0.));
#35926=DIRECTION('center_axis',(0.,1.,0.));
#35927=DIRECTION('ref_axis',(1.,0.,0.));
#35928=DIRECTION('',(0.,1.,0.));
#35929=DIRECTION('center_axis',(0.,1.,0.));
#35930=DIRECTION('ref_axis',(1.,0.,0.));
#35931=DIRECTION('',(0.,1.,0.));
#35932=DIRECTION('center_axis',(0.,0.,-1.));
#35933=DIRECTION('ref_axis',(1.,0.,0.));
#35934=DIRECTION('',(0.,0.,-1.));
#35935=DIRECTION('center_axis',(0.,0.,-1.));
#35936=DIRECTION('ref_axis',(1.,0.,0.));
#35937=DIRECTION('',(0.,0.,-1.));
#35938=DIRECTION('center_axis',(0.,0.,-1.));
#35939=DIRECTION('ref_axis',(1.,0.,0.));
#35940=DIRECTION('center_axis',(0.,0.,1.));
#35941=DIRECTION('ref_axis',(1.,0.,0.));
#35942=DIRECTION('center_axis',(1.,0.,0.));
#35943=DIRECTION('ref_axis',(0.,0.,-1.));
#35944=DIRECTION('',(1.,0.,0.));
#35945=DIRECTION('',(1.,0.,0.));
#35946=DIRECTION('center_axis',(1.,0.,0.));
#35947=DIRECTION('ref_axis',(0.,0.,-1.));
#35948=DIRECTION('center_axis',(1.,0.,0.));
#35949=DIRECTION('ref_axis',(0.,0.,-1.));
#35950=DIRECTION('center_axis',(-1.,0.,0.));
#35951=DIRECTION('ref_axis',(0.,0.,-1.));
#35952=DIRECTION('',(-1.,0.,0.));
#35953=DIRECTION('center_axis',(0.,-1.,0.));
#35954=DIRECTION('ref_axis',(1.,0.,0.));
#35955=DIRECTION('axis',(0.,0.,1.));
#35956=DIRECTION('refdir',(1.,0.,0.));
#35957=DIRECTION('center_axis',(-0.707106781186548,-0.707106781186548,0.));
#35958=DIRECTION('ref_axis',(-3.33066907387547E-16,3.33066907387547E-16,
1.));
#35959=DIRECTION('center_axis',(-0.707106781186548,-0.707106781186548,0.));
#35960=DIRECTION('ref_axis',(-3.33066907387547E-16,3.33066907387547E-16,
1.));
#35961=DIRECTION('',(0.707106781186548,0.707106781186548,0.));
#35962=DIRECTION('center_axis',(-0.707106781186548,-0.707106781186548,0.));
#35963=DIRECTION('ref_axis',(-3.33066907387547E-16,3.33066907387547E-16,
1.));
#35964=DIRECTION('center_axis',(-0.707106781186548,-0.707106781186548,0.));
#35965=DIRECTION('ref_axis',(-3.33066907387547E-16,3.33066907387547E-16,
1.));
#35966=DIRECTION('',(0.706176214723467,-0.706176214723467,0.0512865237432823));
#35967=DIRECTION('center_axis',(0.,0.,1.));
#35968=DIRECTION('ref_axis',(1.,0.,0.));
#35969=DIRECTION('center_axis',(0.,-1.,0.));
#35970=DIRECTION('ref_axis',(-1.,0.,0.));
#35971=DIRECTION('center_axis',(0.,0.,-1.));
#35972=DIRECTION('ref_axis',(1.,0.,0.));
#35973=DIRECTION('center_axis',(0.0706021761589144,-0.0018421410289849,
-0.997502851744322));
#35974=DIRECTION('ref_axis',(0.663761346011967,-0.746379469565852,0.0483586905424292));
#35975=DIRECTION('center_axis',(0.0706021761589144,-0.0018421410289849,
-0.997502851744322));
#35976=DIRECTION('ref_axis',(0.663761346011967,-0.746379469565852,0.0483586905424292));
#35977=DIRECTION('center_axis',(0.77193023561705,-0.635707252861099,0.));
#35978=DIRECTION('ref_axis',(3.20476749376334E-17,3.89150338528406E-17,
1.));
#35979=DIRECTION('center_axis',(0.77193023561705,-0.635707252861099,1.13428418954078E-16));
#35980=DIRECTION('ref_axis',(-5.55111512312578E-17,1.11022302462516E-16,
1.));
#35981=DIRECTION('',(-0.77193023561705,0.635707252861099,0.));
#35982=DIRECTION('center_axis',(0.77193023561705,-0.635707252861099,1.13428418954078E-16));
#35983=DIRECTION('ref_axis',(-5.55111512312578E-17,1.11022302462516E-16,
1.));
#35984=DIRECTION('',(-0.635023434538235,-0.771099884796429,-0.0463703057375958));
#35985=DIRECTION('center_axis',(0.,0.,1.));
#35986=DIRECTION('ref_axis',(1.,0.,0.));
#35987=DIRECTION('center_axis',(0.,-1.,0.));
#35988=DIRECTION('ref_axis',(-1.,0.,0.));
#35989=DIRECTION('center_axis',(0.,0.,-1.));
#35990=DIRECTION('ref_axis',(1.,0.,0.));
#35991=DIRECTION('center_axis',(0.070602176935317,0.00184214179195253,-0.99750285168796));
#35992=DIRECTION('ref_axis',(0.997163482507387,0.0260178454018302,0.0706262052951131));
#35993=DIRECTION('center_axis',(0.070602176935317,0.00184214179195253,-0.99750285168796));
#35994=DIRECTION('ref_axis',(0.997163482507387,0.0260178454018302,0.0706262052951131));
#35995=DIRECTION('axis',(0.,0.,1.));
#35996=DIRECTION('refdir',(1.,0.,0.));
#35997=DIRECTION('center_axis',(1.,0.,0.));
#35998=DIRECTION('ref_axis',(0.,1.,0.));
#35999=DIRECTION('',(-1.,0.,0.));
#36000=DIRECTION('center_axis',(1.,0.,0.));
#36001=DIRECTION('ref_axis',(0.,1.,0.));
#36002=DIRECTION('center_axis',(1.,0.,0.));
#36003=DIRECTION('ref_axis',(0.,1.,0.));
#36004=DIRECTION('',(-1.,0.,0.));
#36005=DIRECTION('center_axis',(1.,0.,0.));
#36006=DIRECTION('ref_axis',(0.,1.,0.));
#36007=DIRECTION('',(-1.,0.,0.));
#36008=DIRECTION('center_axis',(1.,0.,0.));
#36009=DIRECTION('ref_axis',(0.,1.,0.));
#36010=DIRECTION('',(-1.,0.,0.));
#36011=DIRECTION('center_axis',(1.,0.,0.));
#36012=DIRECTION('ref_axis',(0.,1.,0.));
#36013=DIRECTION('',(-1.,0.,0.));
#36014=DIRECTION('center_axis',(1.,0.,0.));
#36015=DIRECTION('ref_axis',(0.,1.,0.));
#36016=DIRECTION('',(-1.,0.,0.));
#36017=DIRECTION('center_axis',(1.,0.,0.));
#36018=DIRECTION('ref_axis',(0.,1.,0.));
#36019=DIRECTION('',(-1.,0.,0.));
#36020=DIRECTION('center_axis',(1.,0.,0.));
#36021=DIRECTION('ref_axis',(0.,1.,0.));
#36022=DIRECTION('',(-1.,0.,0.));
#36023=DIRECTION('center_axis',(1.,0.,0.));
#36024=DIRECTION('ref_axis',(0.,1.,0.));
#36025=DIRECTION('',(-1.,0.,0.));
#36026=DIRECTION('center_axis',(1.,0.,0.));
#36027=DIRECTION('ref_axis',(0.,1.,0.));
#36028=DIRECTION('',(-1.,0.,0.));
#36029=DIRECTION('center_axis',(1.,0.,0.));
#36030=DIRECTION('ref_axis',(0.,1.,5.66627894982857E-14));
#36031=DIRECTION('',(1.,0.,0.));
#36032=DIRECTION('center_axis',(1.,0.,0.));
#36033=DIRECTION('ref_axis',(0.,1.,5.66627894982857E-14));
#36034=DIRECTION('center_axis',(1.,0.,0.));
#36035=DIRECTION('ref_axis',(0.,1.,5.66627894982857E-14));
#36036=DIRECTION('',(1.,0.,0.));
#36037=DIRECTION('center_axis',(1.,0.,0.));
#36038=DIRECTION('ref_axis',(0.,1.,5.66627894982857E-14));
#36039=DIRECTION('',(1.,0.,0.));
#36040=DIRECTION('center_axis',(1.,0.,0.));
#36041=DIRECTION('ref_axis',(0.,1.,5.66627894982857E-14));
#36042=DIRECTION('',(1.,0.,0.));
#36043=DIRECTION('center_axis',(1.,0.,0.));
#36044=DIRECTION('ref_axis',(0.,1.,5.66627894982857E-14));
#36045=DIRECTION('',(1.,0.,0.));
#36046=DIRECTION('center_axis',(1.,0.,0.));
#36047=DIRECTION('ref_axis',(0.,1.,5.66627894982857E-14));
#36048=DIRECTION('',(1.,0.,0.));
#36049=DIRECTION('center_axis',(1.,0.,0.));
#36050=DIRECTION('ref_axis',(0.,1.,5.66627894982857E-14));
#36051=DIRECTION('',(1.,0.,0.));
#36052=DIRECTION('center_axis',(1.,0.,0.));
#36053=DIRECTION('ref_axis',(0.,1.,5.66627894982857E-14));
#36054=DIRECTION('',(1.,0.,0.));
#36055=DIRECTION('center_axis',(1.,0.,0.));
#36056=DIRECTION('ref_axis',(0.,1.,5.66627894982857E-14));
#36057=DIRECTION('',(1.,0.,0.));
#36058=DIRECTION('center_axis',(1.,0.,0.));
#36059=DIRECTION('ref_axis',(0.,1.,5.66627894982857E-14));
#36060=DIRECTION('',(1.,0.,0.));
#36061=DIRECTION('center_axis',(1.,0.,0.));
#36062=DIRECTION('ref_axis',(0.,0.,-1.));
#36063=DIRECTION('center_axis',(-1.,0.,0.));
#36064=DIRECTION('ref_axis',(0.,1.,0.));
#36065=DIRECTION('center_axis',(-1.,0.,0.));
#36066=DIRECTION('ref_axis',(0.,1.,0.));
#36067=DIRECTION('center_axis',(1.,0.,0.));
#36068=DIRECTION('ref_axis',(0.,0.,-1.));
#36069=DIRECTION('center_axis',(1.,0.,0.));
#36070=DIRECTION('ref_axis',(0.,1.,0.));
#36071=DIRECTION('center_axis',(1.,0.,0.));
#36072=DIRECTION('ref_axis',(0.,1.,0.));
#36073=DIRECTION('center_axis',(-1.,0.,0.));
#36074=DIRECTION('ref_axis',(0.,1.,5.66627894982857E-14));
#36075=DIRECTION('center_axis',(1.,0.,0.));
#36076=DIRECTION('ref_axis',(0.,1.,5.66627894982857E-14));
#36077=DIRECTION('center_axis',(0.,-0.479608080343199,0.877482814230291));
#36078=DIRECTION('ref_axis',(0.,-0.877482814230291,-0.479608080343199));
#36079=DIRECTION('',(-1.,0.,0.));
#36080=DIRECTION('',(0.,-0.877482814230291,-0.479608080343199));
#36081=DIRECTION('',(1.,0.,0.));
#36082=DIRECTION('',(0.,-0.877482814230291,-0.479608080343199));
#36083=DIRECTION('center_axis',(1.,0.,0.));
#36084=DIRECTION('ref_axis',(0.,-0.17364817766693,-0.984807753012208));
#36085=DIRECTION('center_axis',(-1.,0.,0.));
#36086=DIRECTION('ref_axis',(0.,1.,0.));
#36087=DIRECTION('',(0.,0.660528501019527,-0.750800971856654));
#36088=DIRECTION('center_axis',(0.,-0.750800971856655,-0.660528501019527));
#36089=DIRECTION('ref_axis',(0.,0.660528501019527,-0.750800971856654));
#36090=DIRECTION('',(1.,0.,0.));
#36091=DIRECTION('',(0.,0.660528501019527,-0.750800971856654));
#36092=DIRECTION('center_axis',(1.,0.,0.));
#36093=DIRECTION('ref_axis',(0.,-0.17364817766693,-0.984807753012208));
#36094=DIRECTION('center_axis',(1.,0.,0.));
#36095=DIRECTION('ref_axis',(0.,1.,0.));
#36096=DIRECTION('center_axis',(0.,-0.319948464304144,0.947434947734893));
#36097=DIRECTION('ref_axis',(0.,-0.947434947734893,-0.319948464304144));
#36098=DIRECTION('',(-1.,0.,0.));
#36099=DIRECTION('',(0.,-0.947434947734893,-0.319948464304144));
#36100=DIRECTION('',(1.,0.,0.));
#36101=DIRECTION('',(0.,-0.947434947734893,-0.319948464304144));
#36102=DIRECTION('center_axis',(1.,0.,0.));
#36103=DIRECTION('ref_axis',(0.,-0.342020143325669,-0.939692620785908));
#36104=DIRECTION('center_axis',(-1.,0.,0.));
#36105=DIRECTION('ref_axis',(0.,1.,0.));
#36106=DIRECTION('',(0.,0.520118368336093,-0.854094188552644));
#36107=DIRECTION('center_axis',(0.,-0.854094188552644,-0.520118368336093));
#36108=DIRECTION('ref_axis',(0.,0.520118368336093,-0.854094188552644));
#36109=DIRECTION('',(1.,0.,0.));
#36110=DIRECTION('',(0.,0.520118368336093,-0.854094188552644));
#36111=DIRECTION('center_axis',(1.,0.,0.));
#36112=DIRECTION('ref_axis',(0.,-0.342020143325669,-0.939692620785908));
#36113=DIRECTION('center_axis',(1.,0.,0.));
#36114=DIRECTION('ref_axis',(0.,1.,0.));
#36115=DIRECTION('center_axis',(0.,-0.150567376078943,0.988599749777787));
#36116=DIRECTION('ref_axis',(0.,-0.988599749777787,-0.150567376078943));
#36117=DIRECTION('',(-1.,0.,0.));
#36118=DIRECTION('',(0.,-0.988599749777787,-0.150567376078943));
#36119=DIRECTION('',(1.,0.,0.));
#36120=DIRECTION('',(0.,-0.988599749777787,-0.150567376078943));
#36121=DIRECTION('center_axis',(1.,0.,0.));
#36122=DIRECTION('ref_axis',(0.,-0.5,-0.866025403784438));
#36123=DIRECTION('center_axis',(-1.,0.,0.));
#36124=DIRECTION('ref_axis',(0.,1.,0.));
#36125=DIRECTION('',(0.,0.363904702223362,-0.931436185521974));
#36126=DIRECTION('center_axis',(0.,-0.931436185521975,-0.363904702223362));
#36127=DIRECTION('ref_axis',(0.,0.363904702223362,-0.931436185521975));
#36128=DIRECTION('',(1.,0.,0.));
#36129=DIRECTION('',(0.,0.363904702223362,-0.931436185521974));
#36130=DIRECTION('center_axis',(1.,0.,0.));
#36131=DIRECTION('ref_axis',(0.,-0.5,-0.866025403784438));
#36132=DIRECTION('center_axis',(1.,0.,0.));
#36133=DIRECTION('ref_axis',(0.,1.,0.));
#36134=DIRECTION('center_axis',(0.,0.0233886256776475,0.999726448679293));
#36135=DIRECTION('ref_axis',(0.,-0.999726448679293,0.0233886256776475));
#36136=DIRECTION('',(-1.,0.,0.));
#36137=DIRECTION('',(0.,-0.999726448679293,0.0233886256776475));
#36138=DIRECTION('',(1.,0.,0.));
#36139=DIRECTION('',(0.,-0.999726448679293,0.0233886256776475));
#36140=DIRECTION('center_axis',(1.,0.,0.));
#36141=DIRECTION('ref_axis',(0.,-0.64278760968654,-0.766044443118978));
#36142=DIRECTION('center_axis',(-1.,0.,0.));
#36143=DIRECTION('ref_axis',(0.,1.,0.));
#36144=DIRECTION('',(0.,0.196633975878238,-0.980476965323672));
#36145=DIRECTION('center_axis',(0.,-0.980476965323672,-0.196633975878238));
#36146=DIRECTION('ref_axis',(0.,0.196633975878238,-0.980476965323672));
#36147=DIRECTION('',(1.,0.,0.));
#36148=DIRECTION('',(0.,0.196633975878238,-0.980476965323672));
#36149=DIRECTION('center_axis',(1.,0.,0.));
#36150=DIRECTION('ref_axis',(0.,-0.64278760968654,-0.766044443118978));
#36151=DIRECTION('center_axis',(1.,0.,0.));
#36152=DIRECTION('ref_axis',(0.,1.,0.));
#36153=DIRECTION('center_axis',(0.,0.196633975878239,0.980476965323672));
#36154=DIRECTION('ref_axis',(0.,-0.980476965323671,0.196633975878239));
#36155=DIRECTION('',(-1.,0.,0.));
#36156=DIRECTION('',(0.,-0.980476965323671,0.196633975878239));
#36157=DIRECTION('',(1.,0.,0.));
#36158=DIRECTION('',(0.,-0.980476965323671,0.196633975878239));
#36159=DIRECTION('center_axis',(1.,0.,0.));
#36160=DIRECTION('ref_axis',(0.,-0.766044443118978,-0.642787609686539));
#36161=DIRECTION('center_axis',(-1.,0.,0.));
#36162=DIRECTION('ref_axis',(0.,1.,0.));
#36163=DIRECTION('',(0.,0.0233886256776471,-0.999726448679293));
#36164=DIRECTION('center_axis',(0.,-0.999726448679293,-0.0233886256776472));
#36165=DIRECTION('ref_axis',(0.,0.0233886256776472,-0.999726448679293));
#36166=DIRECTION('',(1.,0.,0.));
#36167=DIRECTION('',(0.,0.0233886256776471,-0.999726448679293));
#36168=DIRECTION('center_axis',(1.,0.,0.));
#36169=DIRECTION('ref_axis',(0.,-0.766044443118978,-0.642787609686539));
#36170=DIRECTION('center_axis',(1.,0.,0.));
#36171=DIRECTION('ref_axis',(0.,1.,0.));
#36172=DIRECTION('center_axis',(0.,0.363904702223362,0.931436185521974));
#36173=DIRECTION('ref_axis',(0.,-0.931436185521974,0.363904702223362));
#36174=DIRECTION('',(-1.,0.,0.));
#36175=DIRECTION('',(0.,-0.931436185521974,0.363904702223362));
#36176=DIRECTION('',(1.,0.,0.));
#36177=DIRECTION('',(0.,-0.931436185521974,0.363904702223362));
#36178=DIRECTION('center_axis',(1.,0.,0.));
#36179=DIRECTION('ref_axis',(0.,-0.866025403784439,-0.5));
#36180=DIRECTION('center_axis',(-1.,0.,0.));
#36181=DIRECTION('ref_axis',(0.,1.,0.));
#36182=DIRECTION('',(0.,-0.150567376078944,-0.988599749777787));
#36183=DIRECTION('center_axis',(0.,-0.988599749777787,0.150567376078944));
#36184=DIRECTION('ref_axis',(0.,-0.150567376078944,-0.988599749777787));
#36185=DIRECTION('',(1.,0.,0.));
#36186=DIRECTION('',(0.,-0.150567376078944,-0.988599749777787));
#36187=DIRECTION('center_axis',(1.,0.,0.));
#36188=DIRECTION('ref_axis',(0.,-0.866025403784439,-0.5));
#36189=DIRECTION('center_axis',(1.,0.,0.));
#36190=DIRECTION('ref_axis',(0.,1.,0.));
#36191=DIRECTION('center_axis',(0.,0.520118368336095,0.854094188552644));
#36192=DIRECTION('ref_axis',(0.,-0.854094188552644,0.520118368336094));
#36193=DIRECTION('',(-1.,0.,0.));
#36194=DIRECTION('',(0.,-0.854094188552644,0.520118368336095));
#36195=DIRECTION('',(1.,0.,0.));
#36196=DIRECTION('',(0.,-0.854094188552644,0.520118368336095));
#36197=DIRECTION('center_axis',(1.,0.,0.));
#36198=DIRECTION('ref_axis',(0.,-0.939692620785909,-0.342020143325668));
#36199=DIRECTION('center_axis',(-1.,0.,0.));
#36200=DIRECTION('ref_axis',(0.,1.,0.));
#36201=DIRECTION('',(0.,-0.319948464304145,-0.947434947734893));
#36202=DIRECTION('center_axis',(0.,-0.947434947734893,0.319948464304145));
#36203=DIRECTION('ref_axis',(0.,-0.319948464304145,-0.947434947734893));
#36204=DIRECTION('',(1.,0.,0.));
#36205=DIRECTION('',(0.,-0.319948464304145,-0.947434947734893));
#36206=DIRECTION('center_axis',(1.,0.,0.));
#36207=DIRECTION('ref_axis',(0.,-0.939692620785909,-0.342020143325668));
#36208=DIRECTION('center_axis',(1.,0.,0.));
#36209=DIRECTION('ref_axis',(0.,1.,0.));
#36210=DIRECTION('center_axis',(0.,0.660528501019527,0.750800971856654));
#36211=DIRECTION('ref_axis',(0.,-0.750800971856654,0.660528501019527));
#36212=DIRECTION('',(-1.,0.,0.));
#36213=DIRECTION('',(0.,-0.750800971856654,0.660528501019527));
#36214=DIRECTION('',(1.,0.,0.));
#36215=DIRECTION('',(0.,-0.750800971856654,0.660528501019527));
#36216=DIRECTION('center_axis',(1.,0.,0.));
#36217=DIRECTION('ref_axis',(0.,-0.984807753012208,-0.17364817766693));
#36218=DIRECTION('center_axis',(-1.,0.,0.));
#36219=DIRECTION('ref_axis',(0.,1.,0.));
#36220=DIRECTION('',(0.,-0.479608080343199,-0.877482814230291));
#36221=DIRECTION('center_axis',(0.,-0.877482814230291,0.479608080343199));
#36222=DIRECTION('ref_axis',(0.,-0.479608080343199,-0.877482814230291));
#36223=DIRECTION('',(1.,0.,0.));
#36224=DIRECTION('',(0.,-0.479608080343199,-0.877482814230291));
#36225=DIRECTION('center_axis',(1.,0.,0.));
#36226=DIRECTION('ref_axis',(0.,-0.984807753012208,-0.17364817766693));
#36227=DIRECTION('center_axis',(1.,0.,0.));
#36228=DIRECTION('ref_axis',(0.,1.,0.));
#36229=DIRECTION('center_axis',(0.,0.780868809443031,0.624695047554424));
#36230=DIRECTION('ref_axis',(0.,-0.624695047554424,0.780868809443031));
#36231=DIRECTION('',(-1.,0.,0.));
#36232=DIRECTION('',(0.,-0.624695047554424,0.780868809443031));
#36233=DIRECTION('',(1.,0.,0.));
#36234=DIRECTION('',(0.,-0.624695047554424,0.780868809443031));
#36235=DIRECTION('center_axis',(1.,0.,0.));
#36236=DIRECTION('ref_axis',(0.,-1.,1.83697019872103E-16));
#36237=DIRECTION('center_axis',(-1.,0.,0.));
#36238=DIRECTION('ref_axis',(0.,1.,0.));
#36239=DIRECTION('',(0.,-0.624695047554424,-0.78086880944303));
#36240=DIRECTION('center_axis',(0.,-0.78086880944303,0.624695047554424));
#36241=DIRECTION('ref_axis',(0.,-0.624695047554424,-0.78086880944303));
#36242=DIRECTION('',(1.,0.,0.));
#36243=DIRECTION('',(0.,-0.624695047554424,-0.78086880944303));
#36244=DIRECTION('center_axis',(1.,0.,0.));
#36245=DIRECTION('ref_axis',(0.,-1.,1.83697019872103E-16));
#36246=DIRECTION('center_axis',(1.,0.,0.));
#36247=DIRECTION('ref_axis',(0.,1.,0.));
#36248=DIRECTION('center_axis',(0.,0.877482814230291,0.479608080343199));
#36249=DIRECTION('ref_axis',(0.,-0.479608080343199,0.877482814230291));
#36250=DIRECTION('',(-1.,0.,0.));
#36251=DIRECTION('',(0.,-0.479608080343199,0.877482814230291));
#36252=DIRECTION('',(1.,0.,0.));
#36253=DIRECTION('',(0.,-0.479608080343199,0.877482814230291));
#36254=DIRECTION('center_axis',(1.,0.,0.));
#36255=DIRECTION('ref_axis',(0.,-0.984807753012208,0.17364817766693));
#36256=DIRECTION('center_axis',(-1.,0.,0.));
#36257=DIRECTION('ref_axis',(0.,1.,0.));
#36258=DIRECTION('',(0.,-0.750800971856654,-0.660528501019527));
#36259=DIRECTION('center_axis',(0.,-0.660528501019527,0.750800971856655));
#36260=DIRECTION('ref_axis',(0.,-0.750800971856654,-0.660528501019527));
#36261=DIRECTION('',(1.,0.,0.));
#36262=DIRECTION('',(0.,-0.750800971856654,-0.660528501019527));
#36263=DIRECTION('center_axis',(1.,0.,0.));
#36264=DIRECTION('ref_axis',(0.,-0.984807753012208,0.17364817766693));
#36265=DIRECTION('center_axis',(1.,0.,0.));
#36266=DIRECTION('ref_axis',(0.,1.,0.));
#36267=DIRECTION('center_axis',(0.,0.947434947734893,0.319948464304144));
#36268=DIRECTION('ref_axis',(0.,-0.319948464304144,0.947434947734893));
#36269=DIRECTION('',(-1.,0.,0.));
#36270=DIRECTION('',(0.,-0.319948464304144,0.947434947734893));
#36271=DIRECTION('',(1.,0.,0.));
#36272=DIRECTION('',(0.,-0.319948464304144,0.947434947734893));
#36273=DIRECTION('center_axis',(1.,0.,0.));
#36274=DIRECTION('ref_axis',(0.,-0.939692620785908,0.342020143325669));
#36275=DIRECTION('center_axis',(-1.,0.,0.));
#36276=DIRECTION('ref_axis',(0.,1.,0.));
#36277=DIRECTION('',(0.,-0.854094188552644,-0.520118368336093));
#36278=DIRECTION('center_axis',(0.,-0.520118368336093,0.854094188552644));
#36279=DIRECTION('ref_axis',(0.,-0.854094188552644,-0.520118368336093));
#36280=DIRECTION('',(1.,0.,0.));
#36281=DIRECTION('',(0.,-0.854094188552644,-0.520118368336093));
#36282=DIRECTION('center_axis',(1.,0.,0.));
#36283=DIRECTION('ref_axis',(0.,-0.939692620785908,0.342020143325669));
#36284=DIRECTION('center_axis',(1.,0.,0.));
#36285=DIRECTION('ref_axis',(0.,1.,0.));
#36286=DIRECTION('center_axis',(0.,0.988599749777787,0.150567376078943));
#36287=DIRECTION('ref_axis',(0.,-0.150567376078943,0.988599749777787));
#36288=DIRECTION('',(-1.,0.,0.));
#36289=DIRECTION('',(0.,-0.150567376078943,0.988599749777787));
#36290=DIRECTION('',(1.,0.,0.));
#36291=DIRECTION('',(0.,-0.150567376078943,0.988599749777787));
#36292=DIRECTION('center_axis',(1.,0.,0.));
#36293=DIRECTION('ref_axis',(0.,-0.866025403784438,0.5));
#36294=DIRECTION('center_axis',(-1.,0.,0.));
#36295=DIRECTION('ref_axis',(0.,1.,0.));
#36296=DIRECTION('',(0.,-0.931436185521974,-0.363904702223362));
#36297=DIRECTION('center_axis',(0.,-0.363904702223362,0.931436185521975));
#36298=DIRECTION('ref_axis',(0.,-0.931436185521975,-0.363904702223362));
#36299=DIRECTION('',(1.,0.,0.));
#36300=DIRECTION('',(0.,-0.931436185521974,-0.363904702223362));
#36301=DIRECTION('center_axis',(1.,0.,0.));
#36302=DIRECTION('ref_axis',(0.,-0.866025403784438,0.5));
#36303=DIRECTION('center_axis',(1.,0.,0.));
#36304=DIRECTION('ref_axis',(0.,1.,0.));
#36305=DIRECTION('center_axis',(0.,0.999726448679293,-0.0233886256776474));
#36306=DIRECTION('ref_axis',(0.,0.0233886256776474,0.999726448679293));
#36307=DIRECTION('',(-1.,0.,0.));
#36308=DIRECTION('',(0.,0.0233886256776475,0.999726448679293));
#36309=DIRECTION('',(1.,0.,0.));
#36310=DIRECTION('',(0.,0.0233886256776475,0.999726448679293));
#36311=DIRECTION('center_axis',(1.,0.,0.));
#36312=DIRECTION('ref_axis',(0.,-0.766044443118978,0.642787609686539));
#36313=DIRECTION('center_axis',(-1.,0.,0.));
#36314=DIRECTION('ref_axis',(0.,1.,0.));
#36315=DIRECTION('',(0.,-0.980476965323672,-0.196633975878238));
#36316=DIRECTION('center_axis',(0.,-0.196633975878238,0.980476965323672));
#36317=DIRECTION('ref_axis',(0.,-0.980476965323672,-0.196633975878238));
#36318=DIRECTION('',(1.,0.,0.));
#36319=DIRECTION('',(0.,-0.980476965323672,-0.196633975878238));
#36320=DIRECTION('center_axis',(1.,0.,0.));
#36321=DIRECTION('ref_axis',(0.,-0.766044443118978,0.642787609686539));
#36322=DIRECTION('center_axis',(1.,0.,0.));
#36323=DIRECTION('ref_axis',(0.,1.,0.));
#36324=DIRECTION('center_axis',(0.,0.980476965323672,-0.196633975878239));
#36325=DIRECTION('ref_axis',(0.,0.196633975878239,0.980476965323671));
#36326=DIRECTION('',(-1.,0.,0.));
#36327=DIRECTION('',(0.,0.196633975878239,0.980476965323671));
#36328=DIRECTION('',(1.,0.,0.));
#36329=DIRECTION('',(0.,0.196633975878239,0.980476965323671));
#36330=DIRECTION('center_axis',(1.,0.,0.));
#36331=DIRECTION('ref_axis',(0.,-0.642787609686539,0.766044443118978));
#36332=DIRECTION('center_axis',(-1.,0.,0.));
#36333=DIRECTION('ref_axis',(0.,1.,0.));
#36334=DIRECTION('',(0.,-0.999726448679293,-0.0233886256776472));
#36335=DIRECTION('center_axis',(0.,-0.0233886256776472,0.999726448679293));
#36336=DIRECTION('ref_axis',(0.,-0.999726448679293,-0.0233886256776472));
#36337=DIRECTION('',(1.,0.,0.));
#36338=DIRECTION('',(0.,-0.999726448679293,-0.0233886256776472));
#36339=DIRECTION('center_axis',(1.,0.,0.));
#36340=DIRECTION('ref_axis',(0.,-0.642787609686539,0.766044443118978));
#36341=DIRECTION('center_axis',(1.,0.,0.));
#36342=DIRECTION('ref_axis',(0.,1.,0.));
#36343=DIRECTION('center_axis',(0.,0.931436185521974,-0.363904702223363));
#36344=DIRECTION('ref_axis',(0.,0.363904702223363,0.931436185521974));
#36345=DIRECTION('',(-1.,0.,0.));
#36346=DIRECTION('',(0.,0.363904702223363,0.931436185521974));
#36347=DIRECTION('',(1.,0.,0.));
#36348=DIRECTION('',(0.,0.363904702223363,0.931436185521974));
#36349=DIRECTION('center_axis',(1.,0.,0.));
#36350=DIRECTION('ref_axis',(0.,-0.5,0.866025403784439));
#36351=DIRECTION('center_axis',(-1.,0.,0.));
#36352=DIRECTION('ref_axis',(0.,1.,0.));
#36353=DIRECTION('',(0.,-0.988599749777786,0.150567376078944));
#36354=DIRECTION('center_axis',(0.,0.150567376078944,0.988599749777786));
#36355=DIRECTION('ref_axis',(0.,-0.988599749777786,0.150567376078944));
#36356=DIRECTION('',(1.,0.,0.));
#36357=DIRECTION('',(0.,-0.988599749777786,0.150567376078944));
#36358=DIRECTION('center_axis',(1.,0.,0.));
#36359=DIRECTION('ref_axis',(0.,-0.5,0.866025403784439));
#36360=DIRECTION('center_axis',(1.,0.,0.));
#36361=DIRECTION('ref_axis',(0.,1.,0.));
#36362=DIRECTION('center_axis',(0.,0.854094188552644,-0.520118368336094));
#36363=DIRECTION('ref_axis',(0.,0.520118368336094,0.854094188552644));
#36364=DIRECTION('',(-1.,0.,0.));
#36365=DIRECTION('',(0.,0.520118368336094,0.854094188552644));
#36366=DIRECTION('',(1.,0.,0.));
#36367=DIRECTION('',(0.,0.520118368336094,0.854094188552644));
#36368=DIRECTION('center_axis',(1.,0.,0.));
#36369=DIRECTION('ref_axis',(0.,-0.342020143325669,0.939692620785909));
#36370=DIRECTION('center_axis',(-1.,0.,0.));
#36371=DIRECTION('ref_axis',(0.,1.,0.));
#36372=DIRECTION('',(0.,-0.947434947734893,0.319948464304145));
#36373=DIRECTION('center_axis',(0.,0.319948464304145,0.947434947734893));
#36374=DIRECTION('ref_axis',(0.,-0.947434947734893,0.319948464304145));
#36375=DIRECTION('',(1.,0.,0.));
#36376=DIRECTION('',(0.,-0.947434947734893,0.319948464304145));
#36377=DIRECTION('center_axis',(1.,0.,0.));
#36378=DIRECTION('ref_axis',(0.,-0.342020143325669,0.939692620785909));
#36379=DIRECTION('center_axis',(1.,0.,0.));
#36380=DIRECTION('ref_axis',(0.,1.,0.));
#36381=DIRECTION('center_axis',(0.,0.750800971856654,-0.660528501019527));
#36382=DIRECTION('ref_axis',(0.,0.660528501019527,0.750800971856654));
#36383=DIRECTION('',(-1.,0.,0.));
#36384=DIRECTION('',(0.,0.660528501019527,0.750800971856654));
#36385=DIRECTION('',(1.,0.,0.));
#36386=DIRECTION('',(0.,0.660528501019527,0.750800971856654));
#36387=DIRECTION('center_axis',(1.,0.,0.));
#36388=DIRECTION('ref_axis',(0.,-0.17364817766693,0.984807753012208));
#36389=DIRECTION('center_axis',(-1.,0.,0.));
#36390=DIRECTION('ref_axis',(0.,1.,0.));
#36391=DIRECTION('',(0.,-0.877482814230291,0.479608080343199));
#36392=DIRECTION('center_axis',(0.,0.479608080343199,0.877482814230291));
#36393=DIRECTION('ref_axis',(0.,-0.877482814230291,0.479608080343199));
#36394=DIRECTION('',(1.,0.,0.));
#36395=DIRECTION('',(0.,-0.877482814230291,0.479608080343199));
#36396=DIRECTION('center_axis',(1.,0.,0.));
#36397=DIRECTION('ref_axis',(0.,-0.17364817766693,0.984807753012208));
#36398=DIRECTION('center_axis',(1.,0.,0.));
#36399=DIRECTION('ref_axis',(0.,1.,0.));
#36400=DIRECTION('center_axis',(0.,0.624695047554424,-0.780868809443031));
#36401=DIRECTION('ref_axis',(0.,0.780868809443031,0.624695047554424));
#36402=DIRECTION('',(-1.,0.,0.));
#36403=DIRECTION('',(0.,0.780868809443031,0.624695047554424));
#36404=DIRECTION('',(1.,0.,0.));
#36405=DIRECTION('',(0.,0.780868809443031,0.624695047554424));
#36406=DIRECTION('center_axis',(1.,0.,0.));
#36407=DIRECTION('ref_axis',(0.,1.22464679914735E-16,1.));
#36408=DIRECTION('center_axis',(-1.,0.,0.));
#36409=DIRECTION('ref_axis',(0.,1.,0.));
#36410=DIRECTION('',(0.,-0.78086880944303,0.624695047554424));
#36411=DIRECTION('center_axis',(-1.,0.,0.));
#36412=DIRECTION('ref_axis',(0.,1.,0.));
#36413=DIRECTION('center_axis',(0.,0.624695047554424,0.78086880944303));
#36414=DIRECTION('ref_axis',(0.,-0.78086880944303,0.624695047554424));
#36415=DIRECTION('',(1.,0.,0.));
#36416=DIRECTION('',(0.,-0.78086880944303,0.624695047554424));
#36417=DIRECTION('center_axis',(1.,0.,0.));
#36418=DIRECTION('ref_axis',(0.,1.22464679914735E-16,1.));
#36419=DIRECTION('center_axis',(1.,0.,0.));
#36420=DIRECTION('ref_axis',(0.,1.,0.));
#36421=DIRECTION('center_axis',(1.,0.,0.));
#36422=DIRECTION('ref_axis',(0.,1.,0.));
#36423=DIRECTION('center_axis',(0.,0.479608080343199,-0.877482814230291));
#36424=DIRECTION('ref_axis',(0.,0.877482814230291,0.479608080343199));
#36425=DIRECTION('',(-1.,0.,0.));
#36426=DIRECTION('',(0.,0.877482814230291,0.479608080343199));
#36427=DIRECTION('',(1.,0.,0.));
#36428=DIRECTION('',(0.,0.877482814230291,0.479608080343199));
#36429=DIRECTION('center_axis',(1.,0.,0.));
#36430=DIRECTION('ref_axis',(0.,0.173648177666931,0.984807753012208));
#36431=DIRECTION('center_axis',(-1.,0.,0.));
#36432=DIRECTION('ref_axis',(0.,1.,0.));
#36433=DIRECTION('',(0.,-0.660528501019527,0.750800971856655));
#36434=DIRECTION('center_axis',(0.,0.750800971856655,0.660528501019527));
#36435=DIRECTION('ref_axis',(0.,-0.660528501019527,0.750800971856655));
#36436=DIRECTION('',(1.,0.,0.));
#36437=DIRECTION('',(0.,-0.660528501019527,0.750800971856655));
#36438=DIRECTION('center_axis',(1.,0.,0.));
#36439=DIRECTION('ref_axis',(0.,0.173648177666931,0.984807753012208));
#36440=DIRECTION('center_axis',(1.,0.,0.));
#36441=DIRECTION('ref_axis',(0.,1.,0.));
#36442=DIRECTION('center_axis',(0.,0.319948464304145,-0.947434947734893));
#36443=DIRECTION('ref_axis',(0.,0.947434947734893,0.319948464304145));
#36444=DIRECTION('',(-1.,0.,0.));
#36445=DIRECTION('',(0.,0.947434947734893,0.319948464304144));
#36446=DIRECTION('',(1.,0.,0.));
#36447=DIRECTION('',(0.,0.947434947734893,0.319948464304144));
#36448=DIRECTION('center_axis',(1.,0.,0.));
#36449=DIRECTION('ref_axis',(0.,0.342020143325669,0.939692620785908));
#36450=DIRECTION('center_axis',(-1.,0.,0.));
#36451=DIRECTION('ref_axis',(0.,1.,0.));
#36452=DIRECTION('',(0.,-0.520118368336094,0.854094188552644));
#36453=DIRECTION('center_axis',(0.,0.854094188552644,0.520118368336094));
#36454=DIRECTION('ref_axis',(0.,-0.520118368336094,0.854094188552644));
#36455=DIRECTION('',(1.,0.,0.));
#36456=DIRECTION('',(0.,-0.520118368336094,0.854094188552644));
#36457=DIRECTION('center_axis',(1.,0.,0.));
#36458=DIRECTION('ref_axis',(0.,0.342020143325669,0.939692620785908));
#36459=DIRECTION('center_axis',(1.,0.,0.));
#36460=DIRECTION('ref_axis',(0.,1.,0.));
#36461=DIRECTION('center_axis',(0.,0.150567376078944,-0.988599749777787));
#36462=DIRECTION('ref_axis',(0.,0.988599749777787,0.150567376078944));
#36463=DIRECTION('',(-1.,0.,0.));
#36464=DIRECTION('',(0.,0.988599749777787,0.150567376078944));
#36465=DIRECTION('',(1.,0.,0.));
#36466=DIRECTION('',(0.,0.988599749777787,0.150567376078944));
#36467=DIRECTION('center_axis',(1.,0.,0.));
#36468=DIRECTION('ref_axis',(0.,0.5,0.866025403784439));
#36469=DIRECTION('center_axis',(-1.,0.,0.));
#36470=DIRECTION('ref_axis',(0.,1.,0.));
#36471=DIRECTION('',(0.,-0.363904702223363,0.931436185521974));
#36472=DIRECTION('center_axis',(0.,0.931436185521974,0.363904702223363));
#36473=DIRECTION('ref_axis',(0.,-0.363904702223363,0.931436185521974));
#36474=DIRECTION('',(1.,0.,0.));
#36475=DIRECTION('',(0.,-0.363904702223363,0.931436185521974));
#36476=DIRECTION('center_axis',(1.,0.,0.));
#36477=DIRECTION('ref_axis',(0.,0.5,0.866025403784439));
#36478=DIRECTION('center_axis',(1.,0.,0.));
#36479=DIRECTION('ref_axis',(0.,1.,0.));
#36480=DIRECTION('center_axis',(0.,-0.0233886256776474,-0.999726448679293));
#36481=DIRECTION('ref_axis',(0.,0.999726448679293,-0.0233886256776474));
#36482=DIRECTION('',(-1.,0.,0.));
#36483=DIRECTION('',(0.,0.999726448679293,-0.0233886256776475));
#36484=DIRECTION('',(1.,0.,0.));
#36485=DIRECTION('',(0.,0.999726448679293,-0.0233886256776475));
#36486=DIRECTION('center_axis',(1.,0.,0.));
#36487=DIRECTION('ref_axis',(0.,0.642787609686539,0.766044443118978));
#36488=DIRECTION('center_axis',(-1.,0.,0.));
#36489=DIRECTION('ref_axis',(0.,1.,0.));
#36490=DIRECTION('',(0.,-0.196633975878238,0.980476965323672));
#36491=DIRECTION('center_axis',(0.,0.980476965323672,0.196633975878238));
#36492=DIRECTION('ref_axis',(0.,-0.196633975878238,0.980476965323672));
#36493=DIRECTION('',(1.,0.,0.));
#36494=DIRECTION('',(0.,-0.196633975878238,0.980476965323672));
#36495=DIRECTION('center_axis',(1.,0.,0.));
#36496=DIRECTION('ref_axis',(0.,0.642787609686539,0.766044443118978));
#36497=DIRECTION('center_axis',(1.,0.,0.));
#36498=DIRECTION('ref_axis',(0.,1.,0.));
#36499=DIRECTION('center_axis',(0.,-0.196633975878238,-0.980476965323672));
#36500=DIRECTION('ref_axis',(0.,0.980476965323672,-0.196633975878239));
#36501=DIRECTION('',(-1.,0.,0.));
#36502=DIRECTION('',(0.,0.980476965323672,-0.196633975878239));
#36503=DIRECTION('',(1.,0.,0.));
#36504=DIRECTION('',(0.,0.980476965323672,-0.196633975878239));
#36505=DIRECTION('center_axis',(1.,0.,0.));
#36506=DIRECTION('ref_axis',(0.,0.766044443118978,0.642787609686539));
#36507=DIRECTION('center_axis',(-1.,0.,0.));
#36508=DIRECTION('ref_axis',(0.,1.,0.));
#36509=DIRECTION('',(0.,-0.0233886256776473,0.999726448679293));
#36510=DIRECTION('center_axis',(0.,0.999726448679293,0.0233886256776472));
#36511=DIRECTION('ref_axis',(0.,-0.0233886256776472,0.999726448679293));
#36512=DIRECTION('',(1.,0.,0.));
#36513=DIRECTION('',(0.,-0.0233886256776473,0.999726448679293));
#36514=DIRECTION('center_axis',(1.,0.,0.));
#36515=DIRECTION('ref_axis',(0.,0.766044443118978,0.642787609686539));
#36516=DIRECTION('center_axis',(1.,0.,0.));
#36517=DIRECTION('ref_axis',(0.,1.,0.));
#36518=DIRECTION('center_axis',(0.,-0.363904702223363,-0.931436185521974));
#36519=DIRECTION('ref_axis',(0.,0.931436185521974,-0.363904702223363));
#36520=DIRECTION('',(-1.,0.,0.));
#36521=DIRECTION('',(0.,0.931436185521974,-0.363904702223363));
#36522=DIRECTION('',(1.,0.,0.));
#36523=DIRECTION('',(0.,0.931436185521974,-0.363904702223363));
#36524=DIRECTION('center_axis',(1.,0.,0.));
#36525=DIRECTION('ref_axis',(0.,0.866025403784439,0.5));
#36526=DIRECTION('center_axis',(-1.,0.,0.));
#36527=DIRECTION('ref_axis',(0.,1.,0.));
#36528=DIRECTION('',(0.,0.150567376078944,0.988599749777786));
#36529=DIRECTION('center_axis',(0.,0.988599749777786,-0.150567376078944));
#36530=DIRECTION('ref_axis',(0.,0.150567376078944,0.988599749777786));
#36531=DIRECTION('',(1.,0.,0.));
#36532=DIRECTION('',(0.,0.150567376078944,0.988599749777786));
#36533=DIRECTION('center_axis',(1.,0.,0.));
#36534=DIRECTION('ref_axis',(0.,0.866025403784439,0.5));
#36535=DIRECTION('center_axis',(1.,0.,0.));
#36536=DIRECTION('ref_axis',(0.,1.,0.));
#36537=DIRECTION('center_axis',(0.,-0.520118368336094,-0.854094188552644));
#36538=DIRECTION('ref_axis',(0.,0.854094188552644,-0.520118368336094));
#36539=DIRECTION('',(-1.,0.,0.));
#36540=DIRECTION('',(0.,0.854094188552644,-0.520118368336094));
#36541=DIRECTION('',(1.,0.,0.));
#36542=DIRECTION('',(0.,0.854094188552644,-0.520118368336094));
#36543=DIRECTION('center_axis',(1.,0.,0.));
#36544=DIRECTION('ref_axis',(0.,0.939692620785908,0.342020143325669));
#36545=DIRECTION('center_axis',(-1.,0.,0.));
#36546=DIRECTION('ref_axis',(0.,1.,0.));
#36547=DIRECTION('',(0.,0.319948464304145,0.947434947734893));
#36548=DIRECTION('center_axis',(0.,0.947434947734893,-0.319948464304145));
#36549=DIRECTION('ref_axis',(0.,0.319948464304145,0.947434947734893));
#36550=DIRECTION('',(1.,0.,0.));
#36551=DIRECTION('',(0.,0.319948464304145,0.947434947734893));
#36552=DIRECTION('center_axis',(1.,0.,0.));
#36553=DIRECTION('ref_axis',(0.,0.939692620785908,0.342020143325669));
#36554=DIRECTION('center_axis',(1.,0.,0.));
#36555=DIRECTION('ref_axis',(0.,1.,0.));
#36556=DIRECTION('center_axis',(0.,-0.660528501019527,-0.750800971856654));
#36557=DIRECTION('ref_axis',(0.,0.750800971856654,-0.660528501019527));
#36558=DIRECTION('',(-1.,0.,0.));
#36559=DIRECTION('',(0.,0.750800971856654,-0.660528501019527));
#36560=DIRECTION('',(1.,0.,0.));
#36561=DIRECTION('',(0.,0.750800971856654,-0.660528501019527));
#36562=DIRECTION('center_axis',(1.,0.,0.));
#36563=DIRECTION('ref_axis',(0.,0.984807753012208,0.17364817766693));
#36564=DIRECTION('center_axis',(-1.,0.,0.));
#36565=DIRECTION('ref_axis',(0.,1.,0.));
#36566=DIRECTION('',(0.,0.479608080343199,0.877482814230291));
#36567=DIRECTION('center_axis',(0.,0.877482814230291,-0.479608080343199));
#36568=DIRECTION('ref_axis',(0.,0.479608080343199,0.877482814230291));
#36569=DIRECTION('',(1.,0.,0.));
#36570=DIRECTION('',(0.,0.479608080343199,0.877482814230291));
#36571=DIRECTION('center_axis',(1.,0.,0.));
#36572=DIRECTION('ref_axis',(0.,0.984807753012208,0.17364817766693));
#36573=DIRECTION('center_axis',(1.,0.,0.));
#36574=DIRECTION('ref_axis',(0.,1.,0.));
#36575=DIRECTION('center_axis',(0.,-0.780868809443031,-0.624695047554424));
#36576=DIRECTION('ref_axis',(0.,0.624695047554424,-0.780868809443031));
#36577=DIRECTION('',(-1.,0.,0.));
#36578=DIRECTION('',(0.,0.624695047554424,-0.78086880944303));
#36579=DIRECTION('',(1.,0.,0.));
#36580=DIRECTION('',(0.,0.624695047554424,-0.78086880944303));
#36581=DIRECTION('center_axis',(1.,0.,0.));
#36582=DIRECTION('ref_axis',(0.,1.,-6.12323399573677E-17));
#36583=DIRECTION('center_axis',(-1.,0.,0.));
#36584=DIRECTION('ref_axis',(0.,1.,0.));
#36585=DIRECTION('',(0.,0.624695047554424,0.78086880944303));
#36586=DIRECTION('center_axis',(0.,0.780868809443031,-0.624695047554424));
#36587=DIRECTION('ref_axis',(0.,0.624695047554424,0.780868809443031));
#36588=DIRECTION('',(1.,0.,0.));
#36589=DIRECTION('',(0.,0.624695047554424,0.78086880944303));
#36590=DIRECTION('center_axis',(1.,0.,0.));
#36591=DIRECTION('ref_axis',(0.,1.,-6.12323399573677E-17));
#36592=DIRECTION('center_axis',(1.,0.,0.));
#36593=DIRECTION('ref_axis',(0.,1.,0.));
#36594=DIRECTION('center_axis',(0.,-0.877482814230291,-0.479608080343199));
#36595=DIRECTION('ref_axis',(0.,0.479608080343199,-0.877482814230291));
#36596=DIRECTION('',(-1.,0.,0.));
#36597=DIRECTION('',(0.,0.479608080343199,-0.877482814230291));
#36598=DIRECTION('',(1.,0.,0.));
#36599=DIRECTION('',(0.,0.479608080343199,-0.877482814230291));
#36600=DIRECTION('center_axis',(1.,0.,0.));
#36601=DIRECTION('ref_axis',(0.,0.984807753012208,-0.17364817766693));
#36602=DIRECTION('center_axis',(-1.,0.,0.));
#36603=DIRECTION('ref_axis',(0.,1.,0.));
#36604=DIRECTION('',(0.,0.750800971856654,0.660528501019527));
#36605=DIRECTION('center_axis',(0.,0.660528501019527,-0.750800971856655));
#36606=DIRECTION('ref_axis',(0.,0.750800971856654,0.660528501019527));
#36607=DIRECTION('',(1.,0.,0.));
#36608=DIRECTION('',(0.,0.750800971856654,0.660528501019527));
#36609=DIRECTION('center_axis',(1.,0.,0.));
#36610=DIRECTION('ref_axis',(0.,0.984807753012208,-0.17364817766693));
#36611=DIRECTION('center_axis',(1.,0.,0.));
#36612=DIRECTION('ref_axis',(0.,1.,0.));
#36613=DIRECTION('center_axis',(0.,-0.947434947734893,-0.319948464304145));
#36614=DIRECTION('ref_axis',(0.,0.319948464304145,-0.947434947734893));
#36615=DIRECTION('',(-1.,0.,0.));
#36616=DIRECTION('',(0.,0.319948464304145,-0.947434947734893));
#36617=DIRECTION('',(1.,0.,0.));
#36618=DIRECTION('',(0.,0.319948464304145,-0.947434947734893));
#36619=DIRECTION('center_axis',(1.,0.,0.));
#36620=DIRECTION('ref_axis',(0.,0.939692620785908,-0.342020143325669));
#36621=DIRECTION('center_axis',(-1.,0.,0.));
#36622=DIRECTION('ref_axis',(0.,1.,0.));
#36623=DIRECTION('',(0.,0.854094188552644,0.520118368336094));
#36624=DIRECTION('center_axis',(0.,0.520118368336094,-0.854094188552644));
#36625=DIRECTION('ref_axis',(0.,0.854094188552644,0.520118368336094));
#36626=DIRECTION('',(1.,0.,0.));
#36627=DIRECTION('',(0.,0.854094188552644,0.520118368336094));
#36628=DIRECTION('center_axis',(1.,0.,0.));
#36629=DIRECTION('ref_axis',(0.,0.939692620785908,-0.342020143325669));
#36630=DIRECTION('center_axis',(1.,0.,0.));
#36631=DIRECTION('ref_axis',(0.,1.,0.));
#36632=DIRECTION('center_axis',(0.,-0.988599749777787,-0.150567376078944));
#36633=DIRECTION('ref_axis',(0.,0.150567376078944,-0.988599749777787));
#36634=DIRECTION('',(-1.,0.,0.));
#36635=DIRECTION('',(0.,0.150567376078944,-0.988599749777787));
#36636=DIRECTION('',(1.,0.,0.));
#36637=DIRECTION('',(0.,0.150567376078944,-0.988599749777787));
#36638=DIRECTION('center_axis',(1.,0.,0.));
#36639=DIRECTION('ref_axis',(0.,0.866025403784439,-0.5));
#36640=DIRECTION('center_axis',(-1.,0.,0.));
#36641=DIRECTION('ref_axis',(0.,1.,0.));
#36642=DIRECTION('',(0.,0.931436185521974,0.363904702223362));
#36643=DIRECTION('center_axis',(0.,0.363904702223362,-0.931436185521974));
#36644=DIRECTION('ref_axis',(0.,0.931436185521974,0.363904702223362));
#36645=DIRECTION('',(1.,0.,0.));
#36646=DIRECTION('',(0.,0.931436185521974,0.363904702223362));
#36647=DIRECTION('center_axis',(1.,0.,0.));
#36648=DIRECTION('ref_axis',(0.,0.866025403784439,-0.5));
#36649=DIRECTION('center_axis',(1.,0.,0.));
#36650=DIRECTION('ref_axis',(0.,1.,0.));
#36651=DIRECTION('center_axis',(0.,-0.999726448679293,0.0233886256776472));
#36652=DIRECTION('ref_axis',(0.,-0.0233886256776472,-0.999726448679293));
#36653=DIRECTION('',(-1.,0.,0.));
#36654=DIRECTION('',(0.,-0.0233886256776473,-0.999726448679293));
#36655=DIRECTION('',(1.,0.,0.));
#36656=DIRECTION('',(0.,-0.0233886256776473,-0.999726448679293));
#36657=DIRECTION('center_axis',(1.,0.,0.));
#36658=DIRECTION('ref_axis',(0.,0.766044443118978,-0.642787609686539));
#36659=DIRECTION('center_axis',(-1.,0.,0.));
#36660=DIRECTION('ref_axis',(0.,1.,0.));
#36661=DIRECTION('',(0.,0.980476965323672,0.196633975878239));
#36662=DIRECTION('center_axis',(0.,0.196633975878238,-0.980476965323672));
#36663=DIRECTION('ref_axis',(0.,0.980476965323672,0.196633975878239));
#36664=DIRECTION('',(1.,0.,0.));
#36665=DIRECTION('',(0.,0.980476965323672,0.196633975878239));
#36666=DIRECTION('center_axis',(1.,0.,0.));
#36667=DIRECTION('ref_axis',(0.,0.766044443118978,-0.642787609686539));
#36668=DIRECTION('center_axis',(1.,0.,0.));
#36669=DIRECTION('ref_axis',(0.,1.,0.));
#36670=DIRECTION('center_axis',(0.,-0.980476965323672,0.196633975878239));
#36671=DIRECTION('ref_axis',(0.,-0.196633975878239,-0.980476965323671));
#36672=DIRECTION('',(-1.,0.,0.));
#36673=DIRECTION('',(0.,-0.196633975878239,-0.980476965323671));
#36674=DIRECTION('',(1.,0.,0.));
#36675=DIRECTION('',(0.,-0.196633975878239,-0.980476965323671));
#36676=DIRECTION('center_axis',(1.,0.,0.));
#36677=DIRECTION('ref_axis',(0.,0.642787609686539,-0.766044443118978));
#36678=DIRECTION('center_axis',(-1.,0.,0.));
#36679=DIRECTION('ref_axis',(0.,1.,0.));
#36680=DIRECTION('',(0.,0.999726448679293,0.0233886256776472));
#36681=DIRECTION('center_axis',(0.,0.0233886256776472,-0.999726448679293));
#36682=DIRECTION('ref_axis',(0.,0.999726448679293,0.0233886256776472));
#36683=DIRECTION('',(1.,0.,0.));
#36684=DIRECTION('',(0.,0.999726448679293,0.0233886256776472));
#36685=DIRECTION('center_axis',(1.,0.,0.));
#36686=DIRECTION('ref_axis',(0.,0.642787609686539,-0.766044443118978));
#36687=DIRECTION('center_axis',(1.,0.,0.));
#36688=DIRECTION('ref_axis',(0.,1.,0.));
#36689=DIRECTION('center_axis',(0.,-0.931436185521974,0.363904702223363));
#36690=DIRECTION('ref_axis',(0.,-0.363904702223363,-0.931436185521974));
#36691=DIRECTION('',(-1.,0.,0.));
#36692=DIRECTION('',(0.,-0.363904702223363,-0.931436185521974));
#36693=DIRECTION('',(1.,0.,0.));
#36694=DIRECTION('',(0.,-0.363904702223363,-0.931436185521974));
#36695=DIRECTION('center_axis',(1.,0.,0.));
#36696=DIRECTION('ref_axis',(0.,0.5,-0.866025403784439));
#36697=DIRECTION('center_axis',(-1.,0.,0.));
#36698=DIRECTION('ref_axis',(0.,1.,0.));
#36699=DIRECTION('',(0.,0.988599749777787,-0.150567376078944));
#36700=DIRECTION('center_axis',(0.,-0.150567376078944,-0.988599749777787));
#36701=DIRECTION('ref_axis',(0.,0.988599749777787,-0.150567376078944));
#36702=DIRECTION('',(1.,0.,0.));
#36703=DIRECTION('',(0.,0.988599749777787,-0.150567376078944));
#36704=DIRECTION('center_axis',(1.,0.,0.));
#36705=DIRECTION('ref_axis',(0.,0.5,-0.866025403784439));
#36706=DIRECTION('center_axis',(1.,0.,0.));
#36707=DIRECTION('ref_axis',(0.,1.,0.));
#36708=DIRECTION('center_axis',(0.,-0.854094188552644,0.520118368336094));
#36709=DIRECTION('ref_axis',(0.,-0.520118368336094,-0.854094188552644));
#36710=DIRECTION('',(-1.,0.,0.));
#36711=DIRECTION('',(0.,-0.520118368336094,-0.854094188552644));
#36712=DIRECTION('',(1.,0.,0.));
#36713=DIRECTION('',(0.,-0.520118368336094,-0.854094188552644));
#36714=DIRECTION('center_axis',(1.,0.,0.));
#36715=DIRECTION('ref_axis',(0.,0.342020143325669,-0.939692620785908));
#36716=DIRECTION('center_axis',(-1.,0.,0.));
#36717=DIRECTION('ref_axis',(0.,1.,0.));
#36718=DIRECTION('',(0.,0.947434947734893,-0.319948464304145));
#36719=DIRECTION('center_axis',(0.,-0.319948464304145,-0.947434947734893));
#36720=DIRECTION('ref_axis',(0.,0.947434947734893,-0.319948464304145));
#36721=DIRECTION('',(1.,0.,0.));
#36722=DIRECTION('',(0.,0.947434947734893,-0.319948464304145));
#36723=DIRECTION('center_axis',(1.,0.,0.));
#36724=DIRECTION('ref_axis',(0.,0.342020143325669,-0.939692620785908));
#36725=DIRECTION('center_axis',(1.,0.,0.));
#36726=DIRECTION('ref_axis',(0.,1.,0.));
#36727=DIRECTION('center_axis',(0.,-0.750800971856655,0.660528501019527));
#36728=DIRECTION('ref_axis',(0.,-0.660528501019527,-0.750800971856654));
#36729=DIRECTION('',(-1.,0.,0.));
#36730=DIRECTION('',(0.,-0.660528501019527,-0.750800971856654));
#36731=DIRECTION('',(1.,0.,0.));
#36732=DIRECTION('',(0.,-0.660528501019527,-0.750800971856654));
#36733=DIRECTION('center_axis',(1.,0.,0.));
#36734=DIRECTION('ref_axis',(0.,0.17364817766693,-0.984807753012208));
#36735=DIRECTION('center_axis',(-1.,0.,0.));
#36736=DIRECTION('ref_axis',(0.,1.,0.));
#36737=DIRECTION('',(0.,0.877482814230291,-0.479608080343199));
#36738=DIRECTION('center_axis',(0.,-0.479608080343199,-0.877482814230291));
#36739=DIRECTION('ref_axis',(0.,0.877482814230291,-0.479608080343199));
#36740=DIRECTION('',(1.,0.,0.));
#36741=DIRECTION('',(0.,0.877482814230291,-0.479608080343199));
#36742=DIRECTION('center_axis',(1.,0.,0.));
#36743=DIRECTION('ref_axis',(0.,0.17364817766693,-0.984807753012208));
#36744=DIRECTION('center_axis',(1.,0.,0.));
#36745=DIRECTION('ref_axis',(0.,1.,0.));
#36746=DIRECTION('center_axis',(0.,-0.624695047554424,0.780868809443031));
#36747=DIRECTION('ref_axis',(0.,-0.780868809443031,-0.624695047554424));
#36748=DIRECTION('',(-1.,0.,0.));
#36749=DIRECTION('',(0.,-0.78086880944303,-0.624695047554424));
#36750=DIRECTION('',(1.,0.,0.));
#36751=DIRECTION('',(0.,-0.78086880944303,-0.624695047554424));
#36752=DIRECTION('center_axis',(1.,0.,0.));
#36753=DIRECTION('ref_axis',(0.,0.,-1.));
#36754=DIRECTION('center_axis',(-1.,0.,0.));
#36755=DIRECTION('ref_axis',(0.,1.,0.));
#36756=DIRECTION('',(0.,0.78086880944303,-0.624695047554424));
#36757=DIRECTION('center_axis',(0.,-0.624695047554424,-0.780868809443031));
#36758=DIRECTION('ref_axis',(0.,0.780868809443031,-0.624695047554424));
#36759=DIRECTION('',(1.,0.,0.));
#36760=DIRECTION('',(0.,0.78086880944303,-0.624695047554424));
#36761=DIRECTION('center_axis',(1.,0.,0.));
#36762=DIRECTION('ref_axis',(0.,0.,-1.));
#36763=DIRECTION('center_axis',(1.,0.,0.));
#36764=DIRECTION('ref_axis',(0.,1.,0.));
#36765=DIRECTION('center_axis',(1.,0.,0.));
#36766=DIRECTION('ref_axis',(0.,1.,0.));
#36767=DIRECTION('',(0.517550572850554,-0.855652619082103,-1.04787224114095E-16));
#36768=DIRECTION('center_axis',(-1.,0.,0.));
#36769=DIRECTION('ref_axis',(0.,1.,0.));
#36770=DIRECTION('center_axis',(0.,0.5,0.866025403784439));
#36771=DIRECTION('ref_axis',(0.,0.866025403784439,-0.5));
#36772=DIRECTION('',(0.,0.866025403784439,-0.5));
#36773=DIRECTION('',(-1.,0.,0.));
#36774=DIRECTION('',(0.,0.866025403784439,-0.5));
#36775=DIRECTION('',(-1.,0.,0.));
#36776=DIRECTION('center_axis',(0.,-0.5,0.866025403784439));
#36777=DIRECTION('ref_axis',(0.,0.866025403784439,0.5));
#36778=DIRECTION('',(0.,0.866025403784439,0.5));
#36779=DIRECTION('',(-1.,0.,0.));
#36780=DIRECTION('',(0.,0.866025403784439,0.5));
#36781=DIRECTION('center_axis',(0.,-1.,-1.92296268638356E-16));
#36782=DIRECTION('ref_axis',(0.,-1.92296268638356E-16,1.));
#36783=DIRECTION('',(0.,-1.92296268638356E-16,1.));
#36784=DIRECTION('',(-1.,0.,0.));
#36785=DIRECTION('',(0.,-1.92296268638356E-16,1.));
#36786=DIRECTION('center_axis',(0.,-0.5,-0.866025403784439));
#36787=DIRECTION('ref_axis',(0.,-0.866025403784439,0.5));
#36788=DIRECTION('',(0.,-0.866025403784439,0.5));
#36789=DIRECTION('',(-1.,0.,0.));
#36790=DIRECTION('',(0.,-0.866025403784439,0.5));
#36791=DIRECTION('center_axis',(0.,0.5,-0.866025403784439));
#36792=DIRECTION('ref_axis',(0.,-0.866025403784439,-0.5));
#36793=DIRECTION('',(0.,-0.866025403784439,-0.5));
#36794=DIRECTION('',(-1.,0.,0.));
#36795=DIRECTION('',(0.,-0.866025403784439,-0.5));
#36796=DIRECTION('center_axis',(0.,1.,-3.84592537276713E-16));
#36797=DIRECTION('ref_axis',(0.,-3.84592537276713E-16,-1.));
#36798=DIRECTION('',(0.,-3.84592537276713E-16,-1.));
#36799=DIRECTION('',(0.,-3.84592537276713E-16,-1.));
#36800=DIRECTION('center_axis',(-1.,0.,0.));
#36801=DIRECTION('ref_axis',(0.,0.,1.));
#36802=DIRECTION('center_axis',(1.,0.,0.));
#36803=DIRECTION('ref_axis',(0.,0.,-1.));
#36804=DIRECTION('center_axis',(1.,0.,0.));
#36805=DIRECTION('ref_axis',(0.,-1.,1.83697019872103E-16));
#36806=DIRECTION('center_axis',(0.,-1.,-1.22464679914735E-16));
#36807=DIRECTION('ref_axis',(0.,-1.22464679914735E-16,1.));
#36808=DIRECTION('center_axis',(-1.,0.,0.));
#36809=DIRECTION('ref_axis',(0.,-1.,1.83697019872103E-16));
#36810=DIRECTION('center_axis',(1.,0.,0.));
#36811=DIRECTION('ref_axis',(0.,-1.,1.83697019872103E-16));
#36812=DIRECTION('center_axis',(1.,0.,0.));
#36813=DIRECTION('ref_axis',(0.,1.,0.));
#36814=DIRECTION('',(-1.,0.,0.));
#36815=DIRECTION('center_axis',(1.,0.,0.));
#36816=DIRECTION('ref_axis',(0.,0.,-1.));
#36817=DIRECTION('center_axis',(-1.,0.,0.));
#36818=DIRECTION('ref_axis',(0.,0.,1.));
#36819=DIRECTION('center_axis',(1.,0.,0.));
#36820=DIRECTION('ref_axis',(0.,0.,-1.));
#36821=DIRECTION('center_axis',(-1.,0.,0.));
#36822=DIRECTION('ref_axis',(0.,0.,1.));
#36823=DIRECTION('center_axis',(1.,0.,0.));
#36824=DIRECTION('ref_axis',(0.,0.,-1.));
#36825=DIRECTION('center_axis',(1.,0.,0.));
#36826=DIRECTION('ref_axis',(0.,1.,0.));
#36827=DIRECTION('',(-0.707106781186548,0.707106781186547,8.65956056235493E-17));
#36828=DIRECTION('center_axis',(1.,0.,0.));
#36829=DIRECTION('ref_axis',(0.,1.,0.));
#36830=DIRECTION('center_axis',(-1.,0.,0.));
#36831=DIRECTION('ref_axis',(0.,1.,0.));
#36832=DIRECTION('center_axis',(-1.,0.,0.));
#36833=DIRECTION('ref_axis',(0.,1.,0.));
#36834=DIRECTION('center_axis',(1.,0.,0.));
#36835=DIRECTION('ref_axis',(0.,0.,-1.));
#36836=DIRECTION('',(-0.554700196225228,-0.832050294337845,-1.01896772969045E-16));
#36837=DIRECTION('center_axis',(1.,0.,0.));
#36838=DIRECTION('ref_axis',(0.,1.,0.));
#36839=DIRECTION('center_axis',(1.,0.,0.));
#36840=DIRECTION('ref_axis',(0.,0.,-1.));
#36841=DIRECTION('',(-1.,0.,0.));
#36842=DIRECTION('center_axis',(-1.,0.,0.));
#36843=DIRECTION('ref_axis',(0.,0.,1.));
#36844=DIRECTION('center_axis',(1.,0.,0.));
#36845=DIRECTION('ref_axis',(0.,1.,0.));
#36846=DIRECTION('center_axis',(1.,0.,0.));
#36847=DIRECTION('ref_axis',(0.,0.,-1.));
#36848=DIRECTION('',(-1.,0.,0.));
#36849=DIRECTION('',(-1.,0.,0.));
#36850=DIRECTION('center_axis',(-1.,0.,0.));
#36851=DIRECTION('ref_axis',(0.,1.,0.));
#36852=DIRECTION('center_axis',(1.,0.,0.));
#36853=DIRECTION('ref_axis',(0.,0.,-1.));
#36854=DIRECTION('',(-0.707106781186547,-0.707106781186548,-8.65956056235494E-17));
#36855=DIRECTION('center_axis',(1.,0.,0.));
#36856=DIRECTION('ref_axis',(0.,0.,-1.));
#36857=DIRECTION('axis',(0.,0.,1.));
#36858=DIRECTION('refdir',(1.,0.,0.));
#36859=DIRECTION('center_axis',(1.,0.,0.));
#36860=DIRECTION('ref_axis',(0.,1.,0.));
#36861=DIRECTION('center_axis',(1.,0.,0.));
#36862=DIRECTION('ref_axis',(0.,0.,-1.));
#36863=DIRECTION('',(-1.,0.,0.));
#36864=DIRECTION('center_axis',(1.,0.,0.));
#36865=DIRECTION('ref_axis',(0.,0.,-1.));
#36866=DIRECTION('center_axis',(-1.,0.,0.));
#36867=DIRECTION('ref_axis',(0.,0.,1.));
#36868=DIRECTION('center_axis',(1.,0.,0.));
#36869=DIRECTION('ref_axis',(0.,0.,-1.));
#36870=DIRECTION('center_axis',(1.,0.,0.));
#36871=DIRECTION('ref_axis',(0.,1.,0.));
#36872=DIRECTION('center_axis',(1.,0.,0.));
#36873=DIRECTION('ref_axis',(0.,0.,-1.));
#36874=DIRECTION('',(-1.,0.,0.));
#36875=DIRECTION('center_axis',(1.,0.,0.));
#36876=DIRECTION('ref_axis',(0.,0.,-1.));
#36877=DIRECTION('axis',(0.,0.,1.));
#36878=DIRECTION('refdir',(1.,0.,0.));
#36879=DIRECTION('center_axis',(6.12323399573677E-17,0.,1.));
#36880=DIRECTION('ref_axis',(1.,0.,0.));
#36881=DIRECTION('center_axis',(1.22464679914735E-16,-1.,0.));
#36882=DIRECTION('ref_axis',(-1.,-1.22464679914735E-16,0.));
#36883=DIRECTION('axis',(0.,0.,1.));
#36884=DIRECTION('refdir',(1.,0.,0.));
#36885=DIRECTION('center_axis',(-1.,0.,0.));
#36886=DIRECTION('ref_axis',(0.,0.,1.));
#36887=DIRECTION('center_axis',(1.,0.,0.));
#36888=DIRECTION('ref_axis',(0.,0.,-1.));
#36889=DIRECTION('center_axis',(1.,0.,0.));
#36890=DIRECTION('ref_axis',(0.,1.,0.));
#36891=DIRECTION('center_axis',(1.,0.,0.));
#36892=DIRECTION('ref_axis',(0.,0.,-1.));
#36893=DIRECTION('',(-0.707106781186548,0.707106781186548,8.65956056235493E-17));
#36894=DIRECTION('center_axis',(1.,0.,0.));
#36895=DIRECTION('ref_axis',(0.,1.,0.));
#36896=DIRECTION('center_axis',(1.,0.,0.));
#36897=DIRECTION('ref_axis',(0.,0.,-1.));
#36898=DIRECTION('',(-1.,0.,0.));
#36899=DIRECTION('center_axis',(-1.,0.,0.));
#36900=DIRECTION('ref_axis',(0.,1.,0.));
#36901=DIRECTION('center_axis',(1.,0.,0.));
#36902=DIRECTION('ref_axis',(0.,0.,-1.));
#36903=DIRECTION('',(-0.707106781186548,-0.707106781186547,-8.65956056235493E-17));
#36904=DIRECTION('center_axis',(1.,0.,0.));
#36905=DIRECTION('ref_axis',(0.,0.,-1.));
#36906=DIRECTION('axis',(0.,0.,1.));
#36907=DIRECTION('refdir',(1.,0.,0.));
#36908=DIRECTION('center_axis',(0.0411785507768663,-0.00185466079691824,
0.999150082414672));
#36909=DIRECTION('ref_axis',(-0.998138206004012,0.0449556326208044,0.0412202961022186));
#36910=DIRECTION('center_axis',(0.0411785507792225,-0.00185466078915363,
-0.999150082414589));
#36911=DIRECTION('ref_axis',(-0.334687746107947,-0.94225211030106,-0.0120446352531285));
#36912=DIRECTION('center_axis',(0.0411785507792225,-0.00185466078915363,
-0.999150082414589));
#36913=DIRECTION('ref_axis',(-0.334687746107947,-0.94225211030106,-0.0120446352531285));
#36914=DIRECTION('center_axis',(0.0411785507768663,-0.00185466079691824,
0.999150082414672));
#36915=DIRECTION('ref_axis',(-0.998138206004013,0.0449556326208044,0.0412202961022186));
#36916=DIRECTION('axis',(0.,0.,1.));
#36917=DIRECTION('refdir',(1.,0.,0.));
#36918=DIRECTION('center_axis',(-1.,0.,0.));
#36919=DIRECTION('ref_axis',(0.,-1.,0.));
#36920=DIRECTION('center_axis',(-1.,0.,0.));
#36921=DIRECTION('ref_axis',(0.,-1.,0.));
#36922=DIRECTION('',(-0.707106781186547,0.707106781186548,8.65956056235494E-17));
#36923=DIRECTION('center_axis',(1.,0.,0.));
#36924=DIRECTION('ref_axis',(0.,-1.,0.));
#36925=DIRECTION('center_axis',(1.,0.,0.));
#36926=DIRECTION('ref_axis',(0.,-1.,0.));
#36927=DIRECTION('center_axis',(1.,0.,0.));
#36928=DIRECTION('ref_axis',(0.,1.,0.));
#36929=DIRECTION('',(-1.,0.,0.));
#36930=DIRECTION('center_axis',(1.,0.,0.));
#36931=DIRECTION('ref_axis',(0.,0.,-1.));
#36932=DIRECTION('center_axis',(1.,0.,0.));
#36933=DIRECTION('ref_axis',(0.,0.,-1.));
#36934=DIRECTION('center_axis',(1.,0.,0.));
#36935=DIRECTION('ref_axis',(0.,0.,-1.));
#36936=DIRECTION('center_axis',(1.,0.,0.));
#36937=DIRECTION('ref_axis',(0.,1.,0.));
#36938=DIRECTION('',(-1.,0.,0.));
#36939=DIRECTION('center_axis',(1.,0.,0.));
#36940=DIRECTION('ref_axis',(0.,0.,-1.));
#36941=DIRECTION('center_axis',(-1.,0.,0.));
#36942=DIRECTION('ref_axis',(0.,0.,1.));
#36943=DIRECTION('center_axis',(1.,0.,0.));
#36944=DIRECTION('ref_axis',(0.,0.,-1.));
#36945=DIRECTION('center_axis',(1.,0.,0.));
#36946=DIRECTION('ref_axis',(0.,1.,0.));
#36947=DIRECTION('',(-0.707106781186546,0.707106781186549,8.65956056235496E-17));
#36948=DIRECTION('axis',(0.,0.,1.));
#36949=DIRECTION('refdir',(1.,0.,0.));
#36950=DIRECTION('center_axis',(1.,0.,0.));
#36951=DIRECTION('ref_axis',(0.,1.,0.));
#36952=DIRECTION('',(-1.,0.,0.));
#36953=DIRECTION('center_axis',(1.,0.,0.));
#36954=DIRECTION('ref_axis',(0.,1.,0.));
#36955=DIRECTION('center_axis',(1.,0.,0.));
#36956=DIRECTION('ref_axis',(0.,1.,0.));
#36957=DIRECTION('',(-1.,0.,0.));
#36958=DIRECTION('center_axis',(1.,0.,0.));
#36959=DIRECTION('ref_axis',(0.,1.,0.));
#36960=DIRECTION('',(-1.,0.,0.));
#36961=DIRECTION('center_axis',(1.,0.,0.));
#36962=DIRECTION('ref_axis',(0.,1.,0.));
#36963=DIRECTION('',(-1.,0.,0.));
#36964=DIRECTION('center_axis',(1.,0.,0.));
#36965=DIRECTION('ref_axis',(0.,1.,0.));
#36966=DIRECTION('',(-1.,0.,0.));
#36967=DIRECTION('center_axis',(1.,0.,0.));
#36968=DIRECTION('ref_axis',(0.,1.,0.));
#36969=DIRECTION('',(-1.,0.,0.));
#36970=DIRECTION('center_axis',(1.,0.,0.));
#36971=DIRECTION('ref_axis',(0.,1.,0.));
#36972=DIRECTION('',(-1.,0.,0.));
#36973=DIRECTION('center_axis',(1.,0.,0.));
#36974=DIRECTION('ref_axis',(0.,1.,0.));
#36975=DIRECTION('',(-1.,0.,0.));
#36976=DIRECTION('center_axis',(1.,0.,0.));
#36977=DIRECTION('ref_axis',(0.,1.,0.));
#36978=DIRECTION('',(-1.,0.,0.));
#36979=DIRECTION('center_axis',(1.,0.,0.));
#36980=DIRECTION('ref_axis',(0.,1.,0.));
#36981=DIRECTION('',(-1.,0.,0.));
#36982=DIRECTION('center_axis',(1.,0.,0.));
#36983=DIRECTION('ref_axis',(0.,1.,0.));
#36984=DIRECTION('',(-1.,0.,0.));
#36985=DIRECTION('center_axis',(1.,0.,0.));
#36986=DIRECTION('ref_axis',(0.,1.,0.));
#36987=DIRECTION('',(-1.,0.,0.));
#36988=DIRECTION('center_axis',(1.,0.,0.));
#36989=DIRECTION('ref_axis',(0.,1.,0.));
#36990=DIRECTION('',(-1.,0.,0.));
#36991=DIRECTION('center_axis',(1.,0.,0.));
#36992=DIRECTION('ref_axis',(0.,1.,0.));
#36993=DIRECTION('',(-1.,0.,0.));
#36994=DIRECTION('center_axis',(1.,0.,0.));
#36995=DIRECTION('ref_axis',(0.,1.,0.));
#36996=DIRECTION('',(-1.,0.,0.));
#36997=DIRECTION('center_axis',(1.,0.,0.));
#36998=DIRECTION('ref_axis',(0.,1.,0.));
#36999=DIRECTION('',(-1.,0.,0.));
#37000=DIRECTION('center_axis',(1.,0.,0.));
#37001=DIRECTION('ref_axis',(0.,1.,0.));
#37002=DIRECTION('',(-1.,0.,0.));
#37003=DIRECTION('center_axis',(1.,0.,0.));
#37004=DIRECTION('ref_axis',(0.,1.,0.));
#37005=DIRECTION('',(-1.,0.,0.));
#37006=DIRECTION('center_axis',(1.,0.,0.));
#37007=DIRECTION('ref_axis',(0.,1.,0.));
#37008=DIRECTION('',(-1.,0.,0.));
#37009=DIRECTION('center_axis',(1.,0.,0.));
#37010=DIRECTION('ref_axis',(0.,1.,0.));
#37011=DIRECTION('',(-1.,0.,0.));
#37012=DIRECTION('center_axis',(1.,0.,0.));
#37013=DIRECTION('ref_axis',(0.,1.,0.));
#37014=DIRECTION('',(-1.,0.,0.));
#37015=DIRECTION('center_axis',(1.,0.,0.));
#37016=DIRECTION('ref_axis',(0.,1.,0.));
#37017=DIRECTION('',(-1.,0.,0.));
#37018=DIRECTION('center_axis',(1.,0.,0.));
#37019=DIRECTION('ref_axis',(0.,1.,0.));
#37020=DIRECTION('',(-1.,0.,0.));
#37021=DIRECTION('center_axis',(1.,0.,0.));
#37022=DIRECTION('ref_axis',(0.,1.,0.));
#37023=DIRECTION('',(-1.,0.,0.));
#37024=DIRECTION('center_axis',(1.,0.,0.));
#37025=DIRECTION('ref_axis',(0.,1.,0.));
#37026=DIRECTION('',(-1.,0.,0.));
#37027=DIRECTION('center_axis',(1.,0.,0.));
#37028=DIRECTION('ref_axis',(0.,1.,0.));
#37029=DIRECTION('',(-1.,0.,0.));
#37030=DIRECTION('center_axis',(1.,0.,0.));
#37031=DIRECTION('ref_axis',(0.,1.,0.));
#37032=DIRECTION('',(-1.,0.,0.));
#37033=DIRECTION('center_axis',(1.,0.,0.));
#37034=DIRECTION('ref_axis',(0.,1.,0.));
#37035=DIRECTION('',(-1.,0.,0.));
#37036=DIRECTION('center_axis',(1.,0.,0.));
#37037=DIRECTION('ref_axis',(0.,1.,0.));
#37038=DIRECTION('',(-1.,0.,0.));
#37039=DIRECTION('center_axis',(1.,0.,0.));
#37040=DIRECTION('ref_axis',(0.,1.,0.));
#37041=DIRECTION('',(-1.,0.,0.));
#37042=DIRECTION('center_axis',(1.,0.,0.));
#37043=DIRECTION('ref_axis',(0.,1.,0.));
#37044=DIRECTION('',(-1.,0.,0.));
#37045=DIRECTION('center_axis',(1.,0.,0.));
#37046=DIRECTION('ref_axis',(0.,1.,0.));
#37047=DIRECTION('',(-1.,0.,0.));
#37048=DIRECTION('center_axis',(1.,0.,0.));
#37049=DIRECTION('ref_axis',(0.,1.,0.));
#37050=DIRECTION('',(-1.,0.,0.));
#37051=DIRECTION('center_axis',(1.,0.,0.));
#37052=DIRECTION('ref_axis',(0.,1.,0.));
#37053=DIRECTION('',(-1.,0.,0.));
#37054=DIRECTION('center_axis',(1.,0.,0.));
#37055=DIRECTION('ref_axis',(0.,1.,0.));
#37056=DIRECTION('',(-1.,0.,0.));
#37057=DIRECTION('center_axis',(1.,0.,0.));
#37058=DIRECTION('ref_axis',(0.,1.,0.));
#37059=DIRECTION('',(-1.,0.,0.));
#37060=DIRECTION('center_axis',(1.,0.,0.));
#37061=DIRECTION('ref_axis',(0.,1.,0.));
#37062=DIRECTION('',(-1.,0.,0.));
#37063=DIRECTION('center_axis',(1.,0.,0.));
#37064=DIRECTION('ref_axis',(0.,1.,0.));
#37065=DIRECTION('',(-1.,0.,0.));
#37066=DIRECTION('center_axis',(1.,0.,0.));
#37067=DIRECTION('ref_axis',(0.,1.,0.));
#37068=DIRECTION('',(-1.,0.,0.));
#37069=DIRECTION('center_axis',(1.,0.,0.));
#37070=DIRECTION('ref_axis',(0.,1.,0.));
#37071=DIRECTION('',(-1.,0.,0.));
#37072=DIRECTION('center_axis',(1.,0.,0.));
#37073=DIRECTION('ref_axis',(0.,1.,0.));
#37074=DIRECTION('',(-1.,0.,0.));
#37075=DIRECTION('center_axis',(1.,0.,0.));
#37076=DIRECTION('ref_axis',(0.,1.,0.));
#37077=DIRECTION('',(-1.,0.,0.));
#37078=DIRECTION('center_axis',(1.,0.,0.));
#37079=DIRECTION('ref_axis',(0.,-0.266010612903804,-0.963970100066668));
#37080=DIRECTION('',(1.,0.,0.));
#37081=DIRECTION('center_axis',(1.,0.,0.));
#37082=DIRECTION('ref_axis',(0.,1.,-4.74988542142691E-13));
#37083=DIRECTION('center_axis',(1.,0.,0.));
#37084=DIRECTION('ref_axis',(0.,1.,-4.74988542142691E-13));
#37085=DIRECTION('',(1.,0.,0.));
#37086=DIRECTION('center_axis',(1.,0.,0.));
#37087=DIRECTION('ref_axis',(0.,1.,-4.74988542142691E-13));
#37088=DIRECTION('',(1.,0.,0.));
#37089=DIRECTION('center_axis',(1.,0.,0.));
#37090=DIRECTION('ref_axis',(0.,1.,-4.74988542142691E-13));
#37091=DIRECTION('',(1.,0.,0.));
#37092=DIRECTION('center_axis',(1.,0.,0.));
#37093=DIRECTION('ref_axis',(0.,1.,-4.74988542142691E-13));
#37094=DIRECTION('',(1.,0.,0.));
#37095=DIRECTION('center_axis',(1.,0.,0.));
#37096=DIRECTION('ref_axis',(0.,1.,-4.74988542142691E-13));
#37097=DIRECTION('',(1.,0.,0.));
#37098=DIRECTION('center_axis',(1.,0.,0.));
#37099=DIRECTION('ref_axis',(0.,1.,-4.74988542142691E-13));
#37100=DIRECTION('',(1.,0.,0.));
#37101=DIRECTION('center_axis',(1.,0.,0.));
#37102=DIRECTION('ref_axis',(0.,1.,-4.74988542142691E-13));
#37103=DIRECTION('',(1.,0.,0.));
#37104=DIRECTION('center_axis',(1.,0.,0.));
#37105=DIRECTION('ref_axis',(0.,1.,-4.74988542142691E-13));
#37106=DIRECTION('',(1.,0.,0.));
#37107=DIRECTION('center_axis',(1.,0.,0.));
#37108=DIRECTION('ref_axis',(0.,1.,-4.74988542142691E-13));
#37109=DIRECTION('',(1.,0.,0.));
#37110=DIRECTION('center_axis',(1.,0.,0.));
#37111=DIRECTION('ref_axis',(0.,1.,-4.74988542142691E-13));
#37112=DIRECTION('',(1.,0.,0.));
#37113=DIRECTION('center_axis',(1.,0.,0.));
#37114=DIRECTION('ref_axis',(0.,1.,-4.74988542142691E-13));
#37115=DIRECTION('',(1.,0.,0.));
#37116=DIRECTION('center_axis',(1.,0.,0.));
#37117=DIRECTION('ref_axis',(0.,1.,-4.74988542142691E-13));
#37118=DIRECTION('',(1.,0.,0.));
#37119=DIRECTION('center_axis',(1.,0.,0.));
#37120=DIRECTION('ref_axis',(0.,1.,-4.74988542142691E-13));
#37121=DIRECTION('',(1.,0.,0.));
#37122=DIRECTION('center_axis',(1.,0.,0.));
#37123=DIRECTION('ref_axis',(0.,1.,-4.74988542142691E-13));
#37124=DIRECTION('',(1.,0.,0.));
#37125=DIRECTION('center_axis',(1.,0.,0.));
#37126=DIRECTION('ref_axis',(0.,1.,-4.74988542142691E-13));
#37127=DIRECTION('',(1.,0.,0.));
#37128=DIRECTION('center_axis',(1.,0.,0.));
#37129=DIRECTION('ref_axis',(0.,1.,-4.74988542142691E-13));
#37130=DIRECTION('',(1.,0.,0.));
#37131=DIRECTION('center_axis',(1.,0.,0.));
#37132=DIRECTION('ref_axis',(0.,1.,-4.74988542142691E-13));
#37133=DIRECTION('',(1.,0.,0.));
#37134=DIRECTION('center_axis',(1.,0.,0.));
#37135=DIRECTION('ref_axis',(0.,1.,-4.74988542142691E-13));
#37136=DIRECTION('',(1.,0.,0.));
#37137=DIRECTION('center_axis',(1.,0.,0.));
#37138=DIRECTION('ref_axis',(0.,1.,-4.74988542142691E-13));
#37139=DIRECTION('',(1.,0.,0.));
#37140=DIRECTION('center_axis',(1.,0.,0.));
#37141=DIRECTION('ref_axis',(0.,1.,-4.74988542142691E-13));
#37142=DIRECTION('',(1.,0.,0.));
#37143=DIRECTION('center_axis',(1.,0.,0.));
#37144=DIRECTION('ref_axis',(0.,1.,-4.74988542142691E-13));
#37145=DIRECTION('',(1.,0.,0.));
#37146=DIRECTION('center_axis',(1.,0.,0.));
#37147=DIRECTION('ref_axis',(0.,1.,-4.74988542142691E-13));
#37148=DIRECTION('',(1.,0.,0.));
#37149=DIRECTION('center_axis',(1.,0.,0.));
#37150=DIRECTION('ref_axis',(0.,1.,-4.74988542142691E-13));
#37151=DIRECTION('',(1.,0.,0.));
#37152=DIRECTION('center_axis',(1.,0.,0.));
#37153=DIRECTION('ref_axis',(0.,1.,-4.74988542142691E-13));
#37154=DIRECTION('',(1.,0.,0.));
#37155=DIRECTION('center_axis',(1.,0.,0.));
#37156=DIRECTION('ref_axis',(0.,1.,-4.74988542142691E-13));
#37157=DIRECTION('',(1.,0.,0.));
#37158=DIRECTION('center_axis',(1.,0.,0.));
#37159=DIRECTION('ref_axis',(0.,1.,-4.74988542142691E-13));
#37160=DIRECTION('',(1.,0.,0.));
#37161=DIRECTION('center_axis',(1.,0.,0.));
#37162=DIRECTION('ref_axis',(0.,1.,-4.74988542142691E-13));
#37163=DIRECTION('',(1.,0.,0.));
#37164=DIRECTION('center_axis',(1.,0.,0.));
#37165=DIRECTION('ref_axis',(0.,1.,-4.74988542142691E-13));
#37166=DIRECTION('',(1.,0.,0.));
#37167=DIRECTION('center_axis',(1.,0.,0.));
#37168=DIRECTION('ref_axis',(0.,1.,-4.74988542142691E-13));
#37169=DIRECTION('',(1.,0.,0.));
#37170=DIRECTION('center_axis',(1.,0.,0.));
#37171=DIRECTION('ref_axis',(0.,1.,-4.74988542142691E-13));
#37172=DIRECTION('',(1.,0.,0.));
#37173=DIRECTION('center_axis',(1.,0.,0.));
#37174=DIRECTION('ref_axis',(0.,1.,-4.74988542142691E-13));
#37175=DIRECTION('',(1.,0.,0.));
#37176=DIRECTION('center_axis',(1.,0.,0.));
#37177=DIRECTION('ref_axis',(0.,1.,-4.74988542142691E-13));
#37178=DIRECTION('',(1.,0.,0.));
#37179=DIRECTION('center_axis',(1.,0.,0.));
#37180=DIRECTION('ref_axis',(0.,1.,-4.74988542142691E-13));
#37181=DIRECTION('',(1.,0.,0.));
#37182=DIRECTION('center_axis',(1.,0.,0.));
#37183=DIRECTION('ref_axis',(0.,1.,-4.74988542142691E-13));
#37184=DIRECTION('',(1.,0.,0.));
#37185=DIRECTION('center_axis',(1.,0.,0.));
#37186=DIRECTION('ref_axis',(0.,1.,-4.74988542142691E-13));
#37187=DIRECTION('',(1.,0.,0.));
#37188=DIRECTION('center_axis',(1.,0.,0.));
#37189=DIRECTION('ref_axis',(0.,1.,-4.74988542142691E-13));
#37190=DIRECTION('',(1.,0.,0.));
#37191=DIRECTION('center_axis',(1.,0.,0.));
#37192=DIRECTION('ref_axis',(0.,1.,-4.74988542142691E-13));
#37193=DIRECTION('',(1.,0.,0.));
#37194=DIRECTION('center_axis',(1.,0.,0.));
#37195=DIRECTION('ref_axis',(0.,1.,-4.74988542142691E-13));
#37196=DIRECTION('',(1.,0.,0.));
#37197=DIRECTION('center_axis',(1.,0.,0.));
#37198=DIRECTION('ref_axis',(0.,1.,-4.74988542142691E-13));
#37199=DIRECTION('',(1.,0.,0.));
#37200=DIRECTION('center_axis',(1.,0.,0.));
#37201=DIRECTION('ref_axis',(0.,1.,-4.74988542142691E-13));
#37202=DIRECTION('',(1.,0.,0.));
#37203=DIRECTION('center_axis',(1.,0.,0.));
#37204=DIRECTION('ref_axis',(0.,1.,-4.74988542142691E-13));
#37205=DIRECTION('',(1.,0.,0.));
#37206=DIRECTION('center_axis',(1.,0.,0.));
#37207=DIRECTION('ref_axis',(0.,0.,-1.));
#37208=DIRECTION('center_axis',(1.,0.,0.));
#37209=DIRECTION('ref_axis',(0.,1.,0.));
#37210=DIRECTION('center_axis',(1.,0.,0.));
#37211=DIRECTION('ref_axis',(0.,0.,-1.));
#37212=DIRECTION('center_axis',(1.,0.,0.));
#37213=DIRECTION('ref_axis',(0.,1.,0.));
#37214=DIRECTION('center_axis',(1.,0.,0.));
#37215=DIRECTION('ref_axis',(0.,1.,0.));
#37216=DIRECTION('center_axis',(-1.,0.,0.));
#37217=DIRECTION('ref_axis',(0.,1.,-4.74988542142691E-13));
#37218=DIRECTION('center_axis',(1.,0.,0.));
#37219=DIRECTION('ref_axis',(0.,1.,-4.74988542142691E-13));
#37220=DIRECTION('center_axis',(1.,0.,0.));
#37221=DIRECTION('ref_axis',(0.,0.,-1.));
#37222=DIRECTION('center_axis',(1.,0.,0.));
#37223=DIRECTION('ref_axis',(0.,1.,0.));
#37224=DIRECTION('center_axis',(0.,-1.,-1.22464679914735E-16));
#37225=DIRECTION('ref_axis',(0.,-1.22464679914735E-16,1.));
#37226=DIRECTION('center_axis',(-1.,0.,0.));
#37227=DIRECTION('ref_axis',(0.,1.,0.));
#37228=DIRECTION('center_axis',(1.,0.,0.));
#37229=DIRECTION('ref_axis',(0.,1.,0.));
#37230=DIRECTION('center_axis',(1.,0.,0.));
#37231=DIRECTION('ref_axis',(0.,0.939072950732287,-0.343717897705305));
#37232=DIRECTION('center_axis',(-1.,0.,0.));
#37233=DIRECTION('ref_axis',(0.,0.,1.));
#37234=DIRECTION('center_axis',(1.,0.,0.));
#37235=DIRECTION('ref_axis',(0.,0.,-1.));
#37236=DIRECTION('center_axis',(0.,-0.443490878258564,0.896278885672003));
#37237=DIRECTION('ref_axis',(0.,-0.896278885672003,-0.443490878258564));
#37238=DIRECTION('',(-1.,0.,0.));
#37239=DIRECTION('',(0.,-0.896278885672003,-0.443490878258564));
#37240=DIRECTION('',(1.,0.,0.));
#37241=DIRECTION('',(0.,-0.896278885672003,-0.443490878258564));
#37242=DIRECTION('center_axis',(1.,0.,0.));
#37243=DIRECTION('ref_axis',(0.,-0.17364817766693,-0.984807753012208));
#37244=DIRECTION('center_axis',(-1.,0.,0.));
#37245=DIRECTION('ref_axis',(0.,1.,0.));
#37246=DIRECTION('',(0.,0.690543841286577,-0.723290538622744));
#37247=DIRECTION('center_axis',(0.,-0.723290538622744,-0.690543841286577));
#37248=DIRECTION('ref_axis',(0.,0.690543841286577,-0.723290538622744));
#37249=DIRECTION('',(1.,0.,0.));
#37250=DIRECTION('',(0.,0.690543841286577,-0.723290538622744));
#37251=DIRECTION('center_axis',(1.,0.,0.));
#37252=DIRECTION('ref_axis',(0.,-0.17364817766693,-0.984807753012208));
#37253=DIRECTION('center_axis',(1.,0.,0.));
#37254=DIRECTION('ref_axis',(0.,1.,0.));
#37255=DIRECTION('center_axis',(0.,-0.281116060120936,0.959673778292437));
#37256=DIRECTION('ref_axis',(0.,-0.959673778292437,-0.281116060120936));
#37257=DIRECTION('',(-1.,0.,0.));
#37258=DIRECTION('',(0.,-0.959673778292437,-0.281116060120936));
#37259=DIRECTION('',(1.,0.,0.));
#37260=DIRECTION('',(0.,-0.959673778292437,-0.281116060120936));
#37261=DIRECTION('center_axis',(1.,0.,0.));
#37262=DIRECTION('ref_axis',(0.,-0.342020143325669,-0.939692620785908));
#37263=DIRECTION('center_axis',(-1.,0.,0.));
#37264=DIRECTION('ref_axis',(0.,1.,0.));
#37265=DIRECTION('',(0.,0.55445484473828,-0.83221380975459));
#37266=DIRECTION('center_axis',(0.,-0.83221380975459,-0.55445484473828));
#37267=DIRECTION('ref_axis',(0.,0.55445484473828,-0.83221380975459));
#37268=DIRECTION('',(1.,0.,0.));
#37269=DIRECTION('',(0.,0.55445484473828,-0.83221380975459));
#37270=DIRECTION('center_axis',(1.,0.,0.));
#37271=DIRECTION('ref_axis',(0.,-0.342020143325669,-0.939692620785908));
#37272=DIRECTION('center_axis',(1.,0.,0.));
#37273=DIRECTION('ref_axis',(0.,1.,0.));
#37274=DIRECTION('center_axis',(0.,-0.110199672748125,0.993909468777819));
#37275=DIRECTION('ref_axis',(0.,-0.993909468777819,-0.110199672748125));
#37276=DIRECTION('',(-1.,0.,0.));
#37277=DIRECTION('',(0.,-0.993909468777819,-0.110199672748125));
#37278=DIRECTION('',(1.,0.,0.));
#37279=DIRECTION('',(0.,-0.993909468777819,-0.110199672748125));
#37280=DIRECTION('center_axis',(1.,0.,0.));
#37281=DIRECTION('ref_axis',(0.,-0.5,-0.866025403784438));
#37282=DIRECTION('center_axis',(-1.,0.,0.));
#37283=DIRECTION('ref_axis',(0.,1.,0.));
#37284=DIRECTION('',(0.,0.401519018300301,-0.91585068539755));
#37285=DIRECTION('center_axis',(0.,-0.91585068539755,-0.401519018300301));
#37286=DIRECTION('ref_axis',(0.,0.401519018300301,-0.91585068539755));
#37287=DIRECTION('',(1.,0.,0.));
#37288=DIRECTION('',(0.,0.401519018300301,-0.91585068539755));
#37289=DIRECTION('center_axis',(1.,0.,0.));
#37290=DIRECTION('ref_axis',(0.,-0.5,-0.866025403784438));
#37291=DIRECTION('center_axis',(1.,0.,0.));
#37292=DIRECTION('ref_axis',(0.,1.,0.));
#37293=DIRECTION('center_axis',(0.,0.0640650759174134,0.997945722996845));
#37294=DIRECTION('ref_axis',(0.,-0.997945722996845,0.0640650759174133));
#37295=DIRECTION('',(-1.,0.,0.));
#37296=DIRECTION('',(0.,-0.997945722996845,0.0640650759174133));
#37297=DIRECTION('',(1.,0.,0.));
#37298=DIRECTION('',(0.,-0.997945722996845,0.0640650759174133));
#37299=DIRECTION('center_axis',(1.,0.,0.));
#37300=DIRECTION('ref_axis',(0.,-0.64278760968654,-0.766044443118978));
#37301=DIRECTION('center_axis',(-1.,0.,0.));
#37302=DIRECTION('ref_axis',(0.,1.,0.));
#37303=DIRECTION('',(0.,0.236383239669693,-0.971659901407514));
#37304=DIRECTION('center_axis',(0.,-0.971659901407514,-0.236383239669693));
#37305=DIRECTION('ref_axis',(0.,0.236383239669693,-0.971659901407514));
#37306=DIRECTION('',(1.,0.,0.));
#37307=DIRECTION('',(0.,0.236383239669693,-0.971659901407514));
#37308=DIRECTION('center_axis',(1.,0.,0.));
#37309=DIRECTION('ref_axis',(0.,-0.64278760968654,-0.766044443118978));
#37310=DIRECTION('center_axis',(1.,0.,0.));
#37311=DIRECTION('ref_axis',(0.,1.,0.));
#37312=DIRECTION('center_axis',(0.,0.236383239669694,0.971659901407514));
#37313=DIRECTION('ref_axis',(0.,-0.971659901407514,0.236383239669694));
#37314=DIRECTION('',(-1.,0.,0.));
#37315=DIRECTION('',(0.,-0.971659901407514,0.236383239669694));
#37316=DIRECTION('',(1.,0.,0.));
#37317=DIRECTION('',(0.,-0.971659901407514,0.236383239669694));
#37318=DIRECTION('center_axis',(1.,0.,0.));
#37319=DIRECTION('ref_axis',(0.,-0.766044443118978,-0.642787609686539));
#37320=DIRECTION('center_axis',(-1.,0.,0.));
#37321=DIRECTION('ref_axis',(0.,1.,0.));
#37322=DIRECTION('',(0.,0.0640650759174129,-0.997945722996845));
#37323=DIRECTION('center_axis',(0.,-0.997945722996845,-0.0640650759174129));
#37324=DIRECTION('ref_axis',(0.,0.0640650759174129,-0.997945722996845));
#37325=DIRECTION('',(1.,0.,0.));
#37326=DIRECTION('',(0.,0.0640650759174129,-0.997945722996845));
#37327=DIRECTION('center_axis',(1.,0.,0.));
#37328=DIRECTION('ref_axis',(0.,-0.766044443118978,-0.642787609686539));
#37329=DIRECTION('center_axis',(1.,0.,0.));
#37330=DIRECTION('ref_axis',(0.,1.,0.));
#37331=DIRECTION('center_axis',(0.,0.401519018300301,0.91585068539755));
#37332=DIRECTION('ref_axis',(0.,-0.91585068539755,0.401519018300301));
#37333=DIRECTION('',(-1.,0.,0.));
#37334=DIRECTION('',(0.,-0.91585068539755,0.401519018300301));
#37335=DIRECTION('',(1.,0.,0.));
#37336=DIRECTION('',(0.,-0.91585068539755,0.401519018300301));
#37337=DIRECTION('center_axis',(1.,0.,0.));
#37338=DIRECTION('ref_axis',(0.,-0.866025403784439,-0.5));
#37339=DIRECTION('center_axis',(-1.,0.,0.));
#37340=DIRECTION('ref_axis',(0.,1.,0.));
#37341=DIRECTION('',(0.,-0.110199672748125,-0.993909468777819));
#37342=DIRECTION('center_axis',(0.,-0.993909468777819,0.110199672748125));
#37343=DIRECTION('ref_axis',(0.,-0.110199672748125,-0.993909468777819));
#37344=DIRECTION('',(1.,0.,0.));
#37345=DIRECTION('',(0.,-0.110199672748125,-0.993909468777819));
#37346=DIRECTION('center_axis',(1.,0.,0.));
#37347=DIRECTION('ref_axis',(0.,-0.866025403784439,-0.5));
#37348=DIRECTION('center_axis',(1.,0.,0.));
#37349=DIRECTION('ref_axis',(0.,1.,0.));
#37350=DIRECTION('center_axis',(0.,0.554454844738281,0.83221380975459));
#37351=DIRECTION('ref_axis',(0.,-0.83221380975459,0.554454844738281));
#37352=DIRECTION('',(-1.,0.,0.));
#37353=DIRECTION('',(0.,-0.83221380975459,0.554454844738281));
#37354=DIRECTION('',(1.,0.,0.));
#37355=DIRECTION('',(0.,-0.83221380975459,0.554454844738281));
#37356=DIRECTION('center_axis',(1.,0.,0.));
#37357=DIRECTION('ref_axis',(0.,-0.939692620785909,-0.342020143325668));
#37358=DIRECTION('center_axis',(-1.,0.,0.));
#37359=DIRECTION('ref_axis',(0.,1.,0.));
#37360=DIRECTION('',(0.,-0.281116060120938,-0.959673778292437));
#37361=DIRECTION('center_axis',(0.,-0.959673778292437,0.281116060120938));
#37362=DIRECTION('ref_axis',(0.,-0.281116060120938,-0.959673778292437));
#37363=DIRECTION('',(1.,0.,0.));
#37364=DIRECTION('',(0.,-0.281116060120938,-0.959673778292437));
#37365=DIRECTION('center_axis',(1.,0.,0.));
#37366=DIRECTION('ref_axis',(0.,-0.939692620785909,-0.342020143325668));
#37367=DIRECTION('center_axis',(1.,0.,0.));
#37368=DIRECTION('ref_axis',(0.,1.,0.));
#37369=DIRECTION('center_axis',(0.,0.690543841286578,0.723290538622743));
#37370=DIRECTION('ref_axis',(0.,-0.723290538622743,0.690543841286577));
#37371=DIRECTION('',(-1.,0.,0.));
#37372=DIRECTION('',(0.,-0.723290538622743,0.690543841286577));
#37373=DIRECTION('',(1.,0.,0.));
#37374=DIRECTION('',(0.,-0.723290538622743,0.690543841286577));
#37375=DIRECTION('center_axis',(1.,0.,0.));
#37376=DIRECTION('ref_axis',(0.,-0.984807753012208,-0.17364817766693));
#37377=DIRECTION('center_axis',(-1.,0.,0.));
#37378=DIRECTION('ref_axis',(0.,1.,0.));
#37379=DIRECTION('',(0.,-0.443490878258565,-0.896278885672003));
#37380=DIRECTION('center_axis',(0.,-0.896278885672003,0.443490878258565));
#37381=DIRECTION('ref_axis',(0.,-0.443490878258565,-0.896278885672003));
#37382=DIRECTION('',(1.,0.,0.));
#37383=DIRECTION('',(0.,-0.443490878258565,-0.896278885672003));
#37384=DIRECTION('center_axis',(1.,0.,0.));
#37385=DIRECTION('ref_axis',(0.,-0.984807753012208,-0.17364817766693));
#37386=DIRECTION('center_axis',(1.,0.,0.));
#37387=DIRECTION('ref_axis',(0.,1.,0.));
#37388=DIRECTION('center_axis',(0.,0.805651012649425,0.592390450477518));
#37389=DIRECTION('ref_axis',(0.,-0.592390450477518,0.805651012649425));
#37390=DIRECTION('',(-1.,0.,0.));
#37391=DIRECTION('',(0.,-0.592390450477518,0.805651012649425));
#37392=DIRECTION('',(1.,0.,0.));
#37393=DIRECTION('',(0.,-0.592390450477518,0.805651012649425));
#37394=DIRECTION('center_axis',(1.,0.,0.));
#37395=DIRECTION('ref_axis',(0.,-1.,1.83697019872103E-16));
#37396=DIRECTION('center_axis',(-1.,0.,0.));
#37397=DIRECTION('ref_axis',(0.,1.,0.));
#37398=DIRECTION('',(0.,-0.592390450477518,-0.805651012649425));
#37399=DIRECTION('center_axis',(0.,-0.805651012649425,0.592390450477518));
#37400=DIRECTION('ref_axis',(0.,-0.592390450477518,-0.805651012649425));
#37401=DIRECTION('',(1.,0.,0.));
#37402=DIRECTION('',(0.,-0.592390450477518,-0.805651012649425));
#37403=DIRECTION('center_axis',(1.,0.,0.));
#37404=DIRECTION('ref_axis',(0.,-1.,1.83697019872103E-16));
#37405=DIRECTION('center_axis',(1.,0.,0.));
#37406=DIRECTION('ref_axis',(0.,1.,0.));
#37407=DIRECTION('center_axis',(0.,0.896278885672003,0.443490878258564));
#37408=DIRECTION('ref_axis',(0.,-0.443490878258564,0.896278885672003));
#37409=DIRECTION('',(-1.,0.,0.));
#37410=DIRECTION('',(0.,-0.443490878258564,0.896278885672003));
#37411=DIRECTION('',(1.,0.,0.));
#37412=DIRECTION('',(0.,-0.443490878258564,0.896278885672003));
#37413=DIRECTION('center_axis',(1.,0.,0.));
#37414=DIRECTION('ref_axis',(0.,-0.984807753012208,0.17364817766693));
#37415=DIRECTION('center_axis',(-1.,0.,0.));
#37416=DIRECTION('ref_axis',(0.,1.,0.));
#37417=DIRECTION('',(0.,-0.723290538622744,-0.690543841286577));
#37418=DIRECTION('center_axis',(0.,-0.690543841286577,0.723290538622744));
#37419=DIRECTION('ref_axis',(0.,-0.723290538622744,-0.690543841286577));
#37420=DIRECTION('',(1.,0.,0.));
#37421=DIRECTION('',(0.,-0.723290538622744,-0.690543841286577));
#37422=DIRECTION('center_axis',(1.,0.,0.));
#37423=DIRECTION('ref_axis',(0.,-0.984807753012208,0.17364817766693));
#37424=DIRECTION('center_axis',(1.,0.,0.));
#37425=DIRECTION('ref_axis',(0.,1.,0.));
#37426=DIRECTION('center_axis',(0.,0.959673778292437,0.281116060120936));
#37427=DIRECTION('ref_axis',(0.,-0.281116060120936,0.959673778292437));
#37428=DIRECTION('',(-1.,0.,0.));
#37429=DIRECTION('',(0.,-0.281116060120936,0.959673778292437));
#37430=DIRECTION('',(1.,0.,0.));
#37431=DIRECTION('',(0.,-0.281116060120936,0.959673778292437));
#37432=DIRECTION('center_axis',(1.,0.,0.));
#37433=DIRECTION('ref_axis',(0.,-0.939692620785908,0.342020143325669));
#37434=DIRECTION('center_axis',(-1.,0.,0.));
#37435=DIRECTION('ref_axis',(0.,1.,0.));
#37436=DIRECTION('',(0.,-0.83221380975459,-0.55445484473828));
#37437=DIRECTION('center_axis',(0.,-0.55445484473828,0.83221380975459));
#37438=DIRECTION('ref_axis',(0.,-0.83221380975459,-0.55445484473828));
#37439=DIRECTION('',(1.,0.,0.));
#37440=DIRECTION('',(0.,-0.83221380975459,-0.55445484473828));
#37441=DIRECTION('center_axis',(1.,0.,0.));
#37442=DIRECTION('ref_axis',(0.,-0.939692620785908,0.342020143325669));
#37443=DIRECTION('center_axis',(1.,0.,0.));
#37444=DIRECTION('ref_axis',(0.,1.,0.));
#37445=DIRECTION('center_axis',(0.,0.993909468777819,0.110199672748125));
#37446=DIRECTION('ref_axis',(0.,-0.110199672748125,0.993909468777819));
#37447=DIRECTION('',(-1.,0.,0.));
#37448=DIRECTION('',(0.,-0.110199672748125,0.993909468777819));
#37449=DIRECTION('',(1.,0.,0.));
#37450=DIRECTION('',(0.,-0.110199672748125,0.993909468777819));
#37451=DIRECTION('center_axis',(1.,0.,0.));
#37452=DIRECTION('ref_axis',(0.,-0.866025403784438,0.5));
#37453=DIRECTION('center_axis',(-1.,0.,0.));
#37454=DIRECTION('ref_axis',(0.,1.,0.));
#37455=DIRECTION('',(0.,-0.91585068539755,-0.401519018300301));
#37456=DIRECTION('center_axis',(0.,-0.401519018300301,0.91585068539755));
#37457=DIRECTION('ref_axis',(0.,-0.91585068539755,-0.401519018300301));
#37458=DIRECTION('',(1.,0.,0.));
#37459=DIRECTION('',(0.,-0.91585068539755,-0.401519018300301));
#37460=DIRECTION('center_axis',(1.,0.,0.));
#37461=DIRECTION('ref_axis',(0.,-0.866025403784438,0.5));
#37462=DIRECTION('center_axis',(1.,0.,0.));
#37463=DIRECTION('ref_axis',(0.,1.,0.));
#37464=DIRECTION('center_axis',(0.,0.997945722996845,-0.0640650759174131));
#37465=DIRECTION('ref_axis',(0.,0.0640650759174131,0.997945722996845));
#37466=DIRECTION('',(-1.,0.,0.));
#37467=DIRECTION('',(0.,0.0640650759174131,0.997945722996845));
#37468=DIRECTION('',(1.,0.,0.));
#37469=DIRECTION('',(0.,0.0640650759174131,0.997945722996845));
#37470=DIRECTION('center_axis',(1.,0.,0.));
#37471=DIRECTION('ref_axis',(0.,-0.766044443118978,0.642787609686539));
#37472=DIRECTION('center_axis',(-1.,0.,0.));
#37473=DIRECTION('ref_axis',(0.,1.,0.));
#37474=DIRECTION('',(0.,-0.971659901407514,-0.236383239669693));
#37475=DIRECTION('center_axis',(0.,-0.236383239669693,0.971659901407514));
#37476=DIRECTION('ref_axis',(0.,-0.971659901407514,-0.236383239669693));
#37477=DIRECTION('',(1.,0.,0.));
#37478=DIRECTION('',(0.,-0.971659901407514,-0.236383239669693));
#37479=DIRECTION('center_axis',(1.,0.,0.));
#37480=DIRECTION('ref_axis',(0.,-0.766044443118978,0.642787609686539));
#37481=DIRECTION('center_axis',(1.,0.,0.));
#37482=DIRECTION('ref_axis',(0.,1.,0.));
#37483=DIRECTION('center_axis',(0.,0.971659901407514,-0.236383239669694));
#37484=DIRECTION('ref_axis',(0.,0.236383239669694,0.971659901407514));
#37485=DIRECTION('',(-1.,0.,0.));
#37486=DIRECTION('',(0.,0.236383239669694,0.971659901407514));
#37487=DIRECTION('',(1.,0.,0.));
#37488=DIRECTION('',(0.,0.236383239669694,0.971659901407514));
#37489=DIRECTION('center_axis',(1.,0.,0.));
#37490=DIRECTION('ref_axis',(0.,-0.642787609686539,0.766044443118978));
#37491=DIRECTION('center_axis',(-1.,0.,0.));
#37492=DIRECTION('ref_axis',(0.,1.,0.));
#37493=DIRECTION('',(0.,-0.997945722996845,-0.064065075917413));
#37494=DIRECTION('center_axis',(0.,-0.064065075917413,0.997945722996845));
#37495=DIRECTION('ref_axis',(0.,-0.997945722996845,-0.064065075917413));
#37496=DIRECTION('',(1.,0.,0.));
#37497=DIRECTION('',(0.,-0.997945722996845,-0.064065075917413));
#37498=DIRECTION('center_axis',(1.,0.,0.));
#37499=DIRECTION('ref_axis',(0.,-0.642787609686539,0.766044443118978));
#37500=DIRECTION('center_axis',(1.,0.,0.));
#37501=DIRECTION('ref_axis',(0.,1.,0.));
#37502=DIRECTION('center_axis',(0.,0.91585068539755,-0.401519018300301));
#37503=DIRECTION('ref_axis',(0.,0.401519018300301,0.91585068539755));
#37504=DIRECTION('',(-1.,0.,0.));
#37505=DIRECTION('',(0.,0.401519018300301,0.91585068539755));
#37506=DIRECTION('',(1.,0.,0.));
#37507=DIRECTION('',(0.,0.401519018300301,0.91585068539755));
#37508=DIRECTION('center_axis',(1.,0.,0.));
#37509=DIRECTION('ref_axis',(0.,-0.5,0.866025403784439));
#37510=DIRECTION('center_axis',(-1.,0.,0.));
#37511=DIRECTION('ref_axis',(0.,1.,0.));
#37512=DIRECTION('',(0.,-0.993909468777819,0.110199672748126));
#37513=DIRECTION('center_axis',(0.,0.110199672748126,0.993909468777819));
#37514=DIRECTION('ref_axis',(0.,-0.993909468777819,0.110199672748126));
#37515=DIRECTION('',(1.,0.,0.));
#37516=DIRECTION('',(0.,-0.993909468777819,0.110199672748126));
#37517=DIRECTION('center_axis',(1.,0.,0.));
#37518=DIRECTION('ref_axis',(0.,-0.5,0.866025403784439));
#37519=DIRECTION('center_axis',(1.,0.,0.));
#37520=DIRECTION('ref_axis',(0.,1.,0.));
#37521=DIRECTION('center_axis',(0.,0.83221380975459,-0.554454844738281));
#37522=DIRECTION('ref_axis',(0.,0.554454844738281,0.83221380975459));
#37523=DIRECTION('',(-1.,0.,0.));
#37524=DIRECTION('',(0.,0.554454844738281,0.83221380975459));
#37525=DIRECTION('',(1.,0.,0.));
#37526=DIRECTION('',(0.,0.554454844738281,0.83221380975459));
#37527=DIRECTION('center_axis',(1.,0.,0.));
#37528=DIRECTION('ref_axis',(0.,-0.342020143325669,0.939692620785909));
#37529=DIRECTION('center_axis',(-1.,0.,0.));
#37530=DIRECTION('ref_axis',(0.,1.,0.));
#37531=DIRECTION('',(0.,-0.959673778292437,0.281116060120937));
#37532=DIRECTION('center_axis',(0.,0.281116060120937,0.959673778292437));
#37533=DIRECTION('ref_axis',(0.,-0.959673778292437,0.281116060120937));
#37534=DIRECTION('',(1.,0.,0.));
#37535=DIRECTION('',(0.,-0.959673778292437,0.281116060120937));
#37536=DIRECTION('center_axis',(1.,0.,0.));
#37537=DIRECTION('ref_axis',(0.,-0.342020143325669,0.939692620785909));
#37538=DIRECTION('center_axis',(1.,0.,0.));
#37539=DIRECTION('ref_axis',(0.,1.,0.));
#37540=DIRECTION('center_axis',(0.,0.723290538622743,-0.690543841286577));
#37541=DIRECTION('ref_axis',(0.,0.690543841286577,0.723290538622743));
#37542=DIRECTION('',(-1.,0.,0.));
#37543=DIRECTION('',(0.,0.690543841286577,0.723290538622743));
#37544=DIRECTION('',(1.,0.,0.));
#37545=DIRECTION('',(0.,0.690543841286577,0.723290538622743));
#37546=DIRECTION('center_axis',(1.,0.,0.));
#37547=DIRECTION('ref_axis',(0.,-0.17364817766693,0.984807753012208));
#37548=DIRECTION('center_axis',(-1.,0.,0.));
#37549=DIRECTION('ref_axis',(0.,1.,0.));
#37550=DIRECTION('',(0.,-0.896278885672003,0.443490878258565));
#37551=DIRECTION('center_axis',(0.,0.443490878258565,0.896278885672003));
#37552=DIRECTION('ref_axis',(0.,-0.896278885672003,0.443490878258565));
#37553=DIRECTION('',(1.,0.,0.));
#37554=DIRECTION('',(0.,-0.896278885672003,0.443490878258565));
#37555=DIRECTION('center_axis',(1.,0.,0.));
#37556=DIRECTION('ref_axis',(0.,-0.17364817766693,0.984807753012208));
#37557=DIRECTION('center_axis',(1.,0.,0.));
#37558=DIRECTION('ref_axis',(0.,1.,0.));
#37559=DIRECTION('center_axis',(0.,0.592390450477518,-0.805651012649425));
#37560=DIRECTION('ref_axis',(0.,0.805651012649425,0.592390450477518));
#37561=DIRECTION('',(-1.,0.,0.));
#37562=DIRECTION('',(0.,0.805651012649425,0.592390450477518));
#37563=DIRECTION('',(1.,0.,0.));
#37564=DIRECTION('',(0.,0.805651012649425,0.592390450477518));
#37565=DIRECTION('center_axis',(1.,0.,0.));
#37566=DIRECTION('ref_axis',(0.,1.22464679914735E-16,1.));
#37567=DIRECTION('center_axis',(-1.,0.,0.));
#37568=DIRECTION('ref_axis',(0.,1.,0.));
#37569=DIRECTION('',(0.,-0.805651012649425,0.592390450477518));
#37570=DIRECTION('center_axis',(-1.,0.,0.));
#37571=DIRECTION('ref_axis',(0.,1.,0.));
#37572=DIRECTION('center_axis',(0.,0.592390450477518,0.805651012649425));
#37573=DIRECTION('ref_axis',(0.,-0.805651012649425,0.592390450477518));
#37574=DIRECTION('',(1.,0.,0.));
#37575=DIRECTION('',(0.,-0.805651012649425,0.592390450477518));
#37576=DIRECTION('center_axis',(1.,0.,0.));
#37577=DIRECTION('ref_axis',(0.,1.22464679914735E-16,1.));
#37578=DIRECTION('center_axis',(1.,0.,0.));
#37579=DIRECTION('ref_axis',(0.,1.,0.));
#37580=DIRECTION('center_axis',(1.,0.,0.));
#37581=DIRECTION('ref_axis',(0.,1.,0.));
#37582=DIRECTION('center_axis',(0.,0.443490878258564,-0.896278885672003));
#37583=DIRECTION('ref_axis',(0.,0.896278885672003,0.443490878258564));
#37584=DIRECTION('',(-1.,0.,0.));
#37585=DIRECTION('',(0.,0.896278885672003,0.443490878258564));
#37586=DIRECTION('',(1.,0.,0.));
#37587=DIRECTION('',(0.,0.896278885672003,0.443490878258564));
#37588=DIRECTION('center_axis',(1.,0.,0.));
#37589=DIRECTION('ref_axis',(0.,0.173648177666931,0.984807753012208));
#37590=DIRECTION('center_axis',(-1.,0.,0.));
#37591=DIRECTION('ref_axis',(0.,1.,0.));
#37592=DIRECTION('',(0.,-0.690543841286577,0.723290538622744));
#37593=DIRECTION('center_axis',(0.,0.723290538622744,0.690543841286577));
#37594=DIRECTION('ref_axis',(0.,-0.690543841286577,0.723290538622744));
#37595=DIRECTION('',(1.,0.,0.));
#37596=DIRECTION('',(0.,-0.690543841286577,0.723290538622744));
#37597=DIRECTION('center_axis',(1.,0.,0.));
#37598=DIRECTION('ref_axis',(0.,0.173648177666931,0.984807753012208));
#37599=DIRECTION('center_axis',(1.,0.,0.));
#37600=DIRECTION('ref_axis',(0.,1.,0.));
#37601=DIRECTION('center_axis',(0.,0.281116060120937,-0.959673778292437));
#37602=DIRECTION('ref_axis',(0.,0.959673778292437,0.281116060120937));
#37603=DIRECTION('',(-1.,0.,0.));
#37604=DIRECTION('',(0.,0.959673778292437,0.281116060120937));
#37605=DIRECTION('',(1.,0.,0.));
#37606=DIRECTION('',(0.,0.959673778292437,0.281116060120937));
#37607=DIRECTION('center_axis',(1.,0.,0.));
#37608=DIRECTION('ref_axis',(0.,0.342020143325669,0.939692620785908));
#37609=DIRECTION('center_axis',(-1.,0.,0.));
#37610=DIRECTION('ref_axis',(0.,1.,0.));
#37611=DIRECTION('',(0.,-0.554454844738281,0.83221380975459));
#37612=DIRECTION('center_axis',(0.,0.83221380975459,0.554454844738281));
#37613=DIRECTION('ref_axis',(0.,-0.554454844738281,0.83221380975459));
#37614=DIRECTION('',(1.,0.,0.));
#37615=DIRECTION('',(0.,-0.554454844738281,0.83221380975459));
#37616=DIRECTION('center_axis',(1.,0.,0.));
#37617=DIRECTION('ref_axis',(0.,0.342020143325669,0.939692620785908));
#37618=DIRECTION('center_axis',(1.,0.,0.));
#37619=DIRECTION('ref_axis',(0.,1.,0.));
#37620=DIRECTION('center_axis',(0.,0.110199672748126,-0.993909468777819));
#37621=DIRECTION('ref_axis',(0.,0.993909468777819,0.110199672748126));
#37622=DIRECTION('',(-1.,0.,0.));
#37623=DIRECTION('',(0.,0.993909468777819,0.110199672748126));
#37624=DIRECTION('',(1.,0.,0.));
#37625=DIRECTION('',(0.,0.993909468777819,0.110199672748126));
#37626=DIRECTION('center_axis',(1.,0.,0.));
#37627=DIRECTION('ref_axis',(0.,0.5,0.866025403784439));
#37628=DIRECTION('center_axis',(-1.,0.,0.));
#37629=DIRECTION('ref_axis',(0.,1.,0.));
#37630=DIRECTION('',(0.,-0.401519018300301,0.91585068539755));
#37631=DIRECTION('center_axis',(0.,0.91585068539755,0.401519018300301));
#37632=DIRECTION('ref_axis',(0.,-0.401519018300301,0.91585068539755));
#37633=DIRECTION('',(1.,0.,0.));
#37634=DIRECTION('',(0.,-0.401519018300301,0.91585068539755));
#37635=DIRECTION('center_axis',(1.,0.,0.));
#37636=DIRECTION('ref_axis',(0.,0.5,0.866025403784439));
#37637=DIRECTION('center_axis',(1.,0.,0.));
#37638=DIRECTION('ref_axis',(0.,1.,0.));
#37639=DIRECTION('center_axis',(0.,-0.0640650759174131,-0.997945722996845));
#37640=DIRECTION('ref_axis',(0.,0.997945722996845,-0.0640650759174131));
#37641=DIRECTION('',(-1.,0.,0.));
#37642=DIRECTION('',(0.,0.997945722996845,-0.0640650759174131));
#37643=DIRECTION('',(1.,0.,0.));
#37644=DIRECTION('',(0.,0.997945722996845,-0.0640650759174131));
#37645=DIRECTION('center_axis',(1.,0.,0.));
#37646=DIRECTION('ref_axis',(0.,0.642787609686539,0.766044443118978));
#37647=DIRECTION('center_axis',(-1.,0.,0.));
#37648=DIRECTION('ref_axis',(0.,1.,0.));
#37649=DIRECTION('',(0.,-0.236383239669693,0.971659901407514));
#37650=DIRECTION('center_axis',(0.,0.971659901407514,0.236383239669693));
#37651=DIRECTION('ref_axis',(0.,-0.236383239669693,0.971659901407514));
#37652=DIRECTION('',(1.,0.,0.));
#37653=DIRECTION('',(0.,-0.236383239669693,0.971659901407514));
#37654=DIRECTION('center_axis',(1.,0.,0.));
#37655=DIRECTION('ref_axis',(0.,0.642787609686539,0.766044443118978));
#37656=DIRECTION('center_axis',(1.,0.,0.));
#37657=DIRECTION('ref_axis',(0.,1.,0.));
#37658=DIRECTION('center_axis',(0.,-0.236383239669693,-0.971659901407514));
#37659=DIRECTION('ref_axis',(0.,0.971659901407514,-0.236383239669693));
#37660=DIRECTION('',(-1.,0.,0.));
#37661=DIRECTION('',(0.,0.971659901407514,-0.236383239669693));
#37662=DIRECTION('',(1.,0.,0.));
#37663=DIRECTION('',(0.,0.971659901407514,-0.236383239669693));
#37664=DIRECTION('center_axis',(1.,0.,0.));
#37665=DIRECTION('ref_axis',(0.,0.766044443118978,0.642787609686539));
#37666=DIRECTION('center_axis',(-1.,0.,0.));
#37667=DIRECTION('ref_axis',(0.,1.,0.));
#37668=DIRECTION('',(0.,-0.0640650759174131,0.997945722996845));
#37669=DIRECTION('center_axis',(0.,0.997945722996845,0.0640650759174131));
#37670=DIRECTION('ref_axis',(0.,-0.0640650759174131,0.997945722996845));
#37671=DIRECTION('',(1.,0.,0.));
#37672=DIRECTION('',(0.,-0.0640650759174131,0.997945722996845));
#37673=DIRECTION('center_axis',(1.,0.,0.));
#37674=DIRECTION('ref_axis',(0.,0.766044443118978,0.642787609686539));
#37675=DIRECTION('center_axis',(1.,0.,0.));
#37676=DIRECTION('ref_axis',(0.,1.,0.));
#37677=DIRECTION('center_axis',(0.,-0.401519018300301,-0.91585068539755));
#37678=DIRECTION('ref_axis',(0.,0.91585068539755,-0.401519018300301));
#37679=DIRECTION('',(-1.,0.,0.));
#37680=DIRECTION('',(0.,0.91585068539755,-0.401519018300301));
#37681=DIRECTION('',(1.,0.,0.));
#37682=DIRECTION('',(0.,0.91585068539755,-0.401519018300301));
#37683=DIRECTION('center_axis',(1.,0.,0.));
#37684=DIRECTION('ref_axis',(0.,0.866025403784439,0.5));
#37685=DIRECTION('center_axis',(-1.,0.,0.));
#37686=DIRECTION('ref_axis',(0.,1.,0.));
#37687=DIRECTION('',(0.,0.110199672748126,0.993909468777819));
#37688=DIRECTION('center_axis',(0.,0.993909468777819,-0.110199672748126));
#37689=DIRECTION('ref_axis',(0.,0.110199672748126,0.993909468777819));
#37690=DIRECTION('',(1.,0.,0.));
#37691=DIRECTION('',(0.,0.110199672748126,0.993909468777819));
#37692=DIRECTION('center_axis',(1.,0.,0.));
#37693=DIRECTION('ref_axis',(0.,0.866025403784439,0.5));
#37694=DIRECTION('center_axis',(1.,0.,0.));
#37695=DIRECTION('ref_axis',(0.,1.,0.));
#37696=DIRECTION('center_axis',(0.,-0.554454844738281,-0.83221380975459));
#37697=DIRECTION('ref_axis',(0.,0.83221380975459,-0.554454844738281));
#37698=DIRECTION('',(-1.,0.,0.));
#37699=DIRECTION('',(0.,0.83221380975459,-0.554454844738281));
#37700=DIRECTION('',(1.,0.,0.));
#37701=DIRECTION('',(0.,0.83221380975459,-0.554454844738281));
#37702=DIRECTION('center_axis',(1.,0.,0.));
#37703=DIRECTION('ref_axis',(0.,0.939692620785908,0.342020143325669));
#37704=DIRECTION('center_axis',(-1.,0.,0.));
#37705=DIRECTION('ref_axis',(0.,1.,0.));
#37706=DIRECTION('',(0.,0.281116060120937,0.959673778292437));
#37707=DIRECTION('center_axis',(0.,0.959673778292437,-0.281116060120937));
#37708=DIRECTION('ref_axis',(0.,0.281116060120937,0.959673778292437));
#37709=DIRECTION('',(1.,0.,0.));
#37710=DIRECTION('',(0.,0.281116060120937,0.959673778292437));
#37711=DIRECTION('center_axis',(1.,0.,0.));
#37712=DIRECTION('ref_axis',(0.,0.939692620785908,0.342020143325669));
#37713=DIRECTION('center_axis',(1.,0.,0.));
#37714=DIRECTION('ref_axis',(0.,1.,0.));
#37715=DIRECTION('center_axis',(0.,-0.690543841286577,-0.723290538622744));
#37716=DIRECTION('ref_axis',(0.,0.723290538622744,-0.690543841286577));
#37717=DIRECTION('',(-1.,0.,0.));
#37718=DIRECTION('',(0.,0.723290538622744,-0.690543841286577));
#37719=DIRECTION('',(1.,0.,0.));
#37720=DIRECTION('',(0.,0.723290538622744,-0.690543841286577));
#37721=DIRECTION('center_axis',(1.,0.,0.));
#37722=DIRECTION('ref_axis',(0.,0.984807753012208,0.17364817766693));
#37723=DIRECTION('center_axis',(-1.,0.,0.));
#37724=DIRECTION('ref_axis',(0.,1.,0.));
#37725=DIRECTION('',(0.,0.443490878258564,0.896278885672003));
#37726=DIRECTION('center_axis',(0.,0.896278885672003,-0.443490878258564));
#37727=DIRECTION('ref_axis',(0.,0.443490878258564,0.896278885672003));
#37728=DIRECTION('',(1.,0.,0.));
#37729=DIRECTION('',(0.,0.443490878258564,0.896278885672003));
#37730=DIRECTION('center_axis',(1.,0.,0.));
#37731=DIRECTION('ref_axis',(0.,0.984807753012208,0.17364817766693));
#37732=DIRECTION('center_axis',(1.,0.,0.));
#37733=DIRECTION('ref_axis',(0.,1.,0.));
#37734=DIRECTION('center_axis',(0.,-0.805651012649425,-0.592390450477518));
#37735=DIRECTION('ref_axis',(0.,0.592390450477518,-0.805651012649425));
#37736=DIRECTION('',(-1.,0.,0.));
#37737=DIRECTION('',(0.,0.592390450477518,-0.805651012649425));
#37738=DIRECTION('',(1.,0.,0.));
#37739=DIRECTION('',(0.,0.592390450477518,-0.805651012649425));
#37740=DIRECTION('center_axis',(1.,0.,0.));
#37741=DIRECTION('ref_axis',(0.,1.,-6.12323399573677E-17));
#37742=DIRECTION('center_axis',(-1.,0.,0.));
#37743=DIRECTION('ref_axis',(0.,1.,0.));
#37744=DIRECTION('',(0.,0.592390450477518,0.805651012649425));
#37745=DIRECTION('center_axis',(0.,0.805651012649425,-0.592390450477518));
#37746=DIRECTION('ref_axis',(0.,0.592390450477518,0.805651012649425));
#37747=DIRECTION('',(1.,0.,0.));
#37748=DIRECTION('',(0.,0.592390450477518,0.805651012649425));
#37749=DIRECTION('center_axis',(1.,0.,0.));
#37750=DIRECTION('ref_axis',(0.,1.,-6.12323399573677E-17));
#37751=DIRECTION('center_axis',(1.,0.,0.));
#37752=DIRECTION('ref_axis',(0.,1.,0.));
#37753=DIRECTION('center_axis',(0.,-0.896278885672003,-0.443490878258564));
#37754=DIRECTION('ref_axis',(0.,0.443490878258564,-0.896278885672003));
#37755=DIRECTION('',(-1.,0.,0.));
#37756=DIRECTION('',(0.,0.443490878258564,-0.896278885672003));
#37757=DIRECTION('',(1.,0.,0.));
#37758=DIRECTION('',(0.,0.443490878258564,-0.896278885672003));
#37759=DIRECTION('center_axis',(1.,0.,0.));
#37760=DIRECTION('ref_axis',(0.,0.984807753012208,-0.17364817766693));
#37761=DIRECTION('center_axis',(-1.,0.,0.));
#37762=DIRECTION('ref_axis',(0.,1.,0.));
#37763=DIRECTION('',(0.,0.723290538622744,0.690543841286577));
#37764=DIRECTION('center_axis',(0.,0.690543841286577,-0.723290538622744));
#37765=DIRECTION('ref_axis',(0.,0.723290538622744,0.690543841286577));
#37766=DIRECTION('',(1.,0.,0.));
#37767=DIRECTION('',(0.,0.723290538622744,0.690543841286577));
#37768=DIRECTION('center_axis',(1.,0.,0.));
#37769=DIRECTION('ref_axis',(0.,0.984807753012208,-0.17364817766693));
#37770=DIRECTION('center_axis',(1.,0.,0.));
#37771=DIRECTION('ref_axis',(0.,1.,0.));
#37772=DIRECTION('center_axis',(0.,-0.959673778292437,-0.281116060120937));
#37773=DIRECTION('ref_axis',(0.,0.281116060120937,-0.959673778292437));
#37774=DIRECTION('',(-1.,0.,0.));
#37775=DIRECTION('',(0.,0.281116060120937,-0.959673778292437));
#37776=DIRECTION('',(1.,0.,0.));
#37777=DIRECTION('',(0.,0.281116060120937,-0.959673778292437));
#37778=DIRECTION('center_axis',(1.,0.,0.));
#37779=DIRECTION('ref_axis',(0.,0.939692620785908,-0.342020143325669));
#37780=DIRECTION('center_axis',(-1.,0.,0.));
#37781=DIRECTION('ref_axis',(0.,1.,0.));
#37782=DIRECTION('',(0.,0.83221380975459,0.554454844738281));
#37783=DIRECTION('center_axis',(0.,0.554454844738281,-0.83221380975459));
#37784=DIRECTION('ref_axis',(0.,0.83221380975459,0.554454844738281));
#37785=DIRECTION('',(1.,0.,0.));
#37786=DIRECTION('',(0.,0.83221380975459,0.554454844738281));
#37787=DIRECTION('center_axis',(1.,0.,0.));
#37788=DIRECTION('ref_axis',(0.,0.939692620785908,-0.342020143325669));
#37789=DIRECTION('center_axis',(1.,0.,0.));
#37790=DIRECTION('ref_axis',(0.,1.,0.));
#37791=DIRECTION('center_axis',(0.,-0.993909468777819,-0.110199672748125));
#37792=DIRECTION('ref_axis',(0.,0.110199672748125,-0.993909468777819));
#37793=DIRECTION('',(-1.,0.,0.));
#37794=DIRECTION('',(0.,0.110199672748125,-0.993909468777819));
#37795=DIRECTION('',(1.,0.,0.));
#37796=DIRECTION('',(0.,0.110199672748125,-0.993909468777819));
#37797=DIRECTION('center_axis',(1.,0.,0.));
#37798=DIRECTION('ref_axis',(0.,0.866025403784439,-0.5));
#37799=DIRECTION('center_axis',(-1.,0.,0.));
#37800=DIRECTION('ref_axis',(0.,1.,0.));
#37801=DIRECTION('',(0.,0.91585068539755,0.401519018300301));
#37802=DIRECTION('center_axis',(0.,0.401519018300301,-0.91585068539755));
#37803=DIRECTION('ref_axis',(0.,0.91585068539755,0.401519018300301));
#37804=DIRECTION('',(1.,0.,0.));
#37805=DIRECTION('',(0.,0.91585068539755,0.401519018300301));
#37806=DIRECTION('center_axis',(1.,0.,0.));
#37807=DIRECTION('ref_axis',(0.,0.866025403784439,-0.5));
#37808=DIRECTION('center_axis',(1.,0.,0.));
#37809=DIRECTION('ref_axis',(0.,1.,0.));
#37810=DIRECTION('center_axis',(0.,-0.997945722996845,0.0640650759174131));
#37811=DIRECTION('ref_axis',(0.,-0.0640650759174131,-0.997945722996845));
#37812=DIRECTION('',(-1.,0.,0.));
#37813=DIRECTION('',(0.,-0.0640650759174131,-0.997945722996845));
#37814=DIRECTION('',(1.,0.,0.));
#37815=DIRECTION('',(0.,-0.0640650759174131,-0.997945722996845));
#37816=DIRECTION('center_axis',(1.,0.,0.));
#37817=DIRECTION('ref_axis',(0.,0.766044443118978,-0.642787609686539));
#37818=DIRECTION('center_axis',(-1.,0.,0.));
#37819=DIRECTION('ref_axis',(0.,1.,0.));
#37820=DIRECTION('',(0.,0.971659901407514,0.236383239669693));
#37821=DIRECTION('center_axis',(0.,0.236383239669693,-0.971659901407514));
#37822=DIRECTION('ref_axis',(0.,0.971659901407514,0.236383239669693));
#37823=DIRECTION('',(1.,0.,0.));
#37824=DIRECTION('',(0.,0.971659901407514,0.236383239669693));
#37825=DIRECTION('center_axis',(1.,0.,0.));
#37826=DIRECTION('ref_axis',(0.,0.766044443118978,-0.642787609686539));
#37827=DIRECTION('center_axis',(1.,0.,0.));
#37828=DIRECTION('ref_axis',(0.,1.,0.));
#37829=DIRECTION('center_axis',(0.,-0.971659901407514,0.236383239669694));
#37830=DIRECTION('ref_axis',(0.,-0.236383239669694,-0.971659901407514));
#37831=DIRECTION('',(-1.,0.,0.));
#37832=DIRECTION('',(0.,-0.236383239669694,-0.971659901407514));
#37833=DIRECTION('',(1.,0.,0.));
#37834=DIRECTION('',(0.,-0.236383239669694,-0.971659901407514));
#37835=DIRECTION('center_axis',(1.,0.,0.));
#37836=DIRECTION('ref_axis',(0.,0.642787609686539,-0.766044443118978));
#37837=DIRECTION('center_axis',(-1.,0.,0.));
#37838=DIRECTION('ref_axis',(0.,1.,0.));
#37839=DIRECTION('',(0.,0.997945722996845,0.064065075917413));
#37840=DIRECTION('center_axis',(0.,0.064065075917413,-0.997945722996845));
#37841=DIRECTION('ref_axis',(0.,0.997945722996845,0.064065075917413));
#37842=DIRECTION('',(1.,0.,0.));
#37843=DIRECTION('',(0.,0.997945722996845,0.064065075917413));
#37844=DIRECTION('center_axis',(1.,0.,0.));
#37845=DIRECTION('ref_axis',(0.,0.642787609686539,-0.766044443118978));
#37846=DIRECTION('center_axis',(1.,0.,0.));
#37847=DIRECTION('ref_axis',(0.,1.,0.));
#37848=DIRECTION('center_axis',(0.,-0.91585068539755,0.401519018300301));
#37849=DIRECTION('ref_axis',(0.,-0.401519018300301,-0.91585068539755));
#37850=DIRECTION('',(-1.,0.,0.));
#37851=DIRECTION('',(0.,-0.401519018300301,-0.91585068539755));
#37852=DIRECTION('',(1.,0.,0.));
#37853=DIRECTION('',(0.,-0.401519018300301,-0.91585068539755));
#37854=DIRECTION('center_axis',(1.,0.,0.));
#37855=DIRECTION('ref_axis',(0.,0.5,-0.866025403784439));
#37856=DIRECTION('center_axis',(-1.,0.,0.));
#37857=DIRECTION('ref_axis',(0.,1.,0.));
#37858=DIRECTION('',(0.,0.993909468777819,-0.110199672748126));
#37859=DIRECTION('center_axis',(0.,-0.110199672748126,-0.993909468777819));
#37860=DIRECTION('ref_axis',(0.,0.993909468777819,-0.110199672748126));
#37861=DIRECTION('',(1.,0.,0.));
#37862=DIRECTION('',(0.,0.993909468777819,-0.110199672748126));
#37863=DIRECTION('center_axis',(1.,0.,0.));
#37864=DIRECTION('ref_axis',(0.,0.5,-0.866025403784439));
#37865=DIRECTION('center_axis',(1.,0.,0.));
#37866=DIRECTION('ref_axis',(0.,1.,0.));
#37867=DIRECTION('center_axis',(0.,-0.83221380975459,0.554454844738281));
#37868=DIRECTION('ref_axis',(0.,-0.554454844738281,-0.83221380975459));
#37869=DIRECTION('',(-1.,0.,0.));
#37870=DIRECTION('',(0.,-0.554454844738281,-0.83221380975459));
#37871=DIRECTION('',(1.,0.,0.));
#37872=DIRECTION('',(0.,-0.554454844738281,-0.83221380975459));
#37873=DIRECTION('center_axis',(1.,0.,0.));
#37874=DIRECTION('ref_axis',(0.,0.342020143325669,-0.939692620785908));
#37875=DIRECTION('center_axis',(-1.,0.,0.));
#37876=DIRECTION('ref_axis',(0.,1.,0.));
#37877=DIRECTION('',(0.,0.959673778292437,-0.281116060120937));
#37878=DIRECTION('center_axis',(0.,-0.281116060120937,-0.959673778292437));
#37879=DIRECTION('ref_axis',(0.,0.959673778292437,-0.281116060120937));
#37880=DIRECTION('',(1.,0.,0.));
#37881=DIRECTION('',(0.,0.959673778292437,-0.281116060120937));
#37882=DIRECTION('center_axis',(1.,0.,0.));
#37883=DIRECTION('ref_axis',(0.,0.342020143325669,-0.939692620785908));
#37884=DIRECTION('center_axis',(1.,0.,0.));
#37885=DIRECTION('ref_axis',(0.,1.,0.));
#37886=DIRECTION('center_axis',(0.,-0.723290538622744,0.690543841286577));
#37887=DIRECTION('ref_axis',(0.,-0.690543841286577,-0.723290538622744));
#37888=DIRECTION('',(-1.,0.,0.));
#37889=DIRECTION('',(0.,-0.690543841286577,-0.723290538622744));
#37890=DIRECTION('',(1.,0.,0.));
#37891=DIRECTION('',(0.,-0.690543841286577,-0.723290538622744));
#37892=DIRECTION('center_axis',(1.,0.,0.));
#37893=DIRECTION('ref_axis',(0.,0.17364817766693,-0.984807753012208));
#37894=DIRECTION('center_axis',(-1.,0.,0.));
#37895=DIRECTION('ref_axis',(0.,1.,0.));
#37896=DIRECTION('',(0.,0.896278885672003,-0.443490878258564));
#37897=DIRECTION('center_axis',(0.,-0.443490878258564,-0.896278885672003));
#37898=DIRECTION('ref_axis',(0.,0.896278885672003,-0.443490878258564));
#37899=DIRECTION('',(1.,0.,0.));
#37900=DIRECTION('',(0.,0.896278885672003,-0.443490878258564));
#37901=DIRECTION('center_axis',(1.,0.,0.));
#37902=DIRECTION('ref_axis',(0.,0.17364817766693,-0.984807753012208));
#37903=DIRECTION('center_axis',(1.,0.,0.));
#37904=DIRECTION('ref_axis',(0.,1.,0.));
#37905=DIRECTION('center_axis',(0.,-0.592390450477518,0.805651012649425));
#37906=DIRECTION('ref_axis',(0.,-0.805651012649425,-0.592390450477518));
#37907=DIRECTION('',(-1.,0.,0.));
#37908=DIRECTION('',(0.,-0.805651012649425,-0.592390450477518));
#37909=DIRECTION('',(1.,0.,0.));
#37910=DIRECTION('',(0.,-0.805651012649425,-0.592390450477518));
#37911=DIRECTION('center_axis',(1.,0.,0.));
#37912=DIRECTION('ref_axis',(0.,0.,-1.));
#37913=DIRECTION('center_axis',(-1.,0.,0.));
#37914=DIRECTION('ref_axis',(0.,1.,0.));
#37915=DIRECTION('',(0.,0.805651012649425,-0.592390450477518));
#37916=DIRECTION('center_axis',(0.,-0.592390450477518,-0.805651012649425));
#37917=DIRECTION('ref_axis',(0.,0.805651012649425,-0.592390450477518));
#37918=DIRECTION('',(1.,0.,0.));
#37919=DIRECTION('',(0.,0.805651012649425,-0.592390450477518));
#37920=DIRECTION('center_axis',(1.,0.,0.));
#37921=DIRECTION('ref_axis',(0.,0.,-1.));
#37922=DIRECTION('center_axis',(1.,0.,0.));
#37923=DIRECTION('ref_axis',(0.,1.,0.));
#37924=DIRECTION('center_axis',(1.,0.,0.));
#37925=DIRECTION('ref_axis',(0.,1.,0.));
#37926=DIRECTION('',(0.519218171713667,-0.854641732050523,-1.04663426157342E-16));
#37927=DIRECTION('center_axis',(-1.,0.,0.));
#37928=DIRECTION('ref_axis',(0.,1.,0.));
#37929=DIRECTION('center_axis',(0.,0.5,0.866025403784439));
#37930=DIRECTION('ref_axis',(0.,0.866025403784439,-0.5));
#37931=DIRECTION('',(0.,0.866025403784439,-0.5));
#37932=DIRECTION('',(-1.,0.,0.));
#37933=DIRECTION('',(0.,0.866025403784439,-0.5));
#37934=DIRECTION('',(-1.,0.,0.));
#37935=DIRECTION('center_axis',(0.,-0.5,0.866025403784439));
#37936=DIRECTION('ref_axis',(0.,0.866025403784439,0.5));
#37937=DIRECTION('',(0.,0.866025403784439,0.5));
#37938=DIRECTION('',(-1.,0.,0.));
#37939=DIRECTION('',(0.,0.866025403784439,0.5));
#37940=DIRECTION('center_axis',(0.,-1.,-1.60246890531964E-16));
#37941=DIRECTION('ref_axis',(0.,-1.60246890531964E-16,1.));
#37942=DIRECTION('',(0.,-1.60246890531964E-16,1.));
#37943=DIRECTION('',(-1.,0.,0.));
#37944=DIRECTION('',(0.,-1.60246890531964E-16,1.));
#37945=DIRECTION('center_axis',(0.,-0.5,-0.866025403784439));
#37946=DIRECTION('ref_axis',(0.,-0.866025403784439,0.5));
#37947=DIRECTION('',(0.,-0.866025403784439,0.5));
#37948=DIRECTION('',(-1.,0.,0.));
#37949=DIRECTION('',(0.,-0.866025403784439,0.5));
#37950=DIRECTION('center_axis',(0.,0.5,-0.866025403784439));
#37951=DIRECTION('ref_axis',(0.,-0.866025403784439,-0.5));
#37952=DIRECTION('',(0.,-0.866025403784439,-0.5));
#37953=DIRECTION('',(-1.,0.,0.));
#37954=DIRECTION('',(0.,-0.866025403784439,-0.5));
#37955=DIRECTION('center_axis',(0.,1.,-3.20493781063927E-16));
#37956=DIRECTION('ref_axis',(0.,-3.20493781063927E-16,-1.));
#37957=DIRECTION('',(0.,-3.20493781063927E-16,-1.));
#37958=DIRECTION('',(0.,-3.20493781063927E-16,-1.));
#37959=DIRECTION('center_axis',(-1.,0.,0.));
#37960=DIRECTION('ref_axis',(0.,0.,1.));
#37961=DIRECTION('center_axis',(-1.,0.,0.));
#37962=DIRECTION('ref_axis',(0.,0.,1.));
#37963=DIRECTION('center_axis',(1.,0.,0.));
#37964=DIRECTION('ref_axis',(0.,0.,-1.));
#37965=DIRECTION('center_axis',(1.,0.,0.));
#37966=DIRECTION('ref_axis',(0.,1.,0.));
#37967=DIRECTION('',(-0.707106781186548,0.707106781186547,8.65956056235493E-17));
#37968=DIRECTION('center_axis',(1.,0.,0.));
#37969=DIRECTION('ref_axis',(0.,1.,0.));
#37970=DIRECTION('center_axis',(1.,0.,0.));
#37971=DIRECTION('ref_axis',(0.,0.,-1.));
#37972=DIRECTION('',(-1.,0.,0.));
#37973=DIRECTION('',(-1.,0.,0.));
#37974=DIRECTION('center_axis',(-1.,0.,0.));
#37975=DIRECTION('ref_axis',(0.,1.,0.));
#37976=DIRECTION('center_axis',(1.,0.,0.));
#37977=DIRECTION('ref_axis',(0.,0.,-1.));
#37978=DIRECTION('',(-0.707106781186548,-0.707106781186547,-8.65956056235493E-17));
#37979=DIRECTION('center_axis',(1.,0.,0.));
#37980=DIRECTION('ref_axis',(0.,0.,-1.));
#37981=DIRECTION('axis',(0.,0.,1.));
#37982=DIRECTION('refdir',(1.,0.,0.));
#37983=DIRECTION('center_axis',(-1.,0.,0.));
#37984=DIRECTION('ref_axis',(0.,0.,1.));
#37985=DIRECTION('center_axis',(1.,0.,0.));
#37986=DIRECTION('ref_axis',(0.,0.,-1.));
#37987=DIRECTION('center_axis',(1.,0.,0.));
#37988=DIRECTION('ref_axis',(0.,1.,0.));
#37989=DIRECTION('center_axis',(1.,0.,0.));
#37990=DIRECTION('ref_axis',(0.,0.,-1.));
#37991=DIRECTION('',(-0.707106781186547,0.707106781186548,8.65956056235493E-17));
#37992=DIRECTION('center_axis',(1.,0.,0.));
#37993=DIRECTION('ref_axis',(0.,1.,0.));
#37994=DIRECTION('center_axis',(1.,0.,0.));
#37995=DIRECTION('ref_axis',(0.,0.,-1.));
#37996=DIRECTION('',(-1.,0.,0.));
#37997=DIRECTION('center_axis',(-1.,0.,0.));
#37998=DIRECTION('ref_axis',(0.,1.,0.));
#37999=DIRECTION('center_axis',(1.,0.,0.));
#38000=DIRECTION('ref_axis',(0.,0.,-1.));
#38001=DIRECTION('',(-0.707106781186548,-0.707106781186547,-8.65956056235493E-17));
#38002=DIRECTION('center_axis',(1.,0.,0.));
#38003=DIRECTION('ref_axis',(0.,0.,-1.));
#38004=DIRECTION('axis',(0.,0.,1.));
#38005=DIRECTION('refdir',(1.,0.,0.));
#38006=DIRECTION('center_axis',(1.,0.,0.));
#38007=DIRECTION('ref_axis',(0.,1.,0.));
#38008=DIRECTION('',(-1.,0.,0.));
#38009=DIRECTION('center_axis',(1.,0.,0.));
#38010=DIRECTION('ref_axis',(0.,1.,0.));
#38011=DIRECTION('center_axis',(1.,0.,0.));
#38012=DIRECTION('ref_axis',(0.,1.,0.));
#38013=DIRECTION('',(-1.,0.,0.));
#38014=DIRECTION('center_axis',(1.,0.,0.));
#38015=DIRECTION('ref_axis',(0.,1.,0.));
#38016=DIRECTION('',(-1.,0.,0.));
#38017=DIRECTION('center_axis',(1.,0.,0.));
#38018=DIRECTION('ref_axis',(0.,1.,0.));
#38019=DIRECTION('',(-1.,0.,0.));
#38020=DIRECTION('center_axis',(1.,0.,0.));
#38021=DIRECTION('ref_axis',(0.,1.,0.));
#38022=DIRECTION('',(-1.,0.,0.));
#38023=DIRECTION('center_axis',(1.,0.,0.));
#38024=DIRECTION('ref_axis',(0.,1.,0.));
#38025=DIRECTION('',(-1.,0.,0.));
#38026=DIRECTION('center_axis',(1.,0.,0.));
#38027=DIRECTION('ref_axis',(0.,1.,0.));
#38028=DIRECTION('',(-1.,0.,0.));
#38029=DIRECTION('center_axis',(1.,0.,0.));
#38030=DIRECTION('ref_axis',(0.,1.,0.));
#38031=DIRECTION('',(-1.,0.,0.));
#38032=DIRECTION('center_axis',(1.,0.,0.));
#38033=DIRECTION('ref_axis',(0.,1.,0.));
#38034=DIRECTION('',(-1.,0.,0.));
#38035=DIRECTION('center_axis',(1.,0.,0.));
#38036=DIRECTION('ref_axis',(0.,1.,0.));
#38037=DIRECTION('',(-1.,0.,0.));
#38038=DIRECTION('center_axis',(1.,0.,0.));
#38039=DIRECTION('ref_axis',(0.,1.,0.));
#38040=DIRECTION('',(-1.,0.,0.));
#38041=DIRECTION('center_axis',(1.,0.,0.));
#38042=DIRECTION('ref_axis',(0.,1.,0.));
#38043=DIRECTION('',(-1.,0.,0.));
#38044=DIRECTION('center_axis',(1.,0.,0.));
#38045=DIRECTION('ref_axis',(0.,1.,0.));
#38046=DIRECTION('',(-1.,0.,0.));
#38047=DIRECTION('center_axis',(1.,0.,0.));
#38048=DIRECTION('ref_axis',(0.,1.,0.));
#38049=DIRECTION('',(-1.,0.,0.));
#38050=DIRECTION('center_axis',(1.,0.,0.));
#38051=DIRECTION('ref_axis',(0.,1.,0.));
#38052=DIRECTION('',(-1.,0.,0.));
#38053=DIRECTION('center_axis',(1.,0.,0.));
#38054=DIRECTION('ref_axis',(0.,1.,0.));
#38055=DIRECTION('',(-1.,0.,0.));
#38056=DIRECTION('center_axis',(1.,0.,0.));
#38057=DIRECTION('ref_axis',(0.,1.,0.));
#38058=DIRECTION('',(-1.,0.,0.));
#38059=DIRECTION('center_axis',(1.,0.,0.));
#38060=DIRECTION('ref_axis',(0.,1.,0.));
#38061=DIRECTION('',(-1.,0.,0.));
#38062=DIRECTION('center_axis',(1.,0.,0.));
#38063=DIRECTION('ref_axis',(0.,1.,0.));
#38064=DIRECTION('',(-1.,0.,0.));
#38065=DIRECTION('center_axis',(1.,0.,0.));
#38066=DIRECTION('ref_axis',(0.,1.,0.));
#38067=DIRECTION('',(-1.,0.,0.));
#38068=DIRECTION('center_axis',(1.,0.,0.));
#38069=DIRECTION('ref_axis',(0.,1.,0.));
#38070=DIRECTION('',(-1.,0.,0.));
#38071=DIRECTION('center_axis',(1.,0.,0.));
#38072=DIRECTION('ref_axis',(0.,1.,0.));
#38073=DIRECTION('',(-1.,0.,0.));
#38074=DIRECTION('center_axis',(1.,0.,0.));
#38075=DIRECTION('ref_axis',(0.,1.,0.));
#38076=DIRECTION('',(-1.,0.,0.));
#38077=DIRECTION('center_axis',(1.,0.,0.));
#38078=DIRECTION('ref_axis',(0.,1.,0.));
#38079=DIRECTION('',(-1.,0.,0.));
#38080=DIRECTION('center_axis',(1.,0.,0.));
#38081=DIRECTION('ref_axis',(0.,1.,0.));
#38082=DIRECTION('',(-1.,0.,0.));
#38083=DIRECTION('center_axis',(1.,0.,0.));
#38084=DIRECTION('ref_axis',(0.,1.,0.));
#38085=DIRECTION('',(-1.,0.,0.));
#38086=DIRECTION('center_axis',(1.,0.,0.));
#38087=DIRECTION('ref_axis',(0.,1.,0.));
#38088=DIRECTION('',(-1.,0.,0.));
#38089=DIRECTION('center_axis',(1.,0.,0.));
#38090=DIRECTION('ref_axis',(0.,1.,0.));
#38091=DIRECTION('',(-1.,0.,0.));
#38092=DIRECTION('center_axis',(1.,0.,0.));
#38093=DIRECTION('ref_axis',(0.,1.,0.));
#38094=DIRECTION('',(-1.,0.,0.));
#38095=DIRECTION('center_axis',(1.,0.,0.));
#38096=DIRECTION('ref_axis',(0.,1.,0.));
#38097=DIRECTION('',(-1.,0.,0.));
#38098=DIRECTION('center_axis',(1.,0.,0.));
#38099=DIRECTION('ref_axis',(0.,1.,0.));
#38100=DIRECTION('',(-1.,0.,0.));
#38101=DIRECTION('center_axis',(1.,0.,0.));
#38102=DIRECTION('ref_axis',(0.,1.,0.));
#38103=DIRECTION('',(-1.,0.,0.));
#38104=DIRECTION('center_axis',(1.,0.,0.));
#38105=DIRECTION('ref_axis',(0.,1.,0.));
#38106=DIRECTION('',(-1.,0.,0.));
#38107=DIRECTION('center_axis',(1.,0.,0.));
#38108=DIRECTION('ref_axis',(0.,1.,0.));
#38109=DIRECTION('',(-1.,0.,0.));
#38110=DIRECTION('center_axis',(1.,0.,0.));
#38111=DIRECTION('ref_axis',(0.,1.,0.));
#38112=DIRECTION('',(-1.,0.,0.));
#38113=DIRECTION('center_axis',(1.,0.,0.));
#38114=DIRECTION('ref_axis',(0.,1.,0.));
#38115=DIRECTION('',(-1.,0.,0.));
#38116=DIRECTION('center_axis',(1.,0.,0.));
#38117=DIRECTION('ref_axis',(0.,1.,0.));
#38118=DIRECTION('',(-1.,0.,0.));
#38119=DIRECTION('center_axis',(1.,0.,0.));
#38120=DIRECTION('ref_axis',(0.,1.,0.));
#38121=DIRECTION('',(-1.,0.,0.));
#38122=DIRECTION('center_axis',(1.,0.,0.));
#38123=DIRECTION('ref_axis',(0.,1.,0.));
#38124=DIRECTION('',(-1.,0.,0.));
#38125=DIRECTION('center_axis',(1.,0.,0.));
#38126=DIRECTION('ref_axis',(0.,1.,0.));
#38127=DIRECTION('',(-1.,0.,0.));
#38128=DIRECTION('center_axis',(1.,0.,0.));
#38129=DIRECTION('ref_axis',(0.,1.,0.));
#38130=DIRECTION('',(-1.,0.,0.));
#38131=DIRECTION('center_axis',(1.,0.,0.));
#38132=DIRECTION('ref_axis',(0.,1.,0.));
#38133=DIRECTION('',(-1.,0.,0.));
#38134=DIRECTION('center_axis',(1.,0.,0.));
#38135=DIRECTION('ref_axis',(0.,1.,0.));
#38136=DIRECTION('',(-1.,0.,0.));
#38137=DIRECTION('center_axis',(1.,0.,0.));
#38138=DIRECTION('ref_axis',(0.,1.,0.));
#38139=DIRECTION('',(-1.,0.,0.));
#38140=DIRECTION('center_axis',(1.,0.,0.));
#38141=DIRECTION('ref_axis',(0.,1.,0.));
#38142=DIRECTION('',(-1.,0.,0.));
#38143=DIRECTION('center_axis',(1.,0.,0.));
#38144=DIRECTION('ref_axis',(0.,1.,0.));
#38145=DIRECTION('',(-1.,0.,0.));
#38146=DIRECTION('center_axis',(1.,0.,0.));
#38147=DIRECTION('ref_axis',(0.,1.,0.));
#38148=DIRECTION('',(-1.,0.,0.));
#38149=DIRECTION('center_axis',(1.,0.,0.));
#38150=DIRECTION('ref_axis',(0.,1.,0.));
#38151=DIRECTION('',(-1.,0.,0.));
#38152=DIRECTION('center_axis',(1.,0.,0.));
#38153=DIRECTION('ref_axis',(0.,1.,0.));
#38154=DIRECTION('',(-1.,0.,0.));
#38155=DIRECTION('center_axis',(1.,0.,0.));
#38156=DIRECTION('ref_axis',(0.,1.,0.));
#38157=DIRECTION('',(-1.,0.,0.));
#38158=DIRECTION('center_axis',(1.,0.,0.));
#38159=DIRECTION('ref_axis',(0.,1.,0.));
#38160=DIRECTION('',(-1.,0.,0.));
#38161=DIRECTION('center_axis',(1.,0.,0.));
#38162=DIRECTION('ref_axis',(0.,1.,0.));
#38163=DIRECTION('',(-1.,0.,0.));
#38164=DIRECTION('center_axis',(1.,0.,0.));
#38165=DIRECTION('ref_axis',(0.,1.,0.));
#38166=DIRECTION('',(-1.,0.,0.));
#38167=DIRECTION('center_axis',(1.,0.,0.));
#38168=DIRECTION('ref_axis',(0.,1.,0.));
#38169=DIRECTION('',(-1.,0.,0.));
#38170=DIRECTION('center_axis',(1.,0.,0.));
#38171=DIRECTION('ref_axis',(0.,1.,0.));
#38172=DIRECTION('',(-1.,0.,0.));
#38173=DIRECTION('center_axis',(1.,0.,0.));
#38174=DIRECTION('ref_axis',(0.,1.,0.));
#38175=DIRECTION('',(-1.,0.,0.));
#38176=DIRECTION('center_axis',(1.,0.,0.));
#38177=DIRECTION('ref_axis',(0.,1.,0.));
#38178=DIRECTION('',(-1.,0.,0.));
#38179=DIRECTION('center_axis',(1.,0.,0.));
#38180=DIRECTION('ref_axis',(0.,1.,0.));
#38181=DIRECTION('',(-1.,0.,0.));
#38182=DIRECTION('center_axis',(1.,0.,0.));
#38183=DIRECTION('ref_axis',(0.,1.,0.));
#38184=DIRECTION('',(-1.,0.,0.));
#38185=DIRECTION('center_axis',(1.,0.,0.));
#38186=DIRECTION('ref_axis',(0.,1.,0.));
#38187=DIRECTION('',(-1.,0.,0.));
#38188=DIRECTION('center_axis',(1.,0.,0.));
#38189=DIRECTION('ref_axis',(0.,1.,0.));
#38190=DIRECTION('',(-1.,0.,0.));
#38191=DIRECTION('center_axis',(1.,0.,0.));
#38192=DIRECTION('ref_axis',(0.,1.,0.));
#38193=DIRECTION('',(-1.,0.,0.));
#38194=DIRECTION('center_axis',(1.,0.,0.));
#38195=DIRECTION('ref_axis',(0.,1.,0.));
#38196=DIRECTION('',(-1.,0.,0.));
#38197=DIRECTION('center_axis',(1.,0.,0.));
#38198=DIRECTION('ref_axis',(0.,1.,0.));
#38199=DIRECTION('',(-1.,0.,0.));
#38200=DIRECTION('center_axis',(1.,0.,0.));
#38201=DIRECTION('ref_axis',(0.,1.,0.));
#38202=DIRECTION('',(-1.,0.,0.));
#38203=DIRECTION('center_axis',(1.,0.,0.));
#38204=DIRECTION('ref_axis',(0.,1.,0.));
#38205=DIRECTION('',(-1.,0.,0.));
#38206=DIRECTION('center_axis',(1.,0.,0.));
#38207=DIRECTION('ref_axis',(0.,1.,0.));
#38208=DIRECTION('',(-1.,0.,0.));
#38209=DIRECTION('center_axis',(1.,0.,0.));
#38210=DIRECTION('ref_axis',(0.,1.,0.));
#38211=DIRECTION('',(-1.,0.,0.));
#38212=DIRECTION('center_axis',(1.,0.,0.));
#38213=DIRECTION('ref_axis',(0.,1.,0.));
#38214=DIRECTION('',(-1.,0.,0.));
#38215=DIRECTION('center_axis',(1.,0.,0.));
#38216=DIRECTION('ref_axis',(0.,1.,-1.17400212830891E-12));
#38217=DIRECTION('',(1.,0.,0.));
#38218=DIRECTION('center_axis',(1.,0.,0.));
#38219=DIRECTION('ref_axis',(0.,1.,-1.17400212830891E-12));
#38220=DIRECTION('center_axis',(1.,0.,0.));
#38221=DIRECTION('ref_axis',(0.,1.,-1.17400212830891E-12));
#38222=DIRECTION('',(1.,0.,0.));
#38223=DIRECTION('center_axis',(1.,0.,0.));
#38224=DIRECTION('ref_axis',(0.,1.,-1.17400212830891E-12));
#38225=DIRECTION('',(1.,0.,0.));
#38226=DIRECTION('center_axis',(1.,0.,0.));
#38227=DIRECTION('ref_axis',(0.,1.,-1.17400212830891E-12));
#38228=DIRECTION('',(1.,0.,0.));
#38229=DIRECTION('center_axis',(1.,0.,0.));
#38230=DIRECTION('ref_axis',(0.,1.,-1.17400212830891E-12));
#38231=DIRECTION('',(1.,0.,0.));
#38232=DIRECTION('center_axis',(1.,0.,0.));
#38233=DIRECTION('ref_axis',(0.,1.,-1.17400212830891E-12));
#38234=DIRECTION('',(1.,0.,0.));
#38235=DIRECTION('center_axis',(1.,0.,0.));
#38236=DIRECTION('ref_axis',(0.,1.,-1.17400212830891E-12));
#38237=DIRECTION('',(1.,0.,0.));
#38238=DIRECTION('center_axis',(1.,0.,0.));
#38239=DIRECTION('ref_axis',(0.,1.,-1.17400212830891E-12));
#38240=DIRECTION('',(1.,0.,0.));
#38241=DIRECTION('center_axis',(1.,0.,0.));
#38242=DIRECTION('ref_axis',(0.,1.,-1.17400212830891E-12));
#38243=DIRECTION('',(1.,0.,0.));
#38244=DIRECTION('center_axis',(1.,0.,0.));
#38245=DIRECTION('ref_axis',(0.,1.,-1.17400212830891E-12));
#38246=DIRECTION('',(1.,0.,0.));
#38247=DIRECTION('center_axis',(1.,0.,0.));
#38248=DIRECTION('ref_axis',(0.,1.,-1.17400212830891E-12));
#38249=DIRECTION('',(1.,0.,0.));
#38250=DIRECTION('center_axis',(1.,0.,0.));
#38251=DIRECTION('ref_axis',(0.,1.,-1.17400212830891E-12));
#38252=DIRECTION('',(1.,0.,0.));
#38253=DIRECTION('center_axis',(1.,0.,0.));
#38254=DIRECTION('ref_axis',(0.,1.,-1.17400212830891E-12));
#38255=DIRECTION('',(1.,0.,0.));
#38256=DIRECTION('center_axis',(1.,0.,0.));
#38257=DIRECTION('ref_axis',(0.,1.,-1.17400212830891E-12));
#38258=DIRECTION('',(1.,0.,0.));
#38259=DIRECTION('center_axis',(1.,0.,0.));
#38260=DIRECTION('ref_axis',(0.,1.,-1.17400212830891E-12));
#38261=DIRECTION('',(1.,0.,0.));
#38262=DIRECTION('center_axis',(1.,0.,0.));
#38263=DIRECTION('ref_axis',(0.,1.,-1.17400212830891E-12));
#38264=DIRECTION('',(1.,0.,0.));
#38265=DIRECTION('center_axis',(1.,0.,0.));
#38266=DIRECTION('ref_axis',(0.,1.,-1.17400212830891E-12));
#38267=DIRECTION('',(1.,0.,0.));
#38268=DIRECTION('center_axis',(1.,0.,0.));
#38269=DIRECTION('ref_axis',(0.,1.,-1.17400212830891E-12));
#38270=DIRECTION('',(1.,0.,0.));
#38271=DIRECTION('center_axis',(1.,0.,0.));
#38272=DIRECTION('ref_axis',(0.,1.,-1.17400212830891E-12));
#38273=DIRECTION('',(1.,0.,0.));
#38274=DIRECTION('center_axis',(1.,0.,0.));
#38275=DIRECTION('ref_axis',(0.,1.,-1.17400212830891E-12));
#38276=DIRECTION('',(1.,0.,0.));
#38277=DIRECTION('center_axis',(1.,0.,0.));
#38278=DIRECTION('ref_axis',(0.,1.,-1.17400212830891E-12));
#38279=DIRECTION('',(1.,0.,0.));
#38280=DIRECTION('center_axis',(1.,0.,0.));
#38281=DIRECTION('ref_axis',(0.,1.,-1.17400212830891E-12));
#38282=DIRECTION('',(1.,0.,0.));
#38283=DIRECTION('center_axis',(1.,0.,0.));
#38284=DIRECTION('ref_axis',(0.,1.,-1.17400212830891E-12));
#38285=DIRECTION('',(1.,0.,0.));
#38286=DIRECTION('center_axis',(1.,0.,0.));
#38287=DIRECTION('ref_axis',(0.,1.,-1.17400212830891E-12));
#38288=DIRECTION('',(1.,0.,0.));
#38289=DIRECTION('center_axis',(1.,0.,0.));
#38290=DIRECTION('ref_axis',(0.,1.,-1.17400212830891E-12));
#38291=DIRECTION('',(1.,0.,0.));
#38292=DIRECTION('center_axis',(1.,0.,0.));
#38293=DIRECTION('ref_axis',(0.,1.,-1.17400212830891E-12));
#38294=DIRECTION('',(1.,0.,0.));
#38295=DIRECTION('center_axis',(1.,0.,0.));
#38296=DIRECTION('ref_axis',(0.,1.,-1.17400212830891E-12));
#38297=DIRECTION('',(1.,0.,0.));
#38298=DIRECTION('center_axis',(1.,0.,0.));
#38299=DIRECTION('ref_axis',(0.,1.,-1.17400212830891E-12));
#38300=DIRECTION('',(1.,0.,0.));
#38301=DIRECTION('center_axis',(1.,0.,0.));
#38302=DIRECTION('ref_axis',(0.,1.,-1.17400212830891E-12));
#38303=DIRECTION('',(1.,0.,0.));
#38304=DIRECTION('center_axis',(1.,0.,0.));
#38305=DIRECTION('ref_axis',(0.,1.,-1.17400212830891E-12));
#38306=DIRECTION('',(1.,0.,0.));
#38307=DIRECTION('center_axis',(1.,0.,0.));
#38308=DIRECTION('ref_axis',(0.,1.,-1.17400212830891E-12));
#38309=DIRECTION('',(1.,0.,0.));
#38310=DIRECTION('center_axis',(1.,0.,0.));
#38311=DIRECTION('ref_axis',(0.,1.,-1.17400212830891E-12));
#38312=DIRECTION('',(1.,0.,0.));
#38313=DIRECTION('center_axis',(1.,0.,0.));
#38314=DIRECTION('ref_axis',(0.,1.,-1.17400212830891E-12));
#38315=DIRECTION('',(1.,0.,0.));
#38316=DIRECTION('center_axis',(1.,0.,0.));
#38317=DIRECTION('ref_axis',(0.,1.,-1.17400212830891E-12));
#38318=DIRECTION('',(1.,0.,0.));
#38319=DIRECTION('center_axis',(1.,0.,0.));
#38320=DIRECTION('ref_axis',(0.,1.,-1.17400212830891E-12));
#38321=DIRECTION('',(1.,0.,0.));
#38322=DIRECTION('center_axis',(1.,0.,0.));
#38323=DIRECTION('ref_axis',(0.,1.,-1.17400212830891E-12));
#38324=DIRECTION('',(1.,0.,0.));
#38325=DIRECTION('center_axis',(1.,0.,0.));
#38326=DIRECTION('ref_axis',(0.,1.,-1.17400212830891E-12));
#38327=DIRECTION('',(1.,0.,0.));
#38328=DIRECTION('center_axis',(1.,0.,0.));
#38329=DIRECTION('ref_axis',(0.,1.,-1.17400212830891E-12));
#38330=DIRECTION('',(1.,0.,0.));
#38331=DIRECTION('center_axis',(1.,0.,0.));
#38332=DIRECTION('ref_axis',(0.,1.,-1.17400212830891E-12));
#38333=DIRECTION('',(1.,0.,0.));
#38334=DIRECTION('center_axis',(1.,0.,0.));
#38335=DIRECTION('ref_axis',(0.,1.,-1.17400212830891E-12));
#38336=DIRECTION('',(1.,0.,0.));
#38337=DIRECTION('center_axis',(1.,0.,0.));
#38338=DIRECTION('ref_axis',(0.,1.,-1.17400212830891E-12));
#38339=DIRECTION('',(1.,0.,0.));
#38340=DIRECTION('center_axis',(1.,0.,0.));
#38341=DIRECTION('ref_axis',(0.,1.,-1.17400212830891E-12));
#38342=DIRECTION('',(1.,0.,0.));
#38343=DIRECTION('center_axis',(1.,0.,0.));
#38344=DIRECTION('ref_axis',(0.,1.,-1.17400212830891E-12));
#38345=DIRECTION('',(1.,0.,0.));
#38346=DIRECTION('center_axis',(1.,0.,0.));
#38347=DIRECTION('ref_axis',(0.,1.,-1.17400212830891E-12));
#38348=DIRECTION('',(1.,0.,0.));
#38349=DIRECTION('center_axis',(1.,0.,0.));
#38350=DIRECTION('ref_axis',(0.,1.,-1.17400212830891E-12));
#38351=DIRECTION('',(1.,0.,0.));
#38352=DIRECTION('center_axis',(1.,0.,0.));
#38353=DIRECTION('ref_axis',(0.,1.,-1.17400212830891E-12));
#38354=DIRECTION('',(1.,0.,0.));
#38355=DIRECTION('center_axis',(1.,0.,0.));
#38356=DIRECTION('ref_axis',(0.,1.,-1.17400212830891E-12));
#38357=DIRECTION('',(1.,0.,0.));
#38358=DIRECTION('center_axis',(1.,0.,0.));
#38359=DIRECTION('ref_axis',(0.,1.,-1.17400212830891E-12));
#38360=DIRECTION('',(1.,0.,0.));
#38361=DIRECTION('center_axis',(1.,0.,0.));
#38362=DIRECTION('ref_axis',(0.,1.,-1.17400212830891E-12));
#38363=DIRECTION('',(1.,0.,0.));
#38364=DIRECTION('center_axis',(1.,0.,0.));
#38365=DIRECTION('ref_axis',(0.,1.,-1.17400212830891E-12));
#38366=DIRECTION('',(1.,0.,0.));
#38367=DIRECTION('center_axis',(1.,0.,0.));
#38368=DIRECTION('ref_axis',(0.,1.,-1.17400212830891E-12));
#38369=DIRECTION('',(1.,0.,0.));
#38370=DIRECTION('center_axis',(1.,0.,0.));
#38371=DIRECTION('ref_axis',(0.,1.,-1.17400212830891E-12));
#38372=DIRECTION('',(1.,0.,0.));
#38373=DIRECTION('center_axis',(1.,0.,0.));
#38374=DIRECTION('ref_axis',(0.,1.,-1.17400212830891E-12));
#38375=DIRECTION('',(1.,0.,0.));
#38376=DIRECTION('center_axis',(1.,0.,0.));
#38377=DIRECTION('ref_axis',(0.,1.,-1.17400212830891E-12));
#38378=DIRECTION('',(1.,0.,0.));
#38379=DIRECTION('center_axis',(1.,0.,0.));
#38380=DIRECTION('ref_axis',(0.,1.,-1.17400212830891E-12));
#38381=DIRECTION('',(1.,0.,0.));
#38382=DIRECTION('center_axis',(1.,0.,0.));
#38383=DIRECTION('ref_axis',(0.,1.,-1.17400212830891E-12));
#38384=DIRECTION('',(1.,0.,0.));
#38385=DIRECTION('center_axis',(1.,0.,0.));
#38386=DIRECTION('ref_axis',(0.,1.,-1.17400212830891E-12));
#38387=DIRECTION('',(1.,0.,0.));
#38388=DIRECTION('center_axis',(1.,0.,0.));
#38389=DIRECTION('ref_axis',(0.,1.,-1.17400212830891E-12));
#38390=DIRECTION('',(1.,0.,0.));
#38391=DIRECTION('center_axis',(1.,0.,0.));
#38392=DIRECTION('ref_axis',(0.,1.,-1.17400212830891E-12));
#38393=DIRECTION('',(1.,0.,0.));
#38394=DIRECTION('center_axis',(1.,0.,0.));
#38395=DIRECTION('ref_axis',(0.,1.,-1.17400212830891E-12));
#38396=DIRECTION('',(1.,0.,0.));
#38397=DIRECTION('center_axis',(1.,0.,0.));
#38398=DIRECTION('ref_axis',(0.,1.,-1.17400212830891E-12));
#38399=DIRECTION('',(1.,0.,0.));
#38400=DIRECTION('center_axis',(1.,0.,0.));
#38401=DIRECTION('ref_axis',(0.,1.,-1.17400212830891E-12));
#38402=DIRECTION('',(1.,0.,0.));
#38403=DIRECTION('center_axis',(1.,0.,0.));
#38404=DIRECTION('ref_axis',(0.,1.,-1.17400212830891E-12));
#38405=DIRECTION('',(1.,0.,0.));
#38406=DIRECTION('center_axis',(1.,0.,0.));
#38407=DIRECTION('ref_axis',(0.,1.,-1.17400212830891E-12));
#38408=DIRECTION('',(1.,0.,0.));
#38409=DIRECTION('center_axis',(1.,0.,0.));
#38410=DIRECTION('ref_axis',(0.,1.,-1.17400212830891E-12));
#38411=DIRECTION('',(1.,0.,0.));
#38412=DIRECTION('center_axis',(1.,0.,0.));
#38413=DIRECTION('ref_axis',(0.,1.,-1.17400212830891E-12));
#38414=DIRECTION('',(1.,0.,0.));
#38415=DIRECTION('center_axis',(1.,0.,0.));
#38416=DIRECTION('ref_axis',(0.,1.,-1.17400212830891E-12));
#38417=DIRECTION('',(1.,0.,0.));
#38418=DIRECTION('center_axis',(1.,0.,0.));
#38419=DIRECTION('ref_axis',(0.,1.,-1.17400212830891E-12));
#38420=DIRECTION('',(1.,0.,0.));
#38421=DIRECTION('center_axis',(1.,0.,0.));
#38422=DIRECTION('ref_axis',(0.,1.,-1.17400212830891E-12));
#38423=DIRECTION('',(1.,0.,0.));
#38424=DIRECTION('center_axis',(1.,0.,0.));
#38425=DIRECTION('ref_axis',(0.,0.,-1.));
#38426=DIRECTION('center_axis',(1.,0.,0.));
#38427=DIRECTION('ref_axis',(0.,1.,0.));
#38428=DIRECTION('center_axis',(1.,0.,0.));
#38429=DIRECTION('ref_axis',(0.,1.,0.));
#38430=DIRECTION('center_axis',(1.,0.,0.));
#38431=DIRECTION('ref_axis',(0.,0.,-1.));
#38432=DIRECTION('center_axis',(1.,0.,0.));
#38433=DIRECTION('ref_axis',(0.,1.,0.));
#38434=DIRECTION('center_axis',(1.,0.,0.));
#38435=DIRECTION('ref_axis',(0.,1.,0.));
#38436=DIRECTION('center_axis',(-1.,0.,0.));
#38437=DIRECTION('ref_axis',(0.,1.,-1.17400212830891E-12));
#38438=DIRECTION('center_axis',(1.,0.,0.));
#38439=DIRECTION('ref_axis',(0.,1.,-1.17400212830891E-12));
#38440=DIRECTION('center_axis',(1.,0.,0.));
#38441=DIRECTION('ref_axis',(0.,0.,-1.));
#38442=DIRECTION('center_axis',(0.,-1.,-1.22464679914735E-16));
#38443=DIRECTION('ref_axis',(0.,-1.22464679914735E-16,1.));
#38444=DIRECTION('center_axis',(-1.,0.,0.));
#38445=DIRECTION('ref_axis',(0.,1.,0.));
#38446=DIRECTION('center_axis',(1.,0.,0.));
#38447=DIRECTION('ref_axis',(0.,1.,0.));
#38448=DIRECTION('center_axis',(1.,0.,0.));
#38449=DIRECTION('ref_axis',(0.,1.,0.));
#38450=DIRECTION('center_axis',(-1.,0.,0.));
#38451=DIRECTION('ref_axis',(0.,0.,1.));
#38452=DIRECTION('center_axis',(1.,0.,0.));
#38453=DIRECTION('ref_axis',(0.,0.,-1.));
#38454=DIRECTION('center_axis',(0.,-0.443490878258566,0.896278885672002));
#38455=DIRECTION('ref_axis',(0.,-0.896278885672002,-0.443490878258566));
#38456=DIRECTION('',(-1.,0.,0.));
#38457=DIRECTION('',(0.,-0.896278885672002,-0.443490878258566));
#38458=DIRECTION('',(1.,0.,0.));
#38459=DIRECTION('',(0.,-0.896278885672002,-0.443490878258566));
#38460=DIRECTION('center_axis',(1.,0.,0.));
#38461=DIRECTION('ref_axis',(0.,-0.17364817766693,-0.984807753012208));
#38462=DIRECTION('center_axis',(-1.,0.,0.));
#38463=DIRECTION('ref_axis',(0.,1.,0.));
#38464=DIRECTION('',(0.,0.690543841286576,-0.723290538622745));
#38465=DIRECTION('center_axis',(0.,-0.723290538622745,-0.690543841286576));
#38466=DIRECTION('ref_axis',(0.,0.690543841286576,-0.723290538622745));
#38467=DIRECTION('',(1.,0.,0.));
#38468=DIRECTION('',(0.,0.690543841286576,-0.723290538622745));
#38469=DIRECTION('center_axis',(1.,0.,0.));
#38470=DIRECTION('ref_axis',(0.,-0.17364817766693,-0.984807753012208));
#38471=DIRECTION('center_axis',(1.,0.,0.));
#38472=DIRECTION('ref_axis',(0.,1.,0.));
#38473=DIRECTION('center_axis',(0.,-0.281116060120938,0.959673778292437));
#38474=DIRECTION('ref_axis',(0.,-0.959673778292437,-0.281116060120938));
#38475=DIRECTION('',(-1.,0.,0.));
#38476=DIRECTION('',(0.,-0.959673778292437,-0.281116060120938));
#38477=DIRECTION('',(1.,0.,0.));
#38478=DIRECTION('',(0.,-0.959673778292437,-0.281116060120938));
#38479=DIRECTION('center_axis',(1.,0.,0.));
#38480=DIRECTION('ref_axis',(0.,-0.342020143325669,-0.939692620785908));
#38481=DIRECTION('center_axis',(-1.,0.,0.));
#38482=DIRECTION('ref_axis',(0.,1.,0.));
#38483=DIRECTION('',(0.,0.554454844738279,-0.832213809754591));
#38484=DIRECTION('center_axis',(0.,-0.832213809754591,-0.554454844738279));
#38485=DIRECTION('ref_axis',(0.,0.554454844738279,-0.832213809754591));
#38486=DIRECTION('',(1.,0.,0.));
#38487=DIRECTION('',(0.,0.554454844738279,-0.832213809754591));
#38488=DIRECTION('center_axis',(1.,0.,0.));
#38489=DIRECTION('ref_axis',(0.,-0.342020143325669,-0.939692620785908));
#38490=DIRECTION('center_axis',(1.,0.,0.));
#38491=DIRECTION('ref_axis',(0.,1.,0.));
#38492=DIRECTION('center_axis',(0.,-0.110199672748126,0.993909468777819));
#38493=DIRECTION('ref_axis',(0.,-0.993909468777819,-0.110199672748126));
#38494=DIRECTION('',(-1.,0.,0.));
#38495=DIRECTION('',(0.,-0.993909468777819,-0.110199672748126));
#38496=DIRECTION('',(1.,0.,0.));
#38497=DIRECTION('',(0.,-0.993909468777819,-0.110199672748126));
#38498=DIRECTION('center_axis',(1.,0.,0.));
#38499=DIRECTION('ref_axis',(0.,-0.5,-0.866025403784438));
#38500=DIRECTION('center_axis',(-1.,0.,0.));
#38501=DIRECTION('ref_axis',(0.,1.,0.));
#38502=DIRECTION('',(0.,0.401519018300299,-0.915850685397551));
#38503=DIRECTION('center_axis',(0.,-0.915850685397551,-0.401519018300299));
#38504=DIRECTION('ref_axis',(0.,0.401519018300299,-0.915850685397551));
#38505=DIRECTION('',(1.,0.,0.));
#38506=DIRECTION('',(0.,0.401519018300299,-0.915850685397551));
#38507=DIRECTION('center_axis',(1.,0.,0.));
#38508=DIRECTION('ref_axis',(0.,-0.5,-0.866025403784438));
#38509=DIRECTION('center_axis',(1.,0.,0.));
#38510=DIRECTION('ref_axis',(0.,1.,0.));
#38511=DIRECTION('center_axis',(0.,0.0640650759174117,0.997945722996845));
#38512=DIRECTION('ref_axis',(0.,-0.997945722996845,0.0640650759174117));
#38513=DIRECTION('',(-1.,0.,0.));
#38514=DIRECTION('',(0.,-0.997945722996845,0.0640650759174117));
#38515=DIRECTION('',(1.,0.,0.));
#38516=DIRECTION('',(0.,-0.997945722996845,0.0640650759174117));
#38517=DIRECTION('center_axis',(1.,0.,0.));
#38518=DIRECTION('ref_axis',(0.,-0.64278760968654,-0.766044443118978));
#38519=DIRECTION('center_axis',(-1.,0.,0.));
#38520=DIRECTION('ref_axis',(0.,1.,0.));
#38521=DIRECTION('',(0.,0.236383239669692,-0.971659901407515));
#38522=DIRECTION('center_axis',(0.,-0.971659901407515,-0.236383239669692));
#38523=DIRECTION('ref_axis',(0.,0.236383239669692,-0.971659901407515));
#38524=DIRECTION('',(1.,0.,0.));
#38525=DIRECTION('',(0.,0.236383239669692,-0.971659901407515));
#38526=DIRECTION('center_axis',(1.,0.,0.));
#38527=DIRECTION('ref_axis',(0.,-0.64278760968654,-0.766044443118978));
#38528=DIRECTION('center_axis',(1.,0.,0.));
#38529=DIRECTION('ref_axis',(0.,1.,0.));
#38530=DIRECTION('center_axis',(0.,0.236383239669692,0.971659901407515));
#38531=DIRECTION('ref_axis',(0.,-0.971659901407515,0.236383239669692));
#38532=DIRECTION('',(-1.,0.,0.));
#38533=DIRECTION('',(0.,-0.971659901407515,0.236383239669692));
#38534=DIRECTION('',(1.,0.,0.));
#38535=DIRECTION('',(0.,-0.971659901407515,0.236383239669692));
#38536=DIRECTION('center_axis',(1.,0.,0.));
#38537=DIRECTION('ref_axis',(0.,-0.766044443118978,-0.642787609686539));
#38538=DIRECTION('center_axis',(-1.,0.,0.));
#38539=DIRECTION('ref_axis',(0.,1.,0.));
#38540=DIRECTION('',(0.,0.0640650759174113,-0.997945722996845));
#38541=DIRECTION('center_axis',(0.,-0.997945722996845,-0.0640650759174113));
#38542=DIRECTION('ref_axis',(0.,0.0640650759174113,-0.997945722996845));
#38543=DIRECTION('',(1.,0.,0.));
#38544=DIRECTION('',(0.,0.0640650759174113,-0.997945722996845));
#38545=DIRECTION('center_axis',(1.,0.,0.));
#38546=DIRECTION('ref_axis',(0.,-0.766044443118978,-0.642787609686539));
#38547=DIRECTION('center_axis',(1.,0.,0.));
#38548=DIRECTION('ref_axis',(0.,1.,0.));
#38549=DIRECTION('center_axis',(0.,0.4015190183003,0.915850685397551));
#38550=DIRECTION('ref_axis',(0.,-0.915850685397551,0.401519018300299));
#38551=DIRECTION('',(-1.,0.,0.));
#38552=DIRECTION('',(0.,-0.915850685397551,0.401519018300299));
#38553=DIRECTION('',(1.,0.,0.));
#38554=DIRECTION('',(0.,-0.915850685397551,0.401519018300299));
#38555=DIRECTION('center_axis',(1.,0.,0.));
#38556=DIRECTION('ref_axis',(0.,-0.866025403784439,-0.5));
#38557=DIRECTION('center_axis',(-1.,0.,0.));
#38558=DIRECTION('ref_axis',(0.,1.,0.));
#38559=DIRECTION('',(0.,-0.110199672748127,-0.993909468777819));
#38560=DIRECTION('center_axis',(0.,-0.993909468777819,0.110199672748127));
#38561=DIRECTION('ref_axis',(0.,-0.110199672748127,-0.993909468777819));
#38562=DIRECTION('',(1.,0.,0.));
#38563=DIRECTION('',(0.,-0.110199672748127,-0.993909468777819));
#38564=DIRECTION('center_axis',(1.,0.,0.));
#38565=DIRECTION('ref_axis',(0.,-0.866025403784439,-0.5));
#38566=DIRECTION('center_axis',(1.,0.,0.));
#38567=DIRECTION('ref_axis',(0.,1.,0.));
#38568=DIRECTION('center_axis',(0.,0.55445484473828,0.832213809754591));
#38569=DIRECTION('ref_axis',(0.,-0.83221380975459,0.55445484473828));
#38570=DIRECTION('',(-1.,0.,0.));
#38571=DIRECTION('',(0.,-0.83221380975459,0.55445484473828));
#38572=DIRECTION('',(1.,0.,0.));
#38573=DIRECTION('',(0.,-0.83221380975459,0.55445484473828));
#38574=DIRECTION('center_axis',(1.,0.,0.));
#38575=DIRECTION('ref_axis',(0.,-0.939692620785909,-0.342020143325668));
#38576=DIRECTION('center_axis',(-1.,0.,0.));
#38577=DIRECTION('ref_axis',(0.,1.,0.));
#38578=DIRECTION('',(0.,-0.281116060120939,-0.959673778292436));
#38579=DIRECTION('center_axis',(0.,-0.959673778292436,0.281116060120939));
#38580=DIRECTION('ref_axis',(0.,-0.281116060120939,-0.959673778292436));
#38581=DIRECTION('',(1.,0.,0.));
#38582=DIRECTION('',(0.,-0.281116060120939,-0.959673778292436));
#38583=DIRECTION('center_axis',(1.,0.,0.));
#38584=DIRECTION('ref_axis',(0.,-0.939692620785909,-0.342020143325668));
#38585=DIRECTION('center_axis',(1.,0.,0.));
#38586=DIRECTION('ref_axis',(0.,1.,0.));
#38587=DIRECTION('center_axis',(0.,0.690543841286576,0.723290538622745));
#38588=DIRECTION('ref_axis',(0.,-0.723290538622744,0.690543841286576));
#38589=DIRECTION('',(-1.,0.,0.));
#38590=DIRECTION('',(0.,-0.723290538622744,0.690543841286576));
#38591=DIRECTION('',(1.,0.,0.));
#38592=DIRECTION('',(0.,-0.723290538622744,0.690543841286576));
#38593=DIRECTION('center_axis',(1.,0.,0.));
#38594=DIRECTION('ref_axis',(0.,-0.984807753012208,-0.17364817766693));
#38595=DIRECTION('center_axis',(-1.,0.,0.));
#38596=DIRECTION('ref_axis',(0.,1.,0.));
#38597=DIRECTION('',(0.,-0.443490878258566,-0.896278885672002));
#38598=DIRECTION('center_axis',(0.,-0.896278885672002,0.443490878258566));
#38599=DIRECTION('ref_axis',(0.,-0.443490878258566,-0.896278885672002));
#38600=DIRECTION('',(1.,0.,0.));
#38601=DIRECTION('',(0.,-0.443490878258566,-0.896278885672002));
#38602=DIRECTION('center_axis',(1.,0.,0.));
#38603=DIRECTION('ref_axis',(0.,-0.984807753012208,-0.17364817766693));
#38604=DIRECTION('center_axis',(1.,0.,0.));
#38605=DIRECTION('ref_axis',(0.,1.,0.));
#38606=DIRECTION('center_axis',(0.,0.805651012649424,0.592390450477519));
#38607=DIRECTION('ref_axis',(0.,-0.592390450477519,0.805651012649424));
#38608=DIRECTION('',(-1.,0.,0.));
#38609=DIRECTION('',(0.,-0.592390450477519,0.805651012649424));
#38610=DIRECTION('',(1.,0.,0.));
#38611=DIRECTION('',(0.,-0.592390450477519,0.805651012649424));
#38612=DIRECTION('center_axis',(1.,0.,0.));
#38613=DIRECTION('ref_axis',(0.,-1.,1.83697019872103E-16));
#38614=DIRECTION('center_axis',(-1.,0.,0.));
#38615=DIRECTION('ref_axis',(0.,1.,0.));
#38616=DIRECTION('',(0.,-0.592390450477519,-0.805651012649424));
#38617=DIRECTION('center_axis',(0.,-0.805651012649424,0.592390450477519));
#38618=DIRECTION('ref_axis',(0.,-0.592390450477519,-0.805651012649424));
#38619=DIRECTION('',(1.,0.,0.));
#38620=DIRECTION('',(0.,-0.592390450477519,-0.805651012649424));
#38621=DIRECTION('center_axis',(1.,0.,0.));
#38622=DIRECTION('ref_axis',(0.,-1.,1.83697019872103E-16));
#38623=DIRECTION('center_axis',(1.,0.,0.));
#38624=DIRECTION('ref_axis',(0.,1.,0.));
#38625=DIRECTION('center_axis',(0.,0.896278885672002,0.443490878258566));
#38626=DIRECTION('ref_axis',(0.,-0.443490878258566,0.896278885672002));
#38627=DIRECTION('',(-1.,0.,0.));
#38628=DIRECTION('',(0.,-0.443490878258566,0.896278885672002));
#38629=DIRECTION('',(1.,0.,0.));
#38630=DIRECTION('',(0.,-0.443490878258566,0.896278885672002));
#38631=DIRECTION('center_axis',(1.,0.,0.));
#38632=DIRECTION('ref_axis',(0.,-0.984807753012208,0.17364817766693));
#38633=DIRECTION('center_axis',(-1.,0.,0.));
#38634=DIRECTION('ref_axis',(0.,1.,0.));
#38635=DIRECTION('',(0.,-0.723290538622745,-0.690543841286576));
#38636=DIRECTION('center_axis',(0.,-0.690543841286576,0.723290538622745));
#38637=DIRECTION('ref_axis',(0.,-0.723290538622745,-0.690543841286576));
#38638=DIRECTION('',(1.,0.,0.));
#38639=DIRECTION('',(0.,-0.723290538622745,-0.690543841286576));
#38640=DIRECTION('center_axis',(1.,0.,0.));
#38641=DIRECTION('ref_axis',(0.,-0.984807753012208,0.17364817766693));
#38642=DIRECTION('center_axis',(1.,0.,0.));
#38643=DIRECTION('ref_axis',(0.,1.,0.));
#38644=DIRECTION('center_axis',(0.,0.959673778292437,0.281116060120938));
#38645=DIRECTION('ref_axis',(0.,-0.281116060120938,0.959673778292437));
#38646=DIRECTION('',(-1.,0.,0.));
#38647=DIRECTION('',(0.,-0.281116060120938,0.959673778292437));
#38648=DIRECTION('',(1.,0.,0.));
#38649=DIRECTION('',(0.,-0.281116060120938,0.959673778292437));
#38650=DIRECTION('center_axis',(1.,0.,0.));
#38651=DIRECTION('ref_axis',(0.,-0.939692620785908,0.342020143325669));
#38652=DIRECTION('center_axis',(-1.,0.,0.));
#38653=DIRECTION('ref_axis',(0.,1.,0.));
#38654=DIRECTION('',(0.,-0.832213809754591,-0.554454844738279));
#38655=DIRECTION('center_axis',(0.,-0.554454844738279,0.832213809754591));
#38656=DIRECTION('ref_axis',(0.,-0.832213809754591,-0.554454844738279));
#38657=DIRECTION('',(1.,0.,0.));
#38658=DIRECTION('',(0.,-0.832213809754591,-0.554454844738279));
#38659=DIRECTION('center_axis',(1.,0.,0.));
#38660=DIRECTION('ref_axis',(0.,-0.939692620785908,0.342020143325669));
#38661=DIRECTION('center_axis',(1.,0.,0.));
#38662=DIRECTION('ref_axis',(0.,1.,0.));
#38663=DIRECTION('center_axis',(0.,0.993909468777819,0.110199672748126));
#38664=DIRECTION('ref_axis',(0.,-0.110199672748126,0.993909468777819));
#38665=DIRECTION('',(-1.,0.,0.));
#38666=DIRECTION('',(0.,-0.110199672748126,0.993909468777819));
#38667=DIRECTION('',(1.,0.,0.));
#38668=DIRECTION('',(0.,-0.110199672748126,0.993909468777819));
#38669=DIRECTION('center_axis',(1.,0.,0.));
#38670=DIRECTION('ref_axis',(0.,-0.866025403784438,0.5));
#38671=DIRECTION('center_axis',(-1.,0.,0.));
#38672=DIRECTION('ref_axis',(0.,1.,0.));
#38673=DIRECTION('',(0.,-0.915850685397551,-0.401519018300299));
#38674=DIRECTION('center_axis',(0.,-0.401519018300299,0.915850685397551));
#38675=DIRECTION('ref_axis',(0.,-0.915850685397551,-0.401519018300299));
#38676=DIRECTION('',(1.,0.,0.));
#38677=DIRECTION('',(0.,-0.915850685397551,-0.401519018300299));
#38678=DIRECTION('center_axis',(1.,0.,0.));
#38679=DIRECTION('ref_axis',(0.,-0.866025403784438,0.5));
#38680=DIRECTION('center_axis',(1.,0.,0.));
#38681=DIRECTION('ref_axis',(0.,1.,0.));
#38682=DIRECTION('center_axis',(0.,0.997945722996845,-0.0640650759174116));
#38683=DIRECTION('ref_axis',(0.,0.0640650759174116,0.997945722996845));
#38684=DIRECTION('',(-1.,0.,0.));
#38685=DIRECTION('',(0.,0.0640650759174116,0.997945722996845));
#38686=DIRECTION('',(1.,0.,0.));
#38687=DIRECTION('',(0.,0.0640650759174116,0.997945722996845));
#38688=DIRECTION('center_axis',(1.,0.,0.));
#38689=DIRECTION('ref_axis',(0.,-0.766044443118978,0.642787609686539));
#38690=DIRECTION('center_axis',(-1.,0.,0.));
#38691=DIRECTION('ref_axis',(0.,1.,0.));
#38692=DIRECTION('',(0.,-0.971659901407515,-0.236383239669692));
#38693=DIRECTION('center_axis',(0.,-0.236383239669692,0.971659901407515));
#38694=DIRECTION('ref_axis',(0.,-0.971659901407515,-0.236383239669692));
#38695=DIRECTION('',(1.,0.,0.));
#38696=DIRECTION('',(0.,-0.971659901407515,-0.236383239669692));
#38697=DIRECTION('center_axis',(1.,0.,0.));
#38698=DIRECTION('ref_axis',(0.,-0.766044443118978,0.642787609686539));
#38699=DIRECTION('center_axis',(1.,0.,0.));
#38700=DIRECTION('ref_axis',(0.,1.,0.));
#38701=DIRECTION('center_axis',(0.,0.971659901407515,-0.236383239669692));
#38702=DIRECTION('ref_axis',(0.,0.236383239669692,0.971659901407515));
#38703=DIRECTION('',(-1.,0.,0.));
#38704=DIRECTION('',(0.,0.236383239669692,0.971659901407515));
#38705=DIRECTION('',(1.,0.,0.));
#38706=DIRECTION('',(0.,0.236383239669692,0.971659901407515));
#38707=DIRECTION('center_axis',(1.,0.,0.));
#38708=DIRECTION('ref_axis',(0.,-0.642787609686539,0.766044443118978));
#38709=DIRECTION('center_axis',(-1.,0.,0.));
#38710=DIRECTION('ref_axis',(0.,1.,0.));
#38711=DIRECTION('',(0.,-0.997945722996845,-0.0640650759174114));
#38712=DIRECTION('center_axis',(0.,-0.0640650759174115,0.997945722996845));
#38713=DIRECTION('ref_axis',(0.,-0.997945722996845,-0.0640650759174114));
#38714=DIRECTION('',(1.,0.,0.));
#38715=DIRECTION('',(0.,-0.997945722996845,-0.0640650759174114));
#38716=DIRECTION('center_axis',(1.,0.,0.));
#38717=DIRECTION('ref_axis',(0.,-0.642787609686539,0.766044443118978));
#38718=DIRECTION('center_axis',(1.,0.,0.));
#38719=DIRECTION('ref_axis',(0.,1.,0.));
#38720=DIRECTION('center_axis',(0.,0.915850685397551,-0.4015190183003));
#38721=DIRECTION('ref_axis',(0.,0.4015190183003,0.915850685397551));
#38722=DIRECTION('',(-1.,0.,0.));
#38723=DIRECTION('',(0.,0.4015190183003,0.915850685397551));
#38724=DIRECTION('',(1.,0.,0.));
#38725=DIRECTION('',(0.,0.4015190183003,0.915850685397551));
#38726=DIRECTION('center_axis',(1.,0.,0.));
#38727=DIRECTION('ref_axis',(0.,-0.5,0.866025403784439));
#38728=DIRECTION('center_axis',(-1.,0.,0.));
#38729=DIRECTION('ref_axis',(0.,1.,0.));
#38730=DIRECTION('',(0.,-0.993909468777818,0.110199672748127));
#38731=DIRECTION('center_axis',(0.,0.110199672748127,0.993909468777819));
#38732=DIRECTION('ref_axis',(0.,-0.993909468777818,0.110199672748127));
#38733=DIRECTION('',(1.,0.,0.));
#38734=DIRECTION('',(0.,-0.993909468777818,0.110199672748127));
#38735=DIRECTION('center_axis',(1.,0.,0.));
#38736=DIRECTION('ref_axis',(0.,-0.5,0.866025403784439));
#38737=DIRECTION('center_axis',(1.,0.,0.));
#38738=DIRECTION('ref_axis',(0.,1.,0.));
#38739=DIRECTION('center_axis',(0.,0.832213809754591,-0.55445484473828));
#38740=DIRECTION('ref_axis',(0.,0.55445484473828,0.832213809754591));
#38741=DIRECTION('',(-1.,0.,0.));
#38742=DIRECTION('',(0.,0.55445484473828,0.832213809754591));
#38743=DIRECTION('',(1.,0.,0.));
#38744=DIRECTION('',(0.,0.55445484473828,0.832213809754591));
#38745=DIRECTION('center_axis',(1.,0.,0.));
#38746=DIRECTION('ref_axis',(0.,-0.342020143325669,0.939692620785909));
#38747=DIRECTION('center_axis',(-1.,0.,0.));
#38748=DIRECTION('ref_axis',(0.,1.,0.));
#38749=DIRECTION('',(0.,-0.959673778292437,0.281116060120939));
#38750=DIRECTION('center_axis',(0.,0.281116060120939,0.959673778292437));
#38751=DIRECTION('ref_axis',(0.,-0.959673778292437,0.281116060120939));
#38752=DIRECTION('',(1.,0.,0.));
#38753=DIRECTION('',(0.,-0.959673778292437,0.281116060120939));
#38754=DIRECTION('center_axis',(1.,0.,0.));
#38755=DIRECTION('ref_axis',(0.,-0.342020143325669,0.939692620785909));
#38756=DIRECTION('center_axis',(1.,0.,0.));
#38757=DIRECTION('ref_axis',(0.,1.,0.));
#38758=DIRECTION('center_axis',(0.,0.723290538622745,-0.690543841286576));
#38759=DIRECTION('ref_axis',(0.,0.690543841286576,0.723290538622745));
#38760=DIRECTION('',(-1.,0.,0.));
#38761=DIRECTION('',(0.,0.690543841286576,0.723290538622745));
#38762=DIRECTION('',(1.,0.,0.));
#38763=DIRECTION('',(0.,0.690543841286576,0.723290538622745));
#38764=DIRECTION('center_axis',(1.,0.,0.));
#38765=DIRECTION('ref_axis',(0.,-0.17364817766693,0.984807753012208));
#38766=DIRECTION('center_axis',(-1.,0.,0.));
#38767=DIRECTION('ref_axis',(0.,1.,0.));
#38768=DIRECTION('',(0.,-0.896278885672002,0.443490878258566));
#38769=DIRECTION('center_axis',(0.,0.443490878258566,0.896278885672002));
#38770=DIRECTION('ref_axis',(0.,-0.896278885672002,0.443490878258566));
#38771=DIRECTION('',(1.,0.,0.));
#38772=DIRECTION('',(0.,-0.896278885672002,0.443490878258566));
#38773=DIRECTION('center_axis',(1.,0.,0.));
#38774=DIRECTION('ref_axis',(0.,-0.17364817766693,0.984807753012208));
#38775=DIRECTION('center_axis',(1.,0.,0.));
#38776=DIRECTION('ref_axis',(0.,1.,0.));
#38777=DIRECTION('center_axis',(0.,0.592390450477519,-0.805651012649424));
#38778=DIRECTION('ref_axis',(0.,0.805651012649424,0.592390450477519));
#38779=DIRECTION('',(-1.,0.,0.));
#38780=DIRECTION('',(0.,0.805651012649424,0.592390450477519));
#38781=DIRECTION('',(1.,0.,0.));
#38782=DIRECTION('',(0.,0.805651012649424,0.592390450477519));
#38783=DIRECTION('center_axis',(1.,0.,0.));
#38784=DIRECTION('ref_axis',(0.,1.22464679914735E-16,1.));
#38785=DIRECTION('center_axis',(-1.,0.,0.));
#38786=DIRECTION('ref_axis',(0.,1.,0.));
#38787=DIRECTION('',(0.,-0.805651012649424,0.592390450477519));
#38788=DIRECTION('center_axis',(-1.,0.,0.));
#38789=DIRECTION('ref_axis',(0.,1.,0.));
#38790=DIRECTION('center_axis',(0.,0.592390450477519,0.805651012649424));
#38791=DIRECTION('ref_axis',(0.,-0.805651012649424,0.592390450477519));
#38792=DIRECTION('',(1.,0.,0.));
#38793=DIRECTION('',(0.,-0.805651012649424,0.592390450477519));
#38794=DIRECTION('center_axis',(1.,0.,0.));
#38795=DIRECTION('ref_axis',(0.,1.22464679914735E-16,1.));
#38796=DIRECTION('center_axis',(1.,0.,0.));
#38797=DIRECTION('ref_axis',(0.,1.,0.));
#38798=DIRECTION('center_axis',(1.,0.,0.));
#38799=DIRECTION('ref_axis',(0.,1.,0.));
#38800=DIRECTION('center_axis',(0.,0.443490878258565,-0.896278885672002));
#38801=DIRECTION('ref_axis',(0.,0.896278885672002,0.443490878258565));
#38802=DIRECTION('',(-1.,0.,0.));
#38803=DIRECTION('',(0.,0.896278885672002,0.443490878258565));
#38804=DIRECTION('',(1.,0.,0.));
#38805=DIRECTION('',(0.,0.896278885672002,0.443490878258565));
#38806=DIRECTION('center_axis',(1.,0.,0.));
#38807=DIRECTION('ref_axis',(0.,0.173648177666931,0.984807753012208));
#38808=DIRECTION('center_axis',(-1.,0.,0.));
#38809=DIRECTION('ref_axis',(0.,1.,0.));
#38810=DIRECTION('',(0.,-0.690543841286576,0.723290538622745));
#38811=DIRECTION('center_axis',(0.,0.723290538622745,0.690543841286576));
#38812=DIRECTION('ref_axis',(0.,-0.690543841286576,0.723290538622745));
#38813=DIRECTION('',(1.,0.,0.));
#38814=DIRECTION('',(0.,-0.690543841286576,0.723290538622745));
#38815=DIRECTION('center_axis',(1.,0.,0.));
#38816=DIRECTION('ref_axis',(0.,0.173648177666931,0.984807753012208));
#38817=DIRECTION('center_axis',(1.,0.,0.));
#38818=DIRECTION('ref_axis',(0.,1.,0.));
#38819=DIRECTION('center_axis',(0.,0.281116060120939,-0.959673778292437));
#38820=DIRECTION('ref_axis',(0.,0.959673778292437,0.281116060120938));
#38821=DIRECTION('',(-1.,0.,0.));
#38822=DIRECTION('',(0.,0.959673778292437,0.281116060120938));
#38823=DIRECTION('',(1.,0.,0.));
#38824=DIRECTION('',(0.,0.959673778292437,0.281116060120938));
#38825=DIRECTION('center_axis',(1.,0.,0.));
#38826=DIRECTION('ref_axis',(0.,0.342020143325669,0.939692620785908));
#38827=DIRECTION('center_axis',(-1.,0.,0.));
#38828=DIRECTION('ref_axis',(0.,1.,0.));
#38829=DIRECTION('',(0.,-0.554454844738279,0.832213809754591));
#38830=DIRECTION('center_axis',(0.,0.832213809754591,0.55445484473828));
#38831=DIRECTION('ref_axis',(0.,-0.554454844738279,0.832213809754591));
#38832=DIRECTION('',(1.,0.,0.));
#38833=DIRECTION('',(0.,-0.554454844738279,0.832213809754591));
#38834=DIRECTION('center_axis',(1.,0.,0.));
#38835=DIRECTION('ref_axis',(0.,0.342020143325669,0.939692620785908));
#38836=DIRECTION('center_axis',(1.,0.,0.));
#38837=DIRECTION('ref_axis',(0.,1.,0.));
#38838=DIRECTION('center_axis',(0.,0.110199672748127,-0.993909468777819));
#38839=DIRECTION('ref_axis',(0.,0.993909468777819,0.110199672748127));
#38840=DIRECTION('',(-1.,0.,0.));
#38841=DIRECTION('',(0.,0.993909468777819,0.110199672748127));
#38842=DIRECTION('',(1.,0.,0.));
#38843=DIRECTION('',(0.,0.993909468777819,0.110199672748127));
#38844=DIRECTION('center_axis',(1.,0.,0.));
#38845=DIRECTION('ref_axis',(0.,0.5,0.866025403784439));
#38846=DIRECTION('center_axis',(-1.,0.,0.));
#38847=DIRECTION('ref_axis',(0.,1.,0.));
#38848=DIRECTION('',(0.,-0.4015190183003,0.915850685397551));
#38849=DIRECTION('center_axis',(0.,0.915850685397551,0.4015190183003));
#38850=DIRECTION('ref_axis',(0.,-0.4015190183003,0.915850685397551));
#38851=DIRECTION('',(1.,0.,0.));
#38852=DIRECTION('',(0.,-0.4015190183003,0.915850685397551));
#38853=DIRECTION('center_axis',(1.,0.,0.));
#38854=DIRECTION('ref_axis',(0.,0.5,0.866025403784439));
#38855=DIRECTION('center_axis',(1.,0.,0.));
#38856=DIRECTION('ref_axis',(0.,1.,0.));
#38857=DIRECTION('center_axis',(0.,-0.0640650759174116,-0.997945722996845));
#38858=DIRECTION('ref_axis',(0.,0.997945722996845,-0.0640650759174116));
#38859=DIRECTION('',(-1.,0.,0.));
#38860=DIRECTION('',(0.,0.997945722996845,-0.0640650759174116));
#38861=DIRECTION('',(1.,0.,0.));
#38862=DIRECTION('',(0.,0.997945722996845,-0.0640650759174116));
#38863=DIRECTION('center_axis',(1.,0.,0.));
#38864=DIRECTION('ref_axis',(0.,0.642787609686539,0.766044443118978));
#38865=DIRECTION('center_axis',(-1.,0.,0.));
#38866=DIRECTION('ref_axis',(0.,1.,0.));
#38867=DIRECTION('',(0.,-0.236383239669692,0.971659901407515));
#38868=DIRECTION('center_axis',(0.,0.971659901407515,0.236383239669692));
#38869=DIRECTION('ref_axis',(0.,-0.236383239669692,0.971659901407515));
#38870=DIRECTION('',(1.,0.,0.));
#38871=DIRECTION('',(0.,-0.236383239669692,0.971659901407515));
#38872=DIRECTION('center_axis',(1.,0.,0.));
#38873=DIRECTION('ref_axis',(0.,0.642787609686539,0.766044443118978));
#38874=DIRECTION('center_axis',(1.,0.,0.));
#38875=DIRECTION('ref_axis',(0.,1.,0.));
#38876=DIRECTION('center_axis',(0.,-0.236383239669692,-0.971659901407515));
#38877=DIRECTION('ref_axis',(0.,0.971659901407515,-0.236383239669692));
#38878=DIRECTION('',(-1.,0.,0.));
#38879=DIRECTION('',(0.,0.971659901407515,-0.236383239669692));
#38880=DIRECTION('',(1.,0.,0.));
#38881=DIRECTION('',(0.,0.971659901407515,-0.236383239669692));
#38882=DIRECTION('center_axis',(1.,0.,0.));
#38883=DIRECTION('ref_axis',(0.,0.766044443118978,0.642787609686539));
#38884=DIRECTION('center_axis',(-1.,0.,0.));
#38885=DIRECTION('ref_axis',(0.,1.,0.));
#38886=DIRECTION('',(0.,-0.0640650759174115,0.997945722996845));
#38887=DIRECTION('center_axis',(0.,0.997945722996845,0.0640650759174115));
#38888=DIRECTION('ref_axis',(0.,-0.0640650759174115,0.997945722996845));
#38889=DIRECTION('',(1.,0.,0.));
#38890=DIRECTION('',(0.,-0.0640650759174115,0.997945722996845));
#38891=DIRECTION('center_axis',(1.,0.,0.));
#38892=DIRECTION('ref_axis',(0.,0.766044443118978,0.642787609686539));
#38893=DIRECTION('center_axis',(1.,0.,0.));
#38894=DIRECTION('ref_axis',(0.,1.,0.));
#38895=DIRECTION('center_axis',(0.,-0.4015190183003,-0.915850685397551));
#38896=DIRECTION('ref_axis',(0.,0.915850685397551,-0.4015190183003));
#38897=DIRECTION('',(-1.,0.,0.));
#38898=DIRECTION('',(0.,0.915850685397551,-0.4015190183003));
#38899=DIRECTION('',(1.,0.,0.));
#38900=DIRECTION('',(0.,0.915850685397551,-0.4015190183003));
#38901=DIRECTION('center_axis',(1.,0.,0.));
#38902=DIRECTION('ref_axis',(0.,0.866025403784439,0.5));
#38903=DIRECTION('center_axis',(-1.,0.,0.));
#38904=DIRECTION('ref_axis',(0.,1.,0.));
#38905=DIRECTION('',(0.,0.110199672748127,0.993909468777819));
#38906=DIRECTION('center_axis',(0.,0.993909468777819,-0.110199672748127));
#38907=DIRECTION('ref_axis',(0.,0.110199672748127,0.993909468777819));
#38908=DIRECTION('',(1.,0.,0.));
#38909=DIRECTION('',(0.,0.110199672748127,0.993909468777819));
#38910=DIRECTION('center_axis',(1.,0.,0.));
#38911=DIRECTION('ref_axis',(0.,0.866025403784439,0.5));
#38912=DIRECTION('center_axis',(1.,0.,0.));
#38913=DIRECTION('ref_axis',(0.,1.,0.));
#38914=DIRECTION('center_axis',(0.,-0.55445484473828,-0.832213809754591));
#38915=DIRECTION('ref_axis',(0.,0.832213809754591,-0.554454844738279));
#38916=DIRECTION('',(-1.,0.,0.));
#38917=DIRECTION('',(0.,0.832213809754591,-0.554454844738279));
#38918=DIRECTION('',(1.,0.,0.));
#38919=DIRECTION('',(0.,0.832213809754591,-0.554454844738279));
#38920=DIRECTION('center_axis',(1.,0.,0.));
#38921=DIRECTION('ref_axis',(0.,0.939692620785908,0.342020143325669));
#38922=DIRECTION('center_axis',(-1.,0.,0.));
#38923=DIRECTION('ref_axis',(0.,1.,0.));
#38924=DIRECTION('',(0.,0.281116060120939,0.959673778292437));
#38925=DIRECTION('center_axis',(0.,0.959673778292437,-0.281116060120939));
#38926=DIRECTION('ref_axis',(0.,0.281116060120939,0.959673778292437));
#38927=DIRECTION('',(1.,0.,0.));
#38928=DIRECTION('',(0.,0.281116060120939,0.959673778292437));
#38929=DIRECTION('center_axis',(1.,0.,0.));
#38930=DIRECTION('ref_axis',(0.,0.939692620785908,0.342020143325669));
#38931=DIRECTION('center_axis',(1.,0.,0.));
#38932=DIRECTION('ref_axis',(0.,1.,0.));
#38933=DIRECTION('center_axis',(0.,-0.690543841286576,-0.723290538622745));
#38934=DIRECTION('ref_axis',(0.,0.723290538622745,-0.690543841286576));
#38935=DIRECTION('',(-1.,0.,0.));
#38936=DIRECTION('',(0.,0.723290538622745,-0.690543841286576));
#38937=DIRECTION('',(1.,0.,0.));
#38938=DIRECTION('',(0.,0.723290538622745,-0.690543841286576));
#38939=DIRECTION('center_axis',(1.,0.,0.));
#38940=DIRECTION('ref_axis',(0.,0.984807753012208,0.17364817766693));
#38941=DIRECTION('center_axis',(-1.,0.,0.));
#38942=DIRECTION('ref_axis',(0.,1.,0.));
#38943=DIRECTION('',(0.,0.443490878258566,0.896278885672002));
#38944=DIRECTION('center_axis',(0.,0.896278885672002,-0.443490878258566));
#38945=DIRECTION('ref_axis',(0.,0.443490878258566,0.896278885672002));
#38946=DIRECTION('',(1.,0.,0.));
#38947=DIRECTION('',(0.,0.443490878258566,0.896278885672002));
#38948=DIRECTION('center_axis',(1.,0.,0.));
#38949=DIRECTION('ref_axis',(0.,0.984807753012208,0.17364817766693));
#38950=DIRECTION('center_axis',(1.,0.,0.));
#38951=DIRECTION('ref_axis',(0.,1.,0.));
#38952=DIRECTION('center_axis',(0.,-0.805651012649424,-0.592390450477519));
#38953=DIRECTION('ref_axis',(0.,0.592390450477519,-0.805651012649424));
#38954=DIRECTION('',(-1.,0.,0.));
#38955=DIRECTION('',(0.,0.592390450477519,-0.805651012649424));
#38956=DIRECTION('',(1.,0.,0.));
#38957=DIRECTION('',(0.,0.592390450477519,-0.805651012649424));
#38958=DIRECTION('center_axis',(1.,0.,0.));
#38959=DIRECTION('ref_axis',(0.,1.,-6.12323399573677E-17));
#38960=DIRECTION('center_axis',(-1.,0.,0.));
#38961=DIRECTION('ref_axis',(0.,1.,0.));
#38962=DIRECTION('',(0.,0.592390450477519,0.805651012649424));
#38963=DIRECTION('center_axis',(0.,0.805651012649424,-0.592390450477519));
#38964=DIRECTION('ref_axis',(0.,0.592390450477519,0.805651012649424));
#38965=DIRECTION('',(1.,0.,0.));
#38966=DIRECTION('',(0.,0.592390450477519,0.805651012649424));
#38967=DIRECTION('center_axis',(1.,0.,0.));
#38968=DIRECTION('ref_axis',(0.,1.,-6.12323399573677E-17));
#38969=DIRECTION('center_axis',(1.,0.,0.));
#38970=DIRECTION('ref_axis',(0.,1.,0.));
#38971=DIRECTION('center_axis',(0.,-0.896278885672002,-0.443490878258566));
#38972=DIRECTION('ref_axis',(0.,0.443490878258566,-0.896278885672002));
#38973=DIRECTION('',(-1.,0.,0.));
#38974=DIRECTION('',(0.,0.443490878258566,-0.896278885672002));
#38975=DIRECTION('',(1.,0.,0.));
#38976=DIRECTION('',(0.,0.443490878258566,-0.896278885672002));
#38977=DIRECTION('center_axis',(1.,0.,0.));
#38978=DIRECTION('ref_axis',(0.,0.984807753012208,-0.17364817766693));
#38979=DIRECTION('center_axis',(-1.,0.,0.));
#38980=DIRECTION('ref_axis',(0.,1.,0.));
#38981=DIRECTION('',(0.,0.723290538622745,0.690543841286576));
#38982=DIRECTION('center_axis',(0.,0.690543841286576,-0.723290538622745));
#38983=DIRECTION('ref_axis',(0.,0.723290538622745,0.690543841286576));
#38984=DIRECTION('',(1.,0.,0.));
#38985=DIRECTION('',(0.,0.723290538622745,0.690543841286576));
#38986=DIRECTION('center_axis',(1.,0.,0.));
#38987=DIRECTION('ref_axis',(0.,0.984807753012208,-0.17364817766693));
#38988=DIRECTION('center_axis',(1.,0.,0.));
#38989=DIRECTION('ref_axis',(0.,1.,0.));
#38990=DIRECTION('center_axis',(0.,-0.959673778292437,-0.281116060120939));
#38991=DIRECTION('ref_axis',(0.,0.281116060120939,-0.959673778292437));
#38992=DIRECTION('',(-1.,0.,0.));
#38993=DIRECTION('',(0.,0.281116060120939,-0.959673778292437));
#38994=DIRECTION('',(1.,0.,0.));
#38995=DIRECTION('',(0.,0.281116060120939,-0.959673778292437));
#38996=DIRECTION('center_axis',(1.,0.,0.));
#38997=DIRECTION('ref_axis',(0.,0.939692620785908,-0.342020143325669));
#38998=DIRECTION('center_axis',(-1.,0.,0.));
#38999=DIRECTION('ref_axis',(0.,1.,0.));
#39000=DIRECTION('',(0.,0.832213809754591,0.554454844738279));
#39001=DIRECTION('center_axis',(0.,0.55445484473828,-0.832213809754591));
#39002=DIRECTION('ref_axis',(0.,0.832213809754591,0.554454844738279));
#39003=DIRECTION('',(1.,0.,0.));
#39004=DIRECTION('',(0.,0.832213809754591,0.554454844738279));
#39005=DIRECTION('center_axis',(1.,0.,0.));
#39006=DIRECTION('ref_axis',(0.,0.939692620785908,-0.342020143325669));
#39007=DIRECTION('center_axis',(1.,0.,0.));
#39008=DIRECTION('ref_axis',(0.,1.,0.));
#39009=DIRECTION('center_axis',(0.,-0.993909468777819,-0.110199672748127));
#39010=DIRECTION('ref_axis',(0.,0.110199672748127,-0.993909468777819));
#39011=DIRECTION('',(-1.,0.,0.));
#39012=DIRECTION('',(0.,0.110199672748127,-0.993909468777819));
#39013=DIRECTION('',(1.,0.,0.));
#39014=DIRECTION('',(0.,0.110199672748127,-0.993909468777819));
#39015=DIRECTION('center_axis',(1.,0.,0.));
#39016=DIRECTION('ref_axis',(0.,0.866025403784439,-0.5));
#39017=DIRECTION('center_axis',(-1.,0.,0.));
#39018=DIRECTION('ref_axis',(0.,1.,0.));
#39019=DIRECTION('',(0.,0.915850685397551,0.401519018300299));
#39020=DIRECTION('center_axis',(0.,0.4015190183003,-0.915850685397551));
#39021=DIRECTION('ref_axis',(0.,0.915850685397551,0.401519018300299));
#39022=DIRECTION('',(1.,0.,0.));
#39023=DIRECTION('',(0.,0.915850685397551,0.401519018300299));
#39024=DIRECTION('center_axis',(1.,0.,0.));
#39025=DIRECTION('ref_axis',(0.,0.866025403784439,-0.5));
#39026=DIRECTION('center_axis',(1.,0.,0.));
#39027=DIRECTION('ref_axis',(0.,1.,0.));
#39028=DIRECTION('center_axis',(0.,-0.997945722996845,0.0640650759174115));
#39029=DIRECTION('ref_axis',(0.,-0.0640650759174115,-0.997945722996845));
#39030=DIRECTION('',(-1.,0.,0.));
#39031=DIRECTION('',(0.,-0.0640650759174115,-0.997945722996845));
#39032=DIRECTION('',(1.,0.,0.));
#39033=DIRECTION('',(0.,-0.0640650759174115,-0.997945722996845));
#39034=DIRECTION('center_axis',(1.,0.,0.));
#39035=DIRECTION('ref_axis',(0.,0.766044443118978,-0.642787609686539));
#39036=DIRECTION('center_axis',(-1.,0.,0.));
#39037=DIRECTION('ref_axis',(0.,1.,0.));
#39038=DIRECTION('',(0.,0.971659901407514,0.236383239669692));
#39039=DIRECTION('center_axis',(0.,0.236383239669692,-0.971659901407515));
#39040=DIRECTION('ref_axis',(0.,0.971659901407515,0.236383239669692));
#39041=DIRECTION('',(1.,0.,0.));
#39042=DIRECTION('',(0.,0.971659901407514,0.236383239669692));
#39043=DIRECTION('center_axis',(1.,0.,0.));
#39044=DIRECTION('ref_axis',(0.,0.766044443118978,-0.642787609686539));
#39045=DIRECTION('center_axis',(1.,0.,0.));
#39046=DIRECTION('ref_axis',(0.,1.,0.));
#39047=DIRECTION('center_axis',(0.,-0.971659901407515,0.236383239669692));
#39048=DIRECTION('ref_axis',(0.,-0.236383239669692,-0.971659901407515));
#39049=DIRECTION('',(-1.,0.,0.));
#39050=DIRECTION('',(0.,-0.236383239669692,-0.971659901407515));
#39051=DIRECTION('',(1.,0.,0.));
#39052=DIRECTION('',(0.,-0.236383239669692,-0.971659901407515));
#39053=DIRECTION('center_axis',(1.,0.,0.));
#39054=DIRECTION('ref_axis',(0.,0.642787609686539,-0.766044443118978));
#39055=DIRECTION('center_axis',(-1.,0.,0.));
#39056=DIRECTION('ref_axis',(0.,1.,0.));
#39057=DIRECTION('',(0.,0.997945722996845,0.0640650759174114));
#39058=DIRECTION('center_axis',(0.,0.0640650759174115,-0.997945722996845));
#39059=DIRECTION('ref_axis',(0.,0.997945722996845,0.0640650759174114));
#39060=DIRECTION('',(1.,0.,0.));
#39061=DIRECTION('',(0.,0.997945722996845,0.0640650759174114));
#39062=DIRECTION('center_axis',(1.,0.,0.));
#39063=DIRECTION('ref_axis',(0.,0.642787609686539,-0.766044443118978));
#39064=DIRECTION('center_axis',(1.,0.,0.));
#39065=DIRECTION('ref_axis',(0.,1.,0.));
#39066=DIRECTION('center_axis',(0.,-0.915850685397551,0.4015190183003));
#39067=DIRECTION('ref_axis',(0.,-0.4015190183003,-0.915850685397551));
#39068=DIRECTION('',(-1.,0.,0.));
#39069=DIRECTION('',(0.,-0.4015190183003,-0.915850685397551));
#39070=DIRECTION('',(1.,0.,0.));
#39071=DIRECTION('',(0.,-0.4015190183003,-0.915850685397551));
#39072=DIRECTION('center_axis',(1.,0.,0.));
#39073=DIRECTION('ref_axis',(0.,0.5,-0.866025403784439));
#39074=DIRECTION('center_axis',(-1.,0.,0.));
#39075=DIRECTION('ref_axis',(0.,1.,0.));
#39076=DIRECTION('',(0.,0.993909468777819,-0.110199672748127));
#39077=DIRECTION('center_axis',(0.,-0.110199672748127,-0.993909468777819));
#39078=DIRECTION('ref_axis',(0.,0.993909468777819,-0.110199672748127));
#39079=DIRECTION('',(1.,0.,0.));
#39080=DIRECTION('',(0.,0.993909468777819,-0.110199672748127));
#39081=DIRECTION('center_axis',(1.,0.,0.));
#39082=DIRECTION('ref_axis',(0.,0.5,-0.866025403784439));
#39083=DIRECTION('center_axis',(1.,0.,0.));
#39084=DIRECTION('ref_axis',(0.,1.,0.));
#39085=DIRECTION('center_axis',(0.,-0.832213809754591,0.55445484473828));
#39086=DIRECTION('ref_axis',(0.,-0.554454844738279,-0.832213809754591));
#39087=DIRECTION('',(-1.,0.,0.));
#39088=DIRECTION('',(0.,-0.554454844738279,-0.832213809754591));
#39089=DIRECTION('',(1.,0.,0.));
#39090=DIRECTION('',(0.,-0.554454844738279,-0.832213809754591));
#39091=DIRECTION('center_axis',(1.,0.,0.));
#39092=DIRECTION('ref_axis',(0.,0.342020143325669,-0.939692620785908));
#39093=DIRECTION('center_axis',(-1.,0.,0.));
#39094=DIRECTION('ref_axis',(0.,1.,0.));
#39095=DIRECTION('',(0.,0.959673778292437,-0.281116060120939));
#39096=DIRECTION('center_axis',(0.,-0.281116060120939,-0.959673778292437));
#39097=DIRECTION('ref_axis',(0.,0.959673778292437,-0.281116060120939));
#39098=DIRECTION('',(1.,0.,0.));
#39099=DIRECTION('',(0.,0.959673778292437,-0.281116060120939));
#39100=DIRECTION('center_axis',(1.,0.,0.));
#39101=DIRECTION('ref_axis',(0.,0.342020143325669,-0.939692620785908));
#39102=DIRECTION('center_axis',(1.,0.,0.));
#39103=DIRECTION('ref_axis',(0.,1.,0.));
#39104=DIRECTION('center_axis',(0.,-0.723290538622745,0.690543841286576));
#39105=DIRECTION('ref_axis',(0.,-0.690543841286576,-0.723290538622745));
#39106=DIRECTION('',(-1.,0.,0.));
#39107=DIRECTION('',(0.,-0.690543841286576,-0.723290538622745));
#39108=DIRECTION('',(1.,0.,0.));
#39109=DIRECTION('',(0.,-0.690543841286576,-0.723290538622745));
#39110=DIRECTION('center_axis',(1.,0.,0.));
#39111=DIRECTION('ref_axis',(0.,0.17364817766693,-0.984807753012208));
#39112=DIRECTION('center_axis',(-1.,0.,0.));
#39113=DIRECTION('ref_axis',(0.,1.,0.));
#39114=DIRECTION('',(0.,0.896278885672002,-0.443490878258566));
#39115=DIRECTION('center_axis',(0.,-0.443490878258566,-0.896278885672002));
#39116=DIRECTION('ref_axis',(0.,0.896278885672002,-0.443490878258566));
#39117=DIRECTION('',(1.,0.,0.));
#39118=DIRECTION('',(0.,0.896278885672002,-0.443490878258566));
#39119=DIRECTION('center_axis',(1.,0.,0.));
#39120=DIRECTION('ref_axis',(0.,0.17364817766693,-0.984807753012208));
#39121=DIRECTION('center_axis',(1.,0.,0.));
#39122=DIRECTION('ref_axis',(0.,1.,0.));
#39123=DIRECTION('center_axis',(0.,-0.592390450477519,0.805651012649424));
#39124=DIRECTION('ref_axis',(0.,-0.805651012649424,-0.592390450477519));
#39125=DIRECTION('',(-1.,0.,0.));
#39126=DIRECTION('',(0.,-0.805651012649424,-0.592390450477519));
#39127=DIRECTION('',(1.,0.,0.));
#39128=DIRECTION('',(0.,-0.805651012649424,-0.592390450477519));
#39129=DIRECTION('center_axis',(1.,0.,0.));
#39130=DIRECTION('ref_axis',(0.,0.,-1.));
#39131=DIRECTION('center_axis',(-1.,0.,0.));
#39132=DIRECTION('ref_axis',(0.,1.,0.));
#39133=DIRECTION('',(0.,0.805651012649424,-0.592390450477519));
#39134=DIRECTION('center_axis',(0.,-0.592390450477519,-0.805651012649424));
#39135=DIRECTION('ref_axis',(0.,0.805651012649424,-0.592390450477519));
#39136=DIRECTION('',(1.,0.,0.));
#39137=DIRECTION('',(0.,0.805651012649424,-0.592390450477519));
#39138=DIRECTION('center_axis',(1.,0.,0.));
#39139=DIRECTION('ref_axis',(0.,0.,-1.));
#39140=DIRECTION('center_axis',(1.,0.,0.));
#39141=DIRECTION('ref_axis',(0.,1.,0.));
#39142=DIRECTION('center_axis',(1.,0.,0.));
#39143=DIRECTION('ref_axis',(0.,1.,0.));
#39144=DIRECTION('',(0.520049754552021,-0.854135968561436,-1.04601487993539E-16));
#39145=DIRECTION('center_axis',(-1.,0.,0.));
#39146=DIRECTION('ref_axis',(0.,1.,0.));
#39147=DIRECTION('center_axis',(0.,0.5,0.866025403784439));
#39148=DIRECTION('ref_axis',(0.,0.866025403784439,-0.5));
#39149=DIRECTION('',(0.,0.866025403784439,-0.5));
#39150=DIRECTION('',(-1.,0.,0.));
#39151=DIRECTION('',(0.,0.866025403784439,-0.5));
#39152=DIRECTION('',(-1.,0.,0.));
#39153=DIRECTION('center_axis',(0.,-0.5,0.866025403784439));
#39154=DIRECTION('ref_axis',(0.,0.866025403784439,0.5));
#39155=DIRECTION('',(0.,0.866025403784439,0.5));
#39156=DIRECTION('',(-1.,0.,0.));
#39157=DIRECTION('',(0.,0.866025403784439,0.5));
#39158=DIRECTION('center_axis',(0.,-1.,-1.92296268638356E-16));
#39159=DIRECTION('ref_axis',(0.,-1.92296268638356E-16,1.));
#39160=DIRECTION('',(0.,-1.92296268638356E-16,1.));
#39161=DIRECTION('',(-1.,0.,0.));
#39162=DIRECTION('',(0.,-1.92296268638356E-16,1.));
#39163=DIRECTION('center_axis',(0.,-0.5,-0.866025403784439));
#39164=DIRECTION('ref_axis',(0.,-0.866025403784439,0.5));
#39165=DIRECTION('',(0.,-0.866025403784439,0.5));
#39166=DIRECTION('',(-1.,0.,0.));
#39167=DIRECTION('',(0.,-0.866025403784439,0.5));
#39168=DIRECTION('center_axis',(0.,0.5,-0.866025403784439));
#39169=DIRECTION('ref_axis',(0.,-0.866025403784439,-0.5));
#39170=DIRECTION('',(0.,-0.866025403784439,-0.5));
#39171=DIRECTION('',(-1.,0.,0.));
#39172=DIRECTION('',(0.,-0.866025403784439,-0.5));
#39173=DIRECTION('center_axis',(0.,1.,-3.84592537276713E-16));
#39174=DIRECTION('ref_axis',(0.,-3.84592537276713E-16,-1.));
#39175=DIRECTION('',(0.,-3.84592537276713E-16,-1.));
#39176=DIRECTION('',(0.,-3.84592537276713E-16,-1.));
#39177=DIRECTION('center_axis',(-1.,0.,0.));
#39178=DIRECTION('ref_axis',(0.,0.,1.));
#39179=DIRECTION('center_axis',(-1.,0.,0.));
#39180=DIRECTION('ref_axis',(0.,0.,1.));
#39181=DIRECTION('center_axis',(1.,0.,0.));
#39182=DIRECTION('ref_axis',(0.,0.,-1.));
#39183=DIRECTION('center_axis',(1.,0.,0.));
#39184=DIRECTION('ref_axis',(0.,1.,0.));
#39185=DIRECTION('',(-0.707106781186548,0.707106781186547,8.65956056235493E-17));
#39186=DIRECTION('center_axis',(1.,0.,0.));
#39187=DIRECTION('ref_axis',(0.,1.,0.));
#39188=DIRECTION('center_axis',(1.,0.,0.));
#39189=DIRECTION('ref_axis',(0.,0.,-1.));
#39190=DIRECTION('',(-1.,0.,0.));
#39191=DIRECTION('',(-1.,0.,0.));
#39192=DIRECTION('center_axis',(-1.,0.,0.));
#39193=DIRECTION('ref_axis',(0.,1.,0.));
#39194=DIRECTION('center_axis',(1.,0.,0.));
#39195=DIRECTION('ref_axis',(0.,0.,-1.));
#39196=DIRECTION('',(-0.707106781186547,-0.707106781186548,-8.65956056235494E-17));
#39197=DIRECTION('center_axis',(1.,0.,0.));
#39198=DIRECTION('ref_axis',(0.,0.,-1.));
#39199=DIRECTION('axis',(0.,0.,1.));
#39200=DIRECTION('refdir',(1.,0.,0.));
#39201=DIRECTION('center_axis',(0.707106781186548,0.707106781186548,0.));
#39202=DIRECTION('ref_axis',(0.,0.,-1.));
#39203=DIRECTION('',(0.707106781186548,-0.707106781186548,0.));
#39204=DIRECTION('',(0.,0.,1.));
#39205=DIRECTION('',(-0.707106781186548,0.707106781186548,0.));
#39206=DIRECTION('',(0.,0.,-1.));
#39207=DIRECTION('center_axis',(0.,-1.,0.));
#39208=DIRECTION('ref_axis',(0.,0.,-1.));
#39209=DIRECTION('',(1.,0.,0.));
#39210=DIRECTION('',(0.,0.,-1.));
#39211=DIRECTION('',(1.,0.,0.));
#39212=DIRECTION('center_axis',(0.,0.753297855187518,0.657679512657864));
#39213=DIRECTION('ref_axis',(1.,0.,0.));
#39214=DIRECTION('',(-1.,0.,0.));
#39215=DIRECTION('',(1.,0.,0.));
#39216=DIRECTION('center_axis',(1.,0.,0.));
#39217=DIRECTION('ref_axis',(0.,1.,0.));
#39218=DIRECTION('center_axis',(1.,0.,0.));
#39219=DIRECTION('ref_axis',(0.,0.,-1.));
#39220=DIRECTION('',(1.,0.,0.));
#39221=DIRECTION('center_axis',(1.,0.,0.));
#39222=DIRECTION('ref_axis',(0.,0.,-1.));
#39223=DIRECTION('center_axis',(-1.,0.,0.));
#39224=DIRECTION('ref_axis',(0.,1.,0.));
#39225=DIRECTION('center_axis',(1.,0.,0.));
#39226=DIRECTION('ref_axis',(0.,0.,-1.));
#39227=DIRECTION('center_axis',(0.,0.753297855187518,-0.657679512657864));
#39228=DIRECTION('ref_axis',(-1.,0.,0.));
#39229=DIRECTION('',(1.,0.,0.));
#39230=DIRECTION('',(-1.,0.,0.));
#39231=DIRECTION('center_axis',(0.,0.,1.));
#39232=DIRECTION('ref_axis',(0.,-1.,0.));
#39233=DIRECTION('',(0.,1.,0.));
#39234=DIRECTION('',(-0.70710678118655,-0.707106781186545,0.));
#39235=DIRECTION('',(0.,-1.,0.));
#39236=DIRECTION('center_axis',(-1.,0.,0.));
#39237=DIRECTION('ref_axis',(0.,1.,0.));
#39238=DIRECTION('center_axis',(1.,0.,0.));
#39239=DIRECTION('ref_axis',(0.,0.,-1.));
#39240=DIRECTION('center_axis',(1.,0.,0.));
#39241=DIRECTION('ref_axis',(0.,0.,-1.));
#39242=DIRECTION('center_axis',(0.707106781186548,4.32978028117747E-17,
0.707106781186548));
#39243=DIRECTION('ref_axis',(0.707106781186548,0.,-0.707106781186548));
#39244=DIRECTION('',(0.707106781186548,-4.32978028117747E-17,-0.707106781186548));
#39245=DIRECTION('',(0.,-1.,6.12323399573677E-17));
#39246=DIRECTION('',(-0.707106781186548,4.32978028117747E-17,0.707106781186548));
#39247=DIRECTION('',(0.,1.,-6.12323399573677E-17));
#39248=DIRECTION('center_axis',(0.,-6.12323399573677E-17,-1.));
#39249=DIRECTION('ref_axis',(0.,1.,-6.12323399573677E-17));
#39250=DIRECTION('',(1.,0.,0.));
#39251=DIRECTION('',(0.,1.,-6.12323399573677E-17));
#39252=DIRECTION('',(1.,0.,0.));
#39253=DIRECTION('center_axis',(0.,-0.657679512657863,0.753297855187519));
#39254=DIRECTION('ref_axis',(1.,0.,0.));
#39255=DIRECTION('',(-1.,0.,0.));
#39256=DIRECTION('',(1.,0.,0.));
#39257=DIRECTION('center_axis',(0.,1.,-6.12323399573677E-17));
#39258=DIRECTION('ref_axis',(0.,6.12323399573677E-17,1.));
#39259=DIRECTION('',(0.,6.12323399573677E-17,1.));
#39260=DIRECTION('',(0.707106781186547,4.32978028117747E-17,0.707106781186548));
#39261=DIRECTION('',(0.,-6.12323399573677E-17,-1.));
#39262=DIRECTION('center_axis',(0.,0.657679512657864,0.753297855187518));
#39263=DIRECTION('ref_axis',(1.,0.,0.));
#39264=DIRECTION('',(1.,0.,0.));
#39265=DIRECTION('',(-1.,0.,0.));
#39266=DIRECTION('center_axis',(1.,0.,0.));
#39267=DIRECTION('ref_axis',(0.,1.,0.));
#39268=DIRECTION('center_axis',(1.,0.,0.));
#39269=DIRECTION('ref_axis',(0.,0.,-1.));
#39270=DIRECTION('',(-1.,0.,0.));
#39271=DIRECTION('center_axis',(1.,0.,0.));
#39272=DIRECTION('ref_axis',(0.,0.,-1.));
#39273=DIRECTION('center_axis',(1.,0.,0.));
#39274=DIRECTION('ref_axis',(0.,1.,0.));
#39275=DIRECTION('center_axis',(1.,0.,0.));
#39276=DIRECTION('ref_axis',(0.,0.,-1.));
#39277=DIRECTION('center_axis',(0.707106781186548,-0.707106781186548,8.65956056235493E-17));
#39278=DIRECTION('ref_axis',(1.22464679914735E-16,0.,-1.));
#39279=DIRECTION('',(0.707106781186548,0.707106781186548,-8.65956056235493E-17));
#39280=DIRECTION('',(0.,-1.22464679914735E-16,-1.));
#39281=DIRECTION('',(-0.707106781186548,-0.707106781186548,8.65956056235493E-17));
#39282=DIRECTION('',(0.,1.22464679914735E-16,1.));
#39283=DIRECTION('center_axis',(0.,1.,-1.22464679914735E-16));
#39284=DIRECTION('ref_axis',(0.,1.22464679914735E-16,1.));
#39285=DIRECTION('',(1.,0.,0.));
#39286=DIRECTION('',(0.,1.22464679914735E-16,1.));
#39287=DIRECTION('',(1.,0.,0.));
#39288=DIRECTION('center_axis',(0.,-0.753297855187518,-0.657679512657863));
#39289=DIRECTION('ref_axis',(-1.,0.,0.));
#39290=DIRECTION('',(1.,0.,0.));
#39291=DIRECTION('center_axis',(-1.,0.,0.));
#39292=DIRECTION('ref_axis',(0.,1.,0.));
#39293=DIRECTION('center_axis',(1.,0.,0.));
#39294=DIRECTION('ref_axis',(0.,0.,-1.));
#39295=DIRECTION('center_axis',(0.,1.22464679914735E-16,1.));
#39296=DIRECTION('ref_axis',(0.,-1.,1.22464679914735E-16));
#39297=DIRECTION('',(0.,-1.,1.22464679914735E-16));
#39298=DIRECTION('',(0.70710678118655,-0.707106781186545,8.6595605623549E-17));
#39299=DIRECTION('',(0.,1.,-1.22464679914735E-16));
#39300=DIRECTION('center_axis',(0.,-0.753297855187519,0.657679512657863));
#39301=DIRECTION('ref_axis',(1.,0.,0.));
#39302=DIRECTION('',(1.,0.,0.));
#39303=DIRECTION('',(-1.,0.,0.));
#39304=DIRECTION('center_axis',(1.,0.,0.));
#39305=DIRECTION('ref_axis',(0.,1.,0.));
#39306=DIRECTION('center_axis',(1.,0.,0.));
#39307=DIRECTION('ref_axis',(0.,0.,-1.));
#39308=DIRECTION('',(-1.,0.,0.));
#39309=DIRECTION('center_axis',(1.,0.,0.));
#39310=DIRECTION('ref_axis',(0.,0.,-1.));
#39311=DIRECTION('center_axis',(1.,0.,0.));
#39312=DIRECTION('ref_axis',(0.,1.,0.));
#39313=DIRECTION('center_axis',(1.,0.,0.));
#39314=DIRECTION('ref_axis',(0.,0.,-1.));
#39315=DIRECTION('center_axis',(-0.707106781186545,0.70710678118655,0.));
#39316=DIRECTION('ref_axis',(0.,0.,1.));
#39317=DIRECTION('',(0.70710678118655,0.707106781186545,0.));
#39318=DIRECTION('',(0.,0.,1.));
#39319=DIRECTION('center_axis',(-0.707106781186548,4.32978028117746E-17,
0.707106781186547));
#39320=DIRECTION('ref_axis',(0.707106781186547,0.,0.707106781186548));
#39321=DIRECTION('',(-0.707106781186547,-4.32978028117747E-17,-0.707106781186548));
#39322=DIRECTION('',(0.,-1.,6.12323399573677E-17));
#39323=DIRECTION('center_axis',(-0.707106781186545,-0.70710678118655,8.65956056235497E-17));
#39324=DIRECTION('ref_axis',(1.22464679914736E-16,0.,1.));
#39325=DIRECTION('',(-0.70710678118655,0.707106781186545,-8.6595605623549E-17));
#39326=DIRECTION('',(0.,-1.22464679914735E-16,-1.));
#39327=DIRECTION('center_axis',(0.707106781186548,-1.29893408435324E-16,
-0.707106781186548));
#39328=DIRECTION('ref_axis',(-0.707106781186548,0.,-0.707106781186548));
#39329=DIRECTION('',(0.707106781186548,1.29893408435324E-16,0.707106781186548));
#39330=DIRECTION('',(0.,1.,-1.83697019872103E-16));
#39331=DIRECTION('',(-0.707106781186548,-1.29893408435324E-16,-0.707106781186548));
#39332=DIRECTION('',(0.,-1.,1.83697019872103E-16));
#39333=DIRECTION('center_axis',(0.,1.83697019872103E-16,1.));
#39334=DIRECTION('ref_axis',(0.,-1.,1.83697019872103E-16));
#39335=DIRECTION('',(1.,0.,0.));
#39336=DIRECTION('',(0.,-1.,1.83697019872103E-16));
#39337=DIRECTION('',(1.,0.,0.));
#39338=DIRECTION('center_axis',(-0.707106781186545,-1.29893408435325E-16,
-0.70710678118655));
#39339=DIRECTION('ref_axis',(-0.70710678118655,0.,0.707106781186545));
#39340=DIRECTION('',(-0.70710678118655,1.29893408435323E-16,0.707106781186545));
#39341=DIRECTION('',(0.70710678118655,-1.29893408435323E-16,-0.707106781186545));
#39342=DIRECTION('',(0.,1.,-1.83697019872103E-16));
#39343=DIRECTION('center_axis',(0.,-0.657679512657865,-0.753297855187517));
#39344=DIRECTION('ref_axis',(-1.,0.,0.));
#39345=DIRECTION('',(-1.,0.,0.));
#39346=DIRECTION('center_axis',(1.,0.,0.));
#39347=DIRECTION('ref_axis',(0.,1.,0.));
#39348=DIRECTION('center_axis',(1.,0.,0.));
#39349=DIRECTION('ref_axis',(0.,0.,-1.));
#39350=DIRECTION('center_axis',(0.,1.,-1.83697019872103E-16));
#39351=DIRECTION('ref_axis',(0.,1.83697019872103E-16,1.));
#39352=DIRECTION('',(0.,-1.83697019872103E-16,-1.));
#39353=DIRECTION('',(0.,1.83697019872103E-16,1.));
#39354=DIRECTION('center_axis',(0.,0.657679512657864,-0.753297855187518));
#39355=DIRECTION('ref_axis',(-1.,0.,0.));
#39356=DIRECTION('',(1.,0.,0.));
#39357=DIRECTION('center_axis',(-1.,0.,0.));
#39358=DIRECTION('ref_axis',(0.,1.,0.));
#39359=DIRECTION('center_axis',(1.,0.,0.));
#39360=DIRECTION('ref_axis',(0.,0.,-1.));
#39361=DIRECTION('center_axis',(0.,-1.,1.83697019872103E-16));
#39362=DIRECTION('ref_axis',(0.,-1.83697019872103E-16,-1.));
#39363=DIRECTION('',(0.,-1.83697019872103E-16,-1.));
#39364=DIRECTION('',(0.,1.83697019872103E-16,1.));
#39365=DIRECTION('center_axis',(-1.,0.,0.));
#39366=DIRECTION('ref_axis',(0.,0.,1.));
#39367=DIRECTION('',(0.,1.,0.));
#39368=DIRECTION('',(0.,1.,-1.22464679914735E-16));
#39369=DIRECTION('',(0.,-6.12323399573677E-17,-1.));
#39370=DIRECTION('center_axis',(1.,0.,0.));
#39371=DIRECTION('ref_axis',(0.,0.,-1.));
#39372=DIRECTION('center_axis',(1.,0.,0.));
#39373=DIRECTION('ref_axis',(0.,0.,-1.));
#39374=DIRECTION('center_axis',(0.,-1.22464679914735E-16,-1.));
#39375=DIRECTION('ref_axis',(0.,1.,-1.22464679914735E-16));
#39376=DIRECTION('',(0.,-1.,1.22464679914735E-16));
#39377=DIRECTION('center_axis',(0.,-1.,6.12323399573677E-17));
#39378=DIRECTION('ref_axis',(0.,-6.12323399573677E-17,-1.));
#39379=DIRECTION('',(0.,6.12323399573677E-17,1.));
#39380=DIRECTION('center_axis',(1.,0.,0.));
#39381=DIRECTION('ref_axis',(0.,1.,0.));
#39382=DIRECTION('center_axis',(1.,0.,0.));
#39383=DIRECTION('ref_axis',(0.,0.,-1.));
#39384=DIRECTION('center_axis',(1.,0.,0.));
#39385=DIRECTION('ref_axis',(0.,1.,0.));
#39386=DIRECTION('center_axis',(0.,0.,-1.));
#39387=DIRECTION('ref_axis',(0.,1.,0.));
#39388=DIRECTION('',(0.,-1.,0.));
#39389=DIRECTION('center_axis',(1.,0.,0.));
#39390=DIRECTION('ref_axis',(0.,1.,0.));
#39391=DIRECTION('center_axis',(1.,0.,0.));
#39392=DIRECTION('ref_axis',(0.,0.,-1.));
#39393=DIRECTION('',(-1.,0.,0.));
#39394=DIRECTION('center_axis',(1.,0.,0.));
#39395=DIRECTION('ref_axis',(0.,0.,-1.));
#39396=DIRECTION('axis',(0.,0.,1.));
#39397=DIRECTION('refdir',(1.,0.,0.));
#39398=DIRECTION('center_axis',(1.,0.,0.));
#39399=DIRECTION('ref_axis',(0.,1.,0.));
#39400=DIRECTION('',(-1.,0.,0.));
#39401=DIRECTION('center_axis',(1.,0.,0.));
#39402=DIRECTION('ref_axis',(0.,1.,0.));
#39403=DIRECTION('center_axis',(1.,0.,0.));
#39404=DIRECTION('ref_axis',(0.,1.,0.));
#39405=DIRECTION('',(-1.,0.,0.));
#39406=DIRECTION('center_axis',(1.,0.,0.));
#39407=DIRECTION('ref_axis',(0.,1.,0.));
#39408=DIRECTION('',(-1.,0.,0.));
#39409=DIRECTION('center_axis',(1.,0.,0.));
#39410=DIRECTION('ref_axis',(0.,1.,0.));
#39411=DIRECTION('',(-1.,0.,0.));
#39412=DIRECTION('center_axis',(1.,0.,0.));
#39413=DIRECTION('ref_axis',(0.,1.,0.));
#39414=DIRECTION('',(-1.,0.,0.));
#39415=DIRECTION('center_axis',(1.,0.,0.));
#39416=DIRECTION('ref_axis',(0.,1.,0.));
#39417=DIRECTION('',(-1.,0.,0.));
#39418=DIRECTION('center_axis',(1.,0.,0.));
#39419=DIRECTION('ref_axis',(0.,1.,0.));
#39420=DIRECTION('',(-1.,0.,0.));
#39421=DIRECTION('center_axis',(1.,0.,0.));
#39422=DIRECTION('ref_axis',(0.,1.,0.));
#39423=DIRECTION('',(-1.,0.,0.));
#39424=DIRECTION('center_axis',(1.,0.,0.));
#39425=DIRECTION('ref_axis',(0.,1.,0.));
#39426=DIRECTION('',(-1.,0.,0.));
#39427=DIRECTION('center_axis',(1.,0.,0.));
#39428=DIRECTION('ref_axis',(0.,1.,0.));
#39429=DIRECTION('',(-1.,0.,0.));
#39430=DIRECTION('center_axis',(1.,0.,0.));
#39431=DIRECTION('ref_axis',(0.,1.,0.));
#39432=DIRECTION('',(-1.,0.,0.));
#39433=DIRECTION('center_axis',(1.,0.,0.));
#39434=DIRECTION('ref_axis',(0.,1.,0.));
#39435=DIRECTION('',(-1.,0.,0.));
#39436=DIRECTION('center_axis',(1.,0.,0.));
#39437=DIRECTION('ref_axis',(0.,1.,0.));
#39438=DIRECTION('',(-1.,0.,0.));
#39439=DIRECTION('center_axis',(1.,0.,0.));
#39440=DIRECTION('ref_axis',(0.,1.,0.));
#39441=DIRECTION('',(-1.,0.,0.));
#39442=DIRECTION('center_axis',(1.,0.,0.));
#39443=DIRECTION('ref_axis',(0.,1.,0.));
#39444=DIRECTION('',(-1.,0.,0.));
#39445=DIRECTION('center_axis',(1.,0.,0.));
#39446=DIRECTION('ref_axis',(0.,1.,0.));
#39447=DIRECTION('',(-1.,0.,0.));
#39448=DIRECTION('center_axis',(1.,0.,0.));
#39449=DIRECTION('ref_axis',(0.,-0.991226743157339,-0.132172401240557));
#39450=DIRECTION('',(1.,0.,0.));
#39451=DIRECTION('center_axis',(1.,0.,0.));
#39452=DIRECTION('ref_axis',(0.,1.,8.34422700308396E-14));
#39453=DIRECTION('center_axis',(1.,0.,0.));
#39454=DIRECTION('ref_axis',(0.,1.,8.34422700308396E-14));
#39455=DIRECTION('',(1.,0.,0.));
#39456=DIRECTION('center_axis',(1.,0.,0.));
#39457=DIRECTION('ref_axis',(0.,1.,8.34422700308396E-14));
#39458=DIRECTION('center_axis',(1.,0.,0.));
#39459=DIRECTION('ref_axis',(0.,1.,8.34422700308396E-14));
#39460=DIRECTION('',(1.,0.,0.));
#39461=DIRECTION('center_axis',(1.,0.,0.));
#39462=DIRECTION('ref_axis',(0.,1.,8.34422700308396E-14));
#39463=DIRECTION('',(1.,0.,0.));
#39464=DIRECTION('center_axis',(1.,0.,0.));
#39465=DIRECTION('ref_axis',(0.,1.,8.34422700308396E-14));
#39466=DIRECTION('',(1.,0.,0.));
#39467=DIRECTION('center_axis',(1.,0.,0.));
#39468=DIRECTION('ref_axis',(0.,1.,8.34422700308396E-14));
#39469=DIRECTION('',(1.,0.,0.));
#39470=DIRECTION('center_axis',(1.,0.,0.));
#39471=DIRECTION('ref_axis',(0.,1.,8.34422700308396E-14));
#39472=DIRECTION('',(1.,0.,0.));
#39473=DIRECTION('center_axis',(1.,0.,0.));
#39474=DIRECTION('ref_axis',(0.,1.,8.34422700308396E-14));
#39475=DIRECTION('',(1.,0.,0.));
#39476=DIRECTION('center_axis',(1.,0.,0.));
#39477=DIRECTION('ref_axis',(0.,1.,8.34422700308396E-14));
#39478=DIRECTION('',(1.,0.,0.));
#39479=DIRECTION('center_axis',(1.,0.,0.));
#39480=DIRECTION('ref_axis',(0.,1.,8.34422700308396E-14));
#39481=DIRECTION('',(1.,0.,0.));
#39482=DIRECTION('center_axis',(1.,0.,0.));
#39483=DIRECTION('ref_axis',(0.,1.,8.34422700308396E-14));
#39484=DIRECTION('',(1.,0.,0.));
#39485=DIRECTION('center_axis',(1.,0.,0.));
#39486=DIRECTION('ref_axis',(0.,1.,8.34422700308396E-14));
#39487=DIRECTION('',(1.,0.,0.));
#39488=DIRECTION('center_axis',(1.,0.,0.));
#39489=DIRECTION('ref_axis',(0.,1.,8.34422700308396E-14));
#39490=DIRECTION('',(1.,0.,0.));
#39491=DIRECTION('center_axis',(1.,0.,0.));
#39492=DIRECTION('ref_axis',(0.,1.,8.34422700308396E-14));
#39493=DIRECTION('',(1.,0.,0.));
#39494=DIRECTION('center_axis',(1.,0.,0.));
#39495=DIRECTION('ref_axis',(0.,1.,8.34422700308396E-14));
#39496=DIRECTION('',(1.,0.,0.));
#39497=DIRECTION('center_axis',(1.,0.,0.));
#39498=DIRECTION('ref_axis',(0.,1.,8.34422700308396E-14));
#39499=DIRECTION('',(1.,0.,0.));
#39500=DIRECTION('center_axis',(-1.,0.,0.));
#39501=DIRECTION('ref_axis',(0.,-1.,0.));
#39502=DIRECTION('center_axis',(-1.,0.,0.));
#39503=DIRECTION('ref_axis',(0.,-1.,0.));
#39504=DIRECTION('',(0.707106781186547,-0.707106781186547,8.65956056235493E-17));
#39505=DIRECTION('center_axis',(1.,0.,0.));
#39506=DIRECTION('ref_axis',(0.,-1.,0.));
#39507=DIRECTION('center_axis',(1.,0.,0.));
#39508=DIRECTION('ref_axis',(0.,-1.,0.));
#39509=DIRECTION('center_axis',(1.,0.,0.));
#39510=DIRECTION('ref_axis',(0.,1.,0.));
#39511=DIRECTION('center_axis',(-1.,0.,0.));
#39512=DIRECTION('ref_axis',(0.,-1.,0.));
#39513=DIRECTION('center_axis',(-1.,0.,0.));
#39514=DIRECTION('ref_axis',(0.,-1.,0.));
#39515=DIRECTION('',(-1.,0.,0.));
#39516=DIRECTION('',(1.,0.,0.));
#39517=DIRECTION('',(-1.,0.,0.));
#39518=DIRECTION('center_axis',(-1.,0.,0.));
#39519=DIRECTION('ref_axis',(0.,0.,1.));
#39520=DIRECTION('center_axis',(1.,0.,0.));
#39521=DIRECTION('ref_axis',(0.,0.,-1.));
#39522=DIRECTION('center_axis',(1.,0.,0.));
#39523=DIRECTION('ref_axis',(0.,-1.,0.));
#39524=DIRECTION('',(0.707106781186547,0.707106781186547,-8.65956056235493E-17));
#39525=DIRECTION('center_axis',(1.,0.,0.));
#39526=DIRECTION('ref_axis',(0.,-1.,0.));
#39527=DIRECTION('center_axis',(1.,0.,0.));
#39528=DIRECTION('ref_axis',(0.,0.,-1.));
#39529=DIRECTION('center_axis',(1.,0.,0.));
#39530=DIRECTION('ref_axis',(0.,0.,-1.));
#39531=DIRECTION('',(0.,-0.651997912940355,0.758220760413101));
#39532=DIRECTION('center_axis',(0.,-1.,0.));
#39533=DIRECTION('ref_axis',(1.,0.,0.));
#39534=DIRECTION('',(0.,-1.,0.));
#39535=DIRECTION('center_axis',(0.,-1.,0.));
#39536=DIRECTION('ref_axis',(1.,0.,0.));
#39537=DIRECTION('center_axis',(0.,-1.,0.));
#39538=DIRECTION('ref_axis',(1.,0.,0.));
#39539=DIRECTION('center_axis',(1.,0.,0.));
#39540=DIRECTION('ref_axis',(0.,1.,0.));
#39541=DIRECTION('center_axis',(1.,0.,0.));
#39542=DIRECTION('ref_axis',(0.,0.,-1.));
#39543=DIRECTION('',(-1.,0.,0.));
#39544=DIRECTION('center_axis',(1.,0.,0.));
#39545=DIRECTION('ref_axis',(0.,0.,-1.));
#39546=DIRECTION('center_axis',(1.,0.,0.));
#39547=DIRECTION('ref_axis',(0.,0.,-1.));
#39548=DIRECTION('center_axis',(1.,0.,0.));
#39549=DIRECTION('ref_axis',(0.,1.,0.));
#39550=DIRECTION('center_axis',(1.,0.,0.));
#39551=DIRECTION('ref_axis',(0.,1.,0.));
#39552=DIRECTION('center_axis',(-1.,0.,0.));
#39553=DIRECTION('ref_axis',(0.,1.,8.34422700308396E-14));
#39554=DIRECTION('center_axis',(1.,0.,0.));
#39555=DIRECTION('ref_axis',(0.,0.888994820201767,0.457917251972918));
#39556=DIRECTION('center_axis',(0.,1.,0.));
#39557=DIRECTION('ref_axis',(1.,0.,0.));
#39558=DIRECTION('center_axis',(0.,1.,0.));
#39559=DIRECTION('ref_axis',(1.,0.,0.));
#39560=DIRECTION('center_axis',(1.,0.,0.));
#39561=DIRECTION('ref_axis',(0.,1.,0.));
#39562=DIRECTION('',(-0.707106781186548,0.707106781186547,8.65956056235493E-17));
#39563=DIRECTION('center_axis',(1.,0.,0.));
#39564=DIRECTION('ref_axis',(0.,0.0481637001355167,-0.998839455562933));
#39565=DIRECTION('center_axis',(1.,0.,0.));
#39566=DIRECTION('ref_axis',(0.,1.,0.));
#39567=DIRECTION('center_axis',(-1.,0.,0.));
#39568=DIRECTION('ref_axis',(0.,0.,1.));
#39569=DIRECTION('center_axis',(1.,0.,0.));
#39570=DIRECTION('ref_axis',(0.,0.,-1.));
#39571=DIRECTION('center_axis',(1.,0.,0.));
#39572=DIRECTION('ref_axis',(0.,1.,0.));
#39573=DIRECTION('',(-0.707106781186547,0.707106781186548,8.65956056235493E-17));
#39574=DIRECTION('center_axis',(-1.,0.,0.));
#39575=DIRECTION('ref_axis',(0.,1.,0.));
#39576=DIRECTION('center_axis',(1.,0.,0.));
#39577=DIRECTION('ref_axis',(0.,0.,-1.));
#39578=DIRECTION('',(-0.707106781186547,-0.707106781186548,-8.65956056235493E-17));
#39579=DIRECTION('center_axis',(1.,0.,0.));
#39580=DIRECTION('ref_axis',(0.,0.,-1.));
#39581=DIRECTION('center_axis',(1.,0.,0.));
#39582=DIRECTION('ref_axis',(0.,0.,-1.));
#39583=DIRECTION('center_axis',(1.,0.,0.));
#39584=DIRECTION('ref_axis',(0.,1.,0.));
#39585=DIRECTION('center_axis',(1.,0.,0.));
#39586=DIRECTION('ref_axis',(0.,0.,-1.));
#39587=DIRECTION('',(-1.,0.,0.));
#39588=DIRECTION('center_axis',(-1.,0.,0.));
#39589=DIRECTION('ref_axis',(0.,1.,0.));
#39590=DIRECTION('',(-0.707106781186546,-0.70710678118655,-8.65956056235496E-17));
#39591=DIRECTION('axis',(0.,0.,1.));
#39592=DIRECTION('refdir',(1.,0.,0.));
#39593=DIRECTION('center_axis',(1.,0.,0.));
#39594=DIRECTION('ref_axis',(0.,1.,0.));
#39595=DIRECTION('',(-1.,0.,0.));
#39596=DIRECTION('center_axis',(1.,0.,0.));
#39597=DIRECTION('ref_axis',(0.,1.,0.));
#39598=DIRECTION('center_axis',(1.,0.,0.));
#39599=DIRECTION('ref_axis',(0.,1.,0.));
#39600=DIRECTION('',(-1.,0.,0.));
#39601=DIRECTION('center_axis',(1.,0.,0.));
#39602=DIRECTION('ref_axis',(0.,1.,0.));
#39603=DIRECTION('',(-1.,0.,0.));
#39604=DIRECTION('center_axis',(1.,0.,0.));
#39605=DIRECTION('ref_axis',(0.,1.,0.));
#39606=DIRECTION('',(-1.,0.,0.));
#39607=DIRECTION('center_axis',(1.,0.,0.));
#39608=DIRECTION('ref_axis',(0.,1.,0.));
#39609=DIRECTION('',(-1.,0.,0.));
#39610=DIRECTION('center_axis',(1.,0.,0.));
#39611=DIRECTION('ref_axis',(0.,1.,0.));
#39612=DIRECTION('',(-1.,0.,0.));
#39613=DIRECTION('center_axis',(1.,0.,0.));
#39614=DIRECTION('ref_axis',(0.,1.,0.));
#39615=DIRECTION('',(-1.,0.,0.));
#39616=DIRECTION('center_axis',(1.,0.,0.));
#39617=DIRECTION('ref_axis',(0.,1.,0.));
#39618=DIRECTION('',(-1.,0.,0.));
#39619=DIRECTION('center_axis',(1.,0.,0.));
#39620=DIRECTION('ref_axis',(0.,1.,0.));
#39621=DIRECTION('',(-1.,0.,0.));
#39622=DIRECTION('center_axis',(1.,0.,0.));
#39623=DIRECTION('ref_axis',(0.,1.,0.));
#39624=DIRECTION('',(-1.,0.,0.));
#39625=DIRECTION('center_axis',(1.,0.,0.));
#39626=DIRECTION('ref_axis',(0.,1.,0.));
#39627=DIRECTION('',(-1.,0.,0.));
#39628=DIRECTION('center_axis',(1.,0.,0.));
#39629=DIRECTION('ref_axis',(0.,1.,0.));
#39630=DIRECTION('',(-1.,0.,0.));
#39631=DIRECTION('center_axis',(1.,0.,0.));
#39632=DIRECTION('ref_axis',(0.,1.,0.));
#39633=DIRECTION('',(-1.,0.,0.));
#39634=DIRECTION('center_axis',(1.,0.,0.));
#39635=DIRECTION('ref_axis',(0.,1.,0.));
#39636=DIRECTION('',(-1.,0.,0.));
#39637=DIRECTION('center_axis',(1.,0.,0.));
#39638=DIRECTION('ref_axis',(0.,1.,0.));
#39639=DIRECTION('',(-1.,0.,0.));
#39640=DIRECTION('center_axis',(1.,0.,0.));
#39641=DIRECTION('ref_axis',(0.,1.,0.));
#39642=DIRECTION('',(-1.,0.,0.));
#39643=DIRECTION('center_axis',(1.,0.,0.));
#39644=DIRECTION('ref_axis',(0.,1.,0.));
#39645=DIRECTION('',(-1.,0.,0.));
#39646=DIRECTION('center_axis',(1.,0.,0.));
#39647=DIRECTION('ref_axis',(0.,1.,0.));
#39648=DIRECTION('',(-1.,0.,0.));
#39649=DIRECTION('center_axis',(1.,0.,0.));
#39650=DIRECTION('ref_axis',(0.,1.,0.));
#39651=DIRECTION('',(-1.,0.,0.));
#39652=DIRECTION('center_axis',(1.,0.,0.));
#39653=DIRECTION('ref_axis',(0.,1.,0.));
#39654=DIRECTION('',(-1.,0.,0.));
#39655=DIRECTION('center_axis',(1.,0.,0.));
#39656=DIRECTION('ref_axis',(0.,1.,0.));
#39657=DIRECTION('',(-1.,0.,0.));
#39658=DIRECTION('center_axis',(1.,0.,0.));
#39659=DIRECTION('ref_axis',(0.,1.,0.));
#39660=DIRECTION('',(-1.,0.,0.));
#39661=DIRECTION('center_axis',(1.,0.,0.));
#39662=DIRECTION('ref_axis',(0.,1.,0.));
#39663=DIRECTION('',(-1.,0.,0.));
#39664=DIRECTION('center_axis',(1.,0.,0.));
#39665=DIRECTION('ref_axis',(0.,1.,0.));
#39666=DIRECTION('',(-1.,0.,0.));
#39667=DIRECTION('center_axis',(1.,0.,0.));
#39668=DIRECTION('ref_axis',(0.,1.,0.));
#39669=DIRECTION('',(-1.,0.,0.));
#39670=DIRECTION('center_axis',(1.,0.,0.));
#39671=DIRECTION('ref_axis',(0.,1.,0.));
#39672=DIRECTION('',(-1.,0.,0.));
#39673=DIRECTION('center_axis',(1.,0.,0.));
#39674=DIRECTION('ref_axis',(0.,1.,0.));
#39675=DIRECTION('',(-1.,0.,0.));
#39676=DIRECTION('center_axis',(1.,0.,0.));
#39677=DIRECTION('ref_axis',(0.,1.,0.));
#39678=DIRECTION('',(-1.,0.,0.));
#39679=DIRECTION('center_axis',(1.,0.,0.));
#39680=DIRECTION('ref_axis',(0.,1.,0.));
#39681=DIRECTION('',(-1.,0.,0.));
#39682=DIRECTION('center_axis',(1.,0.,0.));
#39683=DIRECTION('ref_axis',(0.,1.,0.));
#39684=DIRECTION('',(-1.,0.,0.));
#39685=DIRECTION('center_axis',(1.,0.,0.));
#39686=DIRECTION('ref_axis',(0.,1.,0.));
#39687=DIRECTION('',(-1.,0.,0.));
#39688=DIRECTION('center_axis',(1.,0.,0.));
#39689=DIRECTION('ref_axis',(0.,1.,0.));
#39690=DIRECTION('',(-1.,0.,0.));
#39691=DIRECTION('center_axis',(1.,0.,0.));
#39692=DIRECTION('ref_axis',(0.,1.,0.));
#39693=DIRECTION('',(-1.,0.,0.));
#39694=DIRECTION('center_axis',(1.,0.,0.));
#39695=DIRECTION('ref_axis',(0.,1.,0.));
#39696=DIRECTION('',(-1.,0.,0.));
#39697=DIRECTION('center_axis',(1.,0.,0.));
#39698=DIRECTION('ref_axis',(0.,1.,0.));
#39699=DIRECTION('',(-1.,0.,0.));
#39700=DIRECTION('center_axis',(1.,0.,0.));
#39701=DIRECTION('ref_axis',(0.,1.,0.));
#39702=DIRECTION('',(-1.,0.,0.));
#39703=DIRECTION('center_axis',(1.,0.,0.));
#39704=DIRECTION('ref_axis',(0.,1.,0.));
#39705=DIRECTION('',(-1.,0.,0.));
#39706=DIRECTION('center_axis',(1.,0.,0.));
#39707=DIRECTION('ref_axis',(0.,1.,0.));
#39708=DIRECTION('',(-1.,0.,0.));
#39709=DIRECTION('center_axis',(1.,0.,0.));
#39710=DIRECTION('ref_axis',(0.,1.,0.));
#39711=DIRECTION('',(-1.,0.,0.));
#39712=DIRECTION('center_axis',(1.,0.,0.));
#39713=DIRECTION('ref_axis',(0.,1.,0.));
#39714=DIRECTION('',(-1.,0.,0.));
#39715=DIRECTION('center_axis',(1.,0.,0.));
#39716=DIRECTION('ref_axis',(0.,1.,0.));
#39717=DIRECTION('',(-1.,0.,0.));
#39718=DIRECTION('center_axis',(1.,0.,0.));
#39719=DIRECTION('ref_axis',(0.,1.,0.));
#39720=DIRECTION('',(-1.,0.,0.));
#39721=DIRECTION('center_axis',(1.,0.,0.));
#39722=DIRECTION('ref_axis',(0.,1.,0.));
#39723=DIRECTION('',(-1.,0.,0.));
#39724=DIRECTION('center_axis',(1.,0.,0.));
#39725=DIRECTION('ref_axis',(0.,1.,0.));
#39726=DIRECTION('',(-1.,0.,0.));
#39727=DIRECTION('center_axis',(1.,0.,0.));
#39728=DIRECTION('ref_axis',(0.,1.,0.));
#39729=DIRECTION('',(-1.,0.,0.));
#39730=DIRECTION('center_axis',(1.,0.,0.));
#39731=DIRECTION('ref_axis',(0.,1.,0.));
#39732=DIRECTION('',(-1.,0.,0.));
#39733=DIRECTION('center_axis',(1.,0.,0.));
#39734=DIRECTION('ref_axis',(0.,1.,0.));
#39735=DIRECTION('',(-1.,0.,0.));
#39736=DIRECTION('center_axis',(1.,0.,0.));
#39737=DIRECTION('ref_axis',(0.,1.,0.));
#39738=DIRECTION('',(-1.,0.,0.));
#39739=DIRECTION('center_axis',(1.,0.,0.));
#39740=DIRECTION('ref_axis',(0.,1.,0.));
#39741=DIRECTION('',(-1.,0.,0.));
#39742=DIRECTION('center_axis',(1.,0.,0.));
#39743=DIRECTION('ref_axis',(0.,1.,0.));
#39744=DIRECTION('',(-1.,0.,0.));
#39745=DIRECTION('center_axis',(1.,0.,0.));
#39746=DIRECTION('ref_axis',(0.,1.,0.));
#39747=DIRECTION('',(-1.,0.,0.));
#39748=DIRECTION('center_axis',(1.,0.,0.));
#39749=DIRECTION('ref_axis',(0.,1.,0.));
#39750=DIRECTION('',(-1.,0.,0.));
#39751=DIRECTION('center_axis',(1.,0.,0.));
#39752=DIRECTION('ref_axis',(0.,1.,0.));
#39753=DIRECTION('',(-1.,0.,0.));
#39754=DIRECTION('center_axis',(1.,0.,0.));
#39755=DIRECTION('ref_axis',(0.,1.,0.));
#39756=DIRECTION('',(-1.,0.,0.));
#39757=DIRECTION('center_axis',(1.,0.,0.));
#39758=DIRECTION('ref_axis',(0.,1.,0.));
#39759=DIRECTION('',(-1.,0.,0.));
#39760=DIRECTION('center_axis',(1.,0.,0.));
#39761=DIRECTION('ref_axis',(0.,1.,0.));
#39762=DIRECTION('',(-1.,0.,0.));
#39763=DIRECTION('center_axis',(1.,0.,0.));
#39764=DIRECTION('ref_axis',(0.,1.,0.));
#39765=DIRECTION('',(-1.,0.,0.));
#39766=DIRECTION('center_axis',(1.,0.,0.));
#39767=DIRECTION('ref_axis',(0.,1.,0.));
#39768=DIRECTION('',(-1.,0.,0.));
#39769=DIRECTION('center_axis',(1.,0.,0.));
#39770=DIRECTION('ref_axis',(0.,1.,0.));
#39771=DIRECTION('',(-1.,0.,0.));
#39772=DIRECTION('center_axis',(1.,0.,0.));
#39773=DIRECTION('ref_axis',(0.,1.,0.));
#39774=DIRECTION('',(-1.,0.,0.));
#39775=DIRECTION('center_axis',(1.,0.,0.));
#39776=DIRECTION('ref_axis',(0.,1.,0.));
#39777=DIRECTION('',(-1.,0.,0.));
#39778=DIRECTION('center_axis',(1.,0.,0.));
#39779=DIRECTION('ref_axis',(0.,1.,0.));
#39780=DIRECTION('',(-1.,0.,0.));
#39781=DIRECTION('center_axis',(1.,0.,0.));
#39782=DIRECTION('ref_axis',(0.,1.,0.));
#39783=DIRECTION('',(-1.,0.,0.));
#39784=DIRECTION('center_axis',(1.,0.,0.));
#39785=DIRECTION('ref_axis',(0.,1.,0.));
#39786=DIRECTION('',(-1.,0.,0.));
#39787=DIRECTION('center_axis',(1.,0.,0.));
#39788=DIRECTION('ref_axis',(0.,1.,0.));
#39789=DIRECTION('',(-1.,0.,0.));
#39790=DIRECTION('center_axis',(1.,0.,0.));
#39791=DIRECTION('ref_axis',(0.,1.,0.));
#39792=DIRECTION('',(-1.,0.,0.));
#39793=DIRECTION('center_axis',(1.,0.,0.));
#39794=DIRECTION('ref_axis',(0.,1.,0.));
#39795=DIRECTION('',(-1.,0.,0.));
#39796=DIRECTION('center_axis',(1.,0.,0.));
#39797=DIRECTION('ref_axis',(0.,1.,0.));
#39798=DIRECTION('',(-1.,0.,0.));
#39799=DIRECTION('center_axis',(1.,0.,0.));
#39800=DIRECTION('ref_axis',(0.,1.,0.));
#39801=DIRECTION('',(-1.,0.,0.));
#39802=DIRECTION('center_axis',(1.,0.,0.));
#39803=DIRECTION('ref_axis',(0.,1.,0.));
#39804=DIRECTION('',(-1.,0.,0.));
#39805=DIRECTION('center_axis',(1.,0.,0.));
#39806=DIRECTION('ref_axis',(0.,1.,0.));
#39807=DIRECTION('',(-1.,0.,0.));
#39808=DIRECTION('center_axis',(1.,0.,0.));
#39809=DIRECTION('ref_axis',(0.,1.,0.));
#39810=DIRECTION('',(-1.,0.,0.));
#39811=DIRECTION('center_axis',(1.,0.,0.));
#39812=DIRECTION('ref_axis',(0.,1.,0.));
#39813=DIRECTION('',(-1.,0.,0.));
#39814=DIRECTION('center_axis',(1.,0.,0.));
#39815=DIRECTION('ref_axis',(0.,1.,0.));
#39816=DIRECTION('',(-1.,0.,0.));
#39817=DIRECTION('center_axis',(1.,0.,0.));
#39818=DIRECTION('ref_axis',(0.,1.,0.));
#39819=DIRECTION('',(-1.,0.,0.));
#39820=DIRECTION('center_axis',(1.,0.,0.));
#39821=DIRECTION('ref_axis',(0.,-0.740693059652024,-0.671843576573687));
#39822=DIRECTION('',(1.,0.,0.));
#39823=DIRECTION('center_axis',(1.,0.,0.));
#39824=DIRECTION('ref_axis',(0.,1.,-1.13773497930895E-12));
#39825=DIRECTION('center_axis',(1.,0.,0.));
#39826=DIRECTION('ref_axis',(0.,1.,-1.13773497930895E-12));
#39827=DIRECTION('',(1.,0.,0.));
#39828=DIRECTION('center_axis',(1.,0.,0.));
#39829=DIRECTION('ref_axis',(0.,1.,-1.13773497930895E-12));
#39830=DIRECTION('',(1.,0.,0.));
#39831=DIRECTION('center_axis',(1.,0.,0.));
#39832=DIRECTION('ref_axis',(0.,1.,-1.13773497930895E-12));
#39833=DIRECTION('',(1.,0.,0.));
#39834=DIRECTION('center_axis',(1.,0.,0.));
#39835=DIRECTION('ref_axis',(0.,1.,-1.13773497930895E-12));
#39836=DIRECTION('',(1.,0.,0.));
#39837=DIRECTION('center_axis',(1.,0.,0.));
#39838=DIRECTION('ref_axis',(0.,1.,-1.13773497930895E-12));
#39839=DIRECTION('',(1.,0.,0.));
#39840=DIRECTION('center_axis',(1.,0.,0.));
#39841=DIRECTION('ref_axis',(0.,1.,-1.13773497930895E-12));
#39842=DIRECTION('',(1.,0.,0.));
#39843=DIRECTION('center_axis',(1.,0.,0.));
#39844=DIRECTION('ref_axis',(0.,1.,-1.13773497930895E-12));
#39845=DIRECTION('',(1.,0.,0.));
#39846=DIRECTION('center_axis',(1.,0.,0.));
#39847=DIRECTION('ref_axis',(0.,1.,-1.13773497930895E-12));
#39848=DIRECTION('',(1.,0.,0.));
#39849=DIRECTION('center_axis',(1.,0.,0.));
#39850=DIRECTION('ref_axis',(0.,1.,-1.13773497930895E-12));
#39851=DIRECTION('',(1.,0.,0.));
#39852=DIRECTION('center_axis',(1.,0.,0.));
#39853=DIRECTION('ref_axis',(0.,1.,-1.13773497930895E-12));
#39854=DIRECTION('',(1.,0.,0.));
#39855=DIRECTION('center_axis',(1.,0.,0.));
#39856=DIRECTION('ref_axis',(0.,1.,-1.13773497930895E-12));
#39857=DIRECTION('',(1.,0.,0.));
#39858=DIRECTION('center_axis',(1.,0.,0.));
#39859=DIRECTION('ref_axis',(0.,1.,-1.13773497930895E-12));
#39860=DIRECTION('',(1.,0.,0.));
#39861=DIRECTION('center_axis',(1.,0.,0.));
#39862=DIRECTION('ref_axis',(0.,1.,-1.13773497930895E-12));
#39863=DIRECTION('',(1.,0.,0.));
#39864=DIRECTION('center_axis',(1.,0.,0.));
#39865=DIRECTION('ref_axis',(0.,1.,-1.13773497930895E-12));
#39866=DIRECTION('',(1.,0.,0.));
#39867=DIRECTION('center_axis',(1.,0.,0.));
#39868=DIRECTION('ref_axis',(0.,1.,-1.13773497930895E-12));
#39869=DIRECTION('',(1.,0.,0.));
#39870=DIRECTION('center_axis',(1.,0.,0.));
#39871=DIRECTION('ref_axis',(0.,1.,-1.13773497930895E-12));
#39872=DIRECTION('',(1.,0.,0.));
#39873=DIRECTION('center_axis',(1.,0.,0.));
#39874=DIRECTION('ref_axis',(0.,1.,-1.13773497930895E-12));
#39875=DIRECTION('',(1.,0.,0.));
#39876=DIRECTION('center_axis',(1.,0.,0.));
#39877=DIRECTION('ref_axis',(0.,1.,-1.13773497930895E-12));
#39878=DIRECTION('',(1.,0.,0.));
#39879=DIRECTION('center_axis',(1.,0.,0.));
#39880=DIRECTION('ref_axis',(0.,1.,-1.13773497930895E-12));
#39881=DIRECTION('',(1.,0.,0.));
#39882=DIRECTION('center_axis',(1.,0.,0.));
#39883=DIRECTION('ref_axis',(0.,1.,-1.13773497930895E-12));
#39884=DIRECTION('',(1.,0.,0.));
#39885=DIRECTION('center_axis',(1.,0.,0.));
#39886=DIRECTION('ref_axis',(0.,1.,-1.13773497930895E-12));
#39887=DIRECTION('',(1.,0.,0.));
#39888=DIRECTION('center_axis',(1.,0.,0.));
#39889=DIRECTION('ref_axis',(0.,1.,-1.13773497930895E-12));
#39890=DIRECTION('',(1.,0.,0.));
#39891=DIRECTION('center_axis',(1.,0.,0.));
#39892=DIRECTION('ref_axis',(0.,1.,-1.13773497930895E-12));
#39893=DIRECTION('',(1.,0.,0.));
#39894=DIRECTION('center_axis',(1.,0.,0.));
#39895=DIRECTION('ref_axis',(0.,1.,-1.13773497930895E-12));
#39896=DIRECTION('',(1.,0.,0.));
#39897=DIRECTION('center_axis',(1.,0.,0.));
#39898=DIRECTION('ref_axis',(0.,1.,-1.13773497930895E-12));
#39899=DIRECTION('',(1.,0.,0.));
#39900=DIRECTION('center_axis',(1.,0.,0.));
#39901=DIRECTION('ref_axis',(0.,1.,-1.13773497930895E-12));
#39902=DIRECTION('',(1.,0.,0.));
#39903=DIRECTION('center_axis',(1.,0.,0.));
#39904=DIRECTION('ref_axis',(0.,1.,-1.13773497930895E-12));
#39905=DIRECTION('',(1.,0.,0.));
#39906=DIRECTION('center_axis',(1.,0.,0.));
#39907=DIRECTION('ref_axis',(0.,1.,-1.13773497930895E-12));
#39908=DIRECTION('',(1.,0.,0.));
#39909=DIRECTION('center_axis',(1.,0.,0.));
#39910=DIRECTION('ref_axis',(0.,1.,-1.13773497930895E-12));
#39911=DIRECTION('',(1.,0.,0.));
#39912=DIRECTION('center_axis',(1.,0.,0.));
#39913=DIRECTION('ref_axis',(0.,1.,-1.13773497930895E-12));
#39914=DIRECTION('',(1.,0.,0.));
#39915=DIRECTION('center_axis',(1.,0.,0.));
#39916=DIRECTION('ref_axis',(0.,1.,-1.13773497930895E-12));
#39917=DIRECTION('',(1.,0.,0.));
#39918=DIRECTION('center_axis',(1.,0.,0.));
#39919=DIRECTION('ref_axis',(0.,1.,-1.13773497930895E-12));
#39920=DIRECTION('',(1.,0.,0.));
#39921=DIRECTION('center_axis',(1.,0.,0.));
#39922=DIRECTION('ref_axis',(0.,1.,-1.13773497930895E-12));
#39923=DIRECTION('',(1.,0.,0.));
#39924=DIRECTION('center_axis',(1.,0.,0.));
#39925=DIRECTION('ref_axis',(0.,1.,-1.13773497930895E-12));
#39926=DIRECTION('',(1.,0.,0.));
#39927=DIRECTION('center_axis',(1.,0.,0.));
#39928=DIRECTION('ref_axis',(0.,1.,-1.13773497930895E-12));
#39929=DIRECTION('',(1.,0.,0.));
#39930=DIRECTION('center_axis',(1.,0.,0.));
#39931=DIRECTION('ref_axis',(0.,1.,-1.13773497930895E-12));
#39932=DIRECTION('',(1.,0.,0.));
#39933=DIRECTION('center_axis',(1.,0.,0.));
#39934=DIRECTION('ref_axis',(0.,1.,-1.13773497930895E-12));
#39935=DIRECTION('',(1.,0.,0.));
#39936=DIRECTION('center_axis',(1.,0.,0.));
#39937=DIRECTION('ref_axis',(0.,1.,-1.13773497930895E-12));
#39938=DIRECTION('',(1.,0.,0.));
#39939=DIRECTION('center_axis',(1.,0.,0.));
#39940=DIRECTION('ref_axis',(0.,1.,-1.13773497930895E-12));
#39941=DIRECTION('',(1.,0.,0.));
#39942=DIRECTION('center_axis',(1.,0.,0.));
#39943=DIRECTION('ref_axis',(0.,1.,-1.13773497930895E-12));
#39944=DIRECTION('',(1.,0.,0.));
#39945=DIRECTION('center_axis',(1.,0.,0.));
#39946=DIRECTION('ref_axis',(0.,1.,-1.13773497930895E-12));
#39947=DIRECTION('',(1.,0.,0.));
#39948=DIRECTION('center_axis',(1.,0.,0.));
#39949=DIRECTION('ref_axis',(0.,1.,-1.13773497930895E-12));
#39950=DIRECTION('',(1.,0.,0.));
#39951=DIRECTION('center_axis',(1.,0.,0.));
#39952=DIRECTION('ref_axis',(0.,1.,-1.13773497930895E-12));
#39953=DIRECTION('',(1.,0.,0.));
#39954=DIRECTION('center_axis',(1.,0.,0.));
#39955=DIRECTION('ref_axis',(0.,1.,-1.13773497930895E-12));
#39956=DIRECTION('',(1.,0.,0.));
#39957=DIRECTION('center_axis',(1.,0.,0.));
#39958=DIRECTION('ref_axis',(0.,1.,-1.13773497930895E-12));
#39959=DIRECTION('',(1.,0.,0.));
#39960=DIRECTION('center_axis',(1.,0.,0.));
#39961=DIRECTION('ref_axis',(0.,1.,-1.13773497930895E-12));
#39962=DIRECTION('',(1.,0.,0.));
#39963=DIRECTION('center_axis',(1.,0.,0.));
#39964=DIRECTION('ref_axis',(0.,1.,-1.13773497930895E-12));
#39965=DIRECTION('',(1.,0.,0.));
#39966=DIRECTION('center_axis',(1.,0.,0.));
#39967=DIRECTION('ref_axis',(0.,1.,-1.13773497930895E-12));
#39968=DIRECTION('',(1.,0.,0.));
#39969=DIRECTION('center_axis',(1.,0.,0.));
#39970=DIRECTION('ref_axis',(0.,1.,-1.13773497930895E-12));
#39971=DIRECTION('',(1.,0.,0.));
#39972=DIRECTION('center_axis',(1.,0.,0.));
#39973=DIRECTION('ref_axis',(0.,1.,-1.13773497930895E-12));
#39974=DIRECTION('',(1.,0.,0.));
#39975=DIRECTION('center_axis',(1.,0.,0.));
#39976=DIRECTION('ref_axis',(0.,1.,-1.13773497930895E-12));
#39977=DIRECTION('',(1.,0.,0.));
#39978=DIRECTION('center_axis',(1.,0.,0.));
#39979=DIRECTION('ref_axis',(0.,1.,-1.13773497930895E-12));
#39980=DIRECTION('',(1.,0.,0.));
#39981=DIRECTION('center_axis',(1.,0.,0.));
#39982=DIRECTION('ref_axis',(0.,1.,-1.13773497930895E-12));
#39983=DIRECTION('',(1.,0.,0.));
#39984=DIRECTION('center_axis',(1.,0.,0.));
#39985=DIRECTION('ref_axis',(0.,1.,-1.13773497930895E-12));
#39986=DIRECTION('',(1.,0.,0.));
#39987=DIRECTION('center_axis',(1.,0.,0.));
#39988=DIRECTION('ref_axis',(0.,1.,-1.13773497930895E-12));
#39989=DIRECTION('',(1.,0.,0.));
#39990=DIRECTION('center_axis',(1.,0.,0.));
#39991=DIRECTION('ref_axis',(0.,1.,-1.13773497930895E-12));
#39992=DIRECTION('',(1.,0.,0.));
#39993=DIRECTION('center_axis',(1.,0.,0.));
#39994=DIRECTION('ref_axis',(0.,1.,-1.13773497930895E-12));
#39995=DIRECTION('',(1.,0.,0.));
#39996=DIRECTION('center_axis',(1.,0.,0.));
#39997=DIRECTION('ref_axis',(0.,1.,-1.13773497930895E-12));
#39998=DIRECTION('',(1.,0.,0.));
#39999=DIRECTION('center_axis',(1.,0.,0.));
#40000=DIRECTION('ref_axis',(0.,1.,-1.13773497930895E-12));
#40001=DIRECTION('',(1.,0.,0.));
#40002=DIRECTION('center_axis',(1.,0.,0.));
#40003=DIRECTION('ref_axis',(0.,1.,-1.13773497930895E-12));
#40004=DIRECTION('',(1.,0.,0.));
#40005=DIRECTION('center_axis',(1.,0.,0.));
#40006=DIRECTION('ref_axis',(0.,1.,-1.13773497930895E-12));
#40007=DIRECTION('',(1.,0.,0.));
#40008=DIRECTION('center_axis',(1.,0.,0.));
#40009=DIRECTION('ref_axis',(0.,1.,-1.13773497930895E-12));
#40010=DIRECTION('',(1.,0.,0.));
#40011=DIRECTION('center_axis',(1.,0.,0.));
#40012=DIRECTION('ref_axis',(0.,1.,-1.13773497930895E-12));
#40013=DIRECTION('',(1.,0.,0.));
#40014=DIRECTION('center_axis',(1.,0.,0.));
#40015=DIRECTION('ref_axis',(0.,1.,-1.13773497930895E-12));
#40016=DIRECTION('',(1.,0.,0.));
#40017=DIRECTION('center_axis',(1.,0.,0.));
#40018=DIRECTION('ref_axis',(0.,1.,-1.13773497930895E-12));
#40019=DIRECTION('',(1.,0.,0.));
#40020=DIRECTION('center_axis',(1.,0.,0.));
#40021=DIRECTION('ref_axis',(0.,1.,-1.13773497930895E-12));
#40022=DIRECTION('',(1.,0.,0.));
#40023=DIRECTION('center_axis',(1.,0.,0.));
#40024=DIRECTION('ref_axis',(0.,1.,-1.13773497930895E-12));
#40025=DIRECTION('',(1.,0.,0.));
#40026=DIRECTION('center_axis',(1.,0.,0.));
#40027=DIRECTION('ref_axis',(0.,1.,-1.13773497930895E-12));
#40028=DIRECTION('',(1.,0.,0.));
#40029=DIRECTION('center_axis',(1.,0.,0.));
#40030=DIRECTION('ref_axis',(0.,1.,-1.13773497930895E-12));
#40031=DIRECTION('',(1.,0.,0.));
#40032=DIRECTION('center_axis',(1.,0.,0.));
#40033=DIRECTION('ref_axis',(0.,1.,-1.13773497930895E-12));
#40034=DIRECTION('',(1.,0.,0.));
#40035=DIRECTION('center_axis',(1.,0.,0.));
#40036=DIRECTION('ref_axis',(0.,1.,-1.13773497930895E-12));
#40037=DIRECTION('',(1.,0.,0.));
#40038=DIRECTION('center_axis',(1.,0.,0.));
#40039=DIRECTION('ref_axis',(0.,1.,-1.13773497930895E-12));
#40040=DIRECTION('',(1.,0.,0.));
#40041=DIRECTION('center_axis',(1.,0.,0.));
#40042=DIRECTION('ref_axis',(0.,1.,-1.13773497930895E-12));
#40043=DIRECTION('',(1.,0.,0.));
#40044=DIRECTION('center_axis',(1.,0.,0.));
#40045=DIRECTION('ref_axis',(0.,1.,-1.13773497930895E-12));
#40046=DIRECTION('',(1.,0.,0.));
#40047=DIRECTION('center_axis',(1.,0.,0.));
#40048=DIRECTION('ref_axis',(0.,0.,-1.));
#40049=DIRECTION('center_axis',(-1.,0.,0.));
#40050=DIRECTION('ref_axis',(0.,1.,0.));
#40051=DIRECTION('center_axis',(-1.,0.,0.));
#40052=DIRECTION('ref_axis',(0.,1.,0.));
#40053=DIRECTION('center_axis',(1.,0.,0.));
#40054=DIRECTION('ref_axis',(0.,0.,-1.));
#40055=DIRECTION('center_axis',(1.,0.,0.));
#40056=DIRECTION('ref_axis',(0.,1.,0.));
#40057=DIRECTION('center_axis',(1.,0.,0.));
#40058=DIRECTION('ref_axis',(0.,1.,0.));
#40059=DIRECTION('center_axis',(-1.,0.,0.));
#40060=DIRECTION('ref_axis',(0.,1.,-1.13773497930895E-12));
#40061=DIRECTION('center_axis',(1.,0.,0.));
#40062=DIRECTION('ref_axis',(0.,1.,-1.13773497930895E-12));
#40063=DIRECTION('center_axis',(1.,0.,0.));
#40064=DIRECTION('ref_axis',(0.,1.,0.));
#40065=DIRECTION('center_axis',(1.,0.,0.));
#40066=DIRECTION('ref_axis',(0.,0.,-1.));
#40067=DIRECTION('',(-1.,0.,0.));
#40068=DIRECTION('center_axis',(1.,0.,0.));
#40069=DIRECTION('ref_axis',(0.,0.,-1.));
#40070=DIRECTION('center_axis',(1.,0.,0.));
#40071=DIRECTION('ref_axis',(0.,1.,0.));
#40072=DIRECTION('',(-0.371390676354103,0.92847669088526,1.13705600757556E-16));
#40073=DIRECTION('center_axis',(1.,0.,0.));
#40074=DIRECTION('ref_axis',(0.,0.603448580913459,-0.797401912584571));
#40075=DIRECTION('center_axis',(-1.,0.,0.));
#40076=DIRECTION('ref_axis',(0.,1.,0.));
#40077=DIRECTION('center_axis',(-1.,0.,0.));
#40078=DIRECTION('ref_axis',(0.,1.,0.));
#40079=DIRECTION('center_axis',(1.,0.,0.));
#40080=DIRECTION('ref_axis',(0.,0.,-1.));
#40081=DIRECTION('',(-0.707106781186546,-0.707106781186549,-8.65956056235495E-17));
#40082=DIRECTION('center_axis',(1.,0.,0.));
#40083=DIRECTION('ref_axis',(0.,0.,-1.));
#40084=DIRECTION('center_axis',(0.,0.,1.));
#40085=DIRECTION('ref_axis',(1.,0.,0.));
#40086=DIRECTION('center_axis',(1.22464679914735E-16,-1.,0.));
#40087=DIRECTION('ref_axis',(-1.,-1.22464679914735E-16,0.));
#40088=DIRECTION('axis',(0.,0.,1.));
#40089=DIRECTION('refdir',(1.,0.,0.));
#40090=DIRECTION('center_axis',(-1.,0.,0.));
#40091=DIRECTION('ref_axis',(0.,-1.,0.));
#40092=DIRECTION('center_axis',(-1.,0.,0.));
#40093=DIRECTION('ref_axis',(0.,-1.,0.));
#40094=DIRECTION('',(0.707106781186546,-0.707106781186549,8.65956056235495E-17));
#40095=DIRECTION('center_axis',(1.,0.,0.));
#40096=DIRECTION('ref_axis',(0.,-1.,0.));
#40097=DIRECTION('center_axis',(1.,0.,0.));
#40098=DIRECTION('ref_axis',(0.,-1.,0.));
#40099=DIRECTION('center_axis',(1.,0.,0.));
#40100=DIRECTION('ref_axis',(0.,1.,0.));
#40101=DIRECTION('center_axis',(1.,0.,0.));
#40102=DIRECTION('ref_axis',(0.,0.,-1.));
#40103=DIRECTION('',(-1.,0.,0.));
#40104=DIRECTION('center_axis',(-1.,0.,0.));
#40105=DIRECTION('ref_axis',(0.,0.,1.));
#40106=DIRECTION('center_axis',(1.,0.,0.));
#40107=DIRECTION('ref_axis',(0.,0.,-1.));
#40108=DIRECTION('center_axis',(0.,0.92942454284145,0.369012220887006));
#40109=DIRECTION('ref_axis',(0.,-0.369012220887006,0.929424542841451));
#40110=DIRECTION('',(-1.,0.,0.));
#40111=DIRECTION('',(0.,0.369012220887006,-0.929424542841451));
#40112=DIRECTION('',(1.,0.,0.));
#40113=DIRECTION('center_axis',(1.,0.,0.));
#40114=DIRECTION('ref_axis',(0.,0.,-1.));
#40115=DIRECTION('center_axis',(1.,0.,0.));
#40116=DIRECTION('ref_axis',(0.,0.,-1.));
#40117=DIRECTION('',(-1.,0.,0.));
#40118=DIRECTION('center_axis',(-1.,0.,0.));
#40119=DIRECTION('ref_axis',(0.,0.,-1.));
#40120=DIRECTION('center_axis',(0.,0.92942454284145,-0.369012220887006));
#40121=DIRECTION('ref_axis',(0.,0.369012220887006,0.929424542841451));
#40122=DIRECTION('',(0.,-0.369012220887006,-0.929424542841451));
#40123=DIRECTION('',(1.,0.,0.));
#40124=DIRECTION('center_axis',(-1.,0.,0.));
#40125=DIRECTION('ref_axis',(0.,1.,0.));
#40126=DIRECTION('center_axis',(1.,0.,0.));
#40127=DIRECTION('ref_axis',(0.,0.,-1.));
#40128=DIRECTION('center_axis',(1.,0.,0.));
#40129=DIRECTION('ref_axis',(0.,0.,-1.));
#40130=DIRECTION('center_axis',(1.,0.,0.));
#40131=DIRECTION('ref_axis',(0.,1.,0.));
#40132=DIRECTION('center_axis',(1.,0.,0.));
#40133=DIRECTION('ref_axis',(0.,0.,-1.));
#40134=DIRECTION('',(1.,0.,0.));
#40135=DIRECTION('center_axis',(-1.,0.,0.));
#40136=DIRECTION('ref_axis',(0.,1.,0.));
#40137=DIRECTION('',(-1.,0.,0.));
#40138=DIRECTION('center_axis',(1.,0.,0.));
#40139=DIRECTION('ref_axis',(0.,0.,-1.));
#40140=DIRECTION('',(1.,0.,0.));
#40141=DIRECTION('center_axis',(-1.,0.,0.));
#40142=DIRECTION('ref_axis',(0.,1.,0.));
#40143=DIRECTION('',(-1.,0.,0.));
#40144=DIRECTION('center_axis',(1.,0.,0.));
#40145=DIRECTION('ref_axis',(0.,0.,-1.));
#40146=DIRECTION('',(1.,0.,0.));
#40147=DIRECTION('center_axis',(-1.,0.,0.));
#40148=DIRECTION('ref_axis',(0.,1.,0.));
#40149=DIRECTION('',(-1.,0.,0.));
#40150=DIRECTION('center_axis',(1.,0.,0.));
#40151=DIRECTION('ref_axis',(0.,0.,-1.));
#40152=DIRECTION('',(1.,0.,0.));
#40153=DIRECTION('center_axis',(-1.,0.,0.));
#40154=DIRECTION('ref_axis',(0.,1.,0.));
#40155=DIRECTION('',(-1.,0.,0.));
#40156=DIRECTION('center_axis',(1.,0.,0.));
#40157=DIRECTION('ref_axis',(0.,0.,-1.));
#40158=DIRECTION('',(1.,0.,0.));
#40159=DIRECTION('center_axis',(-1.,0.,0.));
#40160=DIRECTION('ref_axis',(0.,1.,0.));
#40161=DIRECTION('',(-1.,0.,0.));
#40162=DIRECTION('center_axis',(1.,0.,0.));
#40163=DIRECTION('ref_axis',(0.,0.,-1.));
#40164=DIRECTION('',(1.,0.,0.));
#40165=DIRECTION('center_axis',(-1.,0.,0.));
#40166=DIRECTION('ref_axis',(0.,1.,0.));
#40167=DIRECTION('',(-1.,0.,0.));
#40168=DIRECTION('center_axis',(1.,0.,0.));
#40169=DIRECTION('ref_axis',(0.,0.,-1.));
#40170=DIRECTION('',(1.,0.,0.));
#40171=DIRECTION('center_axis',(-1.,0.,0.));
#40172=DIRECTION('ref_axis',(0.,1.,0.));
#40173=DIRECTION('',(-1.,0.,0.));
#40174=DIRECTION('center_axis',(1.,0.,0.));
#40175=DIRECTION('ref_axis',(0.,0.,-1.));
#40176=DIRECTION('',(-1.,0.,0.));
#40177=DIRECTION('center_axis',(1.,0.,0.));
#40178=DIRECTION('ref_axis',(0.,0.,-1.));
#40179=DIRECTION('center_axis',(1.,0.,0.));
#40180=DIRECTION('ref_axis',(0.,0.,-1.));
#40181=DIRECTION('',(1.,0.,0.));
#40182=DIRECTION('center_axis',(-1.,0.,0.));
#40183=DIRECTION('ref_axis',(0.,1.,0.));
#40184=DIRECTION('',(-1.,0.,0.));
#40185=DIRECTION('center_axis',(1.,0.,0.));
#40186=DIRECTION('ref_axis',(0.,0.,-1.));
#40187=DIRECTION('',(1.,0.,0.));
#40188=DIRECTION('center_axis',(-1.,0.,0.));
#40189=DIRECTION('ref_axis',(0.,1.,0.));
#40190=DIRECTION('',(-1.,0.,0.));
#40191=DIRECTION('center_axis',(1.,0.,0.));
#40192=DIRECTION('ref_axis',(0.,0.,-1.));
#40193=DIRECTION('',(1.,0.,0.));
#40194=DIRECTION('center_axis',(-1.,0.,0.));
#40195=DIRECTION('ref_axis',(0.,1.,0.));
#40196=DIRECTION('',(-1.,0.,0.));
#40197=DIRECTION('center_axis',(1.,0.,0.));
#40198=DIRECTION('ref_axis',(0.,0.,-1.));
#40199=DIRECTION('',(1.,0.,0.));
#40200=DIRECTION('center_axis',(-1.,0.,0.));
#40201=DIRECTION('ref_axis',(0.,1.,0.));
#40202=DIRECTION('',(-1.,0.,0.));
#40203=DIRECTION('center_axis',(1.,0.,0.));
#40204=DIRECTION('ref_axis',(0.,0.,-1.));
#40205=DIRECTION('',(1.,0.,0.));
#40206=DIRECTION('center_axis',(-1.,0.,0.));
#40207=DIRECTION('ref_axis',(0.,1.,0.));
#40208=DIRECTION('',(-1.,0.,0.));
#40209=DIRECTION('center_axis',(1.,0.,0.));
#40210=DIRECTION('ref_axis',(0.,0.,-1.));
#40211=DIRECTION('',(1.,0.,0.));
#40212=DIRECTION('center_axis',(-1.,0.,0.));
#40213=DIRECTION('ref_axis',(0.,1.,0.));
#40214=DIRECTION('',(-1.,0.,0.));
#40215=DIRECTION('center_axis',(1.,0.,0.));
#40216=DIRECTION('ref_axis',(0.,0.,-1.));
#40217=DIRECTION('',(1.,0.,0.));
#40218=DIRECTION('center_axis',(-1.,0.,0.));
#40219=DIRECTION('ref_axis',(0.,1.,0.));
#40220=DIRECTION('',(-1.,0.,0.));
#40221=DIRECTION('center_axis',(-1.,0.,0.));
#40222=DIRECTION('ref_axis',(0.,1.,0.));
#40223=DIRECTION('center_axis',(0.,0.698980777356835,0.715140456753522));
#40224=DIRECTION('ref_axis',(1.,0.,0.));
#40225=DIRECTION('',(0.,0.715140456753521,-0.698980777356835));
#40226=DIRECTION('',(1.,0.,0.));
#40227=DIRECTION('center_axis',(1.,0.,0.));
#40228=DIRECTION('ref_axis',(0.,0.4067366430758,-0.913545457642601));
#40229=DIRECTION('center_axis',(1.,0.,0.));
#40230=DIRECTION('ref_axis',(0.,0.4067366430758,-0.913545457642601));
#40231=DIRECTION('',(-1.,0.,0.));
#40232=DIRECTION('center_axis',(-1.,0.,0.));
#40233=DIRECTION('ref_axis',(0.,0.4067366430758,-0.913545457642601));
#40234=DIRECTION('center_axis',(0.,0.999162361311885,0.0409215803416579));
#40235=DIRECTION('ref_axis',(0.,-0.0409215803416579,0.999162361311885));
#40236=DIRECTION('',(0.,0.0409215803416579,-0.999162361311885));
#40237=DIRECTION('center_axis',(-1.,0.,0.));
#40238=DIRECTION('ref_axis',(0.,1.,0.));
#40239=DIRECTION('center_axis',(1.,0.,0.));
#40240=DIRECTION('ref_axis',(0.,0.,-1.));
#40241=DIRECTION('center_axis',(0.,0.347676885426204,0.937614410800268));
#40242=DIRECTION('ref_axis',(1.,0.,0.));
#40243=DIRECTION('',(0.,0.937614410800268,-0.347676885426204));
#40244=DIRECTION('',(1.,0.,0.));
#40245=DIRECTION('center_axis',(1.,0.,0.));
#40246=DIRECTION('ref_axis',(0.,0.743144825477394,-0.669130606358858));
#40247=DIRECTION('center_axis',(1.,0.,0.));
#40248=DIRECTION('ref_axis',(0.,0.743144825477394,-0.669130606358858));
#40249=DIRECTION('',(-1.,0.,0.));
#40250=DIRECTION('center_axis',(-1.,0.,0.));
#40251=DIRECTION('ref_axis',(0.,0.743144825477394,-0.669130606358858));
#40252=DIRECTION('center_axis',(0.,0.896135930406404,0.443779668568366));
#40253=DIRECTION('ref_axis',(0.,-0.443779668568366,0.896135930406404));
#40254=DIRECTION('',(0.,0.443779668568366,-0.896135930406404));
#40255=DIRECTION('center_axis',(-1.,0.,0.));
#40256=DIRECTION('ref_axis',(0.,1.,0.));
#40257=DIRECTION('center_axis',(1.,0.,0.));
#40258=DIRECTION('ref_axis',(0.,0.,-1.));
#40259=DIRECTION('center_axis',(0.,-0.0637434985399573,0.997966315260133));
#40260=DIRECTION('ref_axis',(1.,0.,0.));
#40261=DIRECTION('',(0.,0.997966315260133,0.0637434985399573));
#40262=DIRECTION('',(1.,0.,0.));
#40263=DIRECTION('center_axis',(1.,0.,0.));
#40264=DIRECTION('ref_axis',(0.,0.951056516295154,-0.309016994374947));
#40265=DIRECTION('center_axis',(1.,0.,0.));
#40266=DIRECTION('ref_axis',(0.,0.951056516295154,-0.309016994374947));
#40267=DIRECTION('',(-1.,0.,0.));
#40268=DIRECTION('center_axis',(-1.,0.,0.));
#40269=DIRECTION('ref_axis',(0.,0.951056516295154,-0.309016994374947));
#40270=DIRECTION('center_axis',(0.,0.63815945599431,0.769904220487877));
#40271=DIRECTION('ref_axis',(1.,0.,0.));
#40272=DIRECTION('',(0.,0.769904220487877,-0.63815945599431));
#40273=DIRECTION('center_axis',(-1.,0.,0.));
#40274=DIRECTION('ref_axis',(0.,1.,0.));
#40275=DIRECTION('center_axis',(1.,0.,0.));
#40276=DIRECTION('ref_axis',(0.,0.,-1.));
#40277=DIRECTION('center_axis',(0.,-0.46414205251706,0.885760777572168));
#40278=DIRECTION('ref_axis',(1.,0.,0.));
#40279=DIRECTION('',(0.,0.885760777572168,0.46414205251706));
#40280=DIRECTION('',(1.,0.,0.));
#40281=DIRECTION('center_axis',(1.,0.,0.));
#40282=DIRECTION('ref_axis',(0.,0.994521895368273,0.104528463267653));
#40283=DIRECTION('center_axis',(1.,0.,0.));
#40284=DIRECTION('ref_axis',(0.,0.994521895368273,0.104528463267653));
#40285=DIRECTION('',(-1.,0.,0.));
#40286=DIRECTION('center_axis',(-1.,0.,0.));
#40287=DIRECTION('ref_axis',(0.,0.994521895368273,0.104528463267653));
#40288=DIRECTION('center_axis',(0.,0.269839414144142,0.962905338324773));
#40289=DIRECTION('ref_axis',(1.,0.,0.));
#40290=DIRECTION('',(0.,0.962905338324773,-0.269839414144142));
#40291=DIRECTION('center_axis',(-1.,0.,0.));
#40292=DIRECTION('ref_axis',(0.,1.,0.));
#40293=DIRECTION('center_axis',(1.,0.,0.));
#40294=DIRECTION('ref_axis',(0.,0.,-1.));
#40295=DIRECTION('center_axis',(0.,-0.784286229015789,0.620399154557929));
#40296=DIRECTION('ref_axis',(1.,0.,0.));
#40297=DIRECTION('',(0.,0.620399154557929,0.784286229015789));
#40298=DIRECTION('',(1.,0.,0.));
#40299=DIRECTION('center_axis',(1.,0.,0.));
#40300=DIRECTION('ref_axis',(0.,0.866025403784439,0.5));
#40301=DIRECTION('center_axis',(1.,0.,0.));
#40302=DIRECTION('ref_axis',(0.,0.866025403784439,0.5));
#40303=DIRECTION('',(-1.,0.,0.));
#40304=DIRECTION('center_axis',(-1.,0.,0.));
#40305=DIRECTION('ref_axis',(0.,0.866025403784439,0.5));
#40306=DIRECTION('center_axis',(0.,-0.145138313825661,0.989411375444938));
#40307=DIRECTION('ref_axis',(1.,0.,0.));
#40308=DIRECTION('',(0.,0.989411375444938,0.145138313825661));
#40309=DIRECTION('center_axis',(-1.,0.,0.));
#40310=DIRECTION('ref_axis',(0.,1.,0.));
#40311=DIRECTION('center_axis',(1.,0.,0.));
#40312=DIRECTION('ref_axis',(0.,0.,-1.));
#40313=DIRECTION('center_axis',(0.,-0.968820191500975,0.247764881571245));
#40314=DIRECTION('ref_axis',(0.,-0.247764881571245,-0.968820191500975));
#40315=DIRECTION('',(0.,0.247764881571245,0.968820191500975));
#40316=DIRECTION('',(1.,0.,0.));
#40317=DIRECTION('center_axis',(1.,0.,0.));
#40318=DIRECTION('ref_axis',(0.,0.587785252292473,0.809016994374947));
#40319=DIRECTION('center_axis',(1.,0.,0.));
#40320=DIRECTION('ref_axis',(0.,0.587785252292473,0.809016994374947));
#40321=DIRECTION('',(-1.,0.,0.));
#40322=DIRECTION('center_axis',(-1.,0.,0.));
#40323=DIRECTION('ref_axis',(0.,0.587785252292473,0.809016994374947));
#40324=DIRECTION('center_axis',(0.,-0.535020308794828,0.844839197230507));
#40325=DIRECTION('ref_axis',(1.,0.,0.));
#40326=DIRECTION('',(0.,0.844839197230507,0.535020308794828));
#40327=DIRECTION('center_axis',(-1.,0.,0.));
#40328=DIRECTION('ref_axis',(0.,1.,0.));
#40329=DIRECTION('center_axis',(1.,0.,0.));
#40330=DIRECTION('ref_axis',(0.,0.,-1.));
#40331=DIRECTION('center_axis',(0.,-0.985836341420512,-0.167710190312393));
#40332=DIRECTION('ref_axis',(0.,0.167710190312393,-0.985836341420512));
#40333=DIRECTION('',(0.,-0.167710190312393,0.985836341420512));
#40334=DIRECTION('',(1.,0.,0.));
#40335=DIRECTION('center_axis',(1.,0.,0.));
#40336=DIRECTION('ref_axis',(0.,0.20791169081776,0.978147600733806));
#40337=DIRECTION('center_axis',(1.,0.,0.));
#40338=DIRECTION('ref_axis',(0.,0.20791169081776,0.978147600733806));
#40339=DIRECTION('',(-1.,0.,0.));
#40340=DIRECTION('center_axis',(-1.,0.,0.));
#40341=DIRECTION('ref_axis',(0.,0.20791169081776,0.978147600733806));
#40342=DIRECTION('center_axis',(0.,-0.832392431866445,0.554186646691768));
#40343=DIRECTION('ref_axis',(1.,0.,0.));
#40344=DIRECTION('',(0.,0.554186646691768,0.832392431866445));
#40345=DIRECTION('center_axis',(-1.,0.,0.));
#40346=DIRECTION('ref_axis',(0.,-1.,1.01064309961486E-15));
#40347=DIRECTION('center_axis',(1.,0.,0.));
#40348=DIRECTION('ref_axis',(0.,0.,-1.));
#40349=DIRECTION('center_axis',(0.,-0.832392431866443,-0.55418664669177));
#40350=DIRECTION('ref_axis',(-1.,0.,0.));
#40351=DIRECTION('',(0.,-0.55418664669177,0.832392431866443));
#40352=DIRECTION('',(1.,0.,0.));
#40353=DIRECTION('center_axis',(1.,0.,0.));
#40354=DIRECTION('ref_axis',(0.,-0.207911690817759,0.978147600733806));
#40355=DIRECTION('center_axis',(1.,0.,0.));
#40356=DIRECTION('ref_axis',(0.,-0.207911690817759,0.978147600733806));
#40357=DIRECTION('',(-1.,0.,0.));
#40358=DIRECTION('center_axis',(-1.,0.,0.));
#40359=DIRECTION('ref_axis',(0.,-0.207911690817759,0.978147600733806));
#40360=DIRECTION('center_axis',(0.,-0.985836341420512,0.167710190312393));
#40361=DIRECTION('ref_axis',(0.,-0.167710190312393,-0.985836341420512));
#40362=DIRECTION('',(0.,0.167710190312393,0.985836341420512));
#40363=DIRECTION('center_axis',(-1.,0.,0.));
#40364=DIRECTION('ref_axis',(0.,1.,0.));
#40365=DIRECTION('center_axis',(1.,0.,0.));
#40366=DIRECTION('ref_axis',(0.,0.,-1.));
#40367=DIRECTION('center_axis',(0.,-0.535020308794824,-0.844839197230509));
#40368=DIRECTION('ref_axis',(-1.,0.,0.));
#40369=DIRECTION('',(0.,-0.844839197230509,0.535020308794824));
#40370=DIRECTION('',(1.,0.,0.));
#40371=DIRECTION('center_axis',(1.,0.,0.));
#40372=DIRECTION('ref_axis',(0.,-0.587785252292473,0.809016994374947));
#40373=DIRECTION('center_axis',(1.,0.,0.));
#40374=DIRECTION('ref_axis',(0.,-0.587785252292473,0.809016994374947));
#40375=DIRECTION('',(-1.,0.,0.));
#40376=DIRECTION('center_axis',(-1.,0.,0.));
#40377=DIRECTION('ref_axis',(0.,-0.587785252292473,0.809016994374947));
#40378=DIRECTION('center_axis',(0.,-0.968820191500975,-0.247764881571247));
#40379=DIRECTION('ref_axis',(0.,0.247764881571247,-0.968820191500975));
#40380=DIRECTION('',(0.,-0.247764881571247,0.968820191500975));
#40381=DIRECTION('center_axis',(-1.,0.,0.));
#40382=DIRECTION('ref_axis',(0.,1.,0.));
#40383=DIRECTION('center_axis',(1.,0.,0.));
#40384=DIRECTION('ref_axis',(0.,0.,-1.));
#40385=DIRECTION('center_axis',(0.,-0.145138313825664,-0.989411375444938));
#40386=DIRECTION('ref_axis',(-1.,0.,0.));
#40387=DIRECTION('',(0.,-0.989411375444938,0.145138313825664));
#40388=DIRECTION('',(1.,0.,0.));
#40389=DIRECTION('center_axis',(1.,0.,0.));
#40390=DIRECTION('ref_axis',(0.,-0.866025403784438,0.5));
#40391=DIRECTION('center_axis',(1.,0.,0.));
#40392=DIRECTION('ref_axis',(0.,-0.866025403784438,0.5));
#40393=DIRECTION('',(-1.,0.,0.));
#40394=DIRECTION('center_axis',(-1.,0.,0.));
#40395=DIRECTION('ref_axis',(0.,-0.866025403784438,0.5));
#40396=DIRECTION('center_axis',(0.,-0.784286229015789,-0.620399154557929));
#40397=DIRECTION('ref_axis',(-1.,0.,0.));
#40398=DIRECTION('',(0.,-0.620399154557929,0.784286229015789));
#40399=DIRECTION('center_axis',(-1.,0.,0.));
#40400=DIRECTION('ref_axis',(0.,1.,0.));
#40401=DIRECTION('center_axis',(1.,0.,0.));
#40402=DIRECTION('ref_axis',(0.,0.,-1.));
#40403=DIRECTION('center_axis',(0.,0.269839414144142,-0.962905338324773));
#40404=DIRECTION('ref_axis',(-1.,0.,0.));
#40405=DIRECTION('',(0.,-0.962905338324773,-0.269839414144142));
#40406=DIRECTION('',(1.,0.,0.));
#40407=DIRECTION('center_axis',(1.,0.,0.));
#40408=DIRECTION('ref_axis',(0.,-0.994521895368273,0.104528463267654));
#40409=DIRECTION('center_axis',(1.,0.,0.));
#40410=DIRECTION('ref_axis',(0.,-0.994521895368273,0.104528463267654));
#40411=DIRECTION('',(-1.,0.,0.));
#40412=DIRECTION('center_axis',(-1.,0.,0.));
#40413=DIRECTION('ref_axis',(0.,-0.994521895368273,0.104528463267654));
#40414=DIRECTION('center_axis',(0.,-0.464142052517059,-0.885760777572168));
#40415=DIRECTION('ref_axis',(-1.,0.,0.));
#40416=DIRECTION('',(0.,-0.885760777572168,0.46414205251706));
#40417=DIRECTION('center_axis',(-1.,0.,0.));
#40418=DIRECTION('ref_axis',(0.,1.,0.));
#40419=DIRECTION('center_axis',(1.,0.,0.));
#40420=DIRECTION('ref_axis',(0.,0.,-1.));
#40421=DIRECTION('center_axis',(0.,0.63815945599431,-0.769904220487877));
#40422=DIRECTION('ref_axis',(-1.,0.,0.));
#40423=DIRECTION('',(0.,-0.769904220487877,-0.63815945599431));
#40424=DIRECTION('',(1.,0.,0.));
#40425=DIRECTION('center_axis',(1.,0.,0.));
#40426=DIRECTION('ref_axis',(0.,-0.951056516295154,-0.309016994374947));
#40427=DIRECTION('center_axis',(1.,0.,0.));
#40428=DIRECTION('ref_axis',(0.,-0.951056516295154,-0.309016994374947));
#40429=DIRECTION('',(-1.,0.,0.));
#40430=DIRECTION('center_axis',(-1.,0.,0.));
#40431=DIRECTION('ref_axis',(0.,-0.951056516295154,-0.309016994374947));
#40432=DIRECTION('center_axis',(0.,-0.0637434985399613,-0.997966315260132));
#40433=DIRECTION('ref_axis',(-1.,0.,0.));
#40434=DIRECTION('',(0.,-0.997966315260132,0.0637434985399613));
#40435=DIRECTION('center_axis',(-1.,0.,0.));
#40436=DIRECTION('ref_axis',(0.,1.,0.));
#40437=DIRECTION('center_axis',(1.,0.,0.));
#40438=DIRECTION('ref_axis',(0.,0.,-1.));
#40439=DIRECTION('center_axis',(0.,0.896135930406403,-0.443779668568367));
#40440=DIRECTION('ref_axis',(0.,0.443779668568367,0.896135930406403));
#40441=DIRECTION('',(0.,-0.443779668568367,-0.896135930406403));
#40442=DIRECTION('',(1.,0.,0.));
#40443=DIRECTION('center_axis',(1.,0.,0.));
#40444=DIRECTION('ref_axis',(0.,-0.743144825477395,-0.669130606358858));
#40445=DIRECTION('center_axis',(1.,0.,0.));
#40446=DIRECTION('ref_axis',(0.,-0.743144825477395,-0.669130606358858));
#40447=DIRECTION('',(-1.,0.,0.));
#40448=DIRECTION('center_axis',(-1.,0.,0.));
#40449=DIRECTION('ref_axis',(0.,-0.743144825477395,-0.669130606358858));
#40450=DIRECTION('center_axis',(0.,0.347676885426203,-0.937614410800269));
#40451=DIRECTION('ref_axis',(-1.,0.,0.));
#40452=DIRECTION('',(0.,-0.937614410800269,-0.347676885426203));
#40453=DIRECTION('center_axis',(-1.,0.,0.));
#40454=DIRECTION('ref_axis',(0.,1.,0.));
#40455=DIRECTION('center_axis',(1.,0.,0.));
#40456=DIRECTION('ref_axis',(0.,0.,-1.));
#40457=DIRECTION('center_axis',(0.,0.999162361311885,-0.0409215803416567));
#40458=DIRECTION('ref_axis',(0.,0.0409215803416567,0.999162361311885));
#40459=DIRECTION('',(0.,-0.0409215803416567,-0.999162361311885));
#40460=DIRECTION('',(1.,0.,0.));
#40461=DIRECTION('center_axis',(1.,0.,0.));
#40462=DIRECTION('ref_axis',(0.,-0.406736643075801,-0.913545457642601));
#40463=DIRECTION('center_axis',(1.,0.,0.));
#40464=DIRECTION('ref_axis',(0.,-0.406736643075801,-0.913545457642601));
#40465=DIRECTION('',(-1.,0.,0.));
#40466=DIRECTION('center_axis',(-1.,0.,0.));
#40467=DIRECTION('ref_axis',(0.,-0.406736643075801,-0.913545457642601));
#40468=DIRECTION('center_axis',(0.,0.698980777356831,-0.715140456753525));
#40469=DIRECTION('ref_axis',(-1.,0.,0.));
#40470=DIRECTION('',(0.,-0.715140456753525,-0.698980777356831));
#40471=DIRECTION('center_axis',(0.707106781186543,0.353553390593276,0.612372435695799));
#40472=DIRECTION('ref_axis',(0.654653670707982,0.,-0.75592894601845));
#40473=DIRECTION('',(0.,0.866025403784439,-0.5));
#40474=DIRECTION('',(-0.654653670707982,3.1022589451942E-16,0.75592894601845));
#40475=DIRECTION('',(0.,-0.866025403784439,0.5));
#40476=DIRECTION('',(-0.654653670707982,0.654653670707973,0.377964473009225));
#40477=DIRECTION('center_axis',(0.707106781186543,-0.353553390593276,0.612372435695799));
#40478=DIRECTION('ref_axis',(0.654653670707982,0.,-0.75592894601845));
#40479=DIRECTION('',(0.,0.866025403784439,0.5));
#40480=DIRECTION('',(-0.654653670707982,-0.654653670707973,0.377964473009226));
#40481=DIRECTION('',(0.,-0.866025403784439,-0.5));
#40482=DIRECTION('center_axis',(0.707106781186543,-0.353553390593276,-0.612372435695799));
#40483=DIRECTION('ref_axis',(-0.654653670707982,0.,-0.75592894601845));
#40484=DIRECTION('',(0.,-0.866025403784439,0.5));
#40485=DIRECTION('',(-0.654653670707982,1.38861894618649E-16,-0.75592894601845));
#40486=DIRECTION('',(0.,0.866025403784439,-0.5));
#40487=DIRECTION('',(0.654653670707982,0.654653670707973,0.377964473009225));
#40488=DIRECTION('center_axis',(0.707106781186543,0.353553390593276,-0.612372435695799));
#40489=DIRECTION('ref_axis',(-0.654653670707982,0.,-0.75592894601845));
#40490=DIRECTION('',(0.,0.866025403784439,0.5));
#40491=DIRECTION('',(0.,-0.866025403784439,-0.5));
#40492=DIRECTION('',(-0.654653670707982,0.654653670707973,-0.377964473009225));
#40493=DIRECTION('center_axis',(0.707106781186542,-0.707106781186553,2.26623325918421E-16));
#40494=DIRECTION('ref_axis',(3.20493781063932E-16,0.,-1.));
#40495=DIRECTION('',(0.,3.20493781063927E-16,1.));
#40496=DIRECTION('',(0.,-3.20493781063927E-16,-1.));
#40497=DIRECTION('center_axis',(0.707106781186543,0.707106781186552,1.13311662959211E-16));
#40498=DIRECTION('ref_axis',(1.60246890531966E-16,0.,-1.));
#40499=DIRECTION('',(0.,-1.60246890531964E-16,1.));
#40500=DIRECTION('',(0.,1.60246890531964E-16,-1.));
#40501=DIRECTION('center_axis',(0.,0.5,-0.866025403784439));
#40502=DIRECTION('ref_axis',(0.,-0.866025403784439,-0.5));
#40503=DIRECTION('',(-1.,0.,0.));
#40504=DIRECTION('',(0.,-0.866025403784439,-0.5));
#40505=DIRECTION('',(-1.,0.,0.));
#40506=DIRECTION('center_axis',(0.,1.,-3.20493781063927E-16));
#40507=DIRECTION('ref_axis',(0.,-3.20493781063927E-16,-1.));
#40508=DIRECTION('',(-1.,0.,0.));
#40509=DIRECTION('',(0.,-3.20493781063927E-16,-1.));
#40510=DIRECTION('center_axis',(0.,0.5,0.866025403784439));
#40511=DIRECTION('ref_axis',(0.,0.866025403784439,-0.5));
#40512=DIRECTION('',(-1.,0.,0.));
#40513=DIRECTION('',(0.,0.866025403784439,-0.5));
#40514=DIRECTION('center_axis',(1.,0.,0.));
#40515=DIRECTION('ref_axis',(0.,0.,-1.));
#40516=DIRECTION('center_axis',(1.,0.,0.));
#40517=DIRECTION('ref_axis',(0.,0.,-1.));
#40518=DIRECTION('center_axis',(0.,-0.5,0.866025403784439));
#40519=DIRECTION('ref_axis',(0.,0.866025403784439,0.5));
#40520=DIRECTION('',(-1.,0.,0.));
#40521=DIRECTION('',(0.,0.866025403784439,0.5));
#40522=DIRECTION('center_axis',(0.,-1.,-1.60246890531964E-16));
#40523=DIRECTION('ref_axis',(0.,-1.60246890531964E-16,1.));
#40524=DIRECTION('',(-1.,0.,0.));
#40525=DIRECTION('',(0.,-1.60246890531964E-16,1.));
#40526=DIRECTION('center_axis',(0.,-0.5,-0.866025403784439));
#40527=DIRECTION('ref_axis',(0.,-0.866025403784439,0.5));
#40528=DIRECTION('',(0.,-0.866025403784439,0.5));
#40529=DIRECTION('center_axis',(-1.,0.,0.));
#40530=DIRECTION('ref_axis',(0.,0.,1.));
#40531=DIRECTION('center_axis',(1.,0.,0.));
#40532=DIRECTION('ref_axis',(0.,-0.406736643075801,-0.913545457642601));
#40533=DIRECTION('center_axis',(1.,0.,0.));
#40534=DIRECTION('ref_axis',(0.,-0.743144825477395,-0.669130606358858));
#40535=DIRECTION('center_axis',(1.,0.,0.));
#40536=DIRECTION('ref_axis',(0.,-0.951056516295154,-0.309016994374947));
#40537=DIRECTION('center_axis',(1.,0.,0.));
#40538=DIRECTION('ref_axis',(0.,-0.994521895368273,0.104528463267654));
#40539=DIRECTION('center_axis',(1.,0.,0.));
#40540=DIRECTION('ref_axis',(0.,-0.866025403784438,0.5));
#40541=DIRECTION('center_axis',(1.,0.,0.));
#40542=DIRECTION('ref_axis',(0.,-0.587785252292473,0.809016994374947));
#40543=DIRECTION('center_axis',(1.,0.,0.));
#40544=DIRECTION('ref_axis',(0.,-0.207911690817759,0.978147600733806));
#40545=DIRECTION('center_axis',(1.,0.,0.));
#40546=DIRECTION('ref_axis',(0.,0.20791169081776,0.978147600733805));
#40547=DIRECTION('center_axis',(1.,0.,0.));
#40548=DIRECTION('ref_axis',(0.,0.587785252292473,0.809016994374947));
#40549=DIRECTION('center_axis',(1.,0.,0.));
#40550=DIRECTION('ref_axis',(0.,0.866025403784439,0.5));
#40551=DIRECTION('center_axis',(1.,0.,0.));
#40552=DIRECTION('ref_axis',(0.,0.994521895368273,0.104528463267653));
#40553=DIRECTION('center_axis',(1.,0.,0.));
#40554=DIRECTION('ref_axis',(0.,0.951056516295154,-0.309016994374948));
#40555=DIRECTION('center_axis',(1.,0.,0.));
#40556=DIRECTION('ref_axis',(0.,0.743144825477394,-0.669130606358858));
#40557=DIRECTION('center_axis',(1.,0.,0.));
#40558=DIRECTION('ref_axis',(0.,0.4067366430758,-0.913545457642601));
#40559=DIRECTION('center_axis',(1.,0.,0.));
#40560=DIRECTION('ref_axis',(0.,0.,-1.));
#40561=DIRECTION('center_axis',(-1.,0.,0.));
#40562=DIRECTION('ref_axis',(0.,1.,0.));
#40563=DIRECTION('center_axis',(1.,0.,0.));
#40564=DIRECTION('ref_axis',(0.,1.,0.));
#40565=DIRECTION('center_axis',(1.,0.,0.));
#40566=DIRECTION('ref_axis',(0.,0.,-1.));
#40567=DIRECTION('',(-0.707106781186544,0.707106781186551,8.65956056235498E-17));
#40568=DIRECTION('center_axis',(1.,0.,0.));
#40569=DIRECTION('ref_axis',(0.,1.,0.));
#40570=DIRECTION('center_axis',(1.,0.,0.));
#40571=DIRECTION('ref_axis',(0.,0.,-1.));
#40572=DIRECTION('',(-1.,0.,0.));
#40573=DIRECTION('center_axis',(-1.,0.,0.));
#40574=DIRECTION('ref_axis',(0.,0.,1.));
#40575=DIRECTION('center_axis',(1.,0.,0.));
#40576=DIRECTION('ref_axis',(0.,0.,-1.));
#40577=DIRECTION('center_axis',(1.,0.,0.));
#40578=DIRECTION('ref_axis',(0.,1.,0.));
#40579=DIRECTION('',(-0.70710678118655,0.707106781186545,8.6595605623549E-17));
#40580=DIRECTION('center_axis',(-1.,0.,0.));
#40581=DIRECTION('ref_axis',(0.,0.,1.));
#40582=DIRECTION('axis',(0.,0.,1.));
#40583=DIRECTION('refdir',(1.,0.,0.));
#40584=DIRECTION('center_axis',(1.,0.,0.));
#40585=DIRECTION('ref_axis',(0.,1.,0.));
#40586=DIRECTION('',(-1.,0.,0.));
#40587=DIRECTION('center_axis',(1.,0.,0.));
#40588=DIRECTION('ref_axis',(0.,1.,0.));
#40589=DIRECTION('center_axis',(1.,0.,0.));
#40590=DIRECTION('ref_axis',(0.,1.,0.));
#40591=DIRECTION('',(-1.,0.,0.));
#40592=DIRECTION('center_axis',(1.,0.,0.));
#40593=DIRECTION('ref_axis',(0.,1.,0.));
#40594=DIRECTION('',(-1.,0.,0.));
#40595=DIRECTION('center_axis',(1.,0.,0.));
#40596=DIRECTION('ref_axis',(0.,1.,0.));
#40597=DIRECTION('',(-1.,0.,0.));
#40598=DIRECTION('center_axis',(1.,0.,0.));
#40599=DIRECTION('ref_axis',(0.,1.,0.));
#40600=DIRECTION('',(-1.,0.,0.));
#40601=DIRECTION('center_axis',(1.,0.,0.));
#40602=DIRECTION('ref_axis',(0.,1.,0.));
#40603=DIRECTION('',(-1.,0.,0.));
#40604=DIRECTION('center_axis',(1.,0.,0.));
#40605=DIRECTION('ref_axis',(0.,1.,0.));
#40606=DIRECTION('',(-1.,0.,0.));
#40607=DIRECTION('center_axis',(1.,0.,0.));
#40608=DIRECTION('ref_axis',(5.89165264606854E-17,1.,2.23777851519704E-14));
#40609=DIRECTION('',(1.,0.,0.));
#40610=DIRECTION('center_axis',(1.,0.,0.));
#40611=DIRECTION('ref_axis',(5.89165264606854E-17,1.,2.23777851519704E-14));
#40612=DIRECTION('center_axis',(1.,0.,0.));
#40613=DIRECTION('ref_axis',(5.89165264606854E-17,1.,2.23777851519704E-14));
#40614=DIRECTION('',(1.,0.,0.));
#40615=DIRECTION('center_axis',(1.,0.,0.));
#40616=DIRECTION('ref_axis',(5.89165264606854E-17,1.,2.23777851519704E-14));
#40617=DIRECTION('',(1.,0.,0.));
#40618=DIRECTION('center_axis',(1.,0.,0.));
#40619=DIRECTION('ref_axis',(5.89165264606854E-17,1.,2.23777851519704E-14));
#40620=DIRECTION('',(1.,0.,0.));
#40621=DIRECTION('center_axis',(1.,0.,0.));
#40622=DIRECTION('ref_axis',(5.89165264606854E-17,1.,2.23777851519704E-14));
#40623=DIRECTION('',(1.,0.,0.));
#40624=DIRECTION('center_axis',(1.,0.,0.));
#40625=DIRECTION('ref_axis',(5.89165264606854E-17,1.,2.23777851519704E-14));
#40626=DIRECTION('',(1.,0.,0.));
#40627=DIRECTION('center_axis',(1.,0.,0.));
#40628=DIRECTION('ref_axis',(0.,0.,-1.));
#40629=DIRECTION('center_axis',(-1.,0.,0.));
#40630=DIRECTION('ref_axis',(0.,1.,0.));
#40631=DIRECTION('center_axis',(-1.,0.,0.));
#40632=DIRECTION('ref_axis',(0.,1.,0.));
#40633=DIRECTION('center_axis',(1.,0.,0.));
#40634=DIRECTION('ref_axis',(0.,0.,-1.));
#40635=DIRECTION('center_axis',(1.,0.,0.));
#40636=DIRECTION('ref_axis',(0.,1.,0.));
#40637=DIRECTION('center_axis',(1.,0.,0.));
#40638=DIRECTION('ref_axis',(0.,1.,0.));
#40639=DIRECTION('center_axis',(-1.,0.,0.));
#40640=DIRECTION('ref_axis',(5.89165264606854E-17,1.,2.23777851519704E-14));
#40641=DIRECTION('center_axis',(1.,0.,0.));
#40642=DIRECTION('ref_axis',(5.89165264606854E-17,1.,2.23777851519704E-14));
#40643=DIRECTION('center_axis',(0.,0.5,0.866025403784439));
#40644=DIRECTION('ref_axis',(0.,0.866025403784439,-0.5));
#40645=DIRECTION('',(0.,0.866025403784439,-0.5));
#40646=DIRECTION('',(-1.,0.,0.));
#40647=DIRECTION('',(0.,0.866025403784439,-0.5));
#40648=DIRECTION('',(-1.,0.,0.));
#40649=DIRECTION('center_axis',(0.,-0.5,0.866025403784439));
#40650=DIRECTION('ref_axis',(0.,0.866025403784439,0.5));
#40651=DIRECTION('',(0.,0.866025403784439,0.5));
#40652=DIRECTION('',(-1.,0.,0.));
#40653=DIRECTION('',(0.,0.866025403784439,0.5));
#40654=DIRECTION('center_axis',(0.,-1.,-1.60246890531964E-16));
#40655=DIRECTION('ref_axis',(0.,-1.60246890531964E-16,1.));
#40656=DIRECTION('',(0.,-1.60246890531964E-16,1.));
#40657=DIRECTION('',(-1.,0.,0.));
#40658=DIRECTION('',(0.,-1.60246890531964E-16,1.));
#40659=DIRECTION('center_axis',(0.,-0.5,-0.866025403784439));
#40660=DIRECTION('ref_axis',(0.,-0.866025403784439,0.5));
#40661=DIRECTION('',(0.,-0.866025403784439,0.5));
#40662=DIRECTION('',(-1.,0.,0.));
#40663=DIRECTION('',(0.,-0.866025403784439,0.5));
#40664=DIRECTION('center_axis',(0.,0.5,-0.866025403784439));
#40665=DIRECTION('ref_axis',(0.,-0.866025403784439,-0.5));
#40666=DIRECTION('',(0.,-0.866025403784439,-0.5));
#40667=DIRECTION('',(-1.,0.,0.));
#40668=DIRECTION('',(0.,-0.866025403784439,-0.5));
#40669=DIRECTION('center_axis',(0.,1.,-3.20493781063927E-16));
#40670=DIRECTION('ref_axis',(0.,-3.20493781063927E-16,-1.));
#40671=DIRECTION('',(0.,-3.20493781063927E-16,-1.));
#40672=DIRECTION('',(0.,-3.20493781063927E-16,-1.));
#40673=DIRECTION('center_axis',(-1.,0.,0.));
#40674=DIRECTION('ref_axis',(0.,0.,1.));
#40675=DIRECTION('center_axis',(-1.,0.,0.));
#40676=DIRECTION('ref_axis',(0.,0.,1.));
#40677=DIRECTION('center_axis',(1.,0.,0.));
#40678=DIRECTION('ref_axis',(0.,0.,-1.));
#40679=DIRECTION('center_axis',(1.,0.,0.));
#40680=DIRECTION('ref_axis',(0.,1.,0.));
#40681=DIRECTION('',(-0.707106781186548,0.707106781186547,8.65956056235493E-17));
#40682=DIRECTION('center_axis',(1.,0.,0.));
#40683=DIRECTION('ref_axis',(0.,1.,0.));
#40684=DIRECTION('center_axis',(-1.,0.,0.));
#40685=DIRECTION('ref_axis',(0.,1.,0.));
#40686=DIRECTION('center_axis',(-1.,0.,0.));
#40687=DIRECTION('ref_axis',(0.,1.,0.));
#40688=DIRECTION('center_axis',(1.,0.,0.));
#40689=DIRECTION('ref_axis',(0.,0.,-1.));
#40690=DIRECTION('',(-0.707106781186548,-0.707106781186547,-8.65956056235493E-17));
#40691=DIRECTION('center_axis',(1.,0.,0.));
#40692=DIRECTION('ref_axis',(0.,0.,-1.));
#40693=DIRECTION('',(0.,0.,1.));
#40694=DIRECTION('',(1.,0.,0.));
#40695=DIRECTION('',(0.,0.,1.));
#40696=DIRECTION('',(1.,0.,0.));
#40697=DIRECTION('',(0.,0.,1.));
#40698=DIRECTION('',(1.,0.,0.));
#40699=DIRECTION('',(0.,0.,1.));
#40700=DIRECTION('',(1.,0.,0.));
#40701=DIRECTION('',(0.,0.,1.));
#40702=DIRECTION('',(1.,0.,0.));
#40703=DIRECTION('',(-1.,0.,0.));
#40704=DIRECTION('',(0.,0.,1.));
#40705=DIRECTION('',(-1.,0.,0.));
#40706=DIRECTION('',(0.,0.,1.));
#40707=DIRECTION('',(-1.,0.,0.));
#40708=DIRECTION('',(0.,0.,1.));
#40709=DIRECTION('',(-1.,0.,0.));
#40710=DIRECTION('',(0.,0.,1.));
#40711=DIRECTION('',(-1.,0.,0.));
#40712=DIRECTION('',(0.,0.,1.));
#40713=DIRECTION('',(0.,0.,1.));
#40714=DIRECTION('',(1.,0.,0.));
#40715=DIRECTION('',(-1.,0.,0.));
#40716=DIRECTION('',(0.,0.,1.));
#40717=DIRECTION('',(-1.,0.,0.));
#40718=DIRECTION('',(0.,0.,1.));
#40719=DIRECTION('',(-1.,0.,0.));
#40720=DIRECTION('',(0.,0.,1.));
#40721=DIRECTION('',(-1.,0.,0.));
#40722=DIRECTION('',(0.,0.,1.));
#40723=DIRECTION('',(-1.,0.,0.));
#40724=DIRECTION('',(0.,0.,1.));
#40725=DIRECTION('',(-1.,0.,0.));
#40726=DIRECTION('',(0.,0.,1.));
#40727=DIRECTION('',(-1.,0.,0.));
#40728=DIRECTION('',(0.,0.,1.));
#40729=DIRECTION('',(-1.,0.,0.));
#40730=DIRECTION('',(0.,0.,1.));
#40731=DIRECTION('',(0.,0.,1.));
#40732=DIRECTION('',(0.,-1.,0.));
#40733=DIRECTION('',(0.,0.,1.));
#40734=DIRECTION('',(0.,-1.,0.));
#40735=DIRECTION('',(0.707106781186549,-0.707106781186549,-5.55111512312578E-17));
#40736=DIRECTION('',(-4.16333634234433E-17,5.75982404132925E-18,0.999999999999999));
#40737=DIRECTION('',(0.707106781186549,-0.707106781186549,-5.55111512312578E-17));
#40738=DIRECTION('',(-4.16333634234433E-17,5.75982404132925E-18,0.999999999999999));
#40739=DIRECTION('',(0.707106781186549,-0.707106781186549,-5.55111512312578E-17));
#40740=DIRECTION('',(-4.16333634234433E-17,5.75982404132925E-18,0.999999999999999));
#40741=DIRECTION('',(0.707106781186549,-0.707106781186549,-5.55111512312578E-17));
#40742=DIRECTION('',(-4.16333634234433E-17,5.75982404132925E-18,0.999999999999999));
#40743=DIRECTION('',(-2.77555756156289E-17,-1.08420217248547E-19,1.));
#40744=DIRECTION('',(-0.707106781186547,-0.707106781186547,-9.02056207507939E-17));
#40745=DIRECTION('',(-0.707106781186549,0.707106781186549,5.55111512312578E-17));
#40746=DIRECTION('',(-4.16333634234433E-17,5.75982404132925E-18,0.999999999999999));
#40747=DIRECTION('',(-0.707106781186549,0.707106781186549,5.55111512312578E-17));
#40748=DIRECTION('',(-4.16333634234433E-17,5.75982404132925E-18,0.999999999999999));
#40749=DIRECTION('',(-0.707106781186549,0.707106781186549,5.55111512312578E-17));
#40750=DIRECTION('',(-4.16333634234433E-17,5.75982404132925E-18,0.999999999999999));
#40751=DIRECTION('',(-0.707106781186549,0.707106781186549,5.55111512312578E-17));
#40752=DIRECTION('',(-4.16333634234433E-17,5.75982404132925E-18,0.999999999999999));
#40753=DIRECTION('',(-2.77555756156289E-17,-1.08420217248547E-19,1.));
#40754=DIRECTION('',(0.707106781186547,0.707106781186547,9.02056207507939E-17));
#40755=DIRECTION('',(0.,-1.,0.));
#40756=DIRECTION('',(1.,0.,0.));
#40757=DIRECTION('',(0.,-1.,0.));
#40758=DIRECTION('',(1.,0.,0.));
#40759=DIRECTION('',(0.,-1.,0.));
#40760=DIRECTION('',(1.,0.,0.));
#40761=DIRECTION('',(0.,-1.,0.));
#40762=DIRECTION('',(1.,0.,0.));
#40763=DIRECTION('',(1.,0.,0.));
#40764=DIRECTION('',(0.,0.,1.));
#40765=CARTESIAN_POINT('',(0.,0.,0.));
#40766=CARTESIAN_POINT('',(0.,0.,0.));
#40767=CARTESIAN_POINT('Origin',(85.475,85.475,0.));
#40768=CARTESIAN_POINT('',(85.475,85.475,18.8));
#40769=CARTESIAN_POINT('',(85.725,85.225,18.55));
#40770=CARTESIAN_POINT('',(109.997916666667,60.9520833333331,-5.7229166666665));
#40771=CARTESIAN_POINT('',(85.725,85.225,0.5));
#40772=CARTESIAN_POINT('',(85.725,85.225,0.));
#40773=CARTESIAN_POINT('',(85.475,85.475,0.25));
#40774=CARTESIAN_POINT('',(106.822916666667,64.1270833333331,21.5979166666666));
#40775=CARTESIAN_POINT('',(85.225,85.725,0.5));
#40776=CARTESIAN_POINT('',(78.4145833333332,92.5354166666667,7.31041666666663));
#40777=CARTESIAN_POINT('',(85.225,85.725,18.55));
#40778=CARTESIAN_POINT('',(85.225,85.725,0.));
#40779=CARTESIAN_POINT('',(75.2395833333333,95.7104166666667,8.56458333333343));
#40780=CARTESIAN_POINT('Origin',(85.725,-85.725,0.));
#40781=CARTESIAN_POINT('',(85.725,-85.225,18.55));
#40782=CARTESIAN_POINT('',(85.725,-42.8625,18.55));
#40783=CARTESIAN_POINT('',(85.725,-85.225,0.5));
#40784=CARTESIAN_POINT('',(85.725,-85.225,0.));
#40785=CARTESIAN_POINT('',(85.725,-42.8625,0.5));
#40786=CARTESIAN_POINT('Origin',(85.475,-42.8625,18.8));
#40787=CARTESIAN_POINT('',(85.225,85.225,19.05));
#40788=CARTESIAN_POINT('',(85.225,85.225,19.05));
#40789=CARTESIAN_POINT('',(85.225,-85.225,19.05));
#40790=CARTESIAN_POINT('',(85.225,-42.8625,19.05));
#40791=CARTESIAN_POINT('',(85.475,-85.475,18.8));
#40792=CARTESIAN_POINT('',(85.225,-85.225,19.05));
#40793=CARTESIAN_POINT('',(95.7104166666667,-75.2395833333333,8.56458333333343));
#40794=CARTESIAN_POINT('Origin',(42.8625,85.475,18.8));
#40795=CARTESIAN_POINT('',(-85.225,85.725,18.55));
#40796=CARTESIAN_POINT('',(42.8625,85.725,18.55));
#40797=CARTESIAN_POINT('',(-85.225,85.225,19.05));
#40798=CARTESIAN_POINT('',(-85.225,85.725,18.55));
#40799=CARTESIAN_POINT('',(42.8625,85.225,19.05));
#40800=CARTESIAN_POINT('Origin',(85.475,-85.475,0.));
#40801=CARTESIAN_POINT('',(85.225,-85.725,18.55));
#40802=CARTESIAN_POINT('',(71.4291666666666,-99.5208333333334,4.75416666666677));
#40803=CARTESIAN_POINT('',(85.225,-85.725,0.5));
#40804=CARTESIAN_POINT('',(85.225,-85.725,0.));
#40805=CARTESIAN_POINT('',(85.475,-85.475,0.25));
#40806=CARTESIAN_POINT('',(74.6041666666666,-96.3458333333334,11.1208333333333));
#40807=CARTESIAN_POINT('',(92.5354166666667,-78.4145833333332,7.31041666666663));
#40808=CARTESIAN_POINT('Origin',(85.475,-42.8625,0.25));
#40809=CARTESIAN_POINT('',(85.225,-85.225,0.));
#40810=CARTESIAN_POINT('',(85.225,-85.225,0.));
#40811=CARTESIAN_POINT('',(85.225,85.225,0.));
#40812=CARTESIAN_POINT('',(85.225,-42.8625,0.));
#40813=CARTESIAN_POINT('',(85.225,85.225,0.));
#40814=CARTESIAN_POINT('Origin',(20.,-85.475,0.25));
#40815=CARTESIAN_POINT('',(40.5,-85.725,0.5));
#40816=CARTESIAN_POINT('',(20.,-85.725,0.5));
#40817=CARTESIAN_POINT('',(40.25,-85.475,0.249999999999998));
#40818=CARTESIAN_POINT('',(36.8333333333333,-82.0583333333333,-3.16666666666665));
#40819=CARTESIAN_POINT('',(40.5,-85.225,0.));
#40820=CARTESIAN_POINT('',(40.5,-85.225,0.));
#40821=CARTESIAN_POINT('',(20.,-85.225,0.));
#40822=CARTESIAN_POINT('Origin',(40.,-85.725,0.));
#40823=CARTESIAN_POINT('',(40.5,-85.725,18.55));
#40824=CARTESIAN_POINT('',(20.,-85.725,18.55));
#40825=CARTESIAN_POINT('',(40.5,-85.725,0.));
#40826=CARTESIAN_POINT('',(71.5002890825272,-85.725,7.28103721141815));
#40827=CARTESIAN_POINT('',(74.2629071474075,-85.725,7.28103721141815));
#40828=CARTESIAN_POINT('',(55.7501445412636,-85.725,7.28103721141815));
#40829=CARTESIAN_POINT('',(74.2629071474075,-85.725,6.75000035762787));
#40830=CARTESIAN_POINT('',(74.2629071474075,-85.725,3.64051860570908));
#40831=CARTESIAN_POINT('',(70.9047909975052,-85.725,6.75000035762787));
#40832=CARTESIAN_POINT('',(57.1314535737038,-85.725,6.75000035762787));
#40833=CARTESIAN_POINT('',(70.9047909975052,-85.725,11.2500002384186));
#40834=CARTESIAN_POINT('',(70.9047909975052,-85.725,3.37500017881393));
#40835=CARTESIAN_POINT('',(74.1585417985916,-85.725,11.2500002384186));
#40836=CARTESIAN_POINT('',(55.4523954987526,-85.725,11.2500002384186));
#40837=CARTESIAN_POINT('',(74.1585417985916,-85.725,10.7189633846283));
#40838=CARTESIAN_POINT('',(74.1585417985916,-85.725,5.62500011920929));
#40839=CARTESIAN_POINT('',(71.5002890825272,-85.725,10.7189633846283));
#40840=CARTESIAN_POINT('',(57.0792708992958,-85.725,10.7189633846283));
#40841=CARTESIAN_POINT('',(71.5002890825272,-85.725,9.3407233953476));
#40842=CARTESIAN_POINT('',(71.5002890825272,-85.725,5.35948169231415));
#40843=CARTESIAN_POINT('',(73.989715218544,-85.725,9.3407233953476));
#40844=CARTESIAN_POINT('',(55.7501445412636,-85.725,9.3407233953476));
#40845=CARTESIAN_POINT('',(73.989715218544,-85.725,8.81275618076324));
#40846=CARTESIAN_POINT('',(73.989715218544,-85.725,4.6703616976738));
#40847=CARTESIAN_POINT('',(71.5002890825272,-85.725,8.81275618076324));
#40848=CARTESIAN_POINT('',(56.994857609272,-85.725,8.81275618076324));
#40849=CARTESIAN_POINT('',(71.5002890825272,-85.725,4.40637809038162));
#40850=CARTESIAN_POINT('',(65.901381611824,-85.725,8.74829494953156));
#40851=CARTESIAN_POINT('',(65.210725903511,-85.725,8.74829494953156));
#40852=CARTESIAN_POINT('',(52.950690805912,-85.725,8.74829494953156));
#40853=CARTESIAN_POINT('',(65.210725903511,-85.725,6.75000035762787));
#40854=CARTESIAN_POINT('',(65.210725903511,-85.725,4.37414747476578));
#40855=CARTESIAN_POINT('',(64.6152278184891,-85.725,6.75000035762787));
#40856=CARTESIAN_POINT('',(52.6053629517555,-85.725,6.75000035762787));
#40857=CARTESIAN_POINT('',(64.6152278184891,-85.725,11.2500002384186));
#40858=CARTESIAN_POINT('',(64.6152278184891,-85.725,3.37500017881393));
#40859=CARTESIAN_POINT('',(66.6104527711868,-85.725,11.2500002384186));
#40860=CARTESIAN_POINT('',(52.3076139092445,-85.725,11.2500002384186));
#40861=CARTESIAN_POINT('',(67.5251885652542,-85.725,11.12875187397));
#40862=CARTESIAN_POINT('Ctrl Pts',(66.6104527711868,-85.725,11.2500002384186));
#40863=CARTESIAN_POINT('Ctrl Pts',(67.2120901346207,-85.725,11.2500002384186));
#40864=CARTESIAN_POINT('Ctrl Pts',(67.5251885652542,-85.725,11.12875187397));
#40865=CARTESIAN_POINT('',(68.0255290269852,-85.725,10.7005458474159));
#40866=CARTESIAN_POINT('Ctrl Pts',(67.5251885652542,-85.725,11.12875187397));
#40867=CARTESIAN_POINT('Ctrl Pts',(67.838284611702,-85.725,11.0075035095215));
#40868=CARTESIAN_POINT('Ctrl Pts',(68.0255290269852,-85.725,10.7005458474159));
#40869=CARTESIAN_POINT('',(68.2127734422684,-85.725,10.0221689939499));
#40870=CARTESIAN_POINT('Ctrl Pts',(68.0255290269852,-85.725,10.7005458474159));
#40871=CARTESIAN_POINT('Ctrl Pts',(68.2127734422684,-85.725,10.3935881853104));
#40872=CARTESIAN_POINT('Ctrl Pts',(68.2127734422684,-85.725,10.0221689939499));
#40873=CARTESIAN_POINT('',(67.9027458429337,-85.725,9.21487057209015));
#40874=CARTESIAN_POINT('Ctrl Pts',(68.2127734422684,-85.725,10.0221689939499));
#40875=CARTESIAN_POINT('Ctrl Pts',(68.2127734422684,-85.725,9.54331541061401));
#40876=CARTESIAN_POINT('Ctrl Pts',(67.9027458429337,-85.725,9.21487057209015));
#40877=CARTESIAN_POINT('',(66.945037484169,-85.725,8.79740798473358));
#40878=CARTESIAN_POINT('Ctrl Pts',(67.9027458429337,-85.725,9.21487057209015));
#40879=CARTESIAN_POINT('Ctrl Pts',(67.5927182435989,-85.725,8.88642573356628));
#40880=CARTESIAN_POINT('Ctrl Pts',(66.945037484169,-85.725,8.79740798473358));
#40881=CARTESIAN_POINT('',(67.3041793107986,-85.725,8.57332909107208));
#40882=CARTESIAN_POINT('Ctrl Pts',(66.945037484169,-85.725,8.79740798473358));
#40883=CARTESIAN_POINT('Ctrl Pts',(67.1813961267471,-85.725,8.68383371829987));
#40884=CARTESIAN_POINT('Ctrl Pts',(67.3041793107986,-85.725,8.57332909107208));
#40885=CARTESIAN_POINT('',(67.7983804941177,-85.725,7.97476136684418));
#40886=CARTESIAN_POINT('Ctrl Pts',(67.3041793107986,-85.725,8.57332909107208));
#40887=CARTESIAN_POINT('Ctrl Pts',(67.5650926828384,-85.725,8.33390200138092));
#40888=CARTESIAN_POINT('Ctrl Pts',(67.7983804941177,-85.725,7.97476136684418));
#40889=CARTESIAN_POINT('',(68.5811229944229,-85.725,6.75000035762787));
#40890=CARTESIAN_POINT('',(65.5769632102546,-85.725,11.450623829166));
#40891=CARTESIAN_POINT('',(67.8321453332901,-85.725,6.75000035762787));
#40892=CARTESIAN_POINT('',(54.2905614972115,-85.725,6.75000035762787));
#40893=CARTESIAN_POINT('',(67.2366472482681,-85.725,7.68622124195099));
#40894=CARTESIAN_POINT('',(65.3520878975123,-85.725,10.6490583463875));
#40895=CARTESIAN_POINT('',(66.8069072961807,-85.725,8.30627584457397));
#40896=CARTESIAN_POINT('Ctrl Pts',(67.2366472482681,-85.725,7.68622124195099));
#40897=CARTESIAN_POINT('Ctrl Pts',(66.9757338762283,-85.725,8.09140527248383));
#40898=CARTESIAN_POINT('Ctrl Pts',(66.8069072961807,-85.725,8.30627584457397));
#40899=CARTESIAN_POINT('',(66.5045520067215,-85.725,8.60709452629089));
#40900=CARTESIAN_POINT('Ctrl Pts',(66.8069072961807,-85.725,8.30627584457397));
#40901=CARTESIAN_POINT('Ctrl Pts',(66.6380807161331,-85.725,8.52114641666412));
#40902=CARTESIAN_POINT('Ctrl Pts',(66.5045520067215,-85.725,8.60709452629089));
#40903=CARTESIAN_POINT('',(66.2328954935074,-85.725,8.72680807113647));
#40904=CARTESIAN_POINT('Ctrl Pts',(66.5045520067215,-85.725,8.60709452629089));
#40905=CARTESIAN_POINT('Ctrl Pts',(66.3710280656815,-85.725,8.69304263591766));
#40906=CARTESIAN_POINT('Ctrl Pts',(66.2328954935074,-85.725,8.72680807113647));
#40907=CARTESIAN_POINT('Ctrl Pts',(66.2328954935074,-85.725,8.72680807113647));
#40908=CARTESIAN_POINT('Ctrl Pts',(66.1315985918045,-85.725,8.74829494953156));
#40909=CARTESIAN_POINT('Ctrl Pts',(65.901381611824,-85.725,8.74829494953156));
#40910=CARTESIAN_POINT('',(61.0207542181015,-85.725,7.28103721141815));
#40911=CARTESIAN_POINT('',(63.7833734750748,-85.725,7.28103721141815));
#40912=CARTESIAN_POINT('',(50.5103771090508,-85.725,7.28103721141815));
#40913=CARTESIAN_POINT('',(63.7833734750748,-85.725,6.75000035762787));
#40914=CARTESIAN_POINT('',(63.7833734750748,-85.725,3.64051860570908));
#40915=CARTESIAN_POINT('',(60.4252561330795,-85.725,6.75000035762787));
#40916=CARTESIAN_POINT('',(51.8916867375374,-85.725,6.75000035762787));
#40917=CARTESIAN_POINT('',(60.4252561330795,-85.725,11.2500002384186));
#40918=CARTESIAN_POINT('',(60.4252561330795,-85.725,3.37500017881393));
#40919=CARTESIAN_POINT('',(63.6790081262589,-85.725,11.2500002384186));
#40920=CARTESIAN_POINT('',(50.2126280665398,-85.725,11.2500002384186));
#40921=CARTESIAN_POINT('',(63.6790081262589,-85.725,10.7189633846283));
#40922=CARTESIAN_POINT('',(63.6790081262589,-85.725,5.62500011920929));
#40923=CARTESIAN_POINT('',(61.0207542181015,-85.725,10.7189633846283));
#40924=CARTESIAN_POINT('',(51.8395040631294,-85.725,10.7189633846283));
#40925=CARTESIAN_POINT('',(61.0207542181015,-85.725,9.3407233953476));
#40926=CARTESIAN_POINT('',(61.0207542181015,-85.725,5.35948169231415));
#40927=CARTESIAN_POINT('',(63.5101815462112,-85.725,9.3407233953476));
#40928=CARTESIAN_POINT('',(50.5103771090508,-85.725,9.3407233953476));
#40929=CARTESIAN_POINT('',(63.5101815462112,-85.725,8.81275618076324));
#40930=CARTESIAN_POINT('',(63.5101815462112,-85.725,4.6703616976738));
#40931=CARTESIAN_POINT('',(61.0207542181015,-85.725,8.81275618076324));
#40932=CARTESIAN_POINT('',(51.7550907731056,-85.725,8.81275618076324));
#40933=CARTESIAN_POINT('',(61.0207542181015,-85.725,4.40637809038162));
#40934=CARTESIAN_POINT('',(51.6278477907181,-85.725,8.033083319664));
#40935=CARTESIAN_POINT('',(52.200324177742,-85.725,9.48345863819122));
#40936=CARTESIAN_POINT('Ctrl Pts',(51.6278477907181,-85.725,8.033083319664));
#40937=CARTESIAN_POINT('Ctrl Pts',(51.827370762825,-85.725,8.7851300239563));
#40938=CARTESIAN_POINT('Ctrl Pts',(52.200324177742,-85.725,9.48345863819122));
#40939=CARTESIAN_POINT('',(52.9938098192215,-85.725,10.6606414318085));
#40940=CARTESIAN_POINT('Ctrl Pts',(52.200324177742,-85.725,9.48345863819122));
#40941=CARTESIAN_POINT('Ctrl Pts',(52.573277592659,-85.725,10.1817872524261));
#40942=CARTESIAN_POINT('Ctrl Pts',(52.9938098192215,-85.725,10.6606414318085));
#40943=CARTESIAN_POINT('',(50.7898535728455,-85.725,10.6606414318085));
#40944=CARTESIAN_POINT('',(46.4969049096107,-85.725,10.6606414318085));
#40945=CARTESIAN_POINT('',(50.7898535728455,-85.725,11.1916782855988));
#40946=CARTESIAN_POINT('',(50.7898535728455,-85.725,5.33032071590424));
#40947=CARTESIAN_POINT('',(53.7028821706772,-85.725,11.1916782855988));
#40948=CARTESIAN_POINT('',(45.3949267864227,-85.725,11.1916782855988));
#40949=CARTESIAN_POINT('',(53.7028821706772,-85.725,10.7619374394417));
#40950=CARTESIAN_POINT('',(53.7028821706772,-85.725,5.59583914279938));
#40951=CARTESIAN_POINT('',(52.8510745763779,-85.725,9.54638504981995));
#40952=CARTESIAN_POINT('Ctrl Pts',(53.7028821706772,-85.725,10.7619374394417));
#40953=CARTESIAN_POINT('Ctrl Pts',(53.2731410264969,-85.725,10.3045704364777));
#40954=CARTESIAN_POINT('Ctrl Pts',(52.8510745763779,-85.725,9.54638504981995));
#40955=CARTESIAN_POINT('',(52.198789358139,-85.725,7.98703992366791));
#40956=CARTESIAN_POINT('Ctrl Pts',(52.8510745763779,-85.725,9.54638504981995));
#40957=CARTESIAN_POINT('Ctrl Pts',(52.4290075302124,-85.725,8.78819906711578));
#40958=CARTESIAN_POINT('Ctrl Pts',(52.198789358139,-85.725,7.98703992366791));
#40959=CARTESIAN_POINT('',(51.9869884252548,-85.725,6.75000035762787));
#40960=CARTESIAN_POINT('Ctrl Pts',(52.198789358139,-85.725,7.98703992366791));
#40961=CARTESIAN_POINT('Ctrl Pts',(52.0330324172974,-85.725,7.42223763465881));
#40962=CARTESIAN_POINT('Ctrl Pts',(51.9869884252548,-85.725,6.75000035762787));
#40963=CARTESIAN_POINT('',(51.4191170930862,-85.725,6.75000035762787));
#40964=CARTESIAN_POINT('',(45.9934942126274,-85.725,6.75000035762787));
#40965=CARTESIAN_POINT('Ctrl Pts',(51.4191170930862,-85.725,6.75000035762787));
#40966=CARTESIAN_POINT('Ctrl Pts',(51.4283254146576,-85.725,7.28103721141815));
#40967=CARTESIAN_POINT('Ctrl Pts',(51.6278477907181,-85.725,8.033083319664));
#40968=CARTESIAN_POINT('',(57.9358288049698,-85.725,6.6732611656189));
#40969=CARTESIAN_POINT('',(56.9121249914169,-85.725,6.8512966632843));
#40970=CARTESIAN_POINT('Ctrl Pts',(57.9358288049698,-85.725,6.6732611656189));
#40971=CARTESIAN_POINT('Ctrl Pts',(57.3249825239182,-85.725,6.6732611656189));
#40972=CARTESIAN_POINT('Ctrl Pts',(56.9121249914169,-85.725,6.8512966632843));
#40973=CARTESIAN_POINT('',(56.264444231987,-85.725,7.38693737983704));
#40974=CARTESIAN_POINT('Ctrl Pts',(56.9121249914169,-85.725,6.8512966632843));
#40975=CARTESIAN_POINT('Ctrl Pts',(56.4992662668228,-85.725,7.02933156490326));
#40976=CARTESIAN_POINT('Ctrl Pts',(56.264444231987,-85.725,7.38693737983704));
#40977=CARTESIAN_POINT('',(56.0173436403275,-85.725,8.19577121734619));
#40978=CARTESIAN_POINT('Ctrl Pts',(56.264444231987,-85.725,7.38693737983704));
#40979=CARTESIAN_POINT('Ctrl Pts',(56.0296221971512,-85.725,7.74454319477081));
#40980=CARTESIAN_POINT('Ctrl Pts',(56.0173436403275,-85.725,8.19577121734619));
#40981=CARTESIAN_POINT('',(56.5790756940842,-85.725,8.24488425254822));
#40982=CARTESIAN_POINT('',(47.7138617611228,-85.725,7.46978594535495));
#40983=CARTESIAN_POINT('',(56.764784693718,-85.725,7.69082570075989));
#40984=CARTESIAN_POINT('Ctrl Pts',(56.5790756940842,-85.725,8.24488425254822));
#40985=CARTESIAN_POINT('Ctrl Pts',(56.6189798116684,-85.725,7.907231092453));
#40986=CARTESIAN_POINT('Ctrl Pts',(56.764784693718,-85.725,7.69082570075989));
#40987=CARTESIAN_POINT('',(57.2175475358963,-85.725,7.34089398384094));
#40988=CARTESIAN_POINT('Ctrl Pts',(56.764784693718,-85.725,7.69082570075989));
#40989=CARTESIAN_POINT('Ctrl Pts',(56.9105907678604,-85.725,7.47442030906677));
#40990=CARTESIAN_POINT('Ctrl Pts',(57.2175475358963,-85.725,7.34089398384094));
#40991=CARTESIAN_POINT('',(57.9082020521164,-85.725,7.20736706256866));
#40992=CARTESIAN_POINT('Ctrl Pts',(57.2175475358963,-85.725,7.34089398384094));
#40993=CARTESIAN_POINT('Ctrl Pts',(57.5245054960251,-85.725,7.20736706256866));
#40994=CARTESIAN_POINT('Ctrl Pts',(57.9082020521164,-85.725,7.20736706256866));
#40995=CARTESIAN_POINT('',(58.5098394155502,-85.725,7.3086633682251));
#40996=CARTESIAN_POINT('Ctrl Pts',(57.9082020521164,-85.725,7.20736706256866));
#40997=CARTESIAN_POINT('Ctrl Pts',(58.2489248514175,-85.725,7.20736706256866));
#40998=CARTESIAN_POINT('Ctrl Pts',(58.5098394155502,-85.725,7.3086633682251));
#40999=CARTESIAN_POINT('',(58.8981410264969,-85.725,7.58645975589752));
#41000=CARTESIAN_POINT('Ctrl Pts',(58.5098394155502,-85.725,7.3086633682251));
#41001=CARTESIAN_POINT('Ctrl Pts',(58.7707539796829,-85.725,7.40995967388153));
#41002=CARTESIAN_POINT('Ctrl Pts',(58.8981410264969,-85.725,7.58645975589752));
#41003=CARTESIAN_POINT('',(59.0255280733109,-85.725,7.97169172763824));
#41004=CARTESIAN_POINT('Ctrl Pts',(58.8981410264969,-85.725,7.58645975589752));
#41005=CARTESIAN_POINT('Ctrl Pts',(59.0255280733109,-85.725,7.76296103000641));
#41006=CARTESIAN_POINT('Ctrl Pts',(59.0255280733109,-85.725,7.97169172763824));
#41007=CARTESIAN_POINT('',(58.9027448892593,-85.725,8.34157609939575));
#41008=CARTESIAN_POINT('Ctrl Pts',(59.0255280733109,-85.725,7.97169172763824));
#41009=CARTESIAN_POINT('Ctrl Pts',(59.0255280733109,-85.725,8.18349266052246));
#41010=CARTESIAN_POINT('Ctrl Pts',(58.9027448892593,-85.725,8.34157609939575));
#41011=CARTESIAN_POINT('',(58.4975608587265,-85.725,8.60709452629089));
#41012=CARTESIAN_POINT('Ctrl Pts',(58.9027448892593,-85.725,8.34157609939575));
#41013=CARTESIAN_POINT('Ctrl Pts',(58.7799617052078,-85.725,8.4996589422226));
#41014=CARTESIAN_POINT('Ctrl Pts',(58.4975608587265,-85.725,8.60709452629089));
#41015=CARTESIAN_POINT('',(57.6964017152786,-85.725,8.82656896114349));
#41016=CARTESIAN_POINT('Ctrl Pts',(58.4975608587265,-85.725,8.60709452629089));
#41017=CARTESIAN_POINT('Ctrl Pts',(58.3164557218552,-85.725,8.677694439888));
#41018=CARTESIAN_POINT('Ctrl Pts',(57.6964017152786,-85.725,8.82656896114349));
#41019=CARTESIAN_POINT('',(56.8277117013931,-85.725,9.1074355840683));
#41020=CARTESIAN_POINT('Ctrl Pts',(57.6964017152786,-85.725,8.82656896114349));
#41021=CARTESIAN_POINT('Ctrl Pts',(57.0763465166092,-85.725,8.97544348239899));
#41022=CARTESIAN_POINT('Ctrl Pts',(56.8277117013931,-85.725,9.1074355840683));
#41023=CARTESIAN_POINT('',(56.3473221063614,-85.725,9.52643239498138));
#41024=CARTESIAN_POINT('Ctrl Pts',(56.8277117013931,-85.725,9.1074355840683));
#41025=CARTESIAN_POINT('Ctrl Pts',(56.5054055452347,-85.725,9.27626216411591));
#41026=CARTESIAN_POINT('Ctrl Pts',(56.3473221063614,-85.725,9.52643239498138));
#41027=CARTESIAN_POINT('',(56.1892386674881,-85.725,10.0866302251816));
#41028=CARTESIAN_POINT('Ctrl Pts',(56.3473221063614,-85.725,9.52643239498138));
#41029=CARTESIAN_POINT('Ctrl Pts',(56.1892386674881,-85.725,9.77660322189331));
#41030=CARTESIAN_POINT('Ctrl Pts',(56.1892386674881,-85.725,10.0866302251816));
#41031=CARTESIAN_POINT('',(56.3826223611832,-85.725,10.723567545414));
#41032=CARTESIAN_POINT('Ctrl Pts',(56.1892386674881,-85.725,10.0866302251816));
#41033=CARTESIAN_POINT('Ctrl Pts',(56.1892386674881,-85.725,10.427353322506));
#41034=CARTESIAN_POINT('Ctrl Pts',(56.3826223611832,-85.725,10.723567545414));
#41035=CARTESIAN_POINT('',(56.9474240541458,-85.725,11.1732607483864));
#41036=CARTESIAN_POINT('Ctrl Pts',(56.3826223611832,-85.725,10.723567545414));
#41037=CARTESIAN_POINT('Ctrl Pts',(56.5760060548782,-85.725,11.019781768322));
#41038=CARTESIAN_POINT('Ctrl Pts',(56.9474240541458,-85.725,11.1732607483864));
#41039=CARTESIAN_POINT('',(57.773141503334,-85.725,11.3267394304276));
#41040=CARTESIAN_POINT('Ctrl Pts',(56.9474240541458,-85.725,11.1732607483864));
#41041=CARTESIAN_POINT('Ctrl Pts',(57.3188432455063,-85.725,11.3267394304276));
#41042=CARTESIAN_POINT('Ctrl Pts',(57.773141503334,-85.725,11.3267394304276));
#41043=CARTESIAN_POINT('',(58.6556442975998,-85.725,11.1655866503716));
#41044=CARTESIAN_POINT('Ctrl Pts',(57.773141503334,-85.725,11.3267394304276));
#41045=CARTESIAN_POINT('Ctrl Pts',(58.273481965065,-85.725,11.3267394304276));
#41046=CARTESIAN_POINT('Ctrl Pts',(58.6556442975998,-85.725,11.1655866503716));
#41047=CARTESIAN_POINT('',(59.2434688806534,-85.725,10.6913369297981));
#41048=CARTESIAN_POINT('Ctrl Pts',(58.6556442975998,-85.725,11.1655866503716));
#41049=CARTESIAN_POINT('Ctrl Pts',(59.0378066301346,-85.725,11.0044338703156));
#41050=CARTESIAN_POINT('Ctrl Pts',(59.2434688806534,-85.725,10.6913369297981));
#41051=CARTESIAN_POINT('',(59.4644781351089,-85.725,9.98226487636566));
#41052=CARTESIAN_POINT('Ctrl Pts',(59.2434688806534,-85.725,10.6913369297981));
#41053=CARTESIAN_POINT('Ctrl Pts',(59.4491299390793,-85.725,10.3782402873039));
#41054=CARTESIAN_POINT('Ctrl Pts',(59.4644781351089,-85.725,9.98226487636566));
#41055=CARTESIAN_POINT('',(58.8935371637344,-85.725,9.9392911195755));
#41056=CARTESIAN_POINT('',(49.4135069487441,-85.725,9.22574535346662));
#41057=CARTESIAN_POINT('',(58.5819741487503,-85.725,10.5839019417763));
#41058=CARTESIAN_POINT('Ctrl Pts',(58.8935371637344,-85.725,9.9392911195755));
#41059=CARTESIAN_POINT('Ctrl Pts',(58.8474925756454,-85.725,10.3659620285034));
#41060=CARTESIAN_POINT('Ctrl Pts',(58.5819741487503,-85.725,10.5839019417763));
#41061=CARTESIAN_POINT('',(57.7976974248886,-85.725,10.8018418550491));
#41062=CARTESIAN_POINT('Ctrl Pts',(58.5819741487503,-85.725,10.5839019417763));
#41063=CARTESIAN_POINT('Ctrl Pts',(58.3164557218552,-85.725,10.8018418550491));
#41064=CARTESIAN_POINT('Ctrl Pts',(57.7976974248886,-85.725,10.8018418550491));
#41065=CARTESIAN_POINT('',(57.010351061821,-85.725,10.6038540005684));
#41066=CARTESIAN_POINT('Ctrl Pts',(57.7976974248886,-85.725,10.8018418550491));
#41067=CARTESIAN_POINT('Ctrl Pts',(57.2574516534805,-85.725,10.8018418550491));
#41068=CARTESIAN_POINT('Ctrl Pts',(57.010351061821,-85.725,10.6038540005684));
#41069=CARTESIAN_POINT('',(56.7632504701614,-85.725,10.1265349388123));
#41070=CARTESIAN_POINT('Ctrl Pts',(57.010351061821,-85.725,10.6038540005684));
#41071=CARTESIAN_POINT('Ctrl Pts',(56.7632504701614,-85.725,10.4058664441109));
#41072=CARTESIAN_POINT('Ctrl Pts',(56.7632504701614,-85.725,10.1265349388123));
#41073=CARTESIAN_POINT('',(56.9382163286209,-85.725,9.72748959064484));
#41074=CARTESIAN_POINT('Ctrl Pts',(56.7632504701614,-85.725,10.1265349388123));
#41075=CARTESIAN_POINT('Ctrl Pts',(56.7632504701614,-85.725,9.88403820991516));
#41076=CARTESIAN_POINT('Ctrl Pts',(56.9382163286209,-85.725,9.72748959064484));
#41077=CARTESIAN_POINT('',(57.8360673189163,-85.725,9.4067188501358));
#41078=CARTESIAN_POINT('Ctrl Pts',(56.9382163286209,-85.725,9.72748959064484));
#41079=CARTESIAN_POINT('Ctrl Pts',(57.1101125478745,-85.725,9.57094156742096));
#41080=CARTESIAN_POINT('Ctrl Pts',(57.8360673189163,-85.725,9.4067188501358));
#41081=CARTESIAN_POINT('',(58.8321443796158,-85.725,9.11971354484558));
#41082=CARTESIAN_POINT('Ctrl Pts',(57.8360673189163,-85.725,9.4067188501358));
#41083=CARTESIAN_POINT('Ctrl Pts',(58.5620220899582,-85.725,9.24249672889709));
#41084=CARTESIAN_POINT('Ctrl Pts',(58.8321443796158,-85.725,9.11971354484558));
#41085=CARTESIAN_POINT('',(59.412295460701,-85.725,8.66081202030182));
#41086=CARTESIAN_POINT('Ctrl Pts',(58.8321443796158,-85.725,9.11971354484558));
#41087=CARTESIAN_POINT('Ctrl Pts',(59.2250510454178,-85.725,8.93860900402069));
#41088=CARTESIAN_POINT('Ctrl Pts',(59.412295460701,-85.725,8.66081202030182));
#41089=CARTESIAN_POINT('',(59.5995398759842,-85.725,8.02080535888672));
#41090=CARTESIAN_POINT('Ctrl Pts',(59.412295460701,-85.725,8.66081202030182));
#41091=CARTESIAN_POINT('Ctrl Pts',(59.5995398759842,-85.725,8.38301503658295));
#41092=CARTESIAN_POINT('Ctrl Pts',(59.5995398759842,-85.725,8.02080535888672));
#41093=CARTESIAN_POINT('',(59.3938776254654,-85.725,7.34396362304687));
#41094=CARTESIAN_POINT('Ctrl Pts',(59.5995398759842,-85.725,8.02080535888672));
#41095=CARTESIAN_POINT('Ctrl Pts',(59.5995398759842,-85.725,7.66166472434997));
#41096=CARTESIAN_POINT('Ctrl Pts',(59.3938776254654,-85.725,7.34396362304687));
#41097=CARTESIAN_POINT('',(58.8029834032059,-85.725,6.84976184368133));
#41098=CARTESIAN_POINT('Ctrl Pts',(59.3938776254654,-85.725,7.34396362304687));
#41099=CARTESIAN_POINT('Ctrl Pts',(59.1882153749466,-85.725,7.02626252174377));
#41100=CARTESIAN_POINT('Ctrl Pts',(58.8029834032059,-85.725,6.84976184368133));
#41101=CARTESIAN_POINT('Ctrl Pts',(58.8029834032059,-85.725,6.84976184368133));
#41102=CARTESIAN_POINT('Ctrl Pts',(58.417752623558,-85.725,6.6732611656189));
#41103=CARTESIAN_POINT('Ctrl Pts',(57.9358288049698,-85.725,6.6732611656189));
#41104=CARTESIAN_POINT('',(49.7768934965134,-85.725,7.0799800157547));
#41105=CARTESIAN_POINT('',(48.6902626752853,-85.725,6.67019152641296));
#41106=CARTESIAN_POINT('Ctrl Pts',(49.7768934965134,-85.725,7.0799800157547));
#41107=CARTESIAN_POINT('Ctrl Pts',(49.3471523523331,-85.725,6.67019152641296));
#41108=CARTESIAN_POINT('Ctrl Pts',(48.6902626752853,-85.725,6.67019152641296));
#41109=CARTESIAN_POINT('',(47.7064635753632,-85.725,7.02319288253784));
#41110=CARTESIAN_POINT('Ctrl Pts',(48.6902626752853,-85.725,6.67019152641296));
#41111=CARTESIAN_POINT('Ctrl Pts',(48.0978345274925,-85.725,6.67019152641296));
#41112=CARTESIAN_POINT('Ctrl Pts',(47.7064635753632,-85.725,7.02319288253784));
#41113=CARTESIAN_POINT('',(47.2598400115967,-85.725,7.93792688846588));
#41114=CARTESIAN_POINT('Ctrl Pts',(47.7064635753632,-85.725,7.02319288253784));
#41115=CARTESIAN_POINT('Ctrl Pts',(47.3150923252106,-85.725,7.37619423866272));
#41116=CARTESIAN_POINT('Ctrl Pts',(47.2598400115967,-85.725,7.93792688846588));
#41117=CARTESIAN_POINT('',(47.812363743782,-85.725,8.01159644126892));
#41118=CARTESIAN_POINT('',(43.1733746033117,-85.725,7.39306689126227));
#41119=CARTESIAN_POINT('',(48.136204123497,-85.725,7.33475470542908));
#41120=CARTESIAN_POINT('Ctrl Pts',(47.812363743782,-85.725,8.01159644126892));
#41121=CARTESIAN_POINT('Ctrl Pts',(47.9075207710266,-85.725,7.54195117950439));
#41122=CARTESIAN_POINT('Ctrl Pts',(48.136204123497,-85.725,7.33475470542908));
#41123=CARTESIAN_POINT('',(48.6933323144913,-85.725,7.12755823135376));
#41124=CARTESIAN_POINT('Ctrl Pts',(48.136204123497,-85.725,7.33475470542908));
#41125=CARTESIAN_POINT('Ctrl Pts',(48.3648877739906,-85.725,7.12755823135376));
#41126=CARTESIAN_POINT('Ctrl Pts',(48.6933323144913,-85.725,7.12755823135376));
#41127=CARTESIAN_POINT('',(49.351756811142,-85.725,7.3976811170578));
#41128=CARTESIAN_POINT('Ctrl Pts',(48.6933323144913,-85.725,7.12755823135376));
#41129=CARTESIAN_POINT('Ctrl Pts',(49.0831687450409,-85.725,7.12755823135376));
#41130=CARTESIAN_POINT('Ctrl Pts',(49.351756811142,-85.725,7.3976811170578));
#41131=CARTESIAN_POINT('',(49.620344877243,-85.725,8.06684875488281));
#41132=CARTESIAN_POINT('Ctrl Pts',(49.351756811142,-85.725,7.3976811170578));
#41133=CARTESIAN_POINT('Ctrl Pts',(49.620344877243,-85.725,7.66780400276184));
#41134=CARTESIAN_POINT('Ctrl Pts',(49.620344877243,-85.725,8.06684875488281));
#41135=CARTESIAN_POINT('',(49.3717088699341,-85.725,8.69457745552063));
#41136=CARTESIAN_POINT('Ctrl Pts',(49.620344877243,-85.725,8.06684875488281));
#41137=CARTESIAN_POINT('Ctrl Pts',(49.620344877243,-85.725,8.44747626781464));
#41138=CARTESIAN_POINT('Ctrl Pts',(49.3717088699341,-85.725,8.69457745552063));
#41139=CARTESIAN_POINT('',(48.7393763065338,-85.725,8.94167864322662));
#41140=CARTESIAN_POINT('Ctrl Pts',(49.3717088699341,-85.725,8.69457745552063));
#41141=CARTESIAN_POINT('Ctrl Pts',(49.1230734586716,-85.725,8.94167864322662));
#41142=CARTESIAN_POINT('Ctrl Pts',(48.7393763065338,-85.725,8.94167864322662));
#41143=CARTESIAN_POINT('',(48.3495398759842,-85.725,8.88028705120087));
#41144=CARTESIAN_POINT('Ctrl Pts',(48.7393763065338,-85.725,8.94167864322662));
#41145=CARTESIAN_POINT('Ctrl Pts',(48.5828276872635,-85.725,8.94167864322662));
#41146=CARTESIAN_POINT('Ctrl Pts',(48.3495398759842,-85.725,8.88028705120087));
#41147=CARTESIAN_POINT('',(48.4109314680099,-85.725,9.36527991294861));
#41148=CARTESIAN_POINT('',(47.7305213298712,-85.725,3.99004774891496));
#41149=CARTESIAN_POINT('',(48.4999492168427,-85.725,9.35914063453674));
#41150=CARTESIAN_POINT('Ctrl Pts',(48.4109314680099,-85.725,9.36527991294861));
#41151=CARTESIAN_POINT('Ctrl Pts',(48.4661837816238,-85.725,9.35914063453674));
#41152=CARTESIAN_POINT('Ctrl Pts',(48.4999492168427,-85.725,9.35914063453674));
#41153=CARTESIAN_POINT('',(49.1353514194489,-85.725,9.54331481456757));
#41154=CARTESIAN_POINT('Ctrl Pts',(48.4999492168427,-85.725,9.35914063453674));
#41155=CARTESIAN_POINT('Ctrl Pts',(48.8529505729675,-85.725,9.35914063453674));
#41156=CARTESIAN_POINT('Ctrl Pts',(49.1353514194489,-85.725,9.54331481456757));
#41157=CARTESIAN_POINT('',(49.4177528619766,-85.725,10.111187338829));
#41158=CARTESIAN_POINT('Ctrl Pts',(49.1353514194489,-85.725,9.54331481456757));
#41159=CARTESIAN_POINT('Ctrl Pts',(49.4177528619766,-85.725,9.72748959064484));
#41160=CARTESIAN_POINT('Ctrl Pts',(49.4177528619766,-85.725,10.111187338829));
#41161=CARTESIAN_POINT('',(49.2120906114578,-85.725,10.6145974397659));
#41162=CARTESIAN_POINT('Ctrl Pts',(49.4177528619766,-85.725,10.111187338829));
#41163=CARTESIAN_POINT('Ctrl Pts',(49.4177528619766,-85.725,10.4150750637054));
#41164=CARTESIAN_POINT('Ctrl Pts',(49.2120906114578,-85.725,10.6145974397659));
#41165=CARTESIAN_POINT('',(48.6810540556908,-85.725,10.8141201138496));
#41166=CARTESIAN_POINT('Ctrl Pts',(49.2120906114578,-85.725,10.6145974397659));
#41167=CARTESIAN_POINT('Ctrl Pts',(49.0064295530319,-85.725,10.8141201138496));
#41168=CARTESIAN_POINT('Ctrl Pts',(48.6810540556908,-85.725,10.8141201138496));
#41169=CARTESIAN_POINT('',(48.1438782215118,-85.725,10.6115280985832));
#41170=CARTESIAN_POINT('Ctrl Pts',(48.6810540556908,-85.725,10.8141201138496));
#41171=CARTESIAN_POINT('Ctrl Pts',(48.3587484955788,-85.725,10.8141201138496));
#41172=CARTESIAN_POINT('Ctrl Pts',(48.1438782215118,-85.725,10.6115280985832));
#41173=CARTESIAN_POINT('',(47.8676160573959,-85.725,10.0037517547607));
#41174=CARTESIAN_POINT('Ctrl Pts',(48.1438782215118,-85.725,10.6115280985832));
#41175=CARTESIAN_POINT('Ctrl Pts',(47.9290076494217,-85.725,10.4089357852936));
#41176=CARTESIAN_POINT('Ctrl Pts',(47.8676160573959,-85.725,10.0037517547607));
#41177=CARTESIAN_POINT('',(47.3150923252106,-85.725,10.1019784212112));
#41178=CARTESIAN_POINT('',(44.9163087580087,-85.725,10.528429810748));
#41179=CARTESIAN_POINT('',(47.7755289673805,-85.725,10.9629946351051));
#41180=CARTESIAN_POINT('Ctrl Pts',(47.3150923252106,-85.725,10.1019784212112));
#41181=CARTESIAN_POINT('Ctrl Pts',(47.4163883328438,-85.725,10.6575717926025));
#41182=CARTESIAN_POINT('Ctrl Pts',(47.7755289673805,-85.725,10.9629946351051));
#41183=CARTESIAN_POINT('',(48.6687757968903,-85.725,11.2684174776077));
#41184=CARTESIAN_POINT('Ctrl Pts',(47.7755289673805,-85.725,10.9629946351051));
#41185=CARTESIAN_POINT('Ctrl Pts',(48.134669303894,-85.725,11.2684174776077));
#41186=CARTESIAN_POINT('Ctrl Pts',(48.6687757968903,-85.725,11.2684174776077));
#41187=CARTESIAN_POINT('',(49.3471523523331,-85.725,11.1103343367577));
#41188=CARTESIAN_POINT('Ctrl Pts',(48.6687757968903,-85.725,11.2684174776077));
#41189=CARTESIAN_POINT('Ctrl Pts',(49.0371247529984,-85.725,11.2684174776077));
#41190=CARTESIAN_POINT('Ctrl Pts',(49.3471523523331,-85.725,11.1103343367577));
#41191=CARTESIAN_POINT('',(49.8214020729065,-85.725,10.6790586709976));
#41192=CARTESIAN_POINT('Ctrl Pts',(49.3471523523331,-85.725,11.1103343367577));
#41193=CARTESIAN_POINT('Ctrl Pts',(49.6571799516678,-85.725,10.9522508978844));
#41194=CARTESIAN_POINT('Ctrl Pts',(49.8214020729065,-85.725,10.6790586709976));
#41195=CARTESIAN_POINT('',(49.9856241941452,-85.725,10.0989087820053));
#41196=CARTESIAN_POINT('Ctrl Pts',(49.8214020729065,-85.725,10.6790586709976));
#41197=CARTESIAN_POINT('Ctrl Pts',(49.9856241941452,-85.725,10.4058664441109));
#41198=CARTESIAN_POINT('Ctrl Pts',(49.9856241941452,-85.725,10.0989087820053));
#41199=CARTESIAN_POINT('',(49.8290761709213,-85.725,9.56787192821503));
#41200=CARTESIAN_POINT('Ctrl Pts',(49.9856241941452,-85.725,10.0989087820053));
#41201=CARTESIAN_POINT('Ctrl Pts',(49.9856241941452,-85.725,9.80729901790619));
#41202=CARTESIAN_POINT('Ctrl Pts',(49.8290761709213,-85.725,9.56787192821503));
#41203=CARTESIAN_POINT('',(49.3655695915222,-85.725,9.1872444152832));
#41204=CARTESIAN_POINT('Ctrl Pts',(49.8290761709213,-85.725,9.56787192821503));
#41205=CARTESIAN_POINT('Ctrl Pts',(49.672527551651,-85.725,9.32844483852386));
#41206=CARTESIAN_POINT('Ctrl Pts',(49.3655695915222,-85.725,9.1872444152832));
#41207=CARTESIAN_POINT('',(49.9856241941452,-85.725,8.80508208274841));
#41208=CARTESIAN_POINT('Ctrl Pts',(49.3655695915222,-85.725,9.1872444152832));
#41209=CARTESIAN_POINT('Ctrl Pts',(49.7646149396896,-85.725,9.09515702724457));
#41210=CARTESIAN_POINT('Ctrl Pts',(49.9856241941452,-85.725,8.80508208274841));
#41211=CARTESIAN_POINT('',(50.2066334486008,-85.725,8.07912731170654));
#41212=CARTESIAN_POINT('Ctrl Pts',(49.9856241941452,-85.725,8.80508208274841));
#41213=CARTESIAN_POINT('Ctrl Pts',(50.2066334486008,-85.725,8.51500713825226));
#41214=CARTESIAN_POINT('Ctrl Pts',(50.2066334486008,-85.725,8.07912731170654));
#41215=CARTESIAN_POINT('Ctrl Pts',(50.2066334486008,-85.725,8.07912731170654));
#41216=CARTESIAN_POINT('Ctrl Pts',(50.2066334486008,-85.725,7.48976850509643));
#41217=CARTESIAN_POINT('Ctrl Pts',(49.7768934965134,-85.725,7.0799800157547));
#41218=CARTESIAN_POINT('',(69.2472215890884,-85.725,11.2500002384186));
#41219=CARTESIAN_POINT('',(69.8427196741104,-85.725,11.2500002384186));
#41220=CARTESIAN_POINT('',(54.6236107945442,-85.725,11.2500002384186));
#41221=CARTESIAN_POINT('',(69.8427196741104,-85.725,6.75000035762787));
#41222=CARTESIAN_POINT('',(69.8427196741104,-85.725,5.62500011920929));
#41223=CARTESIAN_POINT('',(69.2472215890884,-85.725,6.75000035762787));
#41224=CARTESIAN_POINT('',(54.9213598370552,-85.725,6.75000035762787));
#41225=CARTESIAN_POINT('',(69.2472215890884,-85.725,3.37500017881393));
#41226=CARTESIAN_POINT('',(76.8014498949051,-85.725,6.6732611656189));
#41227=CARTESIAN_POINT('',(75.7777472734451,-85.725,6.8512966632843));
#41228=CARTESIAN_POINT('Ctrl Pts',(76.8014498949051,-85.725,6.6732611656189));
#41229=CARTESIAN_POINT('Ctrl Pts',(76.1906048059464,-85.725,6.6732611656189));
#41230=CARTESIAN_POINT('Ctrl Pts',(75.7777472734451,-85.725,6.8512966632843));
#41231=CARTESIAN_POINT('',(75.1300665140152,-85.725,7.38693737983704));
#41232=CARTESIAN_POINT('Ctrl Pts',(75.7777472734451,-85.725,6.8512966632843));
#41233=CARTESIAN_POINT('Ctrl Pts',(75.3648873567581,-85.725,7.02933156490326));
#41234=CARTESIAN_POINT('Ctrl Pts',(75.1300665140152,-85.725,7.38693737983704));
#41235=CARTESIAN_POINT('',(74.8829647302628,-85.725,8.19577121734619));
#41236=CARTESIAN_POINT('Ctrl Pts',(75.1300665140152,-85.725,7.38693737983704));
#41237=CARTESIAN_POINT('Ctrl Pts',(74.8952432870865,-85.725,7.74454319477081));
#41238=CARTESIAN_POINT('Ctrl Pts',(74.8829647302628,-85.725,8.19577121734619));
#41239=CARTESIAN_POINT('',(75.4446979761124,-85.725,8.24488425254822));
#41240=CARTESIAN_POINT('',(57.2182322749014,-85.725,6.65132172405981));
#41241=CARTESIAN_POINT('',(75.6304069757462,-85.725,7.69082570075989));
#41242=CARTESIAN_POINT('Ctrl Pts',(75.4446979761124,-85.725,8.24488425254822));
#41243=CARTESIAN_POINT('Ctrl Pts',(75.4846020936966,-85.725,7.907231092453));
#41244=CARTESIAN_POINT('Ctrl Pts',(75.6304069757462,-85.725,7.69082570075989));
#41245=CARTESIAN_POINT('',(76.0831686258316,-85.725,7.34089398384094));
#41246=CARTESIAN_POINT('Ctrl Pts',(75.6304069757462,-85.725,7.69082570075989));
#41247=CARTESIAN_POINT('Ctrl Pts',(75.7762118577957,-85.725,7.47442030906677));
#41248=CARTESIAN_POINT('Ctrl Pts',(76.0831686258316,-85.725,7.34089398384094));
#41249=CARTESIAN_POINT('',(76.7738243341446,-85.725,7.20736706256866));
#41250=CARTESIAN_POINT('Ctrl Pts',(76.0831686258316,-85.725,7.34089398384094));
#41251=CARTESIAN_POINT('Ctrl Pts',(76.3901277780533,-85.725,7.20736706256866));
#41252=CARTESIAN_POINT('Ctrl Pts',(76.7738243341446,-85.725,7.20736706256866));
#41253=CARTESIAN_POINT('',(77.3754616975784,-85.725,7.3086633682251));
#41254=CARTESIAN_POINT('Ctrl Pts',(76.7738243341446,-85.725,7.20736706256866));
#41255=CARTESIAN_POINT('Ctrl Pts',(77.1145459413528,-85.725,7.20736706256866));
#41256=CARTESIAN_POINT('Ctrl Pts',(77.3754616975784,-85.725,7.3086633682251));
#41257=CARTESIAN_POINT('',(77.7637621164322,-85.725,7.58645975589752));
#41258=CARTESIAN_POINT('Ctrl Pts',(77.3754616975784,-85.725,7.3086633682251));
#41259=CARTESIAN_POINT('Ctrl Pts',(77.6363750696182,-85.725,7.40995967388153));
#41260=CARTESIAN_POINT('Ctrl Pts',(77.7637621164322,-85.725,7.58645975589752));
#41261=CARTESIAN_POINT('',(77.8911491632462,-85.725,7.97169172763824));
#41262=CARTESIAN_POINT('Ctrl Pts',(77.7637621164322,-85.725,7.58645975589752));
#41263=CARTESIAN_POINT('Ctrl Pts',(77.8911491632462,-85.725,7.76296103000641));
#41264=CARTESIAN_POINT('Ctrl Pts',(77.8911491632462,-85.725,7.97169172763824));
#41265=CARTESIAN_POINT('',(77.7683659791946,-85.725,8.34157609939575));
#41266=CARTESIAN_POINT('Ctrl Pts',(77.8911491632462,-85.725,7.97169172763824));
#41267=CARTESIAN_POINT('Ctrl Pts',(77.8911491632462,-85.725,8.18349266052246));
#41268=CARTESIAN_POINT('Ctrl Pts',(77.7683659791946,-85.725,8.34157609939575));
#41269=CARTESIAN_POINT('',(77.3631831407547,-85.725,8.60709452629089));
#41270=CARTESIAN_POINT('Ctrl Pts',(77.7683659791946,-85.725,8.34157609939575));
#41271=CARTESIAN_POINT('Ctrl Pts',(77.6455851793289,-85.725,8.4996589422226));
#41272=CARTESIAN_POINT('Ctrl Pts',(77.3631831407547,-85.725,8.60709452629089));
#41273=CARTESIAN_POINT('',(76.5620228052139,-85.725,8.82656896114349));
#41274=CARTESIAN_POINT('Ctrl Pts',(77.3631831407547,-85.725,8.60709452629089));
#41275=CARTESIAN_POINT('Ctrl Pts',(77.1820780038834,-85.725,8.677694439888));
#41276=CARTESIAN_POINT('Ctrl Pts',(76.5620228052139,-85.725,8.82656896114349));
#41277=CARTESIAN_POINT('',(75.6933327913284,-85.725,9.1074355840683));
#41278=CARTESIAN_POINT('Ctrl Pts',(76.5620228052139,-85.725,8.82656896114349));
#41279=CARTESIAN_POINT('Ctrl Pts',(75.9419699907303,-85.725,8.97544348239899));
#41280=CARTESIAN_POINT('Ctrl Pts',(75.6933327913284,-85.725,9.1074355840683));
#41281=CARTESIAN_POINT('',(75.2129431962967,-85.725,9.52643239498138));
#41282=CARTESIAN_POINT('Ctrl Pts',(75.6933327913284,-85.725,9.1074355840683));
#41283=CARTESIAN_POINT('Ctrl Pts',(75.37102663517,-85.725,9.27626216411591));
#41284=CARTESIAN_POINT('Ctrl Pts',(75.2129431962967,-85.725,9.52643239498138));
#41285=CARTESIAN_POINT('',(75.0548621416092,-85.725,10.0866302251816));
#41286=CARTESIAN_POINT('Ctrl Pts',(75.2129431962967,-85.725,9.52643239498138));
#41287=CARTESIAN_POINT('Ctrl Pts',(75.0548621416092,-85.725,9.77660322189331));
#41288=CARTESIAN_POINT('Ctrl Pts',(75.0548621416092,-85.725,10.0866302251816));
#41289=CARTESIAN_POINT('',(75.2482434511185,-85.725,10.723567545414));
#41290=CARTESIAN_POINT('Ctrl Pts',(75.0548621416092,-85.725,10.0866302251816));
#41291=CARTESIAN_POINT('Ctrl Pts',(75.0548621416092,-85.725,10.427353322506));
#41292=CARTESIAN_POINT('Ctrl Pts',(75.2482434511185,-85.725,10.723567545414));
#41293=CARTESIAN_POINT('',(75.8130475282669,-85.725,11.1732607483864));
#41294=CARTESIAN_POINT('Ctrl Pts',(75.2482434511185,-85.725,10.723567545414));
#41295=CARTESIAN_POINT('Ctrl Pts',(75.4416271448135,-85.725,11.019781768322));
#41296=CARTESIAN_POINT('Ctrl Pts',(75.8130475282669,-85.725,11.1732607483864));
#41297=CARTESIAN_POINT('',(76.6387625932693,-85.725,11.3267394304276));
#41298=CARTESIAN_POINT('Ctrl Pts',(75.8130475282669,-85.725,11.1732607483864));
#41299=CARTESIAN_POINT('Ctrl Pts',(76.1844655275345,-85.725,11.3267394304276));
#41300=CARTESIAN_POINT('Ctrl Pts',(76.6387625932693,-85.725,11.3267394304276));
#41301=CARTESIAN_POINT('',(77.521266579628,-85.725,11.1655866503716));
#41302=CARTESIAN_POINT('Ctrl Pts',(76.6387625932693,-85.725,11.3267394304276));
#41303=CARTESIAN_POINT('Ctrl Pts',(77.1391030550003,-85.725,11.3267394304276));
#41304=CARTESIAN_POINT('Ctrl Pts',(77.521266579628,-85.725,11.1655866503716));
#41305=CARTESIAN_POINT('',(78.1090899705887,-85.725,10.6913369297981));
#41306=CARTESIAN_POINT('Ctrl Pts',(77.521266579628,-85.725,11.1655866503716));
#41307=CARTESIAN_POINT('Ctrl Pts',(77.9034277200699,-85.725,11.0044338703156));
#41308=CARTESIAN_POINT('Ctrl Pts',(78.1090899705887,-85.725,10.6913369297981));
#41309=CARTESIAN_POINT('',(78.3300992250443,-85.725,9.98226487636566));
#41310=CARTESIAN_POINT('Ctrl Pts',(78.1090899705887,-85.725,10.6913369297981));
#41311=CARTESIAN_POINT('Ctrl Pts',(78.3147522211075,-85.725,10.3782402873039));
#41312=CARTESIAN_POINT('Ctrl Pts',(78.3300992250443,-85.725,9.98226487636566));
#41313=CARTESIAN_POINT('',(77.7591582536697,-85.725,9.9392911195755));
#41314=CARTESIAN_POINT('',(58.899456308451,-85.725,8.51975339997975));
#41315=CARTESIAN_POINT('',(77.4475952386856,-85.725,10.5839019417763));
#41316=CARTESIAN_POINT('Ctrl Pts',(77.7591582536697,-85.725,9.9392911195755));
#41317=CARTESIAN_POINT('Ctrl Pts',(77.7131148576736,-85.725,10.3659620285034));
#41318=CARTESIAN_POINT('Ctrl Pts',(77.4475952386856,-85.725,10.5839019417763));
#41319=CARTESIAN_POINT('',(76.6633197069168,-85.725,10.8018418550491));
#41320=CARTESIAN_POINT('Ctrl Pts',(77.4475952386856,-85.725,10.5839019417763));
#41321=CARTESIAN_POINT('Ctrl Pts',(77.1820780038834,-85.725,10.8018418550491));
#41322=CARTESIAN_POINT('Ctrl Pts',(76.6633197069168,-85.725,10.8018418550491));
#41323=CARTESIAN_POINT('',(75.8759733438492,-85.725,10.6038540005684));
#41324=CARTESIAN_POINT('Ctrl Pts',(76.6633197069168,-85.725,10.8018418550491));
#41325=CARTESIAN_POINT('Ctrl Pts',(76.1230727434158,-85.725,10.8018418550491));
#41326=CARTESIAN_POINT('Ctrl Pts',(75.8759733438492,-85.725,10.6038540005684));
#41327=CARTESIAN_POINT('',(75.6288715600967,-85.725,10.1265349388123));
#41328=CARTESIAN_POINT('Ctrl Pts',(75.8759733438492,-85.725,10.6038540005684));
#41329=CARTESIAN_POINT('Ctrl Pts',(75.6288715600967,-85.725,10.4058664441109));
#41330=CARTESIAN_POINT('Ctrl Pts',(75.6288715600967,-85.725,10.1265349388123));
#41331=CARTESIAN_POINT('',(75.8038374185562,-85.725,9.72748959064484));
#41332=CARTESIAN_POINT('Ctrl Pts',(75.6288715600967,-85.725,10.1265349388123));
#41333=CARTESIAN_POINT('Ctrl Pts',(75.6288715600967,-85.725,9.88403820991516));
#41334=CARTESIAN_POINT('Ctrl Pts',(75.8038374185562,-85.725,9.72748959064484));
#41335=CARTESIAN_POINT('',(76.7016884088516,-85.725,9.4067188501358));
#41336=CARTESIAN_POINT('Ctrl Pts',(75.8038374185562,-85.725,9.72748959064484));
#41337=CARTESIAN_POINT('Ctrl Pts',(75.9757348299026,-85.725,9.57094156742096));
#41338=CARTESIAN_POINT('Ctrl Pts',(76.7016884088516,-85.725,9.4067188501358));
#41339=CARTESIAN_POINT('',(77.6977654695511,-85.725,9.11971354484558));
#41340=CARTESIAN_POINT('Ctrl Pts',(76.7016884088516,-85.725,9.4067188501358));
#41341=CARTESIAN_POINT('Ctrl Pts',(77.4276443719864,-85.725,9.24249672889709));
#41342=CARTESIAN_POINT('Ctrl Pts',(77.6977654695511,-85.725,9.11971354484558));
#41343=CARTESIAN_POINT('',(78.2779165506363,-85.725,8.66081202030182));
#41344=CARTESIAN_POINT('Ctrl Pts',(77.6977654695511,-85.725,9.11971354484558));
#41345=CARTESIAN_POINT('Ctrl Pts',(78.0906721353531,-85.725,8.93860900402069));
#41346=CARTESIAN_POINT('Ctrl Pts',(78.2779165506363,-85.725,8.66081202030182));
#41347=CARTESIAN_POINT('',(78.4651609659195,-85.725,8.02080535888672));
#41348=CARTESIAN_POINT('Ctrl Pts',(78.2779165506363,-85.725,8.66081202030182));
#41349=CARTESIAN_POINT('Ctrl Pts',(78.4651609659195,-85.725,8.38301503658295));
#41350=CARTESIAN_POINT('Ctrl Pts',(78.4651609659195,-85.725,8.02080535888672));
#41351=CARTESIAN_POINT('',(78.2594987154007,-85.725,7.34396362304687));
#41352=CARTESIAN_POINT('Ctrl Pts',(78.4651609659195,-85.725,8.02080535888672));
#41353=CARTESIAN_POINT('Ctrl Pts',(78.4651609659195,-85.725,7.66166472434997));
#41354=CARTESIAN_POINT('Ctrl Pts',(78.2594987154007,-85.725,7.34396362304687));
#41355=CARTESIAN_POINT('',(77.668606877327,-85.725,6.84976184368133));
#41356=CARTESIAN_POINT('Ctrl Pts',(78.2594987154007,-85.725,7.34396362304687));
#41357=CARTESIAN_POINT('Ctrl Pts',(78.0538388490677,-85.725,7.02626252174377));
#41358=CARTESIAN_POINT('Ctrl Pts',(77.668606877327,-85.725,6.84976184368133));
#41359=CARTESIAN_POINT('Ctrl Pts',(77.668606877327,-85.725,6.84976184368133));
#41360=CARTESIAN_POINT('Ctrl Pts',(77.2833749055862,-85.725,6.6732611656189));
#41361=CARTESIAN_POINT('Ctrl Pts',(76.8014498949051,-85.725,6.6732611656189));
#41362=CARTESIAN_POINT('Origin',(40.25,-85.475,0.));
#41363=CARTESIAN_POINT('',(40.25,-85.475,18.8));
#41364=CARTESIAN_POINT('',(40.,-85.225,18.55));
#41365=CARTESIAN_POINT('',(26.7645833333334,-71.9895833333334,5.31458333333331));
#41366=CARTESIAN_POINT('',(40.,-85.225,0.5));
#41367=CARTESIAN_POINT('',(40.,-85.225,0.));
#41368=CARTESIAN_POINT('',(29.9395833333334,-75.1645833333334,10.5604166666667));
#41369=CARTESIAN_POINT('',(40.0083333333333,-85.2333333333333,19.0416666666667));
#41370=CARTESIAN_POINT('Origin',(40.25,-23.3625,0.25));
#41371=CARTESIAN_POINT('',(40.,-46.725,0.5));
#41372=CARTESIAN_POINT('',(40.,-23.3625,0.5));
#41373=CARTESIAN_POINT('',(40.5,-46.225,0.));
#41374=CARTESIAN_POINT('',(40.,-46.725,0.5));
#41375=CARTESIAN_POINT('',(40.5,-23.3625,0.));
#41376=CARTESIAN_POINT('Origin',(-33.475,-46.475,10.75));
#41377=CARTESIAN_POINT('',(-35.525,-46.725,10.75));
#41378=CARTESIAN_POINT('Origin',(-33.475,-46.725,10.75));
#41379=CARTESIAN_POINT('',(-35.025,-46.225,10.75));
#41380=CARTESIAN_POINT('',(-35.275,-46.475,10.75));
#41381=CARTESIAN_POINT('Origin',(-33.475,-46.225,10.75));
#41382=CARTESIAN_POINT('Origin',(-85.725,-46.725,0.));
#41383=CARTESIAN_POINT('',(-85.225,-46.725,18.55));
#41384=CARTESIAN_POINT('',(40.,-46.725,18.55));
#41385=CARTESIAN_POINT('',(-42.8625,-46.725,18.55));
#41386=CARTESIAN_POINT('',(-85.225,-46.725,0.5));
#41387=CARTESIAN_POINT('',(-85.225,-46.725,0.));
#41388=CARTESIAN_POINT('',(-42.8625,-46.725,0.5));
#41389=CARTESIAN_POINT('',(40.,-46.725,0.));
#41390=CARTESIAN_POINT('',(-35.525,-46.725,3.75));
#41391=CARTESIAN_POINT('Origin',(-33.475,-46.725,3.75));
#41392=CARTESIAN_POINT('Origin',(-33.475,-46.725,10.75));
#41393=CARTESIAN_POINT('',(-35.025,-35.725,10.75));
#41394=CARTESIAN_POINT('',(-35.025,-46.725,10.75));
#41395=CARTESIAN_POINT('Origin',(-33.475,-35.725,10.75));
#41396=CARTESIAN_POINT('Origin',(-33.475,-46.475,3.75));
#41397=CARTESIAN_POINT('',(-35.025,-46.225,3.75));
#41398=CARTESIAN_POINT('',(-35.275,-46.475,3.75));
#41399=CARTESIAN_POINT('Origin',(-33.475,-46.225,3.75));
#41400=CARTESIAN_POINT('Origin',(-33.475,-46.725,3.75));
#41401=CARTESIAN_POINT('',(-35.025,-35.725,3.75));
#41402=CARTESIAN_POINT('',(-35.025,-46.725,3.75));
#41403=CARTESIAN_POINT('Origin',(-33.475,-35.725,3.75));
#41404=CARTESIAN_POINT('Origin',(0.,37.5,9.8));
#41405=CARTESIAN_POINT('',(-4.5,37.5,9.55));
#41406=CARTESIAN_POINT('Origin',(0.,37.5,9.55));
#41407=CARTESIAN_POINT('',(-5.,37.5,10.05));
#41408=CARTESIAN_POINT('',(-4.75,37.5,9.8));
#41409=CARTESIAN_POINT('Origin',(0.,37.5,10.05));
#41410=CARTESIAN_POINT('Origin',(0.,37.5,19.05));
#41411=CARTESIAN_POINT('',(-4.5,37.5,0.4));
#41412=CARTESIAN_POINT('',(-4.5,37.5,19.05));
#41413=CARTESIAN_POINT('Origin',(0.,37.5,0.4));
#41414=CARTESIAN_POINT('Origin',(0.,37.5,10.05));
#41415=CARTESIAN_POINT('',(-7.,37.5,10.05));
#41416=CARTESIAN_POINT('Origin',(0.,37.5,10.05));
#41417=CARTESIAN_POINT('Origin',(-37.5,0.,9.8));
#41418=CARTESIAN_POINT('',(-42.,5.51091059616309E-16,9.55));
#41419=CARTESIAN_POINT('Origin',(-37.5,0.,9.55));
#41420=CARTESIAN_POINT('',(-42.5,-6.12323399573677E-16,10.05));
#41421=CARTESIAN_POINT('',(-42.25,5.81707229594993E-16,9.8));
#41422=CARTESIAN_POINT('Origin',(-37.5,0.,10.05));
#41423=CARTESIAN_POINT('Origin',(-37.5,0.,19.05));
#41424=CARTESIAN_POINT('',(-42.,-5.51091059616309E-16,0.4));
#41425=CARTESIAN_POINT('',(-42.,5.51091059616309E-16,19.05));
#41426=CARTESIAN_POINT('Origin',(-37.5,0.,0.4));
#41427=CARTESIAN_POINT('Origin',(-37.5,0.,10.05));
#41428=CARTESIAN_POINT('',(-44.5,-8.57252759403147E-16,10.05));
#41429=CARTESIAN_POINT('Origin',(-37.5,0.,10.05));
#41430=CARTESIAN_POINT('Origin',(37.5,0.,9.8));
#41431=CARTESIAN_POINT('',(33.,5.51091059616309E-16,9.55));
#41432=CARTESIAN_POINT('Origin',(37.5,0.,9.55));
#41433=CARTESIAN_POINT('',(32.5,-6.12323399573677E-16,10.05));
#41434=CARTESIAN_POINT('',(32.75,5.81707229594993E-16,9.8));
#41435=CARTESIAN_POINT('Origin',(37.5,0.,10.05));
#41436=CARTESIAN_POINT('Origin',(37.5,0.,19.05));
#41437=CARTESIAN_POINT('',(33.,-5.51091059616309E-16,0.4));
#41438=CARTESIAN_POINT('',(33.,5.51091059616309E-16,19.05));
#41439=CARTESIAN_POINT('Origin',(37.5,0.,0.4));
#41440=CARTESIAN_POINT('Origin',(37.5,0.,10.05));
#41441=CARTESIAN_POINT('',(30.5,-8.57252759403147E-16,10.05));
#41442=CARTESIAN_POINT('Origin',(37.5,0.,10.05));
#41443=CARTESIAN_POINT('Origin',(0.,-37.5,9.8));
#41444=CARTESIAN_POINT('',(-4.5,-37.5,9.55));
#41445=CARTESIAN_POINT('Origin',(0.,-37.5,9.55));
#41446=CARTESIAN_POINT('',(-5.,-37.5,10.05));
#41447=CARTESIAN_POINT('',(-4.75,-37.5,9.8));
#41448=CARTESIAN_POINT('Origin',(0.,-37.5,10.05));
#41449=CARTESIAN_POINT('Origin',(0.,-37.5,19.05));
#41450=CARTESIAN_POINT('',(-4.5,-37.5,0.4));
#41451=CARTESIAN_POINT('',(-4.5,-37.5,19.05));
#41452=CARTESIAN_POINT('Origin',(0.,-37.5,0.4));
#41453=CARTESIAN_POINT('Origin',(0.,-37.5,10.05));
#41454=CARTESIAN_POINT('',(-7.,-37.5,10.05));
#41455=CARTESIAN_POINT('Origin',(0.,-37.5,10.05));
#41456=CARTESIAN_POINT('Origin',(20.,-85.475,18.8));
#41457=CARTESIAN_POINT('',(40.5,-85.225,19.05));
#41458=CARTESIAN_POINT('',(20.,-85.225,19.05));
#41459=CARTESIAN_POINT('',(40.5,-85.225,19.05));
#41460=CARTESIAN_POINT('Origin',(40.25,-23.3625,18.8));
#41461=CARTESIAN_POINT('',(40.5,-46.225,19.05));
#41462=CARTESIAN_POINT('',(40.5,-23.3625,19.05));
#41463=CARTESIAN_POINT('',(40.5,-46.225,19.05));
#41464=CARTESIAN_POINT('',(40.,-23.3625,18.55));
#41465=CARTESIAN_POINT('Origin',(-85.725,85.225,18.55));
#41466=CARTESIAN_POINT('',(-85.725,85.225,18.55));
#41467=CARTESIAN_POINT('',(-85.725,85.225,18.55));
#41468=CARTESIAN_POINT('',(-85.225,85.225,19.05));
#41469=CARTESIAN_POINT('Origin',(-85.225,-46.725,18.55));
#41470=CARTESIAN_POINT('',(-85.725,-46.225,18.55));
#41471=CARTESIAN_POINT('',(-85.225,-46.225,19.05));
#41472=CARTESIAN_POINT('',(-85.725,-46.225,18.55));
#41473=CARTESIAN_POINT('',(-85.225,-46.725,18.55));
#41474=CARTESIAN_POINT('',(-85.225,-46.225,19.05));
#41475=CARTESIAN_POINT('Origin',(-85.225,85.225,0.));
#41476=CARTESIAN_POINT('',(-85.225,85.725,0.5));
#41477=CARTESIAN_POINT('',(-85.725,85.225,0.5));
#41478=CARTESIAN_POINT('',(-85.225,85.725,0.5));
#41479=CARTESIAN_POINT('',(-85.225,85.225,0.));
#41480=CARTESIAN_POINT('',(-85.225,85.225,0.));
#41481=CARTESIAN_POINT('',(-85.725,85.225,0.5));
#41482=CARTESIAN_POINT('Origin',(-85.225,-46.225,0.));
#41483=CARTESIAN_POINT('',(-85.725,-46.225,0.5));
#41484=CARTESIAN_POINT('',(-85.725,-46.225,0.5));
#41485=CARTESIAN_POINT('',(-85.225,-46.225,0.));
#41486=CARTESIAN_POINT('',(-85.225,-46.225,0.));
#41487=CARTESIAN_POINT('',(-85.225,-46.725,0.5));
#41488=CARTESIAN_POINT('Origin',(-85.475,42.8625,0.25));
#41489=CARTESIAN_POINT('',(-85.725,42.8625,0.5));
#41490=CARTESIAN_POINT('',(-85.225,42.8625,0.));
#41491=CARTESIAN_POINT('Origin',(-42.8625,-46.475,0.25));
#41492=CARTESIAN_POINT('',(-42.8625,-46.225,0.));
#41493=CARTESIAN_POINT('Origin',(-85.475,-46.475,0.));
#41494=CARTESIAN_POINT('',(-85.725,-46.225,0.));
#41495=CARTESIAN_POINT('Origin',(42.8625,85.475,0.25));
#41496=CARTESIAN_POINT('',(42.8625,85.225,0.));
#41497=CARTESIAN_POINT('',(42.8625,85.725,0.5));
#41498=CARTESIAN_POINT('Origin',(-85.475,85.475,0.));
#41499=CARTESIAN_POINT('',(-85.225,85.725,0.));
#41500=CARTESIAN_POINT('',(-85.725,85.225,0.));
#41501=CARTESIAN_POINT('Origin',(-42.8625,-46.475,18.8));
#41502=CARTESIAN_POINT('',(-42.8625,-46.225,19.05));
#41503=CARTESIAN_POINT('Origin',(-85.475,42.8625,18.8));
#41504=CARTESIAN_POINT('',(-85.225,42.8625,19.05));
#41505=CARTESIAN_POINT('',(-85.725,42.8625,18.55));
#41506=CARTESIAN_POINT('Origin',(40.,-46.725,0.));
#41507=CARTESIAN_POINT('Origin',(0.,0.,19.05));
#41508=CARTESIAN_POINT('',(52.8,-78.,19.05));
#41509=CARTESIAN_POINT('Origin',(56.25,-78.,19.05));
#41510=CARTESIAN_POINT('',(15.3,78.,19.05));
#41511=CARTESIAN_POINT('Origin',(18.75,78.,19.05));
#41512=CARTESIAN_POINT('',(-22.2,78.,19.05));
#41513=CARTESIAN_POINT('Origin',(-18.75,78.,19.05));
#41514=CARTESIAN_POINT('',(-59.7,78.,19.05));
#41515=CARTESIAN_POINT('Origin',(-56.25,78.,19.05));
#41516=CARTESIAN_POINT('',(74.55,18.75,19.05));
#41517=CARTESIAN_POINT('Origin',(78.,18.75,19.05));
#41518=CARTESIAN_POINT('',(74.55,56.25,19.05));
#41519=CARTESIAN_POINT('Origin',(78.,56.25,19.05));
#41520=CARTESIAN_POINT('',(-7.4,-37.5,19.05));
#41521=CARTESIAN_POINT('Origin',(0.,-37.5,19.05));
#41522=CARTESIAN_POINT('',(-44.9,-9.06238631369042E-16,19.05));
#41523=CARTESIAN_POINT('Origin',(-37.5,0.,19.05));
#41524=CARTESIAN_POINT('',(-5.5,-6.73555739531044E-16,19.05));
#41525=CARTESIAN_POINT('Origin',(0.,0.,19.05));
#41526=CARTESIAN_POINT('',(-7.4,37.5,19.05));
#41527=CARTESIAN_POINT('Origin',(0.,37.5,19.05));
#41528=CARTESIAN_POINT('',(30.1,-9.06238631369042E-16,19.05));
#41529=CARTESIAN_POINT('Origin',(37.5,0.,19.05));
#41530=CARTESIAN_POINT('',(52.8,78.,19.05));
#41531=CARTESIAN_POINT('Origin',(56.25,78.,19.05));
#41532=CARTESIAN_POINT('',(-81.45,18.75,19.05));
#41533=CARTESIAN_POINT('Origin',(-78.,18.75,19.05));
#41534=CARTESIAN_POINT('',(-81.45,-18.75,19.05));
#41535=CARTESIAN_POINT('Origin',(-78.,-18.75,19.05));
#41536=CARTESIAN_POINT('',(74.55,-18.75,19.05));
#41537=CARTESIAN_POINT('Origin',(78.,-18.75,19.05));
#41538=CARTESIAN_POINT('',(74.55,-56.25,19.05));
#41539=CARTESIAN_POINT('Origin',(78.,-56.25,19.05));
#41540=CARTESIAN_POINT('',(-81.45,56.25,19.05));
#41541=CARTESIAN_POINT('Origin',(-78.,56.25,19.05));
#41542=CARTESIAN_POINT('Origin',(-85.725,85.725,0.));
#41543=CARTESIAN_POINT('Origin',(0.,0.,0.));
#41544=CARTESIAN_POINT('',(-4.45,5.44967825620572E-16,0.));
#41545=CARTESIAN_POINT('Origin',(0.,0.,0.));
#41546=CARTESIAN_POINT('',(32.6,6.00076931582203E-16,0.));
#41547=CARTESIAN_POINT('Origin',(37.5,0.,0.));
#41548=CARTESIAN_POINT('',(-4.9,37.5,0.));
#41549=CARTESIAN_POINT('Origin',(0.,37.5,0.));
#41550=CARTESIAN_POINT('',(-42.4,6.00076931582203E-16,0.));
#41551=CARTESIAN_POINT('Origin',(-37.5,0.,0.));
#41552=CARTESIAN_POINT('',(-4.9,-37.5,0.));
#41553=CARTESIAN_POINT('Origin',(0.,-37.5,0.));
#41554=CARTESIAN_POINT('Origin',(71.5002890825272,-85.725,7.28103721141815));
#41555=CARTESIAN_POINT('',(71.5002890825272,-85.425,7.28103721141815));
#41556=CARTESIAN_POINT('',(71.5002890825272,-85.725,7.28103721141815));
#41557=CARTESIAN_POINT('',(74.2629071474075,-85.425,7.28103721141815));
#41558=CARTESIAN_POINT('',(71.5002890825272,-85.425,7.28103721141815));
#41559=CARTESIAN_POINT('',(74.2629071474075,-85.725,7.28103721141815));
#41560=CARTESIAN_POINT('Origin',(71.5002890825272,-85.725,8.81275618076324));
#41561=CARTESIAN_POINT('',(71.5002890825272,-85.425,8.81275618076324));
#41562=CARTESIAN_POINT('',(71.5002890825272,-85.725,8.81275618076324));
#41563=CARTESIAN_POINT('',(71.5002890825272,-85.425,8.81275618076324));
#41564=CARTESIAN_POINT('Origin',(73.989715218544,-85.725,8.81275618076324));
#41565=CARTESIAN_POINT('',(73.989715218544,-85.425,8.81275618076324));
#41566=CARTESIAN_POINT('',(73.989715218544,-85.725,8.81275618076324));
#41567=CARTESIAN_POINT('',(73.989715218544,-85.425,8.81275618076324));
#41568=CARTESIAN_POINT('Origin',(73.989715218544,-85.725,9.3407233953476));
#41569=CARTESIAN_POINT('',(73.989715218544,-85.425,9.3407233953476));
#41570=CARTESIAN_POINT('',(73.989715218544,-85.725,9.3407233953476));
#41571=CARTESIAN_POINT('',(73.989715218544,-85.425,9.3407233953476));
#41572=CARTESIAN_POINT('Origin',(71.5002890825272,-85.725,9.3407233953476));
#41573=CARTESIAN_POINT('',(71.5002890825272,-85.425,9.3407233953476));
#41574=CARTESIAN_POINT('',(71.5002890825272,-85.725,9.3407233953476));
#41575=CARTESIAN_POINT('',(71.5002890825272,-85.425,9.3407233953476));
#41576=CARTESIAN_POINT('Origin',(71.5002890825272,-85.725,10.7189633846283));
#41577=CARTESIAN_POINT('',(71.5002890825272,-85.425,10.7189633846283));
#41578=CARTESIAN_POINT('',(71.5002890825272,-85.725,10.7189633846283));
#41579=CARTESIAN_POINT('',(71.5002890825272,-85.425,10.7189633846283));
#41580=CARTESIAN_POINT('Origin',(74.1585417985916,-85.725,10.7189633846283));
#41581=CARTESIAN_POINT('',(74.1585417985916,-85.425,10.7189633846283));
#41582=CARTESIAN_POINT('',(74.1585417985916,-85.725,10.7189633846283));
#41583=CARTESIAN_POINT('',(74.1585417985916,-85.425,10.7189633846283));
#41584=CARTESIAN_POINT('Origin',(74.1585417985916,-85.725,11.2500002384186));
#41585=CARTESIAN_POINT('',(74.1585417985916,-85.425,11.2500002384186));
#41586=CARTESIAN_POINT('',(74.1585417985916,-85.725,11.2500002384186));
#41587=CARTESIAN_POINT('',(74.1585417985916,-85.425,11.2500002384186));
#41588=CARTESIAN_POINT('Origin',(70.9047909975052,-85.725,11.2500002384186));
#41589=CARTESIAN_POINT('',(70.9047909975052,-85.425,11.2500002384186));
#41590=CARTESIAN_POINT('',(70.9047909975052,-85.725,11.2500002384186));
#41591=CARTESIAN_POINT('',(70.9047909975052,-85.425,11.2500002384186));
#41592=CARTESIAN_POINT('Origin',(70.9047909975052,-85.725,6.75000035762787));
#41593=CARTESIAN_POINT('',(70.9047909975052,-85.425,6.75000035762787));
#41594=CARTESIAN_POINT('',(70.9047909975052,-85.725,6.75000035762787));
#41595=CARTESIAN_POINT('',(70.9047909975052,-85.425,6.75000035762787));
#41596=CARTESIAN_POINT('Origin',(74.2629071474075,-85.725,6.75000035762787));
#41597=CARTESIAN_POINT('',(74.2629071474075,-85.425,6.75000035762787));
#41598=CARTESIAN_POINT('',(74.2629071474075,-85.725,6.75000035762787));
#41599=CARTESIAN_POINT('',(74.2629071474075,-85.425,6.75000035762787));
#41600=CARTESIAN_POINT('Origin',(74.2629071474075,-85.725,7.28103721141815));
#41601=CARTESIAN_POINT('',(74.2629071474075,-85.425,7.28103721141815));
#41602=CARTESIAN_POINT('Origin',(72.5838490724564,-85.425,9.00000029802322));
#41603=CARTESIAN_POINT('Origin',(65.901381611824,-85.725,8.74829494953156));
#41604=CARTESIAN_POINT('',(65.901381611824,-85.425,8.74829494953156));
#41605=CARTESIAN_POINT('',(65.901381611824,-85.725,8.74829494953156));
#41606=CARTESIAN_POINT('',(65.210725903511,-85.425,8.74829494953156));
#41607=CARTESIAN_POINT('',(65.901381611824,-85.425,8.74829494953156));
#41608=CARTESIAN_POINT('',(65.210725903511,-85.725,8.74829494953156));
#41609=CARTESIAN_POINT('Ctrl Pts',(66.2328954935074,-85.725,8.72680807113647));
#41610=CARTESIAN_POINT('Ctrl Pts',(66.2328954935074,-85.425,8.72680807113647));
#41611=CARTESIAN_POINT('Ctrl Pts',(66.1315985918045,-85.725,8.74829494953156));
#41612=CARTESIAN_POINT('Ctrl Pts',(66.1315985918045,-85.425,8.74829494953156));
#41613=CARTESIAN_POINT('Ctrl Pts',(65.901381611824,-85.725,8.74829494953156));
#41614=CARTESIAN_POINT('Ctrl Pts',(65.901381611824,-85.425,8.74829494953156));
#41615=CARTESIAN_POINT('',(66.2328954935074,-85.425,8.72680807113647));
#41616=CARTESIAN_POINT('',(66.2328954935074,-85.725,8.72680807113647));
#41617=CARTESIAN_POINT('Ctrl Pts',(66.2328954935074,-85.425,8.72680807113647));
#41618=CARTESIAN_POINT('Ctrl Pts',(66.1315985918045,-85.425,8.74829494953156));
#41619=CARTESIAN_POINT('Ctrl Pts',(65.901381611824,-85.425,8.74829494953156));
#41620=CARTESIAN_POINT('Ctrl Pts',(66.5045520067215,-85.725,8.60709452629089));
#41621=CARTESIAN_POINT('Ctrl Pts',(66.5045520067215,-85.425,8.60709452629089));
#41622=CARTESIAN_POINT('Ctrl Pts',(66.3710280656815,-85.725,8.69304263591766));
#41623=CARTESIAN_POINT('Ctrl Pts',(66.3710280656815,-85.425,8.69304263591766));
#41624=CARTESIAN_POINT('Ctrl Pts',(66.2328954935074,-85.725,8.72680807113647));
#41625=CARTESIAN_POINT('Ctrl Pts',(66.2328954935074,-85.425,8.72680807113647));
#41626=CARTESIAN_POINT('',(66.5045520067215,-85.425,8.60709452629089));
#41627=CARTESIAN_POINT('',(66.5045520067215,-85.725,8.60709452629089));
#41628=CARTESIAN_POINT('Ctrl Pts',(66.5045520067215,-85.425,8.60709452629089));
#41629=CARTESIAN_POINT('Ctrl Pts',(66.3710280656815,-85.425,8.69304263591766));
#41630=CARTESIAN_POINT('Ctrl Pts',(66.2328954935074,-85.425,8.72680807113647));
#41631=CARTESIAN_POINT('Ctrl Pts',(66.8069072961807,-85.725,8.30627584457397));
#41632=CARTESIAN_POINT('Ctrl Pts',(66.8069072961807,-85.425,8.30627584457397));
#41633=CARTESIAN_POINT('Ctrl Pts',(66.6380807161331,-85.725,8.52114641666412));
#41634=CARTESIAN_POINT('Ctrl Pts',(66.6380807161331,-85.425,8.52114641666412));
#41635=CARTESIAN_POINT('Ctrl Pts',(66.5045520067215,-85.725,8.60709452629089));
#41636=CARTESIAN_POINT('Ctrl Pts',(66.5045520067215,-85.425,8.60709452629089));
#41637=CARTESIAN_POINT('',(66.8069072961807,-85.425,8.30627584457397));
#41638=CARTESIAN_POINT('',(66.8069072961807,-85.725,8.30627584457397));
#41639=CARTESIAN_POINT('Ctrl Pts',(66.8069072961807,-85.425,8.30627584457397));
#41640=CARTESIAN_POINT('Ctrl Pts',(66.6380807161331,-85.425,8.52114641666412));
#41641=CARTESIAN_POINT('Ctrl Pts',(66.5045520067215,-85.425,8.60709452629089));
#41642=CARTESIAN_POINT('Ctrl Pts',(67.2366472482681,-85.725,7.68622124195099));
#41643=CARTESIAN_POINT('Ctrl Pts',(67.2366472482681,-85.425,7.68622124195099));
#41644=CARTESIAN_POINT('Ctrl Pts',(66.9757338762283,-85.725,8.09140527248383));
#41645=CARTESIAN_POINT('Ctrl Pts',(66.9757338762283,-85.425,8.09140527248383));
#41646=CARTESIAN_POINT('Ctrl Pts',(66.8069072961807,-85.725,8.30627584457397));
#41647=CARTESIAN_POINT('Ctrl Pts',(66.8069072961807,-85.425,8.30627584457397));
#41648=CARTESIAN_POINT('',(67.2366472482681,-85.425,7.68622124195099));
#41649=CARTESIAN_POINT('',(67.2366472482681,-85.725,7.68622124195099));
#41650=CARTESIAN_POINT('Ctrl Pts',(67.2366472482681,-85.425,7.68622124195099));
#41651=CARTESIAN_POINT('Ctrl Pts',(66.9757338762283,-85.425,8.09140527248383));
#41652=CARTESIAN_POINT('Ctrl Pts',(66.8069072961807,-85.425,8.30627584457397));
#41653=CARTESIAN_POINT('Origin',(67.8321453332901,-85.725,6.75000035762787));
#41654=CARTESIAN_POINT('',(67.8321453332901,-85.425,6.75000035762787));
#41655=CARTESIAN_POINT('',(67.8321453332901,-85.725,6.75000035762787));
#41656=CARTESIAN_POINT('',(67.8321453332901,-85.425,6.75000035762787));
#41657=CARTESIAN_POINT('Origin',(68.5811229944229,-85.725,6.75000035762787));
#41658=CARTESIAN_POINT('',(68.5811229944229,-85.425,6.75000035762787));
#41659=CARTESIAN_POINT('',(68.5811229944229,-85.725,6.75000035762787));
#41660=CARTESIAN_POINT('',(68.5811229944229,-85.425,6.75000035762787));
#41661=CARTESIAN_POINT('Origin',(67.7983804941177,-85.725,7.97476136684418));
#41662=CARTESIAN_POINT('',(67.7983804941177,-85.425,7.97476136684418));
#41663=CARTESIAN_POINT('',(67.7983804941177,-85.725,7.97476136684418));
#41664=CARTESIAN_POINT('',(67.7983804941177,-85.425,7.97476136684418));
#41665=CARTESIAN_POINT('Ctrl Pts',(67.3041793107986,-85.725,8.57332909107208));
#41666=CARTESIAN_POINT('Ctrl Pts',(67.3041793107986,-85.425,8.57332909107208));
#41667=CARTESIAN_POINT('Ctrl Pts',(67.5650926828384,-85.725,8.33390200138092));
#41668=CARTESIAN_POINT('Ctrl Pts',(67.5650926828384,-85.425,8.33390200138092));
#41669=CARTESIAN_POINT('Ctrl Pts',(67.7983804941177,-85.725,7.97476136684418));
#41670=CARTESIAN_POINT('Ctrl Pts',(67.7983804941177,-85.425,7.97476136684418));
#41671=CARTESIAN_POINT('',(67.3041793107986,-85.425,8.57332909107208));
#41672=CARTESIAN_POINT('',(67.3041793107986,-85.725,8.57332909107208));
#41673=CARTESIAN_POINT('Ctrl Pts',(67.3041793107986,-85.425,8.57332909107208));
#41674=CARTESIAN_POINT('Ctrl Pts',(67.5650926828384,-85.425,8.33390200138092));
#41675=CARTESIAN_POINT('Ctrl Pts',(67.7983804941177,-85.425,7.97476136684418));
#41676=CARTESIAN_POINT('Ctrl Pts',(66.945037484169,-85.725,8.79740798473358));
#41677=CARTESIAN_POINT('Ctrl Pts',(66.945037484169,-85.425,8.79740798473358));
#41678=CARTESIAN_POINT('Ctrl Pts',(67.1813961267471,-85.725,8.68383371829987));
#41679=CARTESIAN_POINT('Ctrl Pts',(67.1813961267471,-85.425,8.68383371829987));
#41680=CARTESIAN_POINT('Ctrl Pts',(67.3041793107986,-85.725,8.57332909107208));
#41681=CARTESIAN_POINT('Ctrl Pts',(67.3041793107986,-85.425,8.57332909107208));
#41682=CARTESIAN_POINT('',(66.945037484169,-85.425,8.79740798473358));
#41683=CARTESIAN_POINT('',(66.945037484169,-85.725,8.79740798473358));
#41684=CARTESIAN_POINT('Ctrl Pts',(66.945037484169,-85.425,8.79740798473358));
#41685=CARTESIAN_POINT('Ctrl Pts',(67.1813961267471,-85.425,8.68383371829987));
#41686=CARTESIAN_POINT('Ctrl Pts',(67.3041793107986,-85.425,8.57332909107208));
#41687=CARTESIAN_POINT('Ctrl Pts',(67.9027458429337,-85.725,9.21487057209015));
#41688=CARTESIAN_POINT('Ctrl Pts',(67.9027458429337,-85.425,9.21487057209015));
#41689=CARTESIAN_POINT('Ctrl Pts',(67.5927182435989,-85.725,8.88642573356628));
#41690=CARTESIAN_POINT('Ctrl Pts',(67.5927182435989,-85.425,8.88642573356628));
#41691=CARTESIAN_POINT('Ctrl Pts',(66.945037484169,-85.725,8.79740798473358));
#41692=CARTESIAN_POINT('Ctrl Pts',(66.945037484169,-85.425,8.79740798473358));
#41693=CARTESIAN_POINT('',(67.9027458429337,-85.425,9.21487057209015));
#41694=CARTESIAN_POINT('',(67.9027458429337,-85.725,9.21487057209015));
#41695=CARTESIAN_POINT('Ctrl Pts',(67.9027458429337,-85.425,9.21487057209015));
#41696=CARTESIAN_POINT('Ctrl Pts',(67.5927182435989,-85.425,8.88642573356628));
#41697=CARTESIAN_POINT('Ctrl Pts',(66.945037484169,-85.425,8.79740798473358));
#41698=CARTESIAN_POINT('Ctrl Pts',(68.2127734422684,-85.725,10.0221689939499));
#41699=CARTESIAN_POINT('Ctrl Pts',(68.2127734422684,-85.425,10.0221689939499));
#41700=CARTESIAN_POINT('Ctrl Pts',(68.2127734422684,-85.725,9.54331541061401));
#41701=CARTESIAN_POINT('Ctrl Pts',(68.2127734422684,-85.425,9.54331541061401));
#41702=CARTESIAN_POINT('Ctrl Pts',(67.9027458429337,-85.725,9.21487057209015));
#41703=CARTESIAN_POINT('Ctrl Pts',(67.9027458429337,-85.425,9.21487057209015));
#41704=CARTESIAN_POINT('',(68.2127734422684,-85.425,10.0221689939499));
#41705=CARTESIAN_POINT('',(68.2127734422684,-85.725,10.0221689939499));
#41706=CARTESIAN_POINT('Ctrl Pts',(68.2127734422684,-85.425,10.0221689939499));
#41707=CARTESIAN_POINT('Ctrl Pts',(68.2127734422684,-85.425,9.54331541061401));
#41708=CARTESIAN_POINT('Ctrl Pts',(67.9027458429337,-85.425,9.21487057209015));
#41709=CARTESIAN_POINT('Ctrl Pts',(68.0255290269852,-85.725,10.7005458474159));
#41710=CARTESIAN_POINT('Ctrl Pts',(68.0255290269852,-85.425,10.7005458474159));
#41711=CARTESIAN_POINT('Ctrl Pts',(68.2127734422684,-85.725,10.3935881853104));
#41712=CARTESIAN_POINT('Ctrl Pts',(68.2127734422684,-85.425,10.3935881853104));
#41713=CARTESIAN_POINT('Ctrl Pts',(68.2127734422684,-85.725,10.0221689939499));
#41714=CARTESIAN_POINT('Ctrl Pts',(68.2127734422684,-85.425,10.0221689939499));
#41715=CARTESIAN_POINT('',(68.0255290269852,-85.425,10.7005458474159));
#41716=CARTESIAN_POINT('',(68.0255290269852,-85.725,10.7005458474159));
#41717=CARTESIAN_POINT('Ctrl Pts',(68.0255290269852,-85.425,10.7005458474159));
#41718=CARTESIAN_POINT('Ctrl Pts',(68.2127734422684,-85.425,10.3935881853104));
#41719=CARTESIAN_POINT('Ctrl Pts',(68.2127734422684,-85.425,10.0221689939499));
#41720=CARTESIAN_POINT('Ctrl Pts',(67.5251885652542,-85.725,11.12875187397));
#41721=CARTESIAN_POINT('Ctrl Pts',(67.5251885652542,-85.425,11.12875187397));
#41722=CARTESIAN_POINT('Ctrl Pts',(67.838284611702,-85.725,11.0075035095215));
#41723=CARTESIAN_POINT('Ctrl Pts',(67.838284611702,-85.425,11.0075035095215));
#41724=CARTESIAN_POINT('Ctrl Pts',(68.0255290269852,-85.725,10.7005458474159));
#41725=CARTESIAN_POINT('Ctrl Pts',(68.0255290269852,-85.425,10.7005458474159));
#41726=CARTESIAN_POINT('',(67.5251885652542,-85.425,11.12875187397));
#41727=CARTESIAN_POINT('',(67.5251885652542,-85.725,11.12875187397));
#41728=CARTESIAN_POINT('Ctrl Pts',(67.5251885652542,-85.425,11.12875187397));
#41729=CARTESIAN_POINT('Ctrl Pts',(67.838284611702,-85.425,11.0075035095215));
#41730=CARTESIAN_POINT('Ctrl Pts',(68.0255290269852,-85.425,10.7005458474159));
#41731=CARTESIAN_POINT('Ctrl Pts',(66.6104527711868,-85.725,11.2500002384186));
#41732=CARTESIAN_POINT('Ctrl Pts',(66.6104527711868,-85.425,11.2500002384186));
#41733=CARTESIAN_POINT('Ctrl Pts',(67.2120901346207,-85.725,11.2500002384186));
#41734=CARTESIAN_POINT('Ctrl Pts',(67.2120901346207,-85.425,11.2500002384186));
#41735=CARTESIAN_POINT('Ctrl Pts',(67.5251885652542,-85.725,11.12875187397));
#41736=CARTESIAN_POINT('Ctrl Pts',(67.5251885652542,-85.425,11.12875187397));
#41737=CARTESIAN_POINT('',(66.6104527711868,-85.425,11.2500002384186));
#41738=CARTESIAN_POINT('',(66.6104527711868,-85.725,11.2500002384186));
#41739=CARTESIAN_POINT('Ctrl Pts',(66.6104527711868,-85.425,11.2500002384186));
#41740=CARTESIAN_POINT('Ctrl Pts',(67.2120901346207,-85.425,11.2500002384186));
#41741=CARTESIAN_POINT('Ctrl Pts',(67.5251885652542,-85.425,11.12875187397));
#41742=CARTESIAN_POINT('Origin',(64.6152278184891,-85.725,11.2500002384186));
#41743=CARTESIAN_POINT('',(64.6152278184891,-85.425,11.2500002384186));
#41744=CARTESIAN_POINT('',(64.6152278184891,-85.725,11.2500002384186));
#41745=CARTESIAN_POINT('',(64.6152278184891,-85.425,11.2500002384186));
#41746=CARTESIAN_POINT('Origin',(64.6152278184891,-85.725,6.75000035762787));
#41747=CARTESIAN_POINT('',(64.6152278184891,-85.425,6.75000035762787));
#41748=CARTESIAN_POINT('',(64.6152278184891,-85.725,6.75000035762787));
#41749=CARTESIAN_POINT('',(64.6152278184891,-85.425,6.75000035762787));
#41750=CARTESIAN_POINT('Origin',(65.210725903511,-85.725,6.75000035762787));
#41751=CARTESIAN_POINT('',(65.210725903511,-85.425,6.75000035762787));
#41752=CARTESIAN_POINT('',(65.210725903511,-85.725,6.75000035762787));
#41753=CARTESIAN_POINT('',(65.210725903511,-85.425,6.75000035762787));
#41754=CARTESIAN_POINT('Origin',(65.210725903511,-85.725,8.74829494953156));
#41755=CARTESIAN_POINT('',(65.210725903511,-85.425,8.74829494953156));
#41756=CARTESIAN_POINT('Origin',(66.598175406456,-85.425,9.00000029802322));
#41757=CARTESIAN_POINT('Origin',(61.0207542181015,-85.725,7.28103721141815));
#41758=CARTESIAN_POINT('',(61.0207542181015,-85.425,7.28103721141815));
#41759=CARTESIAN_POINT('',(61.0207542181015,-85.725,7.28103721141815));
#41760=CARTESIAN_POINT('',(63.7833734750748,-85.425,7.28103721141815));
#41761=CARTESIAN_POINT('',(61.0207542181015,-85.425,7.28103721141815));
#41762=CARTESIAN_POINT('',(63.7833734750748,-85.725,7.28103721141815));
#41763=CARTESIAN_POINT('Origin',(61.0207542181015,-85.725,8.81275618076324));
#41764=CARTESIAN_POINT('',(61.0207542181015,-85.425,8.81275618076324));
#41765=CARTESIAN_POINT('',(61.0207542181015,-85.725,8.81275618076324));
#41766=CARTESIAN_POINT('',(61.0207542181015,-85.425,8.81275618076324));
#41767=CARTESIAN_POINT('Origin',(63.5101815462112,-85.725,8.81275618076324));
#41768=CARTESIAN_POINT('',(63.5101815462112,-85.425,8.81275618076324));
#41769=CARTESIAN_POINT('',(63.5101815462112,-85.725,8.81275618076324));
#41770=CARTESIAN_POINT('',(63.5101815462112,-85.425,8.81275618076324));
#41771=CARTESIAN_POINT('Origin',(63.5101815462112,-85.725,9.3407233953476));
#41772=CARTESIAN_POINT('',(63.5101815462112,-85.425,9.3407233953476));
#41773=CARTESIAN_POINT('',(63.5101815462112,-85.725,9.3407233953476));
#41774=CARTESIAN_POINT('',(63.5101815462112,-85.425,9.3407233953476));
#41775=CARTESIAN_POINT('Origin',(61.0207542181015,-85.725,9.3407233953476));
#41776=CARTESIAN_POINT('',(61.0207542181015,-85.425,9.3407233953476));
#41777=CARTESIAN_POINT('',(61.0207542181015,-85.725,9.3407233953476));
#41778=CARTESIAN_POINT('',(61.0207542181015,-85.425,9.3407233953476));
#41779=CARTESIAN_POINT('Origin',(61.0207542181015,-85.725,10.7189633846283));
#41780=CARTESIAN_POINT('',(61.0207542181015,-85.425,10.7189633846283));
#41781=CARTESIAN_POINT('',(61.0207542181015,-85.725,10.7189633846283));
#41782=CARTESIAN_POINT('',(61.0207542181015,-85.425,10.7189633846283));
#41783=CARTESIAN_POINT('Origin',(63.6790081262589,-85.725,10.7189633846283));
#41784=CARTESIAN_POINT('',(63.6790081262589,-85.425,10.7189633846283));
#41785=CARTESIAN_POINT('',(63.6790081262589,-85.725,10.7189633846283));
#41786=CARTESIAN_POINT('',(63.6790081262589,-85.425,10.7189633846283));
#41787=CARTESIAN_POINT('Origin',(63.6790081262589,-85.725,11.2500002384186));
#41788=CARTESIAN_POINT('',(63.6790081262589,-85.425,11.2500002384186));
#41789=CARTESIAN_POINT('',(63.6790081262589,-85.725,11.2500002384186));
#41790=CARTESIAN_POINT('',(63.6790081262589,-85.425,11.2500002384186));
#41791=CARTESIAN_POINT('Origin',(60.4252561330795,-85.725,11.2500002384186));
#41792=CARTESIAN_POINT('',(60.4252561330795,-85.425,11.2500002384186));
#41793=CARTESIAN_POINT('',(60.4252561330795,-85.725,11.2500002384186));
#41794=CARTESIAN_POINT('',(60.4252561330795,-85.425,11.2500002384186));
#41795=CARTESIAN_POINT('Origin',(60.4252561330795,-85.725,6.75000035762787));
#41796=CARTESIAN_POINT('',(60.4252561330795,-85.425,6.75000035762787));
#41797=CARTESIAN_POINT('',(60.4252561330795,-85.725,6.75000035762787));
#41798=CARTESIAN_POINT('',(60.4252561330795,-85.425,6.75000035762787));
#41799=CARTESIAN_POINT('Origin',(63.7833734750748,-85.725,6.75000035762787));
#41800=CARTESIAN_POINT('',(63.7833734750748,-85.425,6.75000035762787));
#41801=CARTESIAN_POINT('',(63.7833734750748,-85.725,6.75000035762787));
#41802=CARTESIAN_POINT('',(63.7833734750748,-85.425,6.75000035762787));
#41803=CARTESIAN_POINT('Origin',(63.7833734750748,-85.725,7.28103721141815));
#41804=CARTESIAN_POINT('',(63.7833734750748,-85.425,7.28103721141815));
#41805=CARTESIAN_POINT('Origin',(62.1043148040771,-85.425,9.00000029802322));
#41806=CARTESIAN_POINT('Ctrl Pts',(51.6278477907181,-85.725,8.033083319664));
#41807=CARTESIAN_POINT('Ctrl Pts',(51.6278477907181,-85.425,8.033083319664));
#41808=CARTESIAN_POINT('Ctrl Pts',(51.827370762825,-85.725,8.7851300239563));
#41809=CARTESIAN_POINT('Ctrl Pts',(51.827370762825,-85.425,8.7851300239563));
#41810=CARTESIAN_POINT('Ctrl Pts',(52.200324177742,-85.725,9.48345863819122));
#41811=CARTESIAN_POINT('Ctrl Pts',(52.200324177742,-85.425,9.48345863819122));
#41812=CARTESIAN_POINT('',(51.6278477907181,-85.425,8.033083319664));
#41813=CARTESIAN_POINT('',(51.6278477907181,-85.725,8.033083319664));
#41814=CARTESIAN_POINT('',(52.200324177742,-85.425,9.48345863819122));
#41815=CARTESIAN_POINT('Ctrl Pts',(51.6278477907181,-85.425,8.033083319664));
#41816=CARTESIAN_POINT('Ctrl Pts',(51.827370762825,-85.425,8.7851300239563));
#41817=CARTESIAN_POINT('Ctrl Pts',(52.200324177742,-85.425,9.48345863819122));
#41818=CARTESIAN_POINT('',(52.200324177742,-85.725,9.48345863819122));
#41819=CARTESIAN_POINT('Ctrl Pts',(51.4191170930862,-85.725,6.75000035762787));
#41820=CARTESIAN_POINT('Ctrl Pts',(51.4191170930862,-85.425,6.75000035762787));
#41821=CARTESIAN_POINT('Ctrl Pts',(51.4283254146576,-85.725,7.28103721141815));
#41822=CARTESIAN_POINT('Ctrl Pts',(51.4283254146576,-85.425,7.28103721141815));
#41823=CARTESIAN_POINT('Ctrl Pts',(51.6278477907181,-85.725,8.033083319664));
#41824=CARTESIAN_POINT('Ctrl Pts',(51.6278477907181,-85.425,8.033083319664));
#41825=CARTESIAN_POINT('',(51.4191170930862,-85.425,6.75000035762787));
#41826=CARTESIAN_POINT('',(51.4191170930862,-85.725,6.75000035762787));
#41827=CARTESIAN_POINT('Ctrl Pts',(51.4191170930862,-85.425,6.75000035762787));
#41828=CARTESIAN_POINT('Ctrl Pts',(51.4283254146576,-85.425,7.28103721141815));
#41829=CARTESIAN_POINT('Ctrl Pts',(51.6278477907181,-85.425,8.033083319664));
#41830=CARTESIAN_POINT('Origin',(51.9869884252548,-85.725,6.75000035762787));
#41831=CARTESIAN_POINT('',(51.9869884252548,-85.425,6.75000035762787));
#41832=CARTESIAN_POINT('',(51.9869884252548,-85.725,6.75000035762787));
#41833=CARTESIAN_POINT('',(51.9869884252548,-85.425,6.75000035762787));
#41834=CARTESIAN_POINT('Ctrl Pts',(52.198789358139,-85.725,7.98703992366791));
#41835=CARTESIAN_POINT('Ctrl Pts',(52.198789358139,-85.425,7.98703992366791));
#41836=CARTESIAN_POINT('Ctrl Pts',(52.0330324172974,-85.725,7.42223763465881));
#41837=CARTESIAN_POINT('Ctrl Pts',(52.0330324172974,-85.425,7.42223763465881));
#41838=CARTESIAN_POINT('Ctrl Pts',(51.9869884252548,-85.725,6.75000035762787));
#41839=CARTESIAN_POINT('Ctrl Pts',(51.9869884252548,-85.425,6.75000035762787));
#41840=CARTESIAN_POINT('',(52.198789358139,-85.425,7.98703992366791));
#41841=CARTESIAN_POINT('',(52.198789358139,-85.725,7.98703992366791));
#41842=CARTESIAN_POINT('Ctrl Pts',(52.198789358139,-85.425,7.98703992366791));
#41843=CARTESIAN_POINT('Ctrl Pts',(52.0330324172974,-85.425,7.42223763465881));
#41844=CARTESIAN_POINT('Ctrl Pts',(51.9869884252548,-85.425,6.75000035762787));
#41845=CARTESIAN_POINT('Ctrl Pts',(52.8510745763779,-85.725,9.54638504981995));
#41846=CARTESIAN_POINT('Ctrl Pts',(52.8510745763779,-85.425,9.54638504981995));
#41847=CARTESIAN_POINT('Ctrl Pts',(52.4290075302124,-85.725,8.78819906711578));
#41848=CARTESIAN_POINT('Ctrl Pts',(52.4290075302124,-85.425,8.78819906711578));
#41849=CARTESIAN_POINT('Ctrl Pts',(52.198789358139,-85.725,7.98703992366791));
#41850=CARTESIAN_POINT('Ctrl Pts',(52.198789358139,-85.425,7.98703992366791));
#41851=CARTESIAN_POINT('',(52.8510745763779,-85.425,9.54638504981995));
#41852=CARTESIAN_POINT('',(52.8510745763779,-85.725,9.54638504981995));
#41853=CARTESIAN_POINT('Ctrl Pts',(52.8510745763779,-85.425,9.54638504981995));
#41854=CARTESIAN_POINT('Ctrl Pts',(52.4290075302124,-85.425,8.78819906711578));
#41855=CARTESIAN_POINT('Ctrl Pts',(52.198789358139,-85.425,7.98703992366791));
#41856=CARTESIAN_POINT('Ctrl Pts',(53.7028821706772,-85.725,10.7619374394417));
#41857=CARTESIAN_POINT('Ctrl Pts',(53.7028821706772,-85.425,10.7619374394417));
#41858=CARTESIAN_POINT('Ctrl Pts',(53.2731410264969,-85.725,10.3045704364777));
#41859=CARTESIAN_POINT('Ctrl Pts',(53.2731410264969,-85.425,10.3045704364777));
#41860=CARTESIAN_POINT('Ctrl Pts',(52.8510745763779,-85.725,9.54638504981995));
#41861=CARTESIAN_POINT('Ctrl Pts',(52.8510745763779,-85.425,9.54638504981995));
#41862=CARTESIAN_POINT('',(53.7028821706772,-85.425,10.7619374394417));
#41863=CARTESIAN_POINT('',(53.7028821706772,-85.725,10.7619374394417));
#41864=CARTESIAN_POINT('Ctrl Pts',(53.7028821706772,-85.425,10.7619374394417));
#41865=CARTESIAN_POINT('Ctrl Pts',(53.2731410264969,-85.425,10.3045704364777));
#41866=CARTESIAN_POINT('Ctrl Pts',(52.8510745763779,-85.425,9.54638504981995));
#41867=CARTESIAN_POINT('Origin',(53.7028821706772,-85.725,11.1916782855988));
#41868=CARTESIAN_POINT('',(53.7028821706772,-85.425,11.1916782855988));
#41869=CARTESIAN_POINT('',(53.7028821706772,-85.725,11.1916782855988));
#41870=CARTESIAN_POINT('',(53.7028821706772,-85.425,11.1916782855988));
#41871=CARTESIAN_POINT('Origin',(50.7898535728455,-85.725,11.1916782855988));
#41872=CARTESIAN_POINT('',(50.7898535728455,-85.425,11.1916782855988));
#41873=CARTESIAN_POINT('',(50.7898535728455,-85.725,11.1916782855988));
#41874=CARTESIAN_POINT('',(50.7898535728455,-85.425,11.1916782855988));
#41875=CARTESIAN_POINT('Origin',(50.7898535728455,-85.725,10.6606414318085));
#41876=CARTESIAN_POINT('',(50.7898535728455,-85.425,10.6606414318085));
#41877=CARTESIAN_POINT('',(50.7898535728455,-85.725,10.6606414318085));
#41878=CARTESIAN_POINT('',(50.7898535728455,-85.425,10.6606414318085));
#41879=CARTESIAN_POINT('Origin',(52.9938098192215,-85.725,10.6606414318085));
#41880=CARTESIAN_POINT('',(52.9938098192215,-85.425,10.6606414318085));
#41881=CARTESIAN_POINT('',(52.9938098192215,-85.725,10.6606414318085));
#41882=CARTESIAN_POINT('',(52.9938098192215,-85.425,10.6606414318085));
#41883=CARTESIAN_POINT('Ctrl Pts',(52.200324177742,-85.725,9.48345863819122));
#41884=CARTESIAN_POINT('Ctrl Pts',(52.200324177742,-85.425,9.48345863819122));
#41885=CARTESIAN_POINT('Ctrl Pts',(52.573277592659,-85.725,10.1817872524261));
#41886=CARTESIAN_POINT('Ctrl Pts',(52.573277592659,-85.425,10.1817872524261));
#41887=CARTESIAN_POINT('Ctrl Pts',(52.9938098192215,-85.725,10.6606414318085));
#41888=CARTESIAN_POINT('Ctrl Pts',(52.9938098192215,-85.425,10.6606414318085));
#41889=CARTESIAN_POINT('Ctrl Pts',(52.200324177742,-85.425,9.48345863819122));
#41890=CARTESIAN_POINT('Ctrl Pts',(52.573277592659,-85.425,10.1817872524261));
#41891=CARTESIAN_POINT('Ctrl Pts',(52.9938098192215,-85.425,10.6606414318085));
#41892=CARTESIAN_POINT('Origin',(52.2463678717613,-85.425,8.97083932161331));
#41893=CARTESIAN_POINT('Ctrl Pts',(57.9358288049698,-85.725,6.6732611656189));
#41894=CARTESIAN_POINT('Ctrl Pts',(57.9358288049698,-85.425,6.6732611656189));
#41895=CARTESIAN_POINT('Ctrl Pts',(57.3249825239182,-85.725,6.6732611656189));
#41896=CARTESIAN_POINT('Ctrl Pts',(57.3249825239182,-85.425,6.6732611656189));
#41897=CARTESIAN_POINT('Ctrl Pts',(56.9121249914169,-85.725,6.8512966632843));
#41898=CARTESIAN_POINT('Ctrl Pts',(56.9121249914169,-85.425,6.8512966632843));
#41899=CARTESIAN_POINT('',(57.9358288049698,-85.425,6.6732611656189));
#41900=CARTESIAN_POINT('',(57.9358288049698,-85.725,6.6732611656189));
#41901=CARTESIAN_POINT('',(56.9121249914169,-85.425,6.8512966632843));
#41902=CARTESIAN_POINT('Ctrl Pts',(57.9358288049698,-85.425,6.6732611656189));
#41903=CARTESIAN_POINT('Ctrl Pts',(57.3249825239182,-85.425,6.6732611656189));
#41904=CARTESIAN_POINT('Ctrl Pts',(56.9121249914169,-85.425,6.8512966632843));
#41905=CARTESIAN_POINT('',(56.9121249914169,-85.725,6.8512966632843));
#41906=CARTESIAN_POINT('Ctrl Pts',(58.8029834032059,-85.725,6.84976184368133));
#41907=CARTESIAN_POINT('Ctrl Pts',(58.8029834032059,-85.425,6.84976184368133));
#41908=CARTESIAN_POINT('Ctrl Pts',(58.417752623558,-85.725,6.6732611656189));
#41909=CARTESIAN_POINT('Ctrl Pts',(58.417752623558,-85.425,6.6732611656189));
#41910=CARTESIAN_POINT('Ctrl Pts',(57.9358288049698,-85.725,6.6732611656189));
#41911=CARTESIAN_POINT('Ctrl Pts',(57.9358288049698,-85.425,6.6732611656189));
#41912=CARTESIAN_POINT('',(58.8029834032059,-85.425,6.84976184368133));
#41913=CARTESIAN_POINT('',(58.8029834032059,-85.725,6.84976184368133));
#41914=CARTESIAN_POINT('Ctrl Pts',(58.8029834032059,-85.425,6.84976184368133));
#41915=CARTESIAN_POINT('Ctrl Pts',(58.417752623558,-85.425,6.6732611656189));
#41916=CARTESIAN_POINT('Ctrl Pts',(57.9358288049698,-85.425,6.6732611656189));
#41917=CARTESIAN_POINT('Ctrl Pts',(59.3938776254654,-85.725,7.34396362304687));
#41918=CARTESIAN_POINT('Ctrl Pts',(59.3938776254654,-85.425,7.34396362304687));
#41919=CARTESIAN_POINT('Ctrl Pts',(59.1882153749466,-85.725,7.02626252174377));
#41920=CARTESIAN_POINT('Ctrl Pts',(59.1882153749466,-85.425,7.02626252174377));
#41921=CARTESIAN_POINT('Ctrl Pts',(58.8029834032059,-85.725,6.84976184368133));
#41922=CARTESIAN_POINT('Ctrl Pts',(58.8029834032059,-85.425,6.84976184368133));
#41923=CARTESIAN_POINT('',(59.3938776254654,-85.425,7.34396362304687));
#41924=CARTESIAN_POINT('',(59.3938776254654,-85.725,7.34396362304687));
#41925=CARTESIAN_POINT('Ctrl Pts',(59.3938776254654,-85.425,7.34396362304687));
#41926=CARTESIAN_POINT('Ctrl Pts',(59.1882153749466,-85.425,7.02626252174377));
#41927=CARTESIAN_POINT('Ctrl Pts',(58.8029834032059,-85.425,6.84976184368133));
#41928=CARTESIAN_POINT('Ctrl Pts',(59.5995398759842,-85.725,8.02080535888672));
#41929=CARTESIAN_POINT('Ctrl Pts',(59.5995398759842,-85.425,8.02080535888672));
#41930=CARTESIAN_POINT('Ctrl Pts',(59.5995398759842,-85.725,7.66166472434997));
#41931=CARTESIAN_POINT('Ctrl Pts',(59.5995398759842,-85.425,7.66166472434997));
#41932=CARTESIAN_POINT('Ctrl Pts',(59.3938776254654,-85.725,7.34396362304687));
#41933=CARTESIAN_POINT('Ctrl Pts',(59.3938776254654,-85.425,7.34396362304687));
#41934=CARTESIAN_POINT('',(59.5995398759842,-85.425,8.02080535888672));
#41935=CARTESIAN_POINT('',(59.5995398759842,-85.725,8.02080535888672));
#41936=CARTESIAN_POINT('Ctrl Pts',(59.5995398759842,-85.425,8.02080535888672));
#41937=CARTESIAN_POINT('Ctrl Pts',(59.5995398759842,-85.425,7.66166472434997));
#41938=CARTESIAN_POINT('Ctrl Pts',(59.3938776254654,-85.425,7.34396362304687));
#41939=CARTESIAN_POINT('Ctrl Pts',(59.412295460701,-85.725,8.66081202030182));
#41940=CARTESIAN_POINT('Ctrl Pts',(59.412295460701,-85.425,8.66081202030182));
#41941=CARTESIAN_POINT('Ctrl Pts',(59.5995398759842,-85.725,8.38301503658295));
#41942=CARTESIAN_POINT('Ctrl Pts',(59.5995398759842,-85.425,8.38301503658295));
#41943=CARTESIAN_POINT('Ctrl Pts',(59.5995398759842,-85.725,8.02080535888672));
#41944=CARTESIAN_POINT('Ctrl Pts',(59.5995398759842,-85.425,8.02080535888672));
#41945=CARTESIAN_POINT('',(59.412295460701,-85.425,8.66081202030182));
#41946=CARTESIAN_POINT('',(59.412295460701,-85.725,8.66081202030182));
#41947=CARTESIAN_POINT('Ctrl Pts',(59.412295460701,-85.425,8.66081202030182));
#41948=CARTESIAN_POINT('Ctrl Pts',(59.5995398759842,-85.425,8.38301503658295));
#41949=CARTESIAN_POINT('Ctrl Pts',(59.5995398759842,-85.425,8.02080535888672));
#41950=CARTESIAN_POINT('Ctrl Pts',(58.8321443796158,-85.725,9.11971354484558));
#41951=CARTESIAN_POINT('Ctrl Pts',(58.8321443796158,-85.425,9.11971354484558));
#41952=CARTESIAN_POINT('Ctrl Pts',(59.2250510454178,-85.725,8.93860900402069));
#41953=CARTESIAN_POINT('Ctrl Pts',(59.2250510454178,-85.425,8.93860900402069));
#41954=CARTESIAN_POINT('Ctrl Pts',(59.412295460701,-85.725,8.66081202030182));
#41955=CARTESIAN_POINT('Ctrl Pts',(59.412295460701,-85.425,8.66081202030182));
#41956=CARTESIAN_POINT('',(58.8321443796158,-85.425,9.11971354484558));
#41957=CARTESIAN_POINT('',(58.8321443796158,-85.725,9.11971354484558));
#41958=CARTESIAN_POINT('Ctrl Pts',(58.8321443796158,-85.425,9.11971354484558));
#41959=CARTESIAN_POINT('Ctrl Pts',(59.2250510454178,-85.425,8.93860900402069));
#41960=CARTESIAN_POINT('Ctrl Pts',(59.412295460701,-85.425,8.66081202030182));
#41961=CARTESIAN_POINT('Ctrl Pts',(57.8360673189163,-85.725,9.4067188501358));
#41962=CARTESIAN_POINT('Ctrl Pts',(57.8360673189163,-85.425,9.4067188501358));
#41963=CARTESIAN_POINT('Ctrl Pts',(58.5620220899582,-85.725,9.24249672889709));
#41964=CARTESIAN_POINT('Ctrl Pts',(58.5620220899582,-85.425,9.24249672889709));
#41965=CARTESIAN_POINT('Ctrl Pts',(58.8321443796158,-85.725,9.11971354484558));
#41966=CARTESIAN_POINT('Ctrl Pts',(58.8321443796158,-85.425,9.11971354484558));
#41967=CARTESIAN_POINT('',(57.8360673189163,-85.425,9.4067188501358));
#41968=CARTESIAN_POINT('',(57.8360673189163,-85.725,9.4067188501358));
#41969=CARTESIAN_POINT('Ctrl Pts',(57.8360673189163,-85.425,9.4067188501358));
#41970=CARTESIAN_POINT('Ctrl Pts',(58.5620220899582,-85.425,9.24249672889709));
#41971=CARTESIAN_POINT('Ctrl Pts',(58.8321443796158,-85.425,9.11971354484558));
#41972=CARTESIAN_POINT('Ctrl Pts',(56.9382163286209,-85.725,9.72748959064484));
#41973=CARTESIAN_POINT('Ctrl Pts',(56.9382163286209,-85.425,9.72748959064484));
#41974=CARTESIAN_POINT('Ctrl Pts',(57.1101125478745,-85.725,9.57094156742096));
#41975=CARTESIAN_POINT('Ctrl Pts',(57.1101125478745,-85.425,9.57094156742096));
#41976=CARTESIAN_POINT('Ctrl Pts',(57.8360673189163,-85.725,9.4067188501358));
#41977=CARTESIAN_POINT('Ctrl Pts',(57.8360673189163,-85.425,9.4067188501358));
#41978=CARTESIAN_POINT('',(56.9382163286209,-85.425,9.72748959064484));
#41979=CARTESIAN_POINT('',(56.9382163286209,-85.725,9.72748959064484));
#41980=CARTESIAN_POINT('Ctrl Pts',(56.9382163286209,-85.425,9.72748959064484));
#41981=CARTESIAN_POINT('Ctrl Pts',(57.1101125478745,-85.425,9.57094156742096));
#41982=CARTESIAN_POINT('Ctrl Pts',(57.8360673189163,-85.425,9.4067188501358));
#41983=CARTESIAN_POINT('Ctrl Pts',(56.7632504701614,-85.725,10.1265349388123));
#41984=CARTESIAN_POINT('Ctrl Pts',(56.7632504701614,-85.425,10.1265349388123));
#41985=CARTESIAN_POINT('Ctrl Pts',(56.7632504701614,-85.725,9.88403820991516));
#41986=CARTESIAN_POINT('Ctrl Pts',(56.7632504701614,-85.425,9.88403820991516));
#41987=CARTESIAN_POINT('Ctrl Pts',(56.9382163286209,-85.725,9.72748959064484));
#41988=CARTESIAN_POINT('Ctrl Pts',(56.9382163286209,-85.425,9.72748959064484));
#41989=CARTESIAN_POINT('',(56.7632504701614,-85.425,10.1265349388123));
#41990=CARTESIAN_POINT('',(56.7632504701614,-85.725,10.1265349388123));
#41991=CARTESIAN_POINT('Ctrl Pts',(56.7632504701614,-85.425,10.1265349388123));
#41992=CARTESIAN_POINT('Ctrl Pts',(56.7632504701614,-85.425,9.88403820991516));
#41993=CARTESIAN_POINT('Ctrl Pts',(56.9382163286209,-85.425,9.72748959064484));
#41994=CARTESIAN_POINT('Ctrl Pts',(57.010351061821,-85.725,10.6038540005684));
#41995=CARTESIAN_POINT('Ctrl Pts',(57.010351061821,-85.425,10.6038540005684));
#41996=CARTESIAN_POINT('Ctrl Pts',(56.7632504701614,-85.725,10.4058664441109));
#41997=CARTESIAN_POINT('Ctrl Pts',(56.7632504701614,-85.425,10.4058664441109));
#41998=CARTESIAN_POINT('Ctrl Pts',(56.7632504701614,-85.725,10.1265349388123));
#41999=CARTESIAN_POINT('Ctrl Pts',(56.7632504701614,-85.425,10.1265349388123));
#42000=CARTESIAN_POINT('',(57.010351061821,-85.425,10.6038540005684));
#42001=CARTESIAN_POINT('',(57.010351061821,-85.725,10.6038540005684));
#42002=CARTESIAN_POINT('Ctrl Pts',(57.010351061821,-85.425,10.6038540005684));
#42003=CARTESIAN_POINT('Ctrl Pts',(56.7632504701614,-85.425,10.4058664441109));
#42004=CARTESIAN_POINT('Ctrl Pts',(56.7632504701614,-85.425,10.1265349388123));
#42005=CARTESIAN_POINT('Ctrl Pts',(57.7976974248886,-85.725,10.8018418550491));
#42006=CARTESIAN_POINT('Ctrl Pts',(57.7976974248886,-85.425,10.8018418550491));
#42007=CARTESIAN_POINT('Ctrl Pts',(57.2574516534805,-85.725,10.8018418550491));
#42008=CARTESIAN_POINT('Ctrl Pts',(57.2574516534805,-85.425,10.8018418550491));
#42009=CARTESIAN_POINT('Ctrl Pts',(57.010351061821,-85.725,10.6038540005684));
#42010=CARTESIAN_POINT('Ctrl Pts',(57.010351061821,-85.425,10.6038540005684));
#42011=CARTESIAN_POINT('',(57.7976974248886,-85.425,10.8018418550491));
#42012=CARTESIAN_POINT('',(57.7976974248886,-85.725,10.8018418550491));
#42013=CARTESIAN_POINT('Ctrl Pts',(57.7976974248886,-85.425,10.8018418550491));
#42014=CARTESIAN_POINT('Ctrl Pts',(57.2574516534805,-85.425,10.8018418550491));
#42015=CARTESIAN_POINT('Ctrl Pts',(57.010351061821,-85.425,10.6038540005684));
#42016=CARTESIAN_POINT('Ctrl Pts',(58.5819741487503,-85.725,10.5839019417763));
#42017=CARTESIAN_POINT('Ctrl Pts',(58.5819741487503,-85.425,10.5839019417763));
#42018=CARTESIAN_POINT('Ctrl Pts',(58.3164557218552,-85.725,10.8018418550491));
#42019=CARTESIAN_POINT('Ctrl Pts',(58.3164557218552,-85.425,10.8018418550491));
#42020=CARTESIAN_POINT('Ctrl Pts',(57.7976974248886,-85.725,10.8018418550491));
#42021=CARTESIAN_POINT('Ctrl Pts',(57.7976974248886,-85.425,10.8018418550491));
#42022=CARTESIAN_POINT('',(58.5819741487503,-85.425,10.5839019417763));
#42023=CARTESIAN_POINT('',(58.5819741487503,-85.725,10.5839019417763));
#42024=CARTESIAN_POINT('Ctrl Pts',(58.5819741487503,-85.425,10.5839019417763));
#42025=CARTESIAN_POINT('Ctrl Pts',(58.3164557218552,-85.425,10.8018418550491));
#42026=CARTESIAN_POINT('Ctrl Pts',(57.7976974248886,-85.425,10.8018418550491));
#42027=CARTESIAN_POINT('Ctrl Pts',(58.8935371637344,-85.725,9.9392911195755));
#42028=CARTESIAN_POINT('Ctrl Pts',(58.8935371637344,-85.425,9.9392911195755));
#42029=CARTESIAN_POINT('Ctrl Pts',(58.8474925756454,-85.725,10.3659620285034));
#42030=CARTESIAN_POINT('Ctrl Pts',(58.8474925756454,-85.425,10.3659620285034));
#42031=CARTESIAN_POINT('Ctrl Pts',(58.5819741487503,-85.725,10.5839019417763));
#42032=CARTESIAN_POINT('Ctrl Pts',(58.5819741487503,-85.425,10.5839019417763));
#42033=CARTESIAN_POINT('',(58.8935371637344,-85.425,9.9392911195755));
#42034=CARTESIAN_POINT('',(58.8935371637344,-85.725,9.9392911195755));
#42035=CARTESIAN_POINT('Ctrl Pts',(58.8935371637344,-85.425,9.9392911195755));
#42036=CARTESIAN_POINT('Ctrl Pts',(58.8474925756454,-85.425,10.3659620285034));
#42037=CARTESIAN_POINT('Ctrl Pts',(58.5819741487503,-85.425,10.5839019417763));
#42038=CARTESIAN_POINT('Origin',(59.4644781351089,-85.725,9.98226487636566));
#42039=CARTESIAN_POINT('',(59.4644781351089,-85.425,9.98226487636566));
#42040=CARTESIAN_POINT('',(59.4644781351089,-85.725,9.98226487636566));
#42041=CARTESIAN_POINT('',(59.4644781351089,-85.425,9.98226487636566));
#42042=CARTESIAN_POINT('Ctrl Pts',(59.2434688806534,-85.725,10.6913369297981));
#42043=CARTESIAN_POINT('Ctrl Pts',(59.2434688806534,-85.425,10.6913369297981));
#42044=CARTESIAN_POINT('Ctrl Pts',(59.4491299390793,-85.725,10.3782402873039));
#42045=CARTESIAN_POINT('Ctrl Pts',(59.4491299390793,-85.425,10.3782402873039));
#42046=CARTESIAN_POINT('Ctrl Pts',(59.4644781351089,-85.725,9.98226487636566));
#42047=CARTESIAN_POINT('Ctrl Pts',(59.4644781351089,-85.425,9.98226487636566));
#42048=CARTESIAN_POINT('',(59.2434688806534,-85.425,10.6913369297981));
#42049=CARTESIAN_POINT('',(59.2434688806534,-85.725,10.6913369297981));
#42050=CARTESIAN_POINT('Ctrl Pts',(59.2434688806534,-85.425,10.6913369297981));
#42051=CARTESIAN_POINT('Ctrl Pts',(59.4491299390793,-85.425,10.3782402873039));
#42052=CARTESIAN_POINT('Ctrl Pts',(59.4644781351089,-85.425,9.98226487636566));
#42053=CARTESIAN_POINT('Ctrl Pts',(58.6556442975998,-85.725,11.1655866503716));
#42054=CARTESIAN_POINT('Ctrl Pts',(58.6556442975998,-85.425,11.1655866503716));
#42055=CARTESIAN_POINT('Ctrl Pts',(59.0378066301346,-85.725,11.0044338703156));
#42056=CARTESIAN_POINT('Ctrl Pts',(59.0378066301346,-85.425,11.0044338703156));
#42057=CARTESIAN_POINT('Ctrl Pts',(59.2434688806534,-85.725,10.6913369297981));
#42058=CARTESIAN_POINT('Ctrl Pts',(59.2434688806534,-85.425,10.6913369297981));
#42059=CARTESIAN_POINT('',(58.6556442975998,-85.425,11.1655866503716));
#42060=CARTESIAN_POINT('',(58.6556442975998,-85.725,11.1655866503716));
#42061=CARTESIAN_POINT('Ctrl Pts',(58.6556442975998,-85.425,11.1655866503716));
#42062=CARTESIAN_POINT('Ctrl Pts',(59.0378066301346,-85.425,11.0044338703156));
#42063=CARTESIAN_POINT('Ctrl Pts',(59.2434688806534,-85.425,10.6913369297981));
#42064=CARTESIAN_POINT('Ctrl Pts',(57.773141503334,-85.725,11.3267394304276));
#42065=CARTESIAN_POINT('Ctrl Pts',(57.773141503334,-85.425,11.3267394304276));
#42066=CARTESIAN_POINT('Ctrl Pts',(58.273481965065,-85.725,11.3267394304276));
#42067=CARTESIAN_POINT('Ctrl Pts',(58.273481965065,-85.425,11.3267394304276));
#42068=CARTESIAN_POINT('Ctrl Pts',(58.6556442975998,-85.725,11.1655866503716));
#42069=CARTESIAN_POINT('Ctrl Pts',(58.6556442975998,-85.425,11.1655866503716));
#42070=CARTESIAN_POINT('',(57.773141503334,-85.425,11.3267394304276));
#42071=CARTESIAN_POINT('',(57.773141503334,-85.725,11.3267394304276));
#42072=CARTESIAN_POINT('Ctrl Pts',(57.773141503334,-85.425,11.3267394304276));
#42073=CARTESIAN_POINT('Ctrl Pts',(58.273481965065,-85.425,11.3267394304276));
#42074=CARTESIAN_POINT('Ctrl Pts',(58.6556442975998,-85.425,11.1655866503716));
#42075=CARTESIAN_POINT('Ctrl Pts',(56.9474240541458,-85.725,11.1732607483864));
#42076=CARTESIAN_POINT('Ctrl Pts',(56.9474240541458,-85.425,11.1732607483864));
#42077=CARTESIAN_POINT('Ctrl Pts',(57.3188432455063,-85.725,11.3267394304276));
#42078=CARTESIAN_POINT('Ctrl Pts',(57.3188432455063,-85.425,11.3267394304276));
#42079=CARTESIAN_POINT('Ctrl Pts',(57.773141503334,-85.725,11.3267394304276));
#42080=CARTESIAN_POINT('Ctrl Pts',(57.773141503334,-85.425,11.3267394304276));
#42081=CARTESIAN_POINT('',(56.9474240541458,-85.425,11.1732607483864));
#42082=CARTESIAN_POINT('',(56.9474240541458,-85.725,11.1732607483864));
#42083=CARTESIAN_POINT('Ctrl Pts',(56.9474240541458,-85.425,11.1732607483864));
#42084=CARTESIAN_POINT('Ctrl Pts',(57.3188432455063,-85.425,11.3267394304276));
#42085=CARTESIAN_POINT('Ctrl Pts',(57.773141503334,-85.425,11.3267394304276));
#42086=CARTESIAN_POINT('Ctrl Pts',(56.3826223611832,-85.725,10.723567545414));
#42087=CARTESIAN_POINT('Ctrl Pts',(56.3826223611832,-85.425,10.723567545414));
#42088=CARTESIAN_POINT('Ctrl Pts',(56.5760060548782,-85.725,11.019781768322));
#42089=CARTESIAN_POINT('Ctrl Pts',(56.5760060548782,-85.425,11.019781768322));
#42090=CARTESIAN_POINT('Ctrl Pts',(56.9474240541458,-85.725,11.1732607483864));
#42091=CARTESIAN_POINT('Ctrl Pts',(56.9474240541458,-85.425,11.1732607483864));
#42092=CARTESIAN_POINT('',(56.3826223611832,-85.425,10.723567545414));
#42093=CARTESIAN_POINT('',(56.3826223611832,-85.725,10.723567545414));
#42094=CARTESIAN_POINT('Ctrl Pts',(56.3826223611832,-85.425,10.723567545414));
#42095=CARTESIAN_POINT('Ctrl Pts',(56.5760060548782,-85.425,11.019781768322));
#42096=CARTESIAN_POINT('Ctrl Pts',(56.9474240541458,-85.425,11.1732607483864));
#42097=CARTESIAN_POINT('Ctrl Pts',(56.1892386674881,-85.725,10.0866302251816));
#42098=CARTESIAN_POINT('Ctrl Pts',(56.1892386674881,-85.425,10.0866302251816));
#42099=CARTESIAN_POINT('Ctrl Pts',(56.1892386674881,-85.725,10.427353322506));
#42100=CARTESIAN_POINT('Ctrl Pts',(56.1892386674881,-85.425,10.427353322506));
#42101=CARTESIAN_POINT('Ctrl Pts',(56.3826223611832,-85.725,10.723567545414));
#42102=CARTESIAN_POINT('Ctrl Pts',(56.3826223611832,-85.425,10.723567545414));
#42103=CARTESIAN_POINT('',(56.1892386674881,-85.425,10.0866302251816));
#42104=CARTESIAN_POINT('',(56.1892386674881,-85.725,10.0866302251816));
#42105=CARTESIAN_POINT('Ctrl Pts',(56.1892386674881,-85.425,10.0866302251816));
#42106=CARTESIAN_POINT('Ctrl Pts',(56.1892386674881,-85.425,10.427353322506));
#42107=CARTESIAN_POINT('Ctrl Pts',(56.3826223611832,-85.425,10.723567545414));
#42108=CARTESIAN_POINT('Ctrl Pts',(56.3473221063614,-85.725,9.52643239498138));
#42109=CARTESIAN_POINT('Ctrl Pts',(56.3473221063614,-85.425,9.52643239498138));
#42110=CARTESIAN_POINT('Ctrl Pts',(56.1892386674881,-85.725,9.77660322189331));
#42111=CARTESIAN_POINT('Ctrl Pts',(56.1892386674881,-85.425,9.77660322189331));
#42112=CARTESIAN_POINT('Ctrl Pts',(56.1892386674881,-85.725,10.0866302251816));
#42113=CARTESIAN_POINT('Ctrl Pts',(56.1892386674881,-85.425,10.0866302251816));
#42114=CARTESIAN_POINT('',(56.3473221063614,-85.425,9.52643239498138));
#42115=CARTESIAN_POINT('',(56.3473221063614,-85.725,9.52643239498138));
#42116=CARTESIAN_POINT('Ctrl Pts',(56.3473221063614,-85.425,9.52643239498138));
#42117=CARTESIAN_POINT('Ctrl Pts',(56.1892386674881,-85.425,9.77660322189331));
#42118=CARTESIAN_POINT('Ctrl Pts',(56.1892386674881,-85.425,10.0866302251816));
#42119=CARTESIAN_POINT('Ctrl Pts',(56.8277117013931,-85.725,9.1074355840683));
#42120=CARTESIAN_POINT('Ctrl Pts',(56.8277117013931,-85.425,9.1074355840683));
#42121=CARTESIAN_POINT('Ctrl Pts',(56.5054055452347,-85.725,9.27626216411591));
#42122=CARTESIAN_POINT('Ctrl Pts',(56.5054055452347,-85.425,9.27626216411591));
#42123=CARTESIAN_POINT('Ctrl Pts',(56.3473221063614,-85.725,9.52643239498138));
#42124=CARTESIAN_POINT('Ctrl Pts',(56.3473221063614,-85.425,9.52643239498138));
#42125=CARTESIAN_POINT('',(56.8277117013931,-85.425,9.1074355840683));
#42126=CARTESIAN_POINT('',(56.8277117013931,-85.725,9.1074355840683));
#42127=CARTESIAN_POINT('Ctrl Pts',(56.8277117013931,-85.425,9.1074355840683));
#42128=CARTESIAN_POINT('Ctrl Pts',(56.5054055452347,-85.425,9.27626216411591));
#42129=CARTESIAN_POINT('Ctrl Pts',(56.3473221063614,-85.425,9.52643239498138));
#42130=CARTESIAN_POINT('Ctrl Pts',(57.6964017152786,-85.725,8.82656896114349));
#42131=CARTESIAN_POINT('Ctrl Pts',(57.6964017152786,-85.425,8.82656896114349));
#42132=CARTESIAN_POINT('Ctrl Pts',(57.0763465166092,-85.725,8.97544348239899));
#42133=CARTESIAN_POINT('Ctrl Pts',(57.0763465166092,-85.425,8.97544348239899));
#42134=CARTESIAN_POINT('Ctrl Pts',(56.8277117013931,-85.725,9.1074355840683));
#42135=CARTESIAN_POINT('Ctrl Pts',(56.8277117013931,-85.425,9.1074355840683));
#42136=CARTESIAN_POINT('',(57.6964017152786,-85.425,8.82656896114349));
#42137=CARTESIAN_POINT('',(57.6964017152786,-85.725,8.82656896114349));
#42138=CARTESIAN_POINT('Ctrl Pts',(57.6964017152786,-85.425,8.82656896114349));
#42139=CARTESIAN_POINT('Ctrl Pts',(57.0763465166092,-85.425,8.97544348239899));
#42140=CARTESIAN_POINT('Ctrl Pts',(56.8277117013931,-85.425,9.1074355840683));
#42141=CARTESIAN_POINT('Ctrl Pts',(58.4975608587265,-85.725,8.60709452629089));
#42142=CARTESIAN_POINT('Ctrl Pts',(58.4975608587265,-85.425,8.60709452629089));
#42143=CARTESIAN_POINT('Ctrl Pts',(58.3164557218552,-85.725,8.677694439888));
#42144=CARTESIAN_POINT('Ctrl Pts',(58.3164557218552,-85.425,8.677694439888));
#42145=CARTESIAN_POINT('Ctrl Pts',(57.6964017152786,-85.725,8.82656896114349));
#42146=CARTESIAN_POINT('Ctrl Pts',(57.6964017152786,-85.425,8.82656896114349));
#42147=CARTESIAN_POINT('',(58.4975608587265,-85.425,8.60709452629089));
#42148=CARTESIAN_POINT('',(58.4975608587265,-85.725,8.60709452629089));
#42149=CARTESIAN_POINT('Ctrl Pts',(58.4975608587265,-85.425,8.60709452629089));
#42150=CARTESIAN_POINT('Ctrl Pts',(58.3164557218552,-85.425,8.677694439888));
#42151=CARTESIAN_POINT('Ctrl Pts',(57.6964017152786,-85.425,8.82656896114349));
#42152=CARTESIAN_POINT('Ctrl Pts',(58.9027448892593,-85.725,8.34157609939575));
#42153=CARTESIAN_POINT('Ctrl Pts',(58.9027448892593,-85.425,8.34157609939575));
#42154=CARTESIAN_POINT('Ctrl Pts',(58.7799617052078,-85.725,8.4996589422226));
#42155=CARTESIAN_POINT('Ctrl Pts',(58.7799617052078,-85.425,8.4996589422226));
#42156=CARTESIAN_POINT('Ctrl Pts',(58.4975608587265,-85.725,8.60709452629089));
#42157=CARTESIAN_POINT('Ctrl Pts',(58.4975608587265,-85.425,8.60709452629089));
#42158=CARTESIAN_POINT('',(58.9027448892593,-85.425,8.34157609939575));
#42159=CARTESIAN_POINT('',(58.9027448892593,-85.725,8.34157609939575));
#42160=CARTESIAN_POINT('Ctrl Pts',(58.9027448892593,-85.425,8.34157609939575));
#42161=CARTESIAN_POINT('Ctrl Pts',(58.7799617052078,-85.425,8.4996589422226));
#42162=CARTESIAN_POINT('Ctrl Pts',(58.4975608587265,-85.425,8.60709452629089));
#42163=CARTESIAN_POINT('Ctrl Pts',(59.0255280733109,-85.725,7.97169172763824));
#42164=CARTESIAN_POINT('Ctrl Pts',(59.0255280733109,-85.425,7.97169172763824));
#42165=CARTESIAN_POINT('Ctrl Pts',(59.0255280733109,-85.725,8.18349266052246));
#42166=CARTESIAN_POINT('Ctrl Pts',(59.0255280733109,-85.425,8.18349266052246));
#42167=CARTESIAN_POINT('Ctrl Pts',(58.9027448892593,-85.725,8.34157609939575));
#42168=CARTESIAN_POINT('Ctrl Pts',(58.9027448892593,-85.425,8.34157609939575));
#42169=CARTESIAN_POINT('',(59.0255280733109,-85.425,7.97169172763824));
#42170=CARTESIAN_POINT('',(59.0255280733109,-85.725,7.97169172763824));
#42171=CARTESIAN_POINT('Ctrl Pts',(59.0255280733109,-85.425,7.97169172763824));
#42172=CARTESIAN_POINT('Ctrl Pts',(59.0255280733109,-85.425,8.18349266052246));
#42173=CARTESIAN_POINT('Ctrl Pts',(58.9027448892593,-85.425,8.34157609939575));
#42174=CARTESIAN_POINT('Ctrl Pts',(58.8981410264969,-85.725,7.58645975589752));
#42175=CARTESIAN_POINT('Ctrl Pts',(58.8981410264969,-85.425,7.58645975589752));
#42176=CARTESIAN_POINT('Ctrl Pts',(59.0255280733109,-85.725,7.76296103000641));
#42177=CARTESIAN_POINT('Ctrl Pts',(59.0255280733109,-85.425,7.76296103000641));
#42178=CARTESIAN_POINT('Ctrl Pts',(59.0255280733109,-85.725,7.97169172763824));
#42179=CARTESIAN_POINT('Ctrl Pts',(59.0255280733109,-85.425,7.97169172763824));
#42180=CARTESIAN_POINT('',(58.8981410264969,-85.425,7.58645975589752));
#42181=CARTESIAN_POINT('',(58.8981410264969,-85.725,7.58645975589752));
#42182=CARTESIAN_POINT('Ctrl Pts',(58.8981410264969,-85.425,7.58645975589752));
#42183=CARTESIAN_POINT('Ctrl Pts',(59.0255280733109,-85.425,7.76296103000641));
#42184=CARTESIAN_POINT('Ctrl Pts',(59.0255280733109,-85.425,7.97169172763824));
#42185=CARTESIAN_POINT('Ctrl Pts',(58.5098394155502,-85.725,7.3086633682251));
#42186=CARTESIAN_POINT('Ctrl Pts',(58.5098394155502,-85.425,7.3086633682251));
#42187=CARTESIAN_POINT('Ctrl Pts',(58.7707539796829,-85.725,7.40995967388153));
#42188=CARTESIAN_POINT('Ctrl Pts',(58.7707539796829,-85.425,7.40995967388153));
#42189=CARTESIAN_POINT('Ctrl Pts',(58.8981410264969,-85.725,7.58645975589752));
#42190=CARTESIAN_POINT('Ctrl Pts',(58.8981410264969,-85.425,7.58645975589752));
#42191=CARTESIAN_POINT('',(58.5098394155502,-85.425,7.3086633682251));
#42192=CARTESIAN_POINT('',(58.5098394155502,-85.725,7.3086633682251));
#42193=CARTESIAN_POINT('Ctrl Pts',(58.5098394155502,-85.425,7.3086633682251));
#42194=CARTESIAN_POINT('Ctrl Pts',(58.7707539796829,-85.425,7.40995967388153));
#42195=CARTESIAN_POINT('Ctrl Pts',(58.8981410264969,-85.425,7.58645975589752));
#42196=CARTESIAN_POINT('Ctrl Pts',(57.9082020521164,-85.725,7.20736706256866));
#42197=CARTESIAN_POINT('Ctrl Pts',(57.9082020521164,-85.425,7.20736706256866));
#42198=CARTESIAN_POINT('Ctrl Pts',(58.2489248514175,-85.725,7.20736706256866));
#42199=CARTESIAN_POINT('Ctrl Pts',(58.2489248514175,-85.425,7.20736706256866));
#42200=CARTESIAN_POINT('Ctrl Pts',(58.5098394155502,-85.725,7.3086633682251));
#42201=CARTESIAN_POINT('Ctrl Pts',(58.5098394155502,-85.425,7.3086633682251));
#42202=CARTESIAN_POINT('',(57.9082020521164,-85.425,7.20736706256866));
#42203=CARTESIAN_POINT('',(57.9082020521164,-85.725,7.20736706256866));
#42204=CARTESIAN_POINT('Ctrl Pts',(57.9082020521164,-85.425,7.20736706256866));
#42205=CARTESIAN_POINT('Ctrl Pts',(58.2489248514175,-85.425,7.20736706256866));
#42206=CARTESIAN_POINT('Ctrl Pts',(58.5098394155502,-85.425,7.3086633682251));
#42207=CARTESIAN_POINT('Ctrl Pts',(57.2175475358963,-85.725,7.34089398384094));
#42208=CARTESIAN_POINT('Ctrl Pts',(57.2175475358963,-85.425,7.34089398384094));
#42209=CARTESIAN_POINT('Ctrl Pts',(57.5245054960251,-85.725,7.20736706256866));
#42210=CARTESIAN_POINT('Ctrl Pts',(57.5245054960251,-85.425,7.20736706256866));
#42211=CARTESIAN_POINT('Ctrl Pts',(57.9082020521164,-85.725,7.20736706256866));
#42212=CARTESIAN_POINT('Ctrl Pts',(57.9082020521164,-85.425,7.20736706256866));
#42213=CARTESIAN_POINT('',(57.2175475358963,-85.425,7.34089398384094));
#42214=CARTESIAN_POINT('',(57.2175475358963,-85.725,7.34089398384094));
#42215=CARTESIAN_POINT('Ctrl Pts',(57.2175475358963,-85.425,7.34089398384094));
#42216=CARTESIAN_POINT('Ctrl Pts',(57.5245054960251,-85.425,7.20736706256866));
#42217=CARTESIAN_POINT('Ctrl Pts',(57.9082020521164,-85.425,7.20736706256866));
#42218=CARTESIAN_POINT('Ctrl Pts',(56.764784693718,-85.725,7.69082570075989));
#42219=CARTESIAN_POINT('Ctrl Pts',(56.764784693718,-85.425,7.69082570075989));
#42220=CARTESIAN_POINT('Ctrl Pts',(56.9105907678604,-85.725,7.47442030906677));
#42221=CARTESIAN_POINT('Ctrl Pts',(56.9105907678604,-85.425,7.47442030906677));
#42222=CARTESIAN_POINT('Ctrl Pts',(57.2175475358963,-85.725,7.34089398384094));
#42223=CARTESIAN_POINT('Ctrl Pts',(57.2175475358963,-85.425,7.34089398384094));
#42224=CARTESIAN_POINT('',(56.764784693718,-85.425,7.69082570075989));
#42225=CARTESIAN_POINT('',(56.764784693718,-85.725,7.69082570075989));
#42226=CARTESIAN_POINT('Ctrl Pts',(56.764784693718,-85.425,7.69082570075989));
#42227=CARTESIAN_POINT('Ctrl Pts',(56.9105907678604,-85.425,7.47442030906677));
#42228=CARTESIAN_POINT('Ctrl Pts',(57.2175475358963,-85.425,7.34089398384094));
#42229=CARTESIAN_POINT('Ctrl Pts',(56.5790756940842,-85.725,8.24488425254822));
#42230=CARTESIAN_POINT('Ctrl Pts',(56.5790756940842,-85.425,8.24488425254822));
#42231=CARTESIAN_POINT('Ctrl Pts',(56.6189798116684,-85.725,7.907231092453));
#42232=CARTESIAN_POINT('Ctrl Pts',(56.6189798116684,-85.425,7.907231092453));
#42233=CARTESIAN_POINT('Ctrl Pts',(56.764784693718,-85.725,7.69082570075989));
#42234=CARTESIAN_POINT('Ctrl Pts',(56.764784693718,-85.425,7.69082570075989));
#42235=CARTESIAN_POINT('',(56.5790756940842,-85.425,8.24488425254822));
#42236=CARTESIAN_POINT('',(56.5790756940842,-85.725,8.24488425254822));
#42237=CARTESIAN_POINT('Ctrl Pts',(56.5790756940842,-85.425,8.24488425254822));
#42238=CARTESIAN_POINT('Ctrl Pts',(56.6189798116684,-85.425,7.907231092453));
#42239=CARTESIAN_POINT('Ctrl Pts',(56.764784693718,-85.425,7.69082570075989));
#42240=CARTESIAN_POINT('Origin',(56.0173436403275,-85.725,8.19577121734619));
#42241=CARTESIAN_POINT('',(56.0173436403275,-85.425,8.19577121734619));
#42242=CARTESIAN_POINT('',(56.0173436403275,-85.725,8.19577121734619));
#42243=CARTESIAN_POINT('',(56.0173436403275,-85.425,8.19577121734619));
#42244=CARTESIAN_POINT('Ctrl Pts',(56.264444231987,-85.725,7.38693737983704));
#42245=CARTESIAN_POINT('Ctrl Pts',(56.264444231987,-85.425,7.38693737983704));
#42246=CARTESIAN_POINT('Ctrl Pts',(56.0296221971512,-85.725,7.74454319477081));
#42247=CARTESIAN_POINT('Ctrl Pts',(56.0296221971512,-85.425,7.74454319477081));
#42248=CARTESIAN_POINT('Ctrl Pts',(56.0173436403275,-85.725,8.19577121734619));
#42249=CARTESIAN_POINT('Ctrl Pts',(56.0173436403275,-85.425,8.19577121734619));
#42250=CARTESIAN_POINT('',(56.264444231987,-85.425,7.38693737983704));
#42251=CARTESIAN_POINT('',(56.264444231987,-85.725,7.38693737983704));
#42252=CARTESIAN_POINT('Ctrl Pts',(56.264444231987,-85.425,7.38693737983704));
#42253=CARTESIAN_POINT('Ctrl Pts',(56.0296221971512,-85.425,7.74454319477081));
#42254=CARTESIAN_POINT('Ctrl Pts',(56.0173436403275,-85.425,8.19577121734619));
#42255=CARTESIAN_POINT('Ctrl Pts',(56.9121249914169,-85.725,6.8512966632843));
#42256=CARTESIAN_POINT('Ctrl Pts',(56.9121249914169,-85.425,6.8512966632843));
#42257=CARTESIAN_POINT('Ctrl Pts',(56.4992662668228,-85.725,7.02933156490326));
#42258=CARTESIAN_POINT('Ctrl Pts',(56.4992662668228,-85.425,7.02933156490326));
#42259=CARTESIAN_POINT('Ctrl Pts',(56.264444231987,-85.725,7.38693737983704));
#42260=CARTESIAN_POINT('Ctrl Pts',(56.264444231987,-85.425,7.38693737983704));
#42261=CARTESIAN_POINT('Ctrl Pts',(56.9121249914169,-85.425,6.8512966632843));
#42262=CARTESIAN_POINT('Ctrl Pts',(56.4992662668228,-85.425,7.02933156490326));
#42263=CARTESIAN_POINT('Ctrl Pts',(56.264444231987,-85.425,7.38693737983704));
#42264=CARTESIAN_POINT('Origin',(57.8084417581558,-85.425,9.00000029802322));
#42265=CARTESIAN_POINT('Ctrl Pts',(49.7768934965134,-85.725,7.0799800157547));
#42266=CARTESIAN_POINT('Ctrl Pts',(49.7768934965134,-85.425,7.0799800157547));
#42267=CARTESIAN_POINT('Ctrl Pts',(49.3471523523331,-85.725,6.67019152641296));
#42268=CARTESIAN_POINT('Ctrl Pts',(49.3471523523331,-85.425,6.67019152641296));
#42269=CARTESIAN_POINT('Ctrl Pts',(48.6902626752853,-85.725,6.67019152641296));
#42270=CARTESIAN_POINT('Ctrl Pts',(48.6902626752853,-85.425,6.67019152641296));
#42271=CARTESIAN_POINT('',(49.7768934965134,-85.425,7.0799800157547));
#42272=CARTESIAN_POINT('',(49.7768934965134,-85.725,7.0799800157547));
#42273=CARTESIAN_POINT('',(48.6902626752853,-85.425,6.67019152641296));
#42274=CARTESIAN_POINT('Ctrl Pts',(49.7768934965134,-85.425,7.0799800157547));
#42275=CARTESIAN_POINT('Ctrl Pts',(49.3471523523331,-85.425,6.67019152641296));
#42276=CARTESIAN_POINT('Ctrl Pts',(48.6902626752853,-85.425,6.67019152641296));
#42277=CARTESIAN_POINT('',(48.6902626752853,-85.725,6.67019152641296));
#42278=CARTESIAN_POINT('Ctrl Pts',(50.2066334486008,-85.725,8.07912731170654));
#42279=CARTESIAN_POINT('Ctrl Pts',(50.2066334486008,-85.425,8.07912731170654));
#42280=CARTESIAN_POINT('Ctrl Pts',(50.2066334486008,-85.725,7.48976850509643));
#42281=CARTESIAN_POINT('Ctrl Pts',(50.2066334486008,-85.425,7.48976850509643));
#42282=CARTESIAN_POINT('Ctrl Pts',(49.7768934965134,-85.725,7.0799800157547));
#42283=CARTESIAN_POINT('Ctrl Pts',(49.7768934965134,-85.425,7.0799800157547));
#42284=CARTESIAN_POINT('',(50.2066334486008,-85.425,8.07912731170654));
#42285=CARTESIAN_POINT('',(50.2066334486008,-85.725,8.07912731170654));
#42286=CARTESIAN_POINT('Ctrl Pts',(50.2066334486008,-85.425,8.07912731170654));
#42287=CARTESIAN_POINT('Ctrl Pts',(50.2066334486008,-85.425,7.48976850509643));
#42288=CARTESIAN_POINT('Ctrl Pts',(49.7768934965134,-85.425,7.0799800157547));
#42289=CARTESIAN_POINT('Ctrl Pts',(49.9856241941452,-85.725,8.80508208274841));
#42290=CARTESIAN_POINT('Ctrl Pts',(49.9856241941452,-85.425,8.80508208274841));
#42291=CARTESIAN_POINT('Ctrl Pts',(50.2066334486008,-85.725,8.51500713825226));
#42292=CARTESIAN_POINT('Ctrl Pts',(50.2066334486008,-85.425,8.51500713825226));
#42293=CARTESIAN_POINT('Ctrl Pts',(50.2066334486008,-85.725,8.07912731170654));
#42294=CARTESIAN_POINT('Ctrl Pts',(50.2066334486008,-85.425,8.07912731170654));
#42295=CARTESIAN_POINT('',(49.9856241941452,-85.425,8.80508208274841));
#42296=CARTESIAN_POINT('',(49.9856241941452,-85.725,8.80508208274841));
#42297=CARTESIAN_POINT('Ctrl Pts',(49.9856241941452,-85.425,8.80508208274841));
#42298=CARTESIAN_POINT('Ctrl Pts',(50.2066334486008,-85.425,8.51500713825226));
#42299=CARTESIAN_POINT('Ctrl Pts',(50.2066334486008,-85.425,8.07912731170654));
#42300=CARTESIAN_POINT('Ctrl Pts',(49.3655695915222,-85.725,9.1872444152832));
#42301=CARTESIAN_POINT('Ctrl Pts',(49.3655695915222,-85.425,9.1872444152832));
#42302=CARTESIAN_POINT('Ctrl Pts',(49.7646149396896,-85.725,9.09515702724457));
#42303=CARTESIAN_POINT('Ctrl Pts',(49.7646149396896,-85.425,9.09515702724457));
#42304=CARTESIAN_POINT('Ctrl Pts',(49.9856241941452,-85.725,8.80508208274841));
#42305=CARTESIAN_POINT('Ctrl Pts',(49.9856241941452,-85.425,8.80508208274841));
#42306=CARTESIAN_POINT('',(49.3655695915222,-85.425,9.1872444152832));
#42307=CARTESIAN_POINT('',(49.3655695915222,-85.725,9.1872444152832));
#42308=CARTESIAN_POINT('Ctrl Pts',(49.3655695915222,-85.425,9.1872444152832));
#42309=CARTESIAN_POINT('Ctrl Pts',(49.7646149396896,-85.425,9.09515702724457));
#42310=CARTESIAN_POINT('Ctrl Pts',(49.9856241941452,-85.425,8.80508208274841));
#42311=CARTESIAN_POINT('Ctrl Pts',(49.8290761709213,-85.725,9.56787192821503));
#42312=CARTESIAN_POINT('Ctrl Pts',(49.8290761709213,-85.425,9.56787192821503));
#42313=CARTESIAN_POINT('Ctrl Pts',(49.672527551651,-85.725,9.32844483852386));
#42314=CARTESIAN_POINT('Ctrl Pts',(49.672527551651,-85.425,9.32844483852386));
#42315=CARTESIAN_POINT('Ctrl Pts',(49.3655695915222,-85.725,9.1872444152832));
#42316=CARTESIAN_POINT('Ctrl Pts',(49.3655695915222,-85.425,9.1872444152832));
#42317=CARTESIAN_POINT('',(49.8290761709213,-85.425,9.56787192821503));
#42318=CARTESIAN_POINT('',(49.8290761709213,-85.725,9.56787192821503));
#42319=CARTESIAN_POINT('Ctrl Pts',(49.8290761709213,-85.425,9.56787192821503));
#42320=CARTESIAN_POINT('Ctrl Pts',(49.672527551651,-85.425,9.32844483852386));
#42321=CARTESIAN_POINT('Ctrl Pts',(49.3655695915222,-85.425,9.1872444152832));
#42322=CARTESIAN_POINT('Ctrl Pts',(49.9856241941452,-85.725,10.0989087820053));
#42323=CARTESIAN_POINT('Ctrl Pts',(49.9856241941452,-85.425,10.0989087820053));
#42324=CARTESIAN_POINT('Ctrl Pts',(49.9856241941452,-85.725,9.80729901790619));
#42325=CARTESIAN_POINT('Ctrl Pts',(49.9856241941452,-85.425,9.80729901790619));
#42326=CARTESIAN_POINT('Ctrl Pts',(49.8290761709213,-85.725,9.56787192821503));
#42327=CARTESIAN_POINT('Ctrl Pts',(49.8290761709213,-85.425,9.56787192821503));
#42328=CARTESIAN_POINT('',(49.9856241941452,-85.425,10.0989087820053));
#42329=CARTESIAN_POINT('',(49.9856241941452,-85.725,10.0989087820053));
#42330=CARTESIAN_POINT('Ctrl Pts',(49.9856241941452,-85.425,10.0989087820053));
#42331=CARTESIAN_POINT('Ctrl Pts',(49.9856241941452,-85.425,9.80729901790619));
#42332=CARTESIAN_POINT('Ctrl Pts',(49.8290761709213,-85.425,9.56787192821503));
#42333=CARTESIAN_POINT('Ctrl Pts',(49.8214020729065,-85.725,10.6790586709976));
#42334=CARTESIAN_POINT('Ctrl Pts',(49.8214020729065,-85.425,10.6790586709976));
#42335=CARTESIAN_POINT('Ctrl Pts',(49.9856241941452,-85.725,10.4058664441109));
#42336=CARTESIAN_POINT('Ctrl Pts',(49.9856241941452,-85.425,10.4058664441109));
#42337=CARTESIAN_POINT('Ctrl Pts',(49.9856241941452,-85.725,10.0989087820053));
#42338=CARTESIAN_POINT('Ctrl Pts',(49.9856241941452,-85.425,10.0989087820053));
#42339=CARTESIAN_POINT('',(49.8214020729065,-85.425,10.6790586709976));
#42340=CARTESIAN_POINT('',(49.8214020729065,-85.725,10.6790586709976));
#42341=CARTESIAN_POINT('Ctrl Pts',(49.8214020729065,-85.425,10.6790586709976));
#42342=CARTESIAN_POINT('Ctrl Pts',(49.9856241941452,-85.425,10.4058664441109));
#42343=CARTESIAN_POINT('Ctrl Pts',(49.9856241941452,-85.425,10.0989087820053));
#42344=CARTESIAN_POINT('Ctrl Pts',(49.3471523523331,-85.725,11.1103343367577));
#42345=CARTESIAN_POINT('Ctrl Pts',(49.3471523523331,-85.425,11.1103343367577));
#42346=CARTESIAN_POINT('Ctrl Pts',(49.6571799516678,-85.725,10.9522508978844));
#42347=CARTESIAN_POINT('Ctrl Pts',(49.6571799516678,-85.425,10.9522508978844));
#42348=CARTESIAN_POINT('Ctrl Pts',(49.8214020729065,-85.725,10.6790586709976));
#42349=CARTESIAN_POINT('Ctrl Pts',(49.8214020729065,-85.425,10.6790586709976));
#42350=CARTESIAN_POINT('',(49.3471523523331,-85.425,11.1103343367577));
#42351=CARTESIAN_POINT('',(49.3471523523331,-85.725,11.1103343367577));
#42352=CARTESIAN_POINT('Ctrl Pts',(49.3471523523331,-85.425,11.1103343367577));
#42353=CARTESIAN_POINT('Ctrl Pts',(49.6571799516678,-85.425,10.9522508978844));
#42354=CARTESIAN_POINT('Ctrl Pts',(49.8214020729065,-85.425,10.6790586709976));
#42355=CARTESIAN_POINT('Ctrl Pts',(48.6687757968903,-85.725,11.2684174776077));
#42356=CARTESIAN_POINT('Ctrl Pts',(48.6687757968903,-85.425,11.2684174776077));
#42357=CARTESIAN_POINT('Ctrl Pts',(49.0371247529984,-85.725,11.2684174776077));
#42358=CARTESIAN_POINT('Ctrl Pts',(49.0371247529984,-85.425,11.2684174776077));
#42359=CARTESIAN_POINT('Ctrl Pts',(49.3471523523331,-85.725,11.1103343367577));
#42360=CARTESIAN_POINT('Ctrl Pts',(49.3471523523331,-85.425,11.1103343367577));
#42361=CARTESIAN_POINT('',(48.6687757968903,-85.425,11.2684174776077));
#42362=CARTESIAN_POINT('',(48.6687757968903,-85.725,11.2684174776077));
#42363=CARTESIAN_POINT('Ctrl Pts',(48.6687757968903,-85.425,11.2684174776077));
#42364=CARTESIAN_POINT('Ctrl Pts',(49.0371247529984,-85.425,11.2684174776077));
#42365=CARTESIAN_POINT('Ctrl Pts',(49.3471523523331,-85.425,11.1103343367577));
#42366=CARTESIAN_POINT('Ctrl Pts',(47.7755289673805,-85.725,10.9629946351051));
#42367=CARTESIAN_POINT('Ctrl Pts',(47.7755289673805,-85.425,10.9629946351051));
#42368=CARTESIAN_POINT('Ctrl Pts',(48.134669303894,-85.725,11.2684174776077));
#42369=CARTESIAN_POINT('Ctrl Pts',(48.134669303894,-85.425,11.2684174776077));
#42370=CARTESIAN_POINT('Ctrl Pts',(48.6687757968903,-85.725,11.2684174776077));
#42371=CARTESIAN_POINT('Ctrl Pts',(48.6687757968903,-85.425,11.2684174776077));
#42372=CARTESIAN_POINT('',(47.7755289673805,-85.425,10.9629946351051));
#42373=CARTESIAN_POINT('',(47.7755289673805,-85.725,10.9629946351051));
#42374=CARTESIAN_POINT('Ctrl Pts',(47.7755289673805,-85.425,10.9629946351051));
#42375=CARTESIAN_POINT('Ctrl Pts',(48.134669303894,-85.425,11.2684174776077));
#42376=CARTESIAN_POINT('Ctrl Pts',(48.6687757968903,-85.425,11.2684174776077));
#42377=CARTESIAN_POINT('Ctrl Pts',(47.3150923252106,-85.725,10.1019784212112));
#42378=CARTESIAN_POINT('Ctrl Pts',(47.3150923252106,-85.425,10.1019784212112));
#42379=CARTESIAN_POINT('Ctrl Pts',(47.4163883328438,-85.725,10.6575717926025));
#42380=CARTESIAN_POINT('Ctrl Pts',(47.4163883328438,-85.425,10.6575717926025));
#42381=CARTESIAN_POINT('Ctrl Pts',(47.7755289673805,-85.725,10.9629946351051));
#42382=CARTESIAN_POINT('Ctrl Pts',(47.7755289673805,-85.425,10.9629946351051));
#42383=CARTESIAN_POINT('',(47.3150923252106,-85.425,10.1019784212112));
#42384=CARTESIAN_POINT('',(47.3150923252106,-85.725,10.1019784212112));
#42385=CARTESIAN_POINT('Ctrl Pts',(47.3150923252106,-85.425,10.1019784212112));
#42386=CARTESIAN_POINT('Ctrl Pts',(47.4163883328438,-85.425,10.6575717926025));
#42387=CARTESIAN_POINT('Ctrl Pts',(47.7755289673805,-85.425,10.9629946351051));
#42388=CARTESIAN_POINT('Origin',(47.8676160573959,-85.725,10.0037517547607));
#42389=CARTESIAN_POINT('',(47.8676160573959,-85.425,10.0037517547607));
#42390=CARTESIAN_POINT('',(47.8676160573959,-85.725,10.0037517547607));
#42391=CARTESIAN_POINT('',(47.8676160573959,-85.425,10.0037517547607));
#42392=CARTESIAN_POINT('Ctrl Pts',(48.1438782215118,-85.725,10.6115280985832));
#42393=CARTESIAN_POINT('Ctrl Pts',(48.1438782215118,-85.425,10.6115280985832));
#42394=CARTESIAN_POINT('Ctrl Pts',(47.9290076494217,-85.725,10.4089357852936));
#42395=CARTESIAN_POINT('Ctrl Pts',(47.9290076494217,-85.425,10.4089357852936));
#42396=CARTESIAN_POINT('Ctrl Pts',(47.8676160573959,-85.725,10.0037517547607));
#42397=CARTESIAN_POINT('Ctrl Pts',(47.8676160573959,-85.425,10.0037517547607));
#42398=CARTESIAN_POINT('',(48.1438782215118,-85.425,10.6115280985832));
#42399=CARTESIAN_POINT('',(48.1438782215118,-85.725,10.6115280985832));
#42400=CARTESIAN_POINT('Ctrl Pts',(48.1438782215118,-85.425,10.6115280985832));
#42401=CARTESIAN_POINT('Ctrl Pts',(47.9290076494217,-85.425,10.4089357852936));
#42402=CARTESIAN_POINT('Ctrl Pts',(47.8676160573959,-85.425,10.0037517547607));
#42403=CARTESIAN_POINT('Ctrl Pts',(48.6810540556908,-85.725,10.8141201138496));
#42404=CARTESIAN_POINT('Ctrl Pts',(48.6810540556908,-85.425,10.8141201138496));
#42405=CARTESIAN_POINT('Ctrl Pts',(48.3587484955788,-85.725,10.8141201138496));
#42406=CARTESIAN_POINT('Ctrl Pts',(48.3587484955788,-85.425,10.8141201138496));
#42407=CARTESIAN_POINT('Ctrl Pts',(48.1438782215118,-85.725,10.6115280985832));
#42408=CARTESIAN_POINT('Ctrl Pts',(48.1438782215118,-85.425,10.6115280985832));
#42409=CARTESIAN_POINT('',(48.6810540556908,-85.425,10.8141201138496));
#42410=CARTESIAN_POINT('',(48.6810540556908,-85.725,10.8141201138496));
#42411=CARTESIAN_POINT('Ctrl Pts',(48.6810540556908,-85.425,10.8141201138496));
#42412=CARTESIAN_POINT('Ctrl Pts',(48.3587484955788,-85.425,10.8141201138496));
#42413=CARTESIAN_POINT('Ctrl Pts',(48.1438782215118,-85.425,10.6115280985832));
#42414=CARTESIAN_POINT('Ctrl Pts',(49.2120906114578,-85.725,10.6145974397659));
#42415=CARTESIAN_POINT('Ctrl Pts',(49.2120906114578,-85.425,10.6145974397659));
#42416=CARTESIAN_POINT('Ctrl Pts',(49.0064295530319,-85.725,10.8141201138496));
#42417=CARTESIAN_POINT('Ctrl Pts',(49.0064295530319,-85.425,10.8141201138496));
#42418=CARTESIAN_POINT('Ctrl Pts',(48.6810540556908,-85.725,10.8141201138496));
#42419=CARTESIAN_POINT('Ctrl Pts',(48.6810540556908,-85.425,10.8141201138496));
#42420=CARTESIAN_POINT('',(49.2120906114578,-85.425,10.6145974397659));
#42421=CARTESIAN_POINT('',(49.2120906114578,-85.725,10.6145974397659));
#42422=CARTESIAN_POINT('Ctrl Pts',(49.2120906114578,-85.425,10.6145974397659));
#42423=CARTESIAN_POINT('Ctrl Pts',(49.0064295530319,-85.425,10.8141201138496));
#42424=CARTESIAN_POINT('Ctrl Pts',(48.6810540556908,-85.425,10.8141201138496));
#42425=CARTESIAN_POINT('Ctrl Pts',(49.4177528619766,-85.725,10.111187338829));
#42426=CARTESIAN_POINT('Ctrl Pts',(49.4177528619766,-85.425,10.111187338829));
#42427=CARTESIAN_POINT('Ctrl Pts',(49.4177528619766,-85.725,10.4150750637054));
#42428=CARTESIAN_POINT('Ctrl Pts',(49.4177528619766,-85.425,10.4150750637054));
#42429=CARTESIAN_POINT('Ctrl Pts',(49.2120906114578,-85.725,10.6145974397659));
#42430=CARTESIAN_POINT('Ctrl Pts',(49.2120906114578,-85.425,10.6145974397659));
#42431=CARTESIAN_POINT('',(49.4177528619766,-85.425,10.111187338829));
#42432=CARTESIAN_POINT('',(49.4177528619766,-85.725,10.111187338829));
#42433=CARTESIAN_POINT('Ctrl Pts',(49.4177528619766,-85.425,10.111187338829));
#42434=CARTESIAN_POINT('Ctrl Pts',(49.4177528619766,-85.425,10.4150750637054));
#42435=CARTESIAN_POINT('Ctrl Pts',(49.2120906114578,-85.425,10.6145974397659));
#42436=CARTESIAN_POINT('Ctrl Pts',(49.1353514194489,-85.725,9.54331481456757));
#42437=CARTESIAN_POINT('Ctrl Pts',(49.1353514194489,-85.425,9.54331481456757));
#42438=CARTESIAN_POINT('Ctrl Pts',(49.4177528619766,-85.725,9.72748959064484));
#42439=CARTESIAN_POINT('Ctrl Pts',(49.4177528619766,-85.425,9.72748959064484));
#42440=CARTESIAN_POINT('Ctrl Pts',(49.4177528619766,-85.725,10.111187338829));
#42441=CARTESIAN_POINT('Ctrl Pts',(49.4177528619766,-85.425,10.111187338829));
#42442=CARTESIAN_POINT('',(49.1353514194489,-85.425,9.54331481456757));
#42443=CARTESIAN_POINT('',(49.1353514194489,-85.725,9.54331481456757));
#42444=CARTESIAN_POINT('Ctrl Pts',(49.1353514194489,-85.425,9.54331481456757));
#42445=CARTESIAN_POINT('Ctrl Pts',(49.4177528619766,-85.425,9.72748959064484));
#42446=CARTESIAN_POINT('Ctrl Pts',(49.4177528619766,-85.425,10.111187338829));
#42447=CARTESIAN_POINT('Ctrl Pts',(48.4999492168427,-85.725,9.35914063453674));
#42448=CARTESIAN_POINT('Ctrl Pts',(48.4999492168427,-85.425,9.35914063453674));
#42449=CARTESIAN_POINT('Ctrl Pts',(48.8529505729675,-85.725,9.35914063453674));
#42450=CARTESIAN_POINT('Ctrl Pts',(48.8529505729675,-85.425,9.35914063453674));
#42451=CARTESIAN_POINT('Ctrl Pts',(49.1353514194489,-85.725,9.54331481456757));
#42452=CARTESIAN_POINT('Ctrl Pts',(49.1353514194489,-85.425,9.54331481456757));
#42453=CARTESIAN_POINT('',(48.4999492168427,-85.425,9.35914063453674));
#42454=CARTESIAN_POINT('',(48.4999492168427,-85.725,9.35914063453674));
#42455=CARTESIAN_POINT('Ctrl Pts',(48.4999492168427,-85.425,9.35914063453674));
#42456=CARTESIAN_POINT('Ctrl Pts',(48.8529505729675,-85.425,9.35914063453674));
#42457=CARTESIAN_POINT('Ctrl Pts',(49.1353514194489,-85.425,9.54331481456757));
#42458=CARTESIAN_POINT('Ctrl Pts',(48.4109314680099,-85.725,9.36527991294861));
#42459=CARTESIAN_POINT('Ctrl Pts',(48.4109314680099,-85.425,9.36527991294861));
#42460=CARTESIAN_POINT('Ctrl Pts',(48.4661837816238,-85.725,9.35914063453674));
#42461=CARTESIAN_POINT('Ctrl Pts',(48.4661837816238,-85.425,9.35914063453674));
#42462=CARTESIAN_POINT('Ctrl Pts',(48.4999492168427,-85.725,9.35914063453674));
#42463=CARTESIAN_POINT('Ctrl Pts',(48.4999492168427,-85.425,9.35914063453674));
#42464=CARTESIAN_POINT('',(48.4109314680099,-85.425,9.36527991294861));
#42465=CARTESIAN_POINT('',(48.4109314680099,-85.725,9.36527991294861));
#42466=CARTESIAN_POINT('Ctrl Pts',(48.4109314680099,-85.425,9.36527991294861));
#42467=CARTESIAN_POINT('Ctrl Pts',(48.4661837816238,-85.425,9.35914063453674));
#42468=CARTESIAN_POINT('Ctrl Pts',(48.4999492168427,-85.425,9.35914063453674));
#42469=CARTESIAN_POINT('Origin',(48.3495398759842,-85.725,8.88028705120087));
#42470=CARTESIAN_POINT('',(48.3495398759842,-85.425,8.88028705120087));
#42471=CARTESIAN_POINT('',(48.3495398759842,-85.725,8.88028705120087));
#42472=CARTESIAN_POINT('',(48.3495398759842,-85.425,8.88028705120087));
#42473=CARTESIAN_POINT('Ctrl Pts',(48.7393763065338,-85.725,8.94167864322662));
#42474=CARTESIAN_POINT('Ctrl Pts',(48.7393763065338,-85.425,8.94167864322662));
#42475=CARTESIAN_POINT('Ctrl Pts',(48.5828276872635,-85.725,8.94167864322662));
#42476=CARTESIAN_POINT('Ctrl Pts',(48.5828276872635,-85.425,8.94167864322662));
#42477=CARTESIAN_POINT('Ctrl Pts',(48.3495398759842,-85.725,8.88028705120087));
#42478=CARTESIAN_POINT('Ctrl Pts',(48.3495398759842,-85.425,8.88028705120087));
#42479=CARTESIAN_POINT('',(48.7393763065338,-85.425,8.94167864322662));
#42480=CARTESIAN_POINT('',(48.7393763065338,-85.725,8.94167864322662));
#42481=CARTESIAN_POINT('Ctrl Pts',(48.7393763065338,-85.425,8.94167864322662));
#42482=CARTESIAN_POINT('Ctrl Pts',(48.5828276872635,-85.425,8.94167864322662));
#42483=CARTESIAN_POINT('Ctrl Pts',(48.3495398759842,-85.425,8.88028705120087));
#42484=CARTESIAN_POINT('Ctrl Pts',(49.3717088699341,-85.725,8.69457745552063));
#42485=CARTESIAN_POINT('Ctrl Pts',(49.3717088699341,-85.425,8.69457745552063));
#42486=CARTESIAN_POINT('Ctrl Pts',(49.1230734586716,-85.725,8.94167864322662));
#42487=CARTESIAN_POINT('Ctrl Pts',(49.1230734586716,-85.425,8.94167864322662));
#42488=CARTESIAN_POINT('Ctrl Pts',(48.7393763065338,-85.725,8.94167864322662));
#42489=CARTESIAN_POINT('Ctrl Pts',(48.7393763065338,-85.425,8.94167864322662));
#42490=CARTESIAN_POINT('',(49.3717088699341,-85.425,8.69457745552063));
#42491=CARTESIAN_POINT('',(49.3717088699341,-85.725,8.69457745552063));
#42492=CARTESIAN_POINT('Ctrl Pts',(49.3717088699341,-85.425,8.69457745552063));
#42493=CARTESIAN_POINT('Ctrl Pts',(49.1230734586716,-85.425,8.94167864322662));
#42494=CARTESIAN_POINT('Ctrl Pts',(48.7393763065338,-85.425,8.94167864322662));
#42495=CARTESIAN_POINT('Ctrl Pts',(49.620344877243,-85.725,8.06684875488281));
#42496=CARTESIAN_POINT('Ctrl Pts',(49.620344877243,-85.425,8.06684875488281));
#42497=CARTESIAN_POINT('Ctrl Pts',(49.620344877243,-85.725,8.44747626781464));
#42498=CARTESIAN_POINT('Ctrl Pts',(49.620344877243,-85.425,8.44747626781464));
#42499=CARTESIAN_POINT('Ctrl Pts',(49.3717088699341,-85.725,8.69457745552063));
#42500=CARTESIAN_POINT('Ctrl Pts',(49.3717088699341,-85.425,8.69457745552063));
#42501=CARTESIAN_POINT('',(49.620344877243,-85.425,8.06684875488281));
#42502=CARTESIAN_POINT('',(49.620344877243,-85.725,8.06684875488281));
#42503=CARTESIAN_POINT('Ctrl Pts',(49.620344877243,-85.425,8.06684875488281));
#42504=CARTESIAN_POINT('Ctrl Pts',(49.620344877243,-85.425,8.44747626781464));
#42505=CARTESIAN_POINT('Ctrl Pts',(49.3717088699341,-85.425,8.69457745552063));
#42506=CARTESIAN_POINT('Ctrl Pts',(49.351756811142,-85.725,7.3976811170578));
#42507=CARTESIAN_POINT('Ctrl Pts',(49.351756811142,-85.425,7.3976811170578));
#42508=CARTESIAN_POINT('Ctrl Pts',(49.620344877243,-85.725,7.66780400276184));
#42509=CARTESIAN_POINT('Ctrl Pts',(49.620344877243,-85.425,7.66780400276184));
#42510=CARTESIAN_POINT('Ctrl Pts',(49.620344877243,-85.725,8.06684875488281));
#42511=CARTESIAN_POINT('Ctrl Pts',(49.620344877243,-85.425,8.06684875488281));
#42512=CARTESIAN_POINT('',(49.351756811142,-85.425,7.3976811170578));
#42513=CARTESIAN_POINT('',(49.351756811142,-85.725,7.3976811170578));
#42514=CARTESIAN_POINT('Ctrl Pts',(49.351756811142,-85.425,7.3976811170578));
#42515=CARTESIAN_POINT('Ctrl Pts',(49.620344877243,-85.425,7.66780400276184));
#42516=CARTESIAN_POINT('Ctrl Pts',(49.620344877243,-85.425,8.06684875488281));
#42517=CARTESIAN_POINT('Ctrl Pts',(48.6933323144913,-85.725,7.12755823135376));
#42518=CARTESIAN_POINT('Ctrl Pts',(48.6933323144913,-85.425,7.12755823135376));
#42519=CARTESIAN_POINT('Ctrl Pts',(49.0831687450409,-85.725,7.12755823135376));
#42520=CARTESIAN_POINT('Ctrl Pts',(49.0831687450409,-85.425,7.12755823135376));
#42521=CARTESIAN_POINT('Ctrl Pts',(49.351756811142,-85.725,7.3976811170578));
#42522=CARTESIAN_POINT('Ctrl Pts',(49.351756811142,-85.425,7.3976811170578));
#42523=CARTESIAN_POINT('',(48.6933323144913,-85.425,7.12755823135376));
#42524=CARTESIAN_POINT('',(48.6933323144913,-85.725,7.12755823135376));
#42525=CARTESIAN_POINT('Ctrl Pts',(48.6933323144913,-85.425,7.12755823135376));
#42526=CARTESIAN_POINT('Ctrl Pts',(49.0831687450409,-85.425,7.12755823135376));
#42527=CARTESIAN_POINT('Ctrl Pts',(49.351756811142,-85.425,7.3976811170578));
#42528=CARTESIAN_POINT('Ctrl Pts',(48.136204123497,-85.725,7.33475470542908));
#42529=CARTESIAN_POINT('Ctrl Pts',(48.136204123497,-85.425,7.33475470542908));
#42530=CARTESIAN_POINT('Ctrl Pts',(48.3648877739906,-85.725,7.12755823135376));
#42531=CARTESIAN_POINT('Ctrl Pts',(48.3648877739906,-85.425,7.12755823135376));
#42532=CARTESIAN_POINT('Ctrl Pts',(48.6933323144913,-85.725,7.12755823135376));
#42533=CARTESIAN_POINT('Ctrl Pts',(48.6933323144913,-85.425,7.12755823135376));
#42534=CARTESIAN_POINT('',(48.136204123497,-85.425,7.33475470542908));
#42535=CARTESIAN_POINT('',(48.136204123497,-85.725,7.33475470542908));
#42536=CARTESIAN_POINT('Ctrl Pts',(48.136204123497,-85.425,7.33475470542908));
#42537=CARTESIAN_POINT('Ctrl Pts',(48.3648877739906,-85.425,7.12755823135376));
#42538=CARTESIAN_POINT('Ctrl Pts',(48.6933323144913,-85.425,7.12755823135376));
#42539=CARTESIAN_POINT('Ctrl Pts',(47.812363743782,-85.725,8.01159644126892));
#42540=CARTESIAN_POINT('Ctrl Pts',(47.812363743782,-85.425,8.01159644126892));
#42541=CARTESIAN_POINT('Ctrl Pts',(47.9075207710266,-85.725,7.54195117950439));
#42542=CARTESIAN_POINT('Ctrl Pts',(47.9075207710266,-85.425,7.54195117950439));
#42543=CARTESIAN_POINT('Ctrl Pts',(48.136204123497,-85.725,7.33475470542908));
#42544=CARTESIAN_POINT('Ctrl Pts',(48.136204123497,-85.425,7.33475470542908));
#42545=CARTESIAN_POINT('',(47.812363743782,-85.425,8.01159644126892));
#42546=CARTESIAN_POINT('',(47.812363743782,-85.725,8.01159644126892));
#42547=CARTESIAN_POINT('Ctrl Pts',(47.812363743782,-85.425,8.01159644126892));
#42548=CARTESIAN_POINT('Ctrl Pts',(47.9075207710266,-85.425,7.54195117950439));
#42549=CARTESIAN_POINT('Ctrl Pts',(48.136204123497,-85.425,7.33475470542908));
#42550=CARTESIAN_POINT('Origin',(47.2598400115967,-85.725,7.93792688846588));
#42551=CARTESIAN_POINT('',(47.2598400115967,-85.425,7.93792688846588));
#42552=CARTESIAN_POINT('',(47.2598400115967,-85.725,7.93792688846588));
#42553=CARTESIAN_POINT('',(47.2598400115967,-85.425,7.93792688846588));
#42554=CARTESIAN_POINT('Ctrl Pts',(47.7064635753632,-85.725,7.02319288253784));
#42555=CARTESIAN_POINT('Ctrl Pts',(47.7064635753632,-85.425,7.02319288253784));
#42556=CARTESIAN_POINT('Ctrl Pts',(47.3150923252106,-85.725,7.37619423866272));
#42557=CARTESIAN_POINT('Ctrl Pts',(47.3150923252106,-85.425,7.37619423866272));
#42558=CARTESIAN_POINT('Ctrl Pts',(47.2598400115967,-85.725,7.93792688846588));
#42559=CARTESIAN_POINT('Ctrl Pts',(47.2598400115967,-85.425,7.93792688846588));
#42560=CARTESIAN_POINT('',(47.7064635753632,-85.425,7.02319288253784));
#42561=CARTESIAN_POINT('',(47.7064635753632,-85.725,7.02319288253784));
#42562=CARTESIAN_POINT('Ctrl Pts',(47.7064635753632,-85.425,7.02319288253784));
#42563=CARTESIAN_POINT('Ctrl Pts',(47.3150923252106,-85.425,7.37619423866272));
#42564=CARTESIAN_POINT('Ctrl Pts',(47.2598400115967,-85.425,7.93792688846588));
#42565=CARTESIAN_POINT('Ctrl Pts',(48.6902626752853,-85.725,6.67019152641296));
#42566=CARTESIAN_POINT('Ctrl Pts',(48.6902626752853,-85.425,6.67019152641296));
#42567=CARTESIAN_POINT('Ctrl Pts',(48.0978345274925,-85.725,6.67019152641296));
#42568=CARTESIAN_POINT('Ctrl Pts',(48.0978345274925,-85.425,6.67019152641296));
#42569=CARTESIAN_POINT('Ctrl Pts',(47.7064635753632,-85.725,7.02319288253784));
#42570=CARTESIAN_POINT('Ctrl Pts',(47.7064635753632,-85.425,7.02319288253784));
#42571=CARTESIAN_POINT('Ctrl Pts',(48.6902626752853,-85.425,6.67019152641296));
#42572=CARTESIAN_POINT('Ctrl Pts',(48.0978345274925,-85.425,6.67019152641296));
#42573=CARTESIAN_POINT('Ctrl Pts',(47.7064635753632,-85.425,7.02319288253784));
#42574=CARTESIAN_POINT('Origin',(48.7332367300987,-85.425,8.96930450201035));
#42575=CARTESIAN_POINT('Origin',(69.2472215890884,-85.725,11.2500002384186));
#42576=CARTESIAN_POINT('',(69.2472215890884,-85.425,11.2500002384186));
#42577=CARTESIAN_POINT('',(69.2472215890884,-85.725,11.2500002384186));
#42578=CARTESIAN_POINT('',(69.8427196741104,-85.425,11.2500002384186));
#42579=CARTESIAN_POINT('',(69.2472215890884,-85.425,11.2500002384186));
#42580=CARTESIAN_POINT('',(69.8427196741104,-85.725,11.2500002384186));
#42581=CARTESIAN_POINT('Origin',(69.2472215890884,-85.725,6.75000035762787));
#42582=CARTESIAN_POINT('',(69.2472215890884,-85.425,6.75000035762787));
#42583=CARTESIAN_POINT('',(69.2472215890884,-85.725,6.75000035762787));
#42584=CARTESIAN_POINT('',(69.2472215890884,-85.425,6.75000035762787));
#42585=CARTESIAN_POINT('Origin',(69.8427196741104,-85.725,6.75000035762787));
#42586=CARTESIAN_POINT('',(69.8427196741104,-85.425,6.75000035762787));
#42587=CARTESIAN_POINT('',(69.8427196741104,-85.725,6.75000035762787));
#42588=CARTESIAN_POINT('',(69.8427196741104,-85.425,6.75000035762787));
#42589=CARTESIAN_POINT('Origin',(69.8427196741104,-85.725,11.2500002384186));
#42590=CARTESIAN_POINT('',(69.8427196741104,-85.425,11.2500002384186));
#42591=CARTESIAN_POINT('Origin',(69.5449706315994,-85.425,9.00000029802322));
#42592=CARTESIAN_POINT('Ctrl Pts',(76.8014498949051,-85.725,6.6732611656189));
#42593=CARTESIAN_POINT('Ctrl Pts',(76.8014498949051,-85.425,6.6732611656189));
#42594=CARTESIAN_POINT('Ctrl Pts',(76.1906048059464,-85.725,6.6732611656189));
#42595=CARTESIAN_POINT('Ctrl Pts',(76.1906048059464,-85.425,6.6732611656189));
#42596=CARTESIAN_POINT('Ctrl Pts',(75.7777472734451,-85.725,6.8512966632843));
#42597=CARTESIAN_POINT('Ctrl Pts',(75.7777472734451,-85.425,6.8512966632843));
#42598=CARTESIAN_POINT('',(76.8014498949051,-85.425,6.6732611656189));
#42599=CARTESIAN_POINT('',(76.8014498949051,-85.725,6.6732611656189));
#42600=CARTESIAN_POINT('',(75.7777472734451,-85.425,6.8512966632843));
#42601=CARTESIAN_POINT('Ctrl Pts',(76.8014498949051,-85.425,6.6732611656189));
#42602=CARTESIAN_POINT('Ctrl Pts',(76.1906048059464,-85.425,6.6732611656189));
#42603=CARTESIAN_POINT('Ctrl Pts',(75.7777472734451,-85.425,6.8512966632843));
#42604=CARTESIAN_POINT('',(75.7777472734451,-85.725,6.8512966632843));
#42605=CARTESIAN_POINT('Ctrl Pts',(77.668606877327,-85.725,6.84976184368133));
#42606=CARTESIAN_POINT('Ctrl Pts',(77.668606877327,-85.425,6.84976184368133));
#42607=CARTESIAN_POINT('Ctrl Pts',(77.2833749055862,-85.725,6.6732611656189));
#42608=CARTESIAN_POINT('Ctrl Pts',(77.2833749055862,-85.425,6.6732611656189));
#42609=CARTESIAN_POINT('Ctrl Pts',(76.8014498949051,-85.725,6.6732611656189));
#42610=CARTESIAN_POINT('Ctrl Pts',(76.8014498949051,-85.425,6.6732611656189));
#42611=CARTESIAN_POINT('',(77.668606877327,-85.425,6.84976184368133));
#42612=CARTESIAN_POINT('',(77.668606877327,-85.725,6.84976184368133));
#42613=CARTESIAN_POINT('Ctrl Pts',(77.668606877327,-85.425,6.84976184368133));
#42614=CARTESIAN_POINT('Ctrl Pts',(77.2833749055862,-85.425,6.6732611656189));
#42615=CARTESIAN_POINT('Ctrl Pts',(76.8014498949051,-85.425,6.6732611656189));
#42616=CARTESIAN_POINT('Ctrl Pts',(78.2594987154007,-85.725,7.34396362304687));
#42617=CARTESIAN_POINT('Ctrl Pts',(78.2594987154007,-85.425,7.34396362304687));
#42618=CARTESIAN_POINT('Ctrl Pts',(78.0538388490677,-85.725,7.02626252174377));
#42619=CARTESIAN_POINT('Ctrl Pts',(78.0538388490677,-85.425,7.02626252174377));
#42620=CARTESIAN_POINT('Ctrl Pts',(77.668606877327,-85.725,6.84976184368133));
#42621=CARTESIAN_POINT('Ctrl Pts',(77.668606877327,-85.425,6.84976184368133));
#42622=CARTESIAN_POINT('',(78.2594987154007,-85.425,7.34396362304687));
#42623=CARTESIAN_POINT('',(78.2594987154007,-85.725,7.34396362304687));
#42624=CARTESIAN_POINT('Ctrl Pts',(78.2594987154007,-85.425,7.34396362304687));
#42625=CARTESIAN_POINT('Ctrl Pts',(78.0538388490677,-85.425,7.02626252174377));
#42626=CARTESIAN_POINT('Ctrl Pts',(77.668606877327,-85.425,6.84976184368133));
#42627=CARTESIAN_POINT('Ctrl Pts',(78.4651609659195,-85.725,8.02080535888672));
#42628=CARTESIAN_POINT('Ctrl Pts',(78.4651609659195,-85.425,8.02080535888672));
#42629=CARTESIAN_POINT('Ctrl Pts',(78.4651609659195,-85.725,7.66166472434997));
#42630=CARTESIAN_POINT('Ctrl Pts',(78.4651609659195,-85.425,7.66166472434997));
#42631=CARTESIAN_POINT('Ctrl Pts',(78.2594987154007,-85.725,7.34396362304687));
#42632=CARTESIAN_POINT('Ctrl Pts',(78.2594987154007,-85.425,7.34396362304687));
#42633=CARTESIAN_POINT('',(78.4651609659195,-85.425,8.02080535888672));
#42634=CARTESIAN_POINT('',(78.4651609659195,-85.725,8.02080535888672));
#42635=CARTESIAN_POINT('Ctrl Pts',(78.4651609659195,-85.425,8.02080535888672));
#42636=CARTESIAN_POINT('Ctrl Pts',(78.4651609659195,-85.425,7.66166472434997));
#42637=CARTESIAN_POINT('Ctrl Pts',(78.2594987154007,-85.425,7.34396362304687));
#42638=CARTESIAN_POINT('Ctrl Pts',(78.2779165506363,-85.725,8.66081202030182));
#42639=CARTESIAN_POINT('Ctrl Pts',(78.2779165506363,-85.425,8.66081202030182));
#42640=CARTESIAN_POINT('Ctrl Pts',(78.4651609659195,-85.725,8.38301503658295));
#42641=CARTESIAN_POINT('Ctrl Pts',(78.4651609659195,-85.425,8.38301503658295));
#42642=CARTESIAN_POINT('Ctrl Pts',(78.4651609659195,-85.725,8.02080535888672));
#42643=CARTESIAN_POINT('Ctrl Pts',(78.4651609659195,-85.425,8.02080535888672));
#42644=CARTESIAN_POINT('',(78.2779165506363,-85.425,8.66081202030182));
#42645=CARTESIAN_POINT('',(78.2779165506363,-85.725,8.66081202030182));
#42646=CARTESIAN_POINT('Ctrl Pts',(78.2779165506363,-85.425,8.66081202030182));
#42647=CARTESIAN_POINT('Ctrl Pts',(78.4651609659195,-85.425,8.38301503658295));
#42648=CARTESIAN_POINT('Ctrl Pts',(78.4651609659195,-85.425,8.02080535888672));
#42649=CARTESIAN_POINT('Ctrl Pts',(77.6977654695511,-85.725,9.11971354484558));
#42650=CARTESIAN_POINT('Ctrl Pts',(77.6977654695511,-85.425,9.11971354484558));
#42651=CARTESIAN_POINT('Ctrl Pts',(78.0906721353531,-85.725,8.93860900402069));
#42652=CARTESIAN_POINT('Ctrl Pts',(78.0906721353531,-85.425,8.93860900402069));
#42653=CARTESIAN_POINT('Ctrl Pts',(78.2779165506363,-85.725,8.66081202030182));
#42654=CARTESIAN_POINT('Ctrl Pts',(78.2779165506363,-85.425,8.66081202030182));
#42655=CARTESIAN_POINT('',(77.6977654695511,-85.425,9.11971354484558));
#42656=CARTESIAN_POINT('',(77.6977654695511,-85.725,9.11971354484558));
#42657=CARTESIAN_POINT('Ctrl Pts',(77.6977654695511,-85.425,9.11971354484558));
#42658=CARTESIAN_POINT('Ctrl Pts',(78.0906721353531,-85.425,8.93860900402069));
#42659=CARTESIAN_POINT('Ctrl Pts',(78.2779165506363,-85.425,8.66081202030182));
#42660=CARTESIAN_POINT('Ctrl Pts',(76.7016884088516,-85.725,9.4067188501358));
#42661=CARTESIAN_POINT('Ctrl Pts',(76.7016884088516,-85.425,9.4067188501358));
#42662=CARTESIAN_POINT('Ctrl Pts',(77.4276443719864,-85.725,9.24249672889709));
#42663=CARTESIAN_POINT('Ctrl Pts',(77.4276443719864,-85.425,9.24249672889709));
#42664=CARTESIAN_POINT('Ctrl Pts',(77.6977654695511,-85.725,9.11971354484558));
#42665=CARTESIAN_POINT('Ctrl Pts',(77.6977654695511,-85.425,9.11971354484558));
#42666=CARTESIAN_POINT('',(76.7016884088516,-85.425,9.4067188501358));
#42667=CARTESIAN_POINT('',(76.7016884088516,-85.725,9.4067188501358));
#42668=CARTESIAN_POINT('Ctrl Pts',(76.7016884088516,-85.425,9.4067188501358));
#42669=CARTESIAN_POINT('Ctrl Pts',(77.4276443719864,-85.425,9.24249672889709));
#42670=CARTESIAN_POINT('Ctrl Pts',(77.6977654695511,-85.425,9.11971354484558));
#42671=CARTESIAN_POINT('Ctrl Pts',(75.8038374185562,-85.725,9.72748959064484));
#42672=CARTESIAN_POINT('Ctrl Pts',(75.8038374185562,-85.425,9.72748959064484));
#42673=CARTESIAN_POINT('Ctrl Pts',(75.9757348299026,-85.725,9.57094156742096));
#42674=CARTESIAN_POINT('Ctrl Pts',(75.9757348299026,-85.425,9.57094156742096));
#42675=CARTESIAN_POINT('Ctrl Pts',(76.7016884088516,-85.725,9.4067188501358));
#42676=CARTESIAN_POINT('Ctrl Pts',(76.7016884088516,-85.425,9.4067188501358));
#42677=CARTESIAN_POINT('',(75.8038374185562,-85.425,9.72748959064484));
#42678=CARTESIAN_POINT('',(75.8038374185562,-85.725,9.72748959064484));
#42679=CARTESIAN_POINT('Ctrl Pts',(75.8038374185562,-85.425,9.72748959064484));
#42680=CARTESIAN_POINT('Ctrl Pts',(75.9757348299026,-85.425,9.57094156742096));
#42681=CARTESIAN_POINT('Ctrl Pts',(76.7016884088516,-85.425,9.4067188501358));
#42682=CARTESIAN_POINT('Ctrl Pts',(75.6288715600967,-85.725,10.1265349388123));
#42683=CARTESIAN_POINT('Ctrl Pts',(75.6288715600967,-85.425,10.1265349388123));
#42684=CARTESIAN_POINT('Ctrl Pts',(75.6288715600967,-85.725,9.88403820991516));
#42685=CARTESIAN_POINT('Ctrl Pts',(75.6288715600967,-85.425,9.88403820991516));
#42686=CARTESIAN_POINT('Ctrl Pts',(75.8038374185562,-85.725,9.72748959064484));
#42687=CARTESIAN_POINT('Ctrl Pts',(75.8038374185562,-85.425,9.72748959064484));
#42688=CARTESIAN_POINT('',(75.6288715600967,-85.425,10.1265349388123));
#42689=CARTESIAN_POINT('',(75.6288715600967,-85.725,10.1265349388123));
#42690=CARTESIAN_POINT('Ctrl Pts',(75.6288715600967,-85.425,10.1265349388123));
#42691=CARTESIAN_POINT('Ctrl Pts',(75.6288715600967,-85.425,9.88403820991516));
#42692=CARTESIAN_POINT('Ctrl Pts',(75.8038374185562,-85.425,9.72748959064484));
#42693=CARTESIAN_POINT('Ctrl Pts',(75.8759733438492,-85.725,10.6038540005684));
#42694=CARTESIAN_POINT('Ctrl Pts',(75.8759733438492,-85.425,10.6038540005684));
#42695=CARTESIAN_POINT('Ctrl Pts',(75.6288715600967,-85.725,10.4058664441109));
#42696=CARTESIAN_POINT('Ctrl Pts',(75.6288715600967,-85.425,10.4058664441109));
#42697=CARTESIAN_POINT('Ctrl Pts',(75.6288715600967,-85.725,10.1265349388123));
#42698=CARTESIAN_POINT('Ctrl Pts',(75.6288715600967,-85.425,10.1265349388123));
#42699=CARTESIAN_POINT('',(75.8759733438492,-85.425,10.6038540005684));
#42700=CARTESIAN_POINT('',(75.8759733438492,-85.725,10.6038540005684));
#42701=CARTESIAN_POINT('Ctrl Pts',(75.8759733438492,-85.425,10.6038540005684));
#42702=CARTESIAN_POINT('Ctrl Pts',(75.6288715600967,-85.425,10.4058664441109));
#42703=CARTESIAN_POINT('Ctrl Pts',(75.6288715600967,-85.425,10.1265349388123));
#42704=CARTESIAN_POINT('Ctrl Pts',(76.6633197069168,-85.725,10.8018418550491));
#42705=CARTESIAN_POINT('Ctrl Pts',(76.6633197069168,-85.425,10.8018418550491));
#42706=CARTESIAN_POINT('Ctrl Pts',(76.1230727434158,-85.725,10.8018418550491));
#42707=CARTESIAN_POINT('Ctrl Pts',(76.1230727434158,-85.425,10.8018418550491));
#42708=CARTESIAN_POINT('Ctrl Pts',(75.8759733438492,-85.725,10.6038540005684));
#42709=CARTESIAN_POINT('Ctrl Pts',(75.8759733438492,-85.425,10.6038540005684));
#42710=CARTESIAN_POINT('',(76.6633197069168,-85.425,10.8018418550491));
#42711=CARTESIAN_POINT('',(76.6633197069168,-85.725,10.8018418550491));
#42712=CARTESIAN_POINT('Ctrl Pts',(76.6633197069168,-85.425,10.8018418550491));
#42713=CARTESIAN_POINT('Ctrl Pts',(76.1230727434158,-85.425,10.8018418550491));
#42714=CARTESIAN_POINT('Ctrl Pts',(75.8759733438492,-85.425,10.6038540005684));
#42715=CARTESIAN_POINT('Ctrl Pts',(77.4475952386856,-85.725,10.5839019417763));
#42716=CARTESIAN_POINT('Ctrl Pts',(77.4475952386856,-85.425,10.5839019417763));
#42717=CARTESIAN_POINT('Ctrl Pts',(77.1820780038834,-85.725,10.8018418550491));
#42718=CARTESIAN_POINT('Ctrl Pts',(77.1820780038834,-85.425,10.8018418550491));
#42719=CARTESIAN_POINT('Ctrl Pts',(76.6633197069168,-85.725,10.8018418550491));
#42720=CARTESIAN_POINT('Ctrl Pts',(76.6633197069168,-85.425,10.8018418550491));
#42721=CARTESIAN_POINT('',(77.4475952386856,-85.425,10.5839019417763));
#42722=CARTESIAN_POINT('',(77.4475952386856,-85.725,10.5839019417763));
#42723=CARTESIAN_POINT('Ctrl Pts',(77.4475952386856,-85.425,10.5839019417763));
#42724=CARTESIAN_POINT('Ctrl Pts',(77.1820780038834,-85.425,10.8018418550491));
#42725=CARTESIAN_POINT('Ctrl Pts',(76.6633197069168,-85.425,10.8018418550491));
#42726=CARTESIAN_POINT('Ctrl Pts',(77.7591582536697,-85.725,9.9392911195755));
#42727=CARTESIAN_POINT('Ctrl Pts',(77.7591582536697,-85.425,9.9392911195755));
#42728=CARTESIAN_POINT('Ctrl Pts',(77.7131148576736,-85.725,10.3659620285034));
#42729=CARTESIAN_POINT('Ctrl Pts',(77.7131148576736,-85.425,10.3659620285034));
#42730=CARTESIAN_POINT('Ctrl Pts',(77.4475952386856,-85.725,10.5839019417763));
#42731=CARTESIAN_POINT('Ctrl Pts',(77.4475952386856,-85.425,10.5839019417763));
#42732=CARTESIAN_POINT('',(77.7591582536697,-85.425,9.9392911195755));
#42733=CARTESIAN_POINT('',(77.7591582536697,-85.725,9.9392911195755));
#42734=CARTESIAN_POINT('Ctrl Pts',(77.7591582536697,-85.425,9.9392911195755));
#42735=CARTESIAN_POINT('Ctrl Pts',(77.7131148576736,-85.425,10.3659620285034));
#42736=CARTESIAN_POINT('Ctrl Pts',(77.4475952386856,-85.425,10.5839019417763));
#42737=CARTESIAN_POINT('Origin',(78.3300992250443,-85.725,9.98226487636566));
#42738=CARTESIAN_POINT('',(78.3300992250443,-85.425,9.98226487636566));
#42739=CARTESIAN_POINT('',(78.3300992250443,-85.725,9.98226487636566));
#42740=CARTESIAN_POINT('',(78.3300992250443,-85.425,9.98226487636566));
#42741=CARTESIAN_POINT('Ctrl Pts',(78.1090899705887,-85.725,10.6913369297981));
#42742=CARTESIAN_POINT('Ctrl Pts',(78.1090899705887,-85.425,10.6913369297981));
#42743=CARTESIAN_POINT('Ctrl Pts',(78.3147522211075,-85.725,10.3782402873039));
#42744=CARTESIAN_POINT('Ctrl Pts',(78.3147522211075,-85.425,10.3782402873039));
#42745=CARTESIAN_POINT('Ctrl Pts',(78.3300992250443,-85.725,9.98226487636566));
#42746=CARTESIAN_POINT('Ctrl Pts',(78.3300992250443,-85.425,9.98226487636566));
#42747=CARTESIAN_POINT('',(78.1090899705887,-85.425,10.6913369297981));
#42748=CARTESIAN_POINT('',(78.1090899705887,-85.725,10.6913369297981));
#42749=CARTESIAN_POINT('Ctrl Pts',(78.1090899705887,-85.425,10.6913369297981));
#42750=CARTESIAN_POINT('Ctrl Pts',(78.3147522211075,-85.425,10.3782402873039));
#42751=CARTESIAN_POINT('Ctrl Pts',(78.3300992250443,-85.425,9.98226487636566));
#42752=CARTESIAN_POINT('Ctrl Pts',(77.521266579628,-85.725,11.1655866503716));
#42753=CARTESIAN_POINT('Ctrl Pts',(77.521266579628,-85.425,11.1655866503716));
#42754=CARTESIAN_POINT('Ctrl Pts',(77.9034277200699,-85.725,11.0044338703156));
#42755=CARTESIAN_POINT('Ctrl Pts',(77.9034277200699,-85.425,11.0044338703156));
#42756=CARTESIAN_POINT('Ctrl Pts',(78.1090899705887,-85.725,10.6913369297981));
#42757=CARTESIAN_POINT('Ctrl Pts',(78.1090899705887,-85.425,10.6913369297981));
#42758=CARTESIAN_POINT('',(77.521266579628,-85.425,11.1655866503716));
#42759=CARTESIAN_POINT('',(77.521266579628,-85.725,11.1655866503716));
#42760=CARTESIAN_POINT('Ctrl Pts',(77.521266579628,-85.425,11.1655866503716));
#42761=CARTESIAN_POINT('Ctrl Pts',(77.9034277200699,-85.425,11.0044338703156));
#42762=CARTESIAN_POINT('Ctrl Pts',(78.1090899705887,-85.425,10.6913369297981));
#42763=CARTESIAN_POINT('Ctrl Pts',(76.6387625932693,-85.725,11.3267394304276));
#42764=CARTESIAN_POINT('Ctrl Pts',(76.6387625932693,-85.425,11.3267394304276));
#42765=CARTESIAN_POINT('Ctrl Pts',(77.1391030550003,-85.725,11.3267394304276));
#42766=CARTESIAN_POINT('Ctrl Pts',(77.1391030550003,-85.425,11.3267394304276));
#42767=CARTESIAN_POINT('Ctrl Pts',(77.521266579628,-85.725,11.1655866503716));
#42768=CARTESIAN_POINT('Ctrl Pts',(77.521266579628,-85.425,11.1655866503716));
#42769=CARTESIAN_POINT('',(76.6387625932693,-85.425,11.3267394304276));
#42770=CARTESIAN_POINT('',(76.6387625932693,-85.725,11.3267394304276));
#42771=CARTESIAN_POINT('Ctrl Pts',(76.6387625932693,-85.425,11.3267394304276));
#42772=CARTESIAN_POINT('Ctrl Pts',(77.1391030550003,-85.425,11.3267394304276));
#42773=CARTESIAN_POINT('Ctrl Pts',(77.521266579628,-85.425,11.1655866503716));
#42774=CARTESIAN_POINT('Ctrl Pts',(75.8130475282669,-85.725,11.1732607483864));
#42775=CARTESIAN_POINT('Ctrl Pts',(75.8130475282669,-85.425,11.1732607483864));
#42776=CARTESIAN_POINT('Ctrl Pts',(76.1844655275345,-85.725,11.3267394304276));
#42777=CARTESIAN_POINT('Ctrl Pts',(76.1844655275345,-85.425,11.3267394304276));
#42778=CARTESIAN_POINT('Ctrl Pts',(76.6387625932693,-85.725,11.3267394304276));
#42779=CARTESIAN_POINT('Ctrl Pts',(76.6387625932693,-85.425,11.3267394304276));
#42780=CARTESIAN_POINT('',(75.8130475282669,-85.425,11.1732607483864));
#42781=CARTESIAN_POINT('',(75.8130475282669,-85.725,11.1732607483864));
#42782=CARTESIAN_POINT('Ctrl Pts',(75.8130475282669,-85.425,11.1732607483864));
#42783=CARTESIAN_POINT('Ctrl Pts',(76.1844655275345,-85.425,11.3267394304276));
#42784=CARTESIAN_POINT('Ctrl Pts',(76.6387625932693,-85.425,11.3267394304276));
#42785=CARTESIAN_POINT('Ctrl Pts',(75.2482434511185,-85.725,10.723567545414));
#42786=CARTESIAN_POINT('Ctrl Pts',(75.2482434511185,-85.425,10.723567545414));
#42787=CARTESIAN_POINT('Ctrl Pts',(75.4416271448135,-85.725,11.019781768322));
#42788=CARTESIAN_POINT('Ctrl Pts',(75.4416271448135,-85.425,11.019781768322));
#42789=CARTESIAN_POINT('Ctrl Pts',(75.8130475282669,-85.725,11.1732607483864));
#42790=CARTESIAN_POINT('Ctrl Pts',(75.8130475282669,-85.425,11.1732607483864));
#42791=CARTESIAN_POINT('',(75.2482434511185,-85.425,10.723567545414));
#42792=CARTESIAN_POINT('',(75.2482434511185,-85.725,10.723567545414));
#42793=CARTESIAN_POINT('Ctrl Pts',(75.2482434511185,-85.425,10.723567545414));
#42794=CARTESIAN_POINT('Ctrl Pts',(75.4416271448135,-85.425,11.019781768322));
#42795=CARTESIAN_POINT('Ctrl Pts',(75.8130475282669,-85.425,11.1732607483864));
#42796=CARTESIAN_POINT('Ctrl Pts',(75.0548621416092,-85.725,10.0866302251816));
#42797=CARTESIAN_POINT('Ctrl Pts',(75.0548621416092,-85.425,10.0866302251816));
#42798=CARTESIAN_POINT('Ctrl Pts',(75.0548621416092,-85.725,10.427353322506));
#42799=CARTESIAN_POINT('Ctrl Pts',(75.0548621416092,-85.425,10.427353322506));
#42800=CARTESIAN_POINT('Ctrl Pts',(75.2482434511185,-85.725,10.723567545414));
#42801=CARTESIAN_POINT('Ctrl Pts',(75.2482434511185,-85.425,10.723567545414));
#42802=CARTESIAN_POINT('',(75.0548621416092,-85.425,10.0866302251816));
#42803=CARTESIAN_POINT('',(75.0548621416092,-85.725,10.0866302251816));
#42804=CARTESIAN_POINT('Ctrl Pts',(75.0548621416092,-85.425,10.0866302251816));
#42805=CARTESIAN_POINT('Ctrl Pts',(75.0548621416092,-85.425,10.427353322506));
#42806=CARTESIAN_POINT('Ctrl Pts',(75.2482434511185,-85.425,10.723567545414));
#42807=CARTESIAN_POINT('Ctrl Pts',(75.2129431962967,-85.725,9.52643239498138));
#42808=CARTESIAN_POINT('Ctrl Pts',(75.2129431962967,-85.425,9.52643239498138));
#42809=CARTESIAN_POINT('Ctrl Pts',(75.0548621416092,-85.725,9.77660322189331));
#42810=CARTESIAN_POINT('Ctrl Pts',(75.0548621416092,-85.425,9.77660322189331));
#42811=CARTESIAN_POINT('Ctrl Pts',(75.0548621416092,-85.725,10.0866302251816));
#42812=CARTESIAN_POINT('Ctrl Pts',(75.0548621416092,-85.425,10.0866302251816));
#42813=CARTESIAN_POINT('',(75.2129431962967,-85.425,9.52643239498138));
#42814=CARTESIAN_POINT('',(75.2129431962967,-85.725,9.52643239498138));
#42815=CARTESIAN_POINT('Ctrl Pts',(75.2129431962967,-85.425,9.52643239498138));
#42816=CARTESIAN_POINT('Ctrl Pts',(75.0548621416092,-85.425,9.77660322189331));
#42817=CARTESIAN_POINT('Ctrl Pts',(75.0548621416092,-85.425,10.0866302251816));
#42818=CARTESIAN_POINT('Ctrl Pts',(75.6933327913284,-85.725,9.1074355840683));
#42819=CARTESIAN_POINT('Ctrl Pts',(75.6933327913284,-85.425,9.1074355840683));
#42820=CARTESIAN_POINT('Ctrl Pts',(75.37102663517,-85.725,9.27626216411591));
#42821=CARTESIAN_POINT('Ctrl Pts',(75.37102663517,-85.425,9.27626216411591));
#42822=CARTESIAN_POINT('Ctrl Pts',(75.2129431962967,-85.725,9.52643239498138));
#42823=CARTESIAN_POINT('Ctrl Pts',(75.2129431962967,-85.425,9.52643239498138));
#42824=CARTESIAN_POINT('',(75.6933327913284,-85.425,9.1074355840683));
#42825=CARTESIAN_POINT('',(75.6933327913284,-85.725,9.1074355840683));
#42826=CARTESIAN_POINT('Ctrl Pts',(75.6933327913284,-85.425,9.1074355840683));
#42827=CARTESIAN_POINT('Ctrl Pts',(75.37102663517,-85.425,9.27626216411591));
#42828=CARTESIAN_POINT('Ctrl Pts',(75.2129431962967,-85.425,9.52643239498138));
#42829=CARTESIAN_POINT('Ctrl Pts',(76.5620228052139,-85.725,8.82656896114349));
#42830=CARTESIAN_POINT('Ctrl Pts',(76.5620228052139,-85.425,8.82656896114349));
#42831=CARTESIAN_POINT('Ctrl Pts',(75.9419699907303,-85.725,8.97544348239899));
#42832=CARTESIAN_POINT('Ctrl Pts',(75.9419699907303,-85.425,8.97544348239899));
#42833=CARTESIAN_POINT('Ctrl Pts',(75.6933327913284,-85.725,9.1074355840683));
#42834=CARTESIAN_POINT('Ctrl Pts',(75.6933327913284,-85.425,9.1074355840683));
#42835=CARTESIAN_POINT('',(76.5620228052139,-85.425,8.82656896114349));
#42836=CARTESIAN_POINT('',(76.5620228052139,-85.725,8.82656896114349));
#42837=CARTESIAN_POINT('Ctrl Pts',(76.5620228052139,-85.425,8.82656896114349));
#42838=CARTESIAN_POINT('Ctrl Pts',(75.9419699907303,-85.425,8.97544348239899));
#42839=CARTESIAN_POINT('Ctrl Pts',(75.6933327913284,-85.425,9.1074355840683));
#42840=CARTESIAN_POINT('Ctrl Pts',(77.3631831407547,-85.725,8.60709452629089));
#42841=CARTESIAN_POINT('Ctrl Pts',(77.3631831407547,-85.425,8.60709452629089));
#42842=CARTESIAN_POINT('Ctrl Pts',(77.1820780038834,-85.725,8.677694439888));
#42843=CARTESIAN_POINT('Ctrl Pts',(77.1820780038834,-85.425,8.677694439888));
#42844=CARTESIAN_POINT('Ctrl Pts',(76.5620228052139,-85.725,8.82656896114349));
#42845=CARTESIAN_POINT('Ctrl Pts',(76.5620228052139,-85.425,8.82656896114349));
#42846=CARTESIAN_POINT('',(77.3631831407547,-85.425,8.60709452629089));
#42847=CARTESIAN_POINT('',(77.3631831407547,-85.725,8.60709452629089));
#42848=CARTESIAN_POINT('Ctrl Pts',(77.3631831407547,-85.425,8.60709452629089));
#42849=CARTESIAN_POINT('Ctrl Pts',(77.1820780038834,-85.425,8.677694439888));
#42850=CARTESIAN_POINT('Ctrl Pts',(76.5620228052139,-85.425,8.82656896114349));
#42851=CARTESIAN_POINT('Ctrl Pts',(77.7683659791946,-85.725,8.34157609939575));
#42852=CARTESIAN_POINT('Ctrl Pts',(77.7683659791946,-85.425,8.34157609939575));
#42853=CARTESIAN_POINT('Ctrl Pts',(77.6455851793289,-85.725,8.4996589422226));
#42854=CARTESIAN_POINT('Ctrl Pts',(77.6455851793289,-85.425,8.4996589422226));
#42855=CARTESIAN_POINT('Ctrl Pts',(77.3631831407547,-85.725,8.60709452629089));
#42856=CARTESIAN_POINT('Ctrl Pts',(77.3631831407547,-85.425,8.60709452629089));
#42857=CARTESIAN_POINT('',(77.7683659791946,-85.425,8.34157609939575));
#42858=CARTESIAN_POINT('',(77.7683659791946,-85.725,8.34157609939575));
#42859=CARTESIAN_POINT('Ctrl Pts',(77.7683659791946,-85.425,8.34157609939575));
#42860=CARTESIAN_POINT('Ctrl Pts',(77.6455851793289,-85.425,8.4996589422226));
#42861=CARTESIAN_POINT('Ctrl Pts',(77.3631831407547,-85.425,8.60709452629089));
#42862=CARTESIAN_POINT('Ctrl Pts',(77.8911491632462,-85.725,7.97169172763824));
#42863=CARTESIAN_POINT('Ctrl Pts',(77.8911491632462,-85.425,7.97169172763824));
#42864=CARTESIAN_POINT('Ctrl Pts',(77.8911491632462,-85.725,8.18349266052246));
#42865=CARTESIAN_POINT('Ctrl Pts',(77.8911491632462,-85.425,8.18349266052246));
#42866=CARTESIAN_POINT('Ctrl Pts',(77.7683659791946,-85.725,8.34157609939575));
#42867=CARTESIAN_POINT('Ctrl Pts',(77.7683659791946,-85.425,8.34157609939575));
#42868=CARTESIAN_POINT('',(77.8911491632462,-85.425,7.97169172763824));
#42869=CARTESIAN_POINT('',(77.8911491632462,-85.725,7.97169172763824));
#42870=CARTESIAN_POINT('Ctrl Pts',(77.8911491632462,-85.425,7.97169172763824));
#42871=CARTESIAN_POINT('Ctrl Pts',(77.8911491632462,-85.425,8.18349266052246));
#42872=CARTESIAN_POINT('Ctrl Pts',(77.7683659791946,-85.425,8.34157609939575));
#42873=CARTESIAN_POINT('Ctrl Pts',(77.7637621164322,-85.725,7.58645975589752));
#42874=CARTESIAN_POINT('Ctrl Pts',(77.7637621164322,-85.425,7.58645975589752));
#42875=CARTESIAN_POINT('Ctrl Pts',(77.8911491632462,-85.725,7.76296103000641));
#42876=CARTESIAN_POINT('Ctrl Pts',(77.8911491632462,-85.425,7.76296103000641));
#42877=CARTESIAN_POINT('Ctrl Pts',(77.8911491632462,-85.725,7.97169172763824));
#42878=CARTESIAN_POINT('Ctrl Pts',(77.8911491632462,-85.425,7.97169172763824));
#42879=CARTESIAN_POINT('',(77.7637621164322,-85.425,7.58645975589752));
#42880=CARTESIAN_POINT('',(77.7637621164322,-85.725,7.58645975589752));
#42881=CARTESIAN_POINT('Ctrl Pts',(77.7637621164322,-85.425,7.58645975589752));
#42882=CARTESIAN_POINT('Ctrl Pts',(77.8911491632462,-85.425,7.76296103000641));
#42883=CARTESIAN_POINT('Ctrl Pts',(77.8911491632462,-85.425,7.97169172763824));
#42884=CARTESIAN_POINT('Ctrl Pts',(77.3754616975784,-85.725,7.3086633682251));
#42885=CARTESIAN_POINT('Ctrl Pts',(77.3754616975784,-85.425,7.3086633682251));
#42886=CARTESIAN_POINT('Ctrl Pts',(77.6363750696182,-85.725,7.40995967388153));
#42887=CARTESIAN_POINT('Ctrl Pts',(77.6363750696182,-85.425,7.40995967388153));
#42888=CARTESIAN_POINT('Ctrl Pts',(77.7637621164322,-85.725,7.58645975589752));
#42889=CARTESIAN_POINT('Ctrl Pts',(77.7637621164322,-85.425,7.58645975589752));
#42890=CARTESIAN_POINT('',(77.3754616975784,-85.425,7.3086633682251));
#42891=CARTESIAN_POINT('',(77.3754616975784,-85.725,7.3086633682251));
#42892=CARTESIAN_POINT('Ctrl Pts',(77.3754616975784,-85.425,7.3086633682251));
#42893=CARTESIAN_POINT('Ctrl Pts',(77.6363750696182,-85.425,7.40995967388153));
#42894=CARTESIAN_POINT('Ctrl Pts',(77.7637621164322,-85.425,7.58645975589752));
#42895=CARTESIAN_POINT('Ctrl Pts',(76.7738243341446,-85.725,7.20736706256866));
#42896=CARTESIAN_POINT('Ctrl Pts',(76.7738243341446,-85.425,7.20736706256866));
#42897=CARTESIAN_POINT('Ctrl Pts',(77.1145459413528,-85.725,7.20736706256866));
#42898=CARTESIAN_POINT('Ctrl Pts',(77.1145459413528,-85.425,7.20736706256866));
#42899=CARTESIAN_POINT('Ctrl Pts',(77.3754616975784,-85.725,7.3086633682251));
#42900=CARTESIAN_POINT('Ctrl Pts',(77.3754616975784,-85.425,7.3086633682251));
#42901=CARTESIAN_POINT('',(76.7738243341446,-85.425,7.20736706256866));
#42902=CARTESIAN_POINT('',(76.7738243341446,-85.725,7.20736706256866));
#42903=CARTESIAN_POINT('Ctrl Pts',(76.7738243341446,-85.425,7.20736706256866));
#42904=CARTESIAN_POINT('Ctrl Pts',(77.1145459413528,-85.425,7.20736706256866));
#42905=CARTESIAN_POINT('Ctrl Pts',(77.3754616975784,-85.425,7.3086633682251));
#42906=CARTESIAN_POINT('Ctrl Pts',(76.0831686258316,-85.725,7.34089398384094));
#42907=CARTESIAN_POINT('Ctrl Pts',(76.0831686258316,-85.425,7.34089398384094));
#42908=CARTESIAN_POINT('Ctrl Pts',(76.3901277780533,-85.725,7.20736706256866));
#42909=CARTESIAN_POINT('Ctrl Pts',(76.3901277780533,-85.425,7.20736706256866));
#42910=CARTESIAN_POINT('Ctrl Pts',(76.7738243341446,-85.725,7.20736706256866));
#42911=CARTESIAN_POINT('Ctrl Pts',(76.7738243341446,-85.425,7.20736706256866));
#42912=CARTESIAN_POINT('',(76.0831686258316,-85.425,7.34089398384094));
#42913=CARTESIAN_POINT('',(76.0831686258316,-85.725,7.34089398384094));
#42914=CARTESIAN_POINT('Ctrl Pts',(76.0831686258316,-85.425,7.34089398384094));
#42915=CARTESIAN_POINT('Ctrl Pts',(76.3901277780533,-85.425,7.20736706256866));
#42916=CARTESIAN_POINT('Ctrl Pts',(76.7738243341446,-85.425,7.20736706256866));
#42917=CARTESIAN_POINT('Ctrl Pts',(75.6304069757462,-85.725,7.69082570075989));
#42918=CARTESIAN_POINT('Ctrl Pts',(75.6304069757462,-85.425,7.69082570075989));
#42919=CARTESIAN_POINT('Ctrl Pts',(75.7762118577957,-85.725,7.47442030906677));
#42920=CARTESIAN_POINT('Ctrl Pts',(75.7762118577957,-85.425,7.47442030906677));
#42921=CARTESIAN_POINT('Ctrl Pts',(76.0831686258316,-85.725,7.34089398384094));
#42922=CARTESIAN_POINT('Ctrl Pts',(76.0831686258316,-85.425,7.34089398384094));
#42923=CARTESIAN_POINT('',(75.6304069757462,-85.425,7.69082570075989));
#42924=CARTESIAN_POINT('',(75.6304069757462,-85.725,7.69082570075989));
#42925=CARTESIAN_POINT('Ctrl Pts',(75.6304069757462,-85.425,7.69082570075989));
#42926=CARTESIAN_POINT('Ctrl Pts',(75.7762118577957,-85.425,7.47442030906677));
#42927=CARTESIAN_POINT('Ctrl Pts',(76.0831686258316,-85.425,7.34089398384094));
#42928=CARTESIAN_POINT('Ctrl Pts',(75.4446979761124,-85.725,8.24488425254822));
#42929=CARTESIAN_POINT('Ctrl Pts',(75.4446979761124,-85.425,8.24488425254822));
#42930=CARTESIAN_POINT('Ctrl Pts',(75.4846020936966,-85.725,7.907231092453));
#42931=CARTESIAN_POINT('Ctrl Pts',(75.4846020936966,-85.425,7.907231092453));
#42932=CARTESIAN_POINT('Ctrl Pts',(75.6304069757462,-85.725,7.69082570075989));
#42933=CARTESIAN_POINT('Ctrl Pts',(75.6304069757462,-85.425,7.69082570075989));
#42934=CARTESIAN_POINT('',(75.4446979761124,-85.425,8.24488425254822));
#42935=CARTESIAN_POINT('',(75.4446979761124,-85.725,8.24488425254822));
#42936=CARTESIAN_POINT('Ctrl Pts',(75.4446979761124,-85.425,8.24488425254822));
#42937=CARTESIAN_POINT('Ctrl Pts',(75.4846020936966,-85.425,7.907231092453));
#42938=CARTESIAN_POINT('Ctrl Pts',(75.6304069757462,-85.425,7.69082570075989));
#42939=CARTESIAN_POINT('Origin',(74.8829647302628,-85.725,8.19577121734619));
#42940=CARTESIAN_POINT('',(74.8829647302628,-85.425,8.19577121734619));
#42941=CARTESIAN_POINT('',(74.8829647302628,-85.725,8.19577121734619));
#42942=CARTESIAN_POINT('',(74.8829647302628,-85.425,8.19577121734619));
#42943=CARTESIAN_POINT('Ctrl Pts',(75.1300665140152,-85.725,7.38693737983704));
#42944=CARTESIAN_POINT('Ctrl Pts',(75.1300665140152,-85.425,7.38693737983704));
#42945=CARTESIAN_POINT('Ctrl Pts',(74.8952432870865,-85.725,7.74454319477081));
#42946=CARTESIAN_POINT('Ctrl Pts',(74.8952432870865,-85.425,7.74454319477081));
#42947=CARTESIAN_POINT('Ctrl Pts',(74.8829647302628,-85.725,8.19577121734619));
#42948=CARTESIAN_POINT('Ctrl Pts',(74.8829647302628,-85.425,8.19577121734619));
#42949=CARTESIAN_POINT('',(75.1300665140152,-85.425,7.38693737983704));
#42950=CARTESIAN_POINT('',(75.1300665140152,-85.725,7.38693737983704));
#42951=CARTESIAN_POINT('Ctrl Pts',(75.1300665140152,-85.425,7.38693737983704));
#42952=CARTESIAN_POINT('Ctrl Pts',(74.8952432870865,-85.425,7.74454319477081));
#42953=CARTESIAN_POINT('Ctrl Pts',(74.8829647302628,-85.425,8.19577121734619));
#42954=CARTESIAN_POINT('Ctrl Pts',(75.7777472734451,-85.725,6.8512966632843));
#42955=CARTESIAN_POINT('Ctrl Pts',(75.7777472734451,-85.425,6.8512966632843));
#42956=CARTESIAN_POINT('Ctrl Pts',(75.3648873567581,-85.725,7.02933156490326));
#42957=CARTESIAN_POINT('Ctrl Pts',(75.3648873567581,-85.425,7.02933156490326));
#42958=CARTESIAN_POINT('Ctrl Pts',(75.1300665140152,-85.725,7.38693737983704));
#42959=CARTESIAN_POINT('Ctrl Pts',(75.1300665140152,-85.425,7.38693737983704));
#42960=CARTESIAN_POINT('Ctrl Pts',(75.7777472734451,-85.425,6.8512966632843));
#42961=CARTESIAN_POINT('Ctrl Pts',(75.3648873567581,-85.425,7.02933156490326));
#42962=CARTESIAN_POINT('Ctrl Pts',(75.1300665140152,-85.425,7.38693737983704));
#42963=CARTESIAN_POINT('Origin',(76.6740628480911,-85.425,9.00000029802322));
#42964=CARTESIAN_POINT('Origin',(0.,0.,0.2));
#42965=CARTESIAN_POINT('',(-4.05,-4.95981953654678E-16,0.4));
#42966=CARTESIAN_POINT('',(-4.25,5.20474889637625E-16,0.2));
#42967=CARTESIAN_POINT('Origin',(0.,0.,0.4));
#42968=CARTESIAN_POINT('Origin',(0.,0.,19.05));
#42969=CARTESIAN_POINT('',(-4.05,-4.95981953654678E-16,17.35));
#42970=CARTESIAN_POINT('Origin',(0.,0.,17.35));
#42971=CARTESIAN_POINT('',(-4.05,4.95981953654678E-16,19.05));
#42972=CARTESIAN_POINT('Origin',(56.25,-78.,18.85));
#42973=CARTESIAN_POINT('',(53.2,-78.,18.65));
#42974=CARTESIAN_POINT('',(53.,-78.,18.85));
#42975=CARTESIAN_POINT('Origin',(56.25,-78.,18.65));
#42976=CARTESIAN_POINT('Origin',(56.25,-78.,19.05));
#42977=CARTESIAN_POINT('',(53.2,-78.,7.05));
#42978=CARTESIAN_POINT('',(53.2,-78.,19.05));
#42979=CARTESIAN_POINT('Origin',(56.25,-78.,7.05));
#42980=CARTESIAN_POINT('Origin',(-78.,56.25,18.85));
#42981=CARTESIAN_POINT('',(-81.05,56.25,18.65));
#42982=CARTESIAN_POINT('',(-81.25,56.25,18.85));
#42983=CARTESIAN_POINT('Origin',(-78.,56.25,18.65));
#42984=CARTESIAN_POINT('Origin',(-78.,56.25,19.05));
#42985=CARTESIAN_POINT('',(-81.05,56.25,7.05));
#42986=CARTESIAN_POINT('',(-81.05,56.25,19.05));
#42987=CARTESIAN_POINT('Origin',(-78.,56.25,7.05));
#42988=CARTESIAN_POINT('Origin',(18.75,78.,18.85));
#42989=CARTESIAN_POINT('',(15.7,78.,18.65));
#42990=CARTESIAN_POINT('',(15.5,78.,18.85));
#42991=CARTESIAN_POINT('Origin',(18.75,78.,18.65));
#42992=CARTESIAN_POINT('Origin',(18.75,78.,19.05));
#42993=CARTESIAN_POINT('',(15.7,78.,7.05));
#42994=CARTESIAN_POINT('',(15.7,78.,19.05));
#42995=CARTESIAN_POINT('Origin',(18.75,78.,7.05));
#42996=CARTESIAN_POINT('Origin',(78.,-56.25,18.85));
#42997=CARTESIAN_POINT('',(74.95,-56.25,18.65));
#42998=CARTESIAN_POINT('',(74.75,-56.25,18.85));
#42999=CARTESIAN_POINT('Origin',(78.,-56.25,18.65));
#43000=CARTESIAN_POINT('Origin',(78.,-56.25,19.05));
#43001=CARTESIAN_POINT('',(74.95,-56.25,7.05));
#43002=CARTESIAN_POINT('',(74.95,-56.25,19.05));
#43003=CARTESIAN_POINT('Origin',(78.,-56.25,7.05));
#43004=CARTESIAN_POINT('Origin',(-18.75,78.,18.85));
#43005=CARTESIAN_POINT('',(-21.8,78.,18.65));
#43006=CARTESIAN_POINT('',(-22.,78.,18.85));
#43007=CARTESIAN_POINT('Origin',(-18.75,78.,18.65));
#43008=CARTESIAN_POINT('Origin',(-18.75,78.,19.05));
#43009=CARTESIAN_POINT('',(-21.8,78.,7.05));
#43010=CARTESIAN_POINT('',(-21.8,78.,19.05));
#43011=CARTESIAN_POINT('Origin',(-18.75,78.,7.05));
#43012=CARTESIAN_POINT('Origin',(78.,-18.75,18.85));
#43013=CARTESIAN_POINT('',(74.95,-18.75,18.65));
#43014=CARTESIAN_POINT('',(74.75,-18.75,18.85));
#43015=CARTESIAN_POINT('Origin',(78.,-18.75,18.65));
#43016=CARTESIAN_POINT('Origin',(78.,-18.75,19.05));
#43017=CARTESIAN_POINT('',(74.95,-18.75,7.05));
#43018=CARTESIAN_POINT('',(74.95,-18.75,19.05));
#43019=CARTESIAN_POINT('Origin',(78.,-18.75,7.05));
#43020=CARTESIAN_POINT('Origin',(-56.25,78.,18.85));
#43021=CARTESIAN_POINT('',(-59.3,78.,18.65));
#43022=CARTESIAN_POINT('',(-59.5,78.,18.85));
#43023=CARTESIAN_POINT('Origin',(-56.25,78.,18.65));
#43024=CARTESIAN_POINT('Origin',(-56.25,78.,19.05));
#43025=CARTESIAN_POINT('',(-59.3,78.,7.05));
#43026=CARTESIAN_POINT('',(-59.3,78.,19.05));
#43027=CARTESIAN_POINT('Origin',(-56.25,78.,7.05));
#43028=CARTESIAN_POINT('Origin',(-78.,-18.75,18.85));
#43029=CARTESIAN_POINT('',(-81.05,-18.75,18.65));
#43030=CARTESIAN_POINT('',(-81.25,-18.75,18.85));
#43031=CARTESIAN_POINT('Origin',(-78.,-18.75,18.65));
#43032=CARTESIAN_POINT('Origin',(-78.,-18.75,19.05));
#43033=CARTESIAN_POINT('',(-81.05,-18.75,7.05));
#43034=CARTESIAN_POINT('',(-81.05,-18.75,19.05));
#43035=CARTESIAN_POINT('Origin',(-78.,-18.75,7.05));
#43036=CARTESIAN_POINT('Origin',(78.,18.75,18.85));
#43037=CARTESIAN_POINT('',(74.95,18.75,18.65));
#43038=CARTESIAN_POINT('',(74.75,18.75,18.85));
#43039=CARTESIAN_POINT('Origin',(78.,18.75,18.65));
#43040=CARTESIAN_POINT('Origin',(78.,18.75,19.05));
#43041=CARTESIAN_POINT('',(74.95,18.75,7.05));
#43042=CARTESIAN_POINT('',(74.95,18.75,19.05));
#43043=CARTESIAN_POINT('Origin',(78.,18.75,7.05));
#43044=CARTESIAN_POINT('Origin',(-78.,18.75,18.85));
#43045=CARTESIAN_POINT('',(-81.05,18.75,18.65));
#43046=CARTESIAN_POINT('',(-81.25,18.75,18.85));
#43047=CARTESIAN_POINT('Origin',(-78.,18.75,18.65));
#43048=CARTESIAN_POINT('Origin',(-78.,18.75,19.05));
#43049=CARTESIAN_POINT('',(-81.05,18.75,7.05));
#43050=CARTESIAN_POINT('',(-81.05,18.75,19.05));
#43051=CARTESIAN_POINT('Origin',(-78.,18.75,7.05));
#43052=CARTESIAN_POINT('Origin',(78.,56.25,18.85));
#43053=CARTESIAN_POINT('',(74.95,56.25,18.65));
#43054=CARTESIAN_POINT('',(74.75,56.25,18.85));
#43055=CARTESIAN_POINT('Origin',(78.,56.25,18.65));
#43056=CARTESIAN_POINT('Origin',(78.,56.25,19.05));
#43057=CARTESIAN_POINT('',(74.95,56.25,7.05));
#43058=CARTESIAN_POINT('',(74.95,56.25,19.05));
#43059=CARTESIAN_POINT('Origin',(78.,56.25,7.05));
#43060=CARTESIAN_POINT('Origin',(56.25,78.,18.85));
#43061=CARTESIAN_POINT('',(53.2,78.,18.65));
#43062=CARTESIAN_POINT('',(53.,78.,18.85));
#43063=CARTESIAN_POINT('Origin',(56.25,78.,18.65));
#43064=CARTESIAN_POINT('Origin',(56.25,78.,19.05));
#43065=CARTESIAN_POINT('',(53.2,78.,7.05));
#43066=CARTESIAN_POINT('',(53.2,78.,19.05));
#43067=CARTESIAN_POINT('Origin',(56.25,78.,7.05));
#43068=CARTESIAN_POINT('Origin',(0.,-37.5,18.85));
#43069=CARTESIAN_POINT('',(-7.,-37.5,18.65));
#43070=CARTESIAN_POINT('',(-7.2,-37.5,18.85));
#43071=CARTESIAN_POINT('Origin',(0.,-37.5,18.65));
#43072=CARTESIAN_POINT('Origin',(0.,-37.5,19.05));
#43073=CARTESIAN_POINT('',(-7.,-37.5,19.05));
#43074=CARTESIAN_POINT('Origin',(37.5,0.,18.85));
#43075=CARTESIAN_POINT('',(30.5,8.57252759403147E-16,18.65));
#43076=CARTESIAN_POINT('',(30.3,-8.81745695386095E-16,18.85));
#43077=CARTESIAN_POINT('Origin',(37.5,0.,18.65));
#43078=CARTESIAN_POINT('Origin',(37.5,0.,19.05));
#43079=CARTESIAN_POINT('',(30.5,8.57252759403147E-16,19.05));
#43080=CARTESIAN_POINT('Origin',(-37.5,0.,18.85));
#43081=CARTESIAN_POINT('',(-44.5,8.57252759403147E-16,18.65));
#43082=CARTESIAN_POINT('',(-44.7,-8.81745695386095E-16,18.85));
#43083=CARTESIAN_POINT('Origin',(-37.5,0.,18.65));
#43084=CARTESIAN_POINT('Origin',(-37.5,0.,19.05));
#43085=CARTESIAN_POINT('',(-44.5,8.57252759403147E-16,19.05));
#43086=CARTESIAN_POINT('Origin',(0.,37.5,18.85));
#43087=CARTESIAN_POINT('',(-7.,37.5,18.65));
#43088=CARTESIAN_POINT('',(-7.2,37.5,18.85));
#43089=CARTESIAN_POINT('Origin',(0.,37.5,18.65));
#43090=CARTESIAN_POINT('Origin',(0.,37.5,19.05));
#43091=CARTESIAN_POINT('',(-7.,37.5,19.05));
#43092=CARTESIAN_POINT('Origin',(0.,-37.5,0.2));
#43093=CARTESIAN_POINT('',(-4.7,-37.5,0.2));
#43094=CARTESIAN_POINT('Origin',(37.5,0.,0.2));
#43095=CARTESIAN_POINT('',(32.8,5.75583995599256E-16,0.2));
#43096=CARTESIAN_POINT('Origin',(-37.5,0.,0.2));
#43097=CARTESIAN_POINT('',(-42.2,5.75583995599256E-16,0.2));
#43098=CARTESIAN_POINT('Origin',(0.,37.5,0.2));
#43099=CARTESIAN_POINT('',(-4.7,37.5,0.2));
#43100=CARTESIAN_POINT('Origin',(-33.475,-35.725,3.75));
#43101=CARTESIAN_POINT('Origin',(-33.475,-35.725,10.75));
#43102=CARTESIAN_POINT('Origin',(56.25,78.,7.05));
#43103=CARTESIAN_POINT('Origin',(78.,56.25,7.05));
#43104=CARTESIAN_POINT('Origin',(-78.,18.75,7.05));
#43105=CARTESIAN_POINT('Origin',(78.,18.75,7.05));
#43106=CARTESIAN_POINT('Origin',(-78.,-18.75,7.05));
#43107=CARTESIAN_POINT('Origin',(-56.25,78.,7.05));
#43108=CARTESIAN_POINT('Origin',(78.,-18.75,7.05));
#43109=CARTESIAN_POINT('Origin',(-18.75,78.,7.05));
#43110=CARTESIAN_POINT('Origin',(78.,-56.25,7.05));
#43111=CARTESIAN_POINT('Origin',(18.75,78.,7.05));
#43112=CARTESIAN_POINT('Origin',(-78.,56.25,7.05));
#43113=CARTESIAN_POINT('Origin',(56.25,-78.,7.05));
#43114=CARTESIAN_POINT('Origin',(0.,0.,19.05));
#43115=CARTESIAN_POINT('',(-5.5,-6.73555739531044E-16,17.35));
#43116=CARTESIAN_POINT('',(-5.5,6.73555739531044E-16,19.05));
#43117=CARTESIAN_POINT('Origin',(0.,0.,17.35));
#43118=CARTESIAN_POINT('Origin',(0.,0.,17.35));
#43119=CARTESIAN_POINT('Origin',(85.725,85.725,0.));
#43120=CARTESIAN_POINT('',(0.,0.,0.));
#43121=CARTESIAN_POINT('Origin',(-56.25,18.75,29.075));
#43122=CARTESIAN_POINT('',(-58.8,18.75,29.325));
#43123=CARTESIAN_POINT('Origin',(-56.25,18.75,29.325));
#43124=CARTESIAN_POINT('',(-58.3,18.75,28.825));
#43125=CARTESIAN_POINT('',(-58.55,18.75,29.075));
#43126=CARTESIAN_POINT('Origin',(-56.25,18.75,28.825));
#43127=CARTESIAN_POINT('Origin',(0.,0.,29.325));
#43128=CARTESIAN_POINT('',(-54.5,-58.,29.325));
#43129=CARTESIAN_POINT('',(-54.5,-82.5,29.325));
#43130=CARTESIAN_POINT('',(-54.5,-35.,29.325));
#43131=CARTESIAN_POINT('',(-49.,-58.,29.325));
#43132=CARTESIAN_POINT('',(-27.,-58.,29.325));
#43133=CARTESIAN_POINT('',(-46.5,-55.5,29.325));
#43134=CARTESIAN_POINT('Origin',(-49.,-55.5,29.325));
#43135=CARTESIAN_POINT('',(-46.5,-43.,29.325));
#43136=CARTESIAN_POINT('',(-46.5,-29.25,29.325));
#43137=CARTESIAN_POINT('',(-43.,-39.5,29.325));
#43138=CARTESIAN_POINT('Origin',(-43.,-43.,29.325));
#43139=CARTESIAN_POINT('',(-12.3389626792531,-39.5,29.325));
#43140=CARTESIAN_POINT('',(-23.,-39.5,29.325));
#43141=CARTESIAN_POINT('',(12.3389626792531,-39.5,29.325));
#43142=CARTESIAN_POINT('Origin',(0.,-37.5,29.325));
#43143=CARTESIAN_POINT('',(39.,-39.5,29.325));
#43144=CARTESIAN_POINT('',(-23.,-39.5,29.325));
#43145=CARTESIAN_POINT('',(42.5,-43.,29.325));
#43146=CARTESIAN_POINT('Origin',(39.,-43.,29.325));
#43147=CARTESIAN_POINT('',(42.5,-67.,29.325));
#43148=CARTESIAN_POINT('',(42.5,-20.,29.325));
#43149=CARTESIAN_POINT('',(45.,-69.5,29.325));
#43150=CARTESIAN_POINT('Origin',(45.,-67.,29.325));
#43151=CARTESIAN_POINT('',(67.,-69.5,29.325));
#43152=CARTESIAN_POINT('',(21.,-69.5,29.325));
#43153=CARTESIAN_POINT('',(69.5,-67.,29.325));
#43154=CARTESIAN_POINT('Origin',(67.,-67.,29.325));
#43155=CARTESIAN_POINT('',(69.5,67.,29.325));
#43156=CARTESIAN_POINT('',(69.5,-35.,29.325));
#43157=CARTESIAN_POINT('',(67.,69.5,29.325));
#43158=CARTESIAN_POINT('Origin',(67.,67.,29.325));
#43159=CARTESIAN_POINT('',(-67.,69.5,29.325));
#43160=CARTESIAN_POINT('',(35.,69.5,29.325));
#43161=CARTESIAN_POINT('',(-69.5,67.,29.325));
#43162=CARTESIAN_POINT('Origin',(-67.,67.,29.325));
#43163=CARTESIAN_POINT('',(-69.5,-51.,29.325));
#43164=CARTESIAN_POINT('',(-69.5,35.,29.325));
#43165=CARTESIAN_POINT('',(-73.,-54.5,29.325));
#43166=CARTESIAN_POINT('Origin',(-73.,-51.,29.325));
#43167=CARTESIAN_POINT('',(-81.,-54.5,29.325));
#43168=CARTESIAN_POINT('',(-27.,-54.5,29.325));
#43169=CARTESIAN_POINT('',(-83.5,-57.,29.325));
#43170=CARTESIAN_POINT('Origin',(-81.,-57.,29.325));
#43171=CARTESIAN_POINT('',(-83.5,-82.5,29.325));
#43172=CARTESIAN_POINT('',(-83.5,-27.,29.325));
#43173=CARTESIAN_POINT('',(-81.,-85.,29.325));
#43174=CARTESIAN_POINT('Origin',(-81.,-82.5,29.325));
#43175=CARTESIAN_POINT('',(-57.,-85.,29.325));
#43176=CARTESIAN_POINT('',(-42.,-85.,29.325));
#43177=CARTESIAN_POINT('Origin',(-57.,-82.5,29.325));
#43178=CARTESIAN_POINT('',(-21.3,56.25,29.325));
#43179=CARTESIAN_POINT('Origin',(-18.75,56.25,29.325));
#43180=CARTESIAN_POINT('',(25.,-1.53080849893419E-15,29.325));
#43181=CARTESIAN_POINT('Origin',(37.5,0.,29.325));
#43182=CARTESIAN_POINT('',(-12.5,37.5,29.325));
#43183=CARTESIAN_POINT('Origin',(0.,37.5,29.325));
#43184=CARTESIAN_POINT('',(-61.5,-79.,29.325));
#43185=CARTESIAN_POINT('Origin',(-60.,-79.,29.325));
#43186=CARTESIAN_POINT('',(47.425,52.425,29.325));
#43187=CARTESIAN_POINT('Origin',(52.425,52.425,29.325));
#43188=CARTESIAN_POINT('',(-57.425,-52.425,29.325));
#43189=CARTESIAN_POINT('Origin',(-52.425,-52.425,29.325));
#43190=CARTESIAN_POINT('',(-56.6629,52.425,29.325));
#43191=CARTESIAN_POINT('Origin',(-52.425,52.425,29.325));
#43192=CARTESIAN_POINT('',(-5.625,-6.88863824520386E-16,29.325));
#43193=CARTESIAN_POINT('Origin',(0.,0.,29.325));
#43194=CARTESIAN_POINT('',(-50.,-1.53080849893419E-15,29.325));
#43195=CARTESIAN_POINT('Origin',(-37.5,0.,29.325));
#43196=CARTESIAN_POINT('Origin',(-56.25,18.75,29.325));
#43197=CARTESIAN_POINT('',(-58.3,18.75,20.825));
#43198=CARTESIAN_POINT('',(-58.3,18.75,29.325));
#43199=CARTESIAN_POINT('Origin',(-56.25,18.75,20.825));
#43200=CARTESIAN_POINT('Origin',(-18.75,56.25,29.075));
#43201=CARTESIAN_POINT('',(-20.8,56.25,28.825));
#43202=CARTESIAN_POINT('',(-21.05,56.25,29.075));
#43203=CARTESIAN_POINT('Origin',(-18.75,56.25,28.825));
#43204=CARTESIAN_POINT('Origin',(-18.75,56.25,29.325));
#43205=CARTESIAN_POINT('',(-20.8,56.25,20.825));
#43206=CARTESIAN_POINT('',(-20.8,56.25,29.325));
#43207=CARTESIAN_POINT('Origin',(-18.75,56.25,20.825));
#43208=CARTESIAN_POINT('Origin',(-27.,-58.25,29.075));
#43209=CARTESIAN_POINT('',(-54.,-58.5,28.825));
#43210=CARTESIAN_POINT('',(-53.5833333333333,-58.9166666666667,28.4083333333333));
#43211=CARTESIAN_POINT('',(-49.,-58.5,28.825));
#43212=CARTESIAN_POINT('',(-27.,-58.5,28.825));
#43213=CARTESIAN_POINT('',(-49.,-58.5,28.825));
#43214=CARTESIAN_POINT('Origin',(-49.,-55.5,29.075));
#43215=CARTESIAN_POINT('',(-46.,-55.5,28.825));
#43216=CARTESIAN_POINT('Origin',(-49.,-55.5,28.825));
#43217=CARTESIAN_POINT('',(-46.,-55.5,28.825));
#43218=CARTESIAN_POINT('Origin',(-46.25,-29.25,29.075));
#43219=CARTESIAN_POINT('',(-46.,-43.,28.825));
#43220=CARTESIAN_POINT('',(-46.,-43.,28.825));
#43221=CARTESIAN_POINT('',(-46.,-29.25,28.825));
#43222=CARTESIAN_POINT('Origin',(-43.,-43.,29.075));
#43223=CARTESIAN_POINT('',(-43.,-40.,28.825));
#43224=CARTESIAN_POINT('Origin',(-43.,-43.,28.825));
#43225=CARTESIAN_POINT('',(-43.,-40.,28.825));
#43226=CARTESIAN_POINT('Origin',(-23.,-39.75,29.075));
#43227=CARTESIAN_POINT('',(-12.034713649895,-39.7557126677597,29.0692873322403));
#43228=CARTESIAN_POINT('Ctrl Pts',(-12.034713649895,-39.7557126677597,29.0692873322403));
#43229=CARTESIAN_POINT('Ctrl Pts',(-12.186838165433,-39.6294523240611,29.1955476759389));
#43230=CARTESIAN_POINT('Ctrl Pts',(-12.3389626809711,-39.499999998538,29.325000001462));
#43231=CARTESIAN_POINT('',(-12.2366945943055,-40.,28.825));
#43232=CARTESIAN_POINT('',(-23.,-40.,28.825));
#43233=CARTESIAN_POINT('',(-13.3898823845721,-41.3947314172564,27.4302685827436));
#43234=CARTESIAN_POINT('Origin',(0.,-37.5,29.075));
#43235=CARTESIAN_POINT('',(-11.8306505499589,-39.508907057272,28.825));
#43236=CARTESIAN_POINT('Ctrl Pts',(-11.8306505487286,-39.5089070557841,
28.824999998538));
#43237=CARTESIAN_POINT('Ctrl Pts',(-11.9316540214349,-39.6310664454554,
28.9450286360224));
#43238=CARTESIAN_POINT('Ctrl Pts',(-12.034713649895,-39.7557126677596,29.0692873322403));
#43239=CARTESIAN_POINT('',(11.8306505499589,-39.508907057272,28.825));
#43240=CARTESIAN_POINT('Origin',(0.,-37.5,28.825));
#43241=CARTESIAN_POINT('',(12.0347136500218,-39.755712667654,29.0692873324511));
#43242=CARTESIAN_POINT('Ctrl Pts',(12.0347136500218,-39.755712667654,29.0692873324511));
#43243=CARTESIAN_POINT('Ctrl Pts',(11.9316540215288,-39.6310664453101,28.9450286361929));
#43244=CARTESIAN_POINT('Ctrl Pts',(11.8306505487286,-39.5089070557841,28.824999998538));
#43245=CARTESIAN_POINT('Ctrl Pts',(12.3389626792531,-39.5,29.325));
#43246=CARTESIAN_POINT('Ctrl Pts',(12.2383051553503,-39.5856558228154,29.2393441771846));
#43247=CARTESIAN_POINT('Ctrl Pts',(12.1368860140384,-39.6709116232476,29.1540883767524));
#43248=CARTESIAN_POINT('Ctrl Pts',(12.0347136501489,-39.7557126675489,29.0692873324511));
#43249=CARTESIAN_POINT('Origin',(-12.0336725721322,-39.754453528636,29.325));
#43250=CARTESIAN_POINT('',(-12.2366945943055,-40.,20.3));
#43251=CARTESIAN_POINT('',(-12.2366945943055,-40.,29.325));
#43252=CARTESIAN_POINT('',(-11.8306505499589,-39.508907057272,20.3));
#43253=CARTESIAN_POINT('',(-12.2366945943055,-40.,20.3));
#43254=CARTESIAN_POINT('',(-11.8306505499589,-39.508907057272,29.325));
#43255=CARTESIAN_POINT('Origin',(-11.8306505499589,-39.508907057272,20.3));
#43256=CARTESIAN_POINT('',(-12.3389626792531,-39.5,19.8));
#43257=CARTESIAN_POINT('Ctrl Pts',(-12.338962679254,-39.5,19.7999999999991));
#43258=CARTESIAN_POINT('Ctrl Pts',(-12.0805946952053,-39.5047062025856,
20.0542864406007));
#43259=CARTESIAN_POINT('Ctrl Pts',(-11.8306505499589,-39.508907057272,20.3));
#43260=CARTESIAN_POINT('',(-12.3389626792531,-39.5,19.8));
#43261=CARTESIAN_POINT('Origin',(-27.,-58.25,20.05));
#43262=CARTESIAN_POINT('',(-54.,-58.5,20.3));
#43263=CARTESIAN_POINT('',(-54.,-58.,19.8));
#43264=CARTESIAN_POINT('',(-54.,-61.125,22.925));
#43265=CARTESIAN_POINT('',(-49.,-58.,19.8));
#43266=CARTESIAN_POINT('',(-27.,-58.,19.8));
#43267=CARTESIAN_POINT('',(-49.,-58.5,20.3));
#43268=CARTESIAN_POINT('',(-49.,-58.,19.8));
#43269=CARTESIAN_POINT('',(-27.,-58.5,20.3));
#43270=CARTESIAN_POINT('Origin',(-49.,-55.5,20.05));
#43271=CARTESIAN_POINT('',(-46.5,-55.5,19.8));
#43272=CARTESIAN_POINT('',(-46.,-55.5,20.3));
#43273=CARTESIAN_POINT('',(-46.5,-55.5,19.8));
#43274=CARTESIAN_POINT('Origin',(-49.,-55.5,20.3));
#43275=CARTESIAN_POINT('Origin',(-49.,-55.5,19.8));
#43276=CARTESIAN_POINT('Origin',(-46.25,-29.25,20.05));
#43277=CARTESIAN_POINT('',(-46.5,-43.,19.8));
#43278=CARTESIAN_POINT('',(-46.,-43.,20.3));
#43279=CARTESIAN_POINT('',(-46.5,-43.,19.8));
#43280=CARTESIAN_POINT('',(-46.,-29.25,20.3));
#43281=CARTESIAN_POINT('',(-46.5,-29.25,19.8));
#43282=CARTESIAN_POINT('Origin',(-43.,-43.,20.05));
#43283=CARTESIAN_POINT('',(-43.,-39.5,19.8));
#43284=CARTESIAN_POINT('',(-43.,-40.,20.3));
#43285=CARTESIAN_POINT('',(-43.,-39.5,19.8));
#43286=CARTESIAN_POINT('Origin',(-43.,-43.,20.3));
#43287=CARTESIAN_POINT('Origin',(-43.,-43.,19.8));
#43288=CARTESIAN_POINT('Origin',(-23.,-39.75,20.05));
#43289=CARTESIAN_POINT('',(-23.,-39.5,19.8));
#43290=CARTESIAN_POINT('',(-23.,-40.,20.3));
#43291=CARTESIAN_POINT('Origin',(0.,-37.5,20.05));
#43292=CARTESIAN_POINT('',(12.034713649895,-39.7557126677597,20.0557126677597));
#43293=CARTESIAN_POINT('',(11.8306505499589,-39.508907057272,20.3));
#43294=CARTESIAN_POINT('Ctrl Pts',(12.034713649895,-39.7557126677597,20.0557126677597));
#43295=CARTESIAN_POINT('Ctrl Pts',(11.9316540220625,-39.6310664462144,20.1799713632209));
#43296=CARTESIAN_POINT('Ctrl Pts',(11.8306505499589,-39.508907057272,20.3));
#43297=CARTESIAN_POINT('Origin',(0.,-37.5,20.3));
#43298=CARTESIAN_POINT('',(12.3389626792531,-39.5,19.8));
#43299=CARTESIAN_POINT('Origin',(0.,-37.5,19.8));
#43300=CARTESIAN_POINT('Ctrl Pts',(12.3389626792531,-39.5,19.8));
#43301=CARTESIAN_POINT('Ctrl Pts',(12.1868381645741,-39.6294523247741,19.929452324774));
#43302=CARTESIAN_POINT('Ctrl Pts',(12.034713649895,-39.7557126677597,20.0557126677597));
#43303=CARTESIAN_POINT('Origin',(-46.,-58.5,19.8));
#43304=CARTESIAN_POINT('',(-46.,-55.5,19.8));
#43305=CARTESIAN_POINT('',(-46.,-43.,19.8));
#43306=CARTESIAN_POINT('Origin',(-43.,-43.,19.8));
#43307=CARTESIAN_POINT('',(-43.,-40.,19.8));
#43308=CARTESIAN_POINT('Origin',(-46.,-40.,19.8));
#43309=CARTESIAN_POINT('Origin',(0.,-37.5,29.325));
#43310=CARTESIAN_POINT('',(11.8306505499589,-39.508907057272,29.325));
#43311=CARTESIAN_POINT('Origin',(12.0336725721322,-39.754453528636,29.325));
#43312=CARTESIAN_POINT('',(12.2366945943055,-40.,20.3));
#43313=CARTESIAN_POINT('',(12.2366945943055,-40.,20.3));
#43314=CARTESIAN_POINT('',(12.2366945943055,-40.,28.825));
#43315=CARTESIAN_POINT('',(12.2366945943055,-40.,29.325));
#43316=CARTESIAN_POINT('',(7.53086665277066,-34.3085019372742,34.5164980627258));
#43317=CARTESIAN_POINT('Origin',(-23.,-39.75,20.05));
#43318=CARTESIAN_POINT('',(39.,-39.5,19.8));
#43319=CARTESIAN_POINT('',(-23.,-39.5,19.8));
#43320=CARTESIAN_POINT('',(39.,-40.,20.3));
#43321=CARTESIAN_POINT('',(39.,-39.5,19.8));
#43322=CARTESIAN_POINT('',(-23.,-40.,20.3));
#43323=CARTESIAN_POINT('Origin',(0.,37.5,20.05));
#43324=CARTESIAN_POINT('',(-12.5,37.5,19.8));
#43325=CARTESIAN_POINT('Origin',(0.,37.5,19.8));
#43326=CARTESIAN_POINT('',(-12.,37.5,20.3));
#43327=CARTESIAN_POINT('',(-12.25,37.5,20.05));
#43328=CARTESIAN_POINT('Origin',(0.,37.5,20.3));
#43329=CARTESIAN_POINT('Origin',(0.,0.,19.8));
#43330=CARTESIAN_POINT('',(-54.,-57.,19.8));
#43331=CARTESIAN_POINT('',(-54.,-42.75,19.8));
#43332=CARTESIAN_POINT('',(-57.,-54.,19.8));
#43333=CARTESIAN_POINT('Origin',(-57.,-57.,19.8));
#43334=CARTESIAN_POINT('',(-71.197224362268,-54.,19.8));
#43335=CARTESIAN_POINT('',(-27.,-54.,19.8));
#43336=CARTESIAN_POINT('',(-69.5,-51.,19.8));
#43337=CARTESIAN_POINT('Origin',(-73.,-51.,19.8));
#43338=CARTESIAN_POINT('',(-69.5,67.,19.8));
#43339=CARTESIAN_POINT('',(-69.5,35.,19.8));
#43340=CARTESIAN_POINT('',(-67.,69.5,19.8));
#43341=CARTESIAN_POINT('Origin',(-67.,67.,19.8));
#43342=CARTESIAN_POINT('',(67.,69.5,19.8));
#43343=CARTESIAN_POINT('',(35.,69.5,19.8));
#43344=CARTESIAN_POINT('',(69.5,67.,19.8));
#43345=CARTESIAN_POINT('Origin',(67.,67.,19.8));
#43346=CARTESIAN_POINT('',(69.5,-67.,19.8));
#43347=CARTESIAN_POINT('',(69.5,-35.,19.8));
#43348=CARTESIAN_POINT('',(67.,-69.5,19.8));
#43349=CARTESIAN_POINT('Origin',(67.,-67.,19.8));
#43350=CARTESIAN_POINT('',(45.,-69.5,19.8));
#43351=CARTESIAN_POINT('',(21.,-69.5,19.8));
#43352=CARTESIAN_POINT('',(42.5,-67.,19.8));
#43353=CARTESIAN_POINT('Origin',(45.,-67.,19.8));
#43354=CARTESIAN_POINT('',(42.5,-43.,19.8));
#43355=CARTESIAN_POINT('',(42.5,-20.,19.8));
#43356=CARTESIAN_POINT('Origin',(39.,-43.,19.8));
#43357=CARTESIAN_POINT('',(-50.,1.53080849893419E-15,19.8));
#43358=CARTESIAN_POINT('Origin',(-37.5,0.,19.8));
#43359=CARTESIAN_POINT('',(-5.025,-6.15385016571545E-16,19.8));
#43360=CARTESIAN_POINT('Origin',(0.,0.,19.8));
#43361=CARTESIAN_POINT('',(25.,1.53080849893419E-15,19.8));
#43362=CARTESIAN_POINT('Origin',(37.5,0.,19.8));
#43363=CARTESIAN_POINT('Origin',(0.,37.5,29.325));
#43364=CARTESIAN_POINT('',(-12.,37.5,28.825));
#43365=CARTESIAN_POINT('Origin',(0.,37.5,28.825));
#43366=CARTESIAN_POINT('',(-12.,37.5,29.325));
#43367=CARTESIAN_POINT('Origin',(-37.5,0.,20.05));
#43368=CARTESIAN_POINT('',(-49.5,-1.46957615897682E-15,20.3));
#43369=CARTESIAN_POINT('',(-49.75,1.50019232895551E-15,20.05));
#43370=CARTESIAN_POINT('Origin',(-37.5,0.,20.3));
#43371=CARTESIAN_POINT('Origin',(-37.5,0.,29.325));
#43372=CARTESIAN_POINT('',(-49.5,1.46957615897682E-15,28.825));
#43373=CARTESIAN_POINT('Origin',(-37.5,0.,28.825));
#43374=CARTESIAN_POINT('',(-49.5,1.46957615897682E-15,29.325));
#43375=CARTESIAN_POINT('Origin',(37.5,0.,20.05));
#43376=CARTESIAN_POINT('',(25.5,-1.46957615897682E-15,20.3));
#43377=CARTESIAN_POINT('',(25.25,1.50019232895551E-15,20.05));
#43378=CARTESIAN_POINT('Origin',(37.5,0.,20.3));
#43379=CARTESIAN_POINT('Origin',(37.5,0.,29.325));
#43380=CARTESIAN_POINT('',(25.5,1.46957615897682E-15,28.825));
#43381=CARTESIAN_POINT('Origin',(37.5,0.,28.825));
#43382=CARTESIAN_POINT('',(25.5,1.46957615897682E-15,29.325));
#43383=CARTESIAN_POINT('Origin',(39.,-43.,20.05));
#43384=CARTESIAN_POINT('',(42.,-43.,20.3));
#43385=CARTESIAN_POINT('',(42.5,-43.,19.8));
#43386=CARTESIAN_POINT('Origin',(39.,-43.,20.3));
#43387=CARTESIAN_POINT('Origin',(42.25,-20.,20.05));
#43388=CARTESIAN_POINT('',(42.,-67.,20.3));
#43389=CARTESIAN_POINT('',(42.5,-67.,19.8));
#43390=CARTESIAN_POINT('',(42.,-20.,20.3));
#43391=CARTESIAN_POINT('Origin',(45.,-67.,20.05));
#43392=CARTESIAN_POINT('',(45.,-70.,20.3));
#43393=CARTESIAN_POINT('',(45.,-69.5,19.8));
#43394=CARTESIAN_POINT('Origin',(45.,-67.,20.3));
#43395=CARTESIAN_POINT('Origin',(21.,-69.75,20.05));
#43396=CARTESIAN_POINT('',(67.,-70.,20.3));
#43397=CARTESIAN_POINT('',(67.,-69.5,19.8));
#43398=CARTESIAN_POINT('',(21.,-70.,20.3));
#43399=CARTESIAN_POINT('Origin',(67.,-67.,20.05));
#43400=CARTESIAN_POINT('',(70.,-67.,20.3));
#43401=CARTESIAN_POINT('',(69.5,-67.,19.8));
#43402=CARTESIAN_POINT('Origin',(67.,-67.,20.3));
#43403=CARTESIAN_POINT('Origin',(69.75,-35.,20.05));
#43404=CARTESIAN_POINT('',(70.,67.,20.3));
#43405=CARTESIAN_POINT('',(69.5,67.,19.8));
#43406=CARTESIAN_POINT('',(70.,-35.,20.3));
#43407=CARTESIAN_POINT('Origin',(67.,67.,20.05));
#43408=CARTESIAN_POINT('',(67.,70.,20.3));
#43409=CARTESIAN_POINT('',(67.,69.5,19.8));
#43410=CARTESIAN_POINT('Origin',(67.,67.,20.3));
#43411=CARTESIAN_POINT('Origin',(35.,69.75,20.05));
#43412=CARTESIAN_POINT('',(-67.,70.,20.3));
#43413=CARTESIAN_POINT('',(-67.,69.5,19.8));
#43414=CARTESIAN_POINT('',(35.,70.,20.3));
#43415=CARTESIAN_POINT('Origin',(-67.,67.,20.05));
#43416=CARTESIAN_POINT('',(-70.,67.,20.3));
#43417=CARTESIAN_POINT('',(-69.5,67.,19.8));
#43418=CARTESIAN_POINT('Origin',(-67.,67.,20.3));
#43419=CARTESIAN_POINT('Origin',(-69.75,35.,20.05));
#43420=CARTESIAN_POINT('',(-70.,-51.,20.3));
#43421=CARTESIAN_POINT('',(-69.5,-51.,19.8));
#43422=CARTESIAN_POINT('',(-70.,35.,20.3));
#43423=CARTESIAN_POINT('Origin',(-73.,-51.,20.05));
#43424=CARTESIAN_POINT('',(-73.,-54.,20.3));
#43425=CARTESIAN_POINT('Ctrl Pts',(-73.,-54.,20.3));
#43426=CARTESIAN_POINT('Ctrl Pts',(-72.1679497056621,-54.,20.3));
#43427=CARTESIAN_POINT('Ctrl Pts',(-71.197224362268,-54.,19.8));
#43428=CARTESIAN_POINT('Origin',(-73.,-51.,20.3));
#43429=CARTESIAN_POINT('Origin',(-23.,-39.75,29.075));
#43430=CARTESIAN_POINT('',(39.,-40.,28.825));
#43431=CARTESIAN_POINT('',(-23.,-40.,28.825));
#43432=CARTESIAN_POINT('',(39.,-40.,28.825));
#43433=CARTESIAN_POINT('Origin',(-54.25,-69.875,1.25));
#43434=CARTESIAN_POINT('',(-54.5,-57.,1.));
#43435=CARTESIAN_POINT('',(-54.,-57.,1.5));
#43436=CARTESIAN_POINT('',(-54.5,-57.,1.));
#43437=CARTESIAN_POINT('',(-54.,-82.5,1.5));
#43438=CARTESIAN_POINT('',(-54.,-69.875,1.5));
#43439=CARTESIAN_POINT('',(-54.5,-82.5,1.));
#43440=CARTESIAN_POINT('',(-54.,-82.5,1.5));
#43441=CARTESIAN_POINT('',(-54.5,-69.875,1.));
#43442=CARTESIAN_POINT('Origin',(-57.,-57.,1.25));
#43443=CARTESIAN_POINT('',(-57.,-54.5,1.));
#43444=CARTESIAN_POINT('',(-57.,-54.,1.5));
#43445=CARTESIAN_POINT('',(-57.,-54.5,1.));
#43446=CARTESIAN_POINT('Origin',(-57.,-57.,1.5));
#43447=CARTESIAN_POINT('Origin',(-57.,-57.,1.));
#43448=CARTESIAN_POINT('Origin',(-61.5,-54.25,1.25));
#43449=CARTESIAN_POINT('',(-81.,-54.5,1.));
#43450=CARTESIAN_POINT('',(-81.,-54.,1.5));
#43451=CARTESIAN_POINT('',(-81.,-54.5,1.));
#43452=CARTESIAN_POINT('',(-61.5,-54.,1.5));
#43453=CARTESIAN_POINT('',(-61.5,-54.5,1.));
#43454=CARTESIAN_POINT('Origin',(-81.,-57.,1.25));
#43455=CARTESIAN_POINT('',(-83.5,-57.,1.));
#43456=CARTESIAN_POINT('',(-84.,-57.,1.5));
#43457=CARTESIAN_POINT('',(-83.5,-57.,1.));
#43458=CARTESIAN_POINT('Origin',(-81.,-57.,1.5));
#43459=CARTESIAN_POINT('Origin',(-81.,-57.,1.));
#43460=CARTESIAN_POINT('Origin',(-83.75,-61.875,1.25));
#43461=CARTESIAN_POINT('',(-83.5,-82.5,1.));
#43462=CARTESIAN_POINT('',(-84.,-82.5,1.5));
#43463=CARTESIAN_POINT('',(-83.5,-82.5,1.));
#43464=CARTESIAN_POINT('',(-84.,-61.875,1.5));
#43465=CARTESIAN_POINT('',(-83.5,-61.875,1.));
#43466=CARTESIAN_POINT('Origin',(-81.,-82.5,1.25));
#43467=CARTESIAN_POINT('',(-81.,-85.,1.));
#43468=CARTESIAN_POINT('',(-81.,-85.5,1.5));
#43469=CARTESIAN_POINT('',(-81.,-85.,1.));
#43470=CARTESIAN_POINT('Origin',(-81.,-82.5,1.5));
#43471=CARTESIAN_POINT('Origin',(-81.,-82.5,1.));
#43472=CARTESIAN_POINT('Origin',(-76.5,-85.25,1.25));
#43473=CARTESIAN_POINT('',(-57.,-85.,1.));
#43474=CARTESIAN_POINT('',(-57.,-85.5,1.5));
#43475=CARTESIAN_POINT('',(-57.,-85.,1.));
#43476=CARTESIAN_POINT('',(-76.5,-85.5,1.5));
#43477=CARTESIAN_POINT('',(-76.5,-85.,1.));
#43478=CARTESIAN_POINT('Origin',(-57.,-82.5,1.25));
#43479=CARTESIAN_POINT('Origin',(-57.,-82.5,1.5));
#43480=CARTESIAN_POINT('Origin',(-57.,-82.5,1.));
#43481=CARTESIAN_POINT('Origin',(-81.,-82.5,1.));
#43482=CARTESIAN_POINT('',(-81.,-85.5,28.825));
#43483=CARTESIAN_POINT('',(-81.,-85.5,1.));
#43484=CARTESIAN_POINT('',(-84.,-82.5,28.825));
#43485=CARTESIAN_POINT('Origin',(-81.,-82.5,28.825));
#43486=CARTESIAN_POINT('',(-84.,-82.5,1.));
#43487=CARTESIAN_POINT('Origin',(-84.,-85.5,1.));
#43488=CARTESIAN_POINT('',(-57.,-85.5,28.825));
#43489=CARTESIAN_POINT('',(-57.,-85.5,10.4));
#43490=CARTESIAN_POINT('',(-42.,-85.5,28.825));
#43491=CARTESIAN_POINT('Origin',(-57.,-82.5,10.4));
#43492=CARTESIAN_POINT('',(-54.,-82.5,17.1715728752538));
#43493=CARTESIAN_POINT('',(-54.,-82.5,10.4));
#43494=CARTESIAN_POINT('',(-54.,-82.5,22.8284271247462));
#43495=CARTESIAN_POINT('Ctrl Pts',(-54.,-82.5,17.1715728752538));
#43496=CARTESIAN_POINT('Ctrl Pts',(-54.,-82.762296060057,17.4961476900572));
#43497=CARTESIAN_POINT('Ctrl Pts',(-54.034665028442,-82.985258794199,17.8667160823623));
#43498=CARTESIAN_POINT('Ctrl Pts',(-54.1231965863205,-83.3837724986897,
18.8181489326506));
#43499=CARTESIAN_POINT('Ctrl Pts',(-54.1715728752538,-83.5,19.4255653846135));
#43500=CARTESIAN_POINT('Ctrl Pts',(-54.1715728752538,-83.5,20.5744346153865));
#43501=CARTESIAN_POINT('Ctrl Pts',(-54.1231965863205,-83.3837724986897,
21.1818510673494));
#43502=CARTESIAN_POINT('Ctrl Pts',(-54.034665028442,-82.985258794199,22.1332839176377));
#43503=CARTESIAN_POINT('Ctrl Pts',(-54.,-82.762296060057,22.5038523099428));
#43504=CARTESIAN_POINT('Ctrl Pts',(-54.,-82.5,22.8284271247462));
#43505=CARTESIAN_POINT('',(-54.,-82.5,28.825));
#43506=CARTESIAN_POINT('',(-54.,-82.5,10.4));
#43507=CARTESIAN_POINT('Origin',(-57.,-82.5,28.825));
#43508=CARTESIAN_POINT('Origin',(-54.,-70.,19.8));
#43509=CARTESIAN_POINT('',(-54.,-57.,10.4));
#43510=CARTESIAN_POINT('',(-54.,-58.5,19.8));
#43511=CARTESIAN_POINT('',(-54.,-35.,28.825));
#43512=CARTESIAN_POINT('',(-54.,-79.,24.5));
#43513=CARTESIAN_POINT('Origin',(-54.,-79.,20.));
#43514=CARTESIAN_POINT('Origin',(-54.,-79.,20.));
#43515=CARTESIAN_POINT('',(-54.,-66.,25.));
#43516=CARTESIAN_POINT('Origin',(-54.,-66.,20.));
#43517=CARTESIAN_POINT('Origin',(-69.,-69.75,1.));
#43518=CARTESIAN_POINT('Origin',(39.,-43.,29.075));
#43519=CARTESIAN_POINT('',(42.,-43.,28.825));
#43520=CARTESIAN_POINT('Origin',(39.,-43.,28.825));
#43521=CARTESIAN_POINT('',(42.,-43.,28.825));
#43522=CARTESIAN_POINT('Origin',(42.25,-20.,29.075));
#43523=CARTESIAN_POINT('',(42.,-67.,28.825));
#43524=CARTESIAN_POINT('',(42.,-67.,28.825));
#43525=CARTESIAN_POINT('',(42.,-20.,28.825));
#43526=CARTESIAN_POINT('Origin',(45.,-67.,29.075));
#43527=CARTESIAN_POINT('',(45.,-70.,28.825));
#43528=CARTESIAN_POINT('Origin',(45.,-67.,28.825));
#43529=CARTESIAN_POINT('',(45.,-70.,28.825));
#43530=CARTESIAN_POINT('Origin',(21.,-69.75,29.075));
#43531=CARTESIAN_POINT('',(67.,-70.,28.825));
#43532=CARTESIAN_POINT('',(67.,-70.,28.825));
#43533=CARTESIAN_POINT('',(21.,-70.,28.825));
#43534=CARTESIAN_POINT('Origin',(67.,-67.,29.075));
#43535=CARTESIAN_POINT('',(70.,-67.,28.825));
#43536=CARTESIAN_POINT('Origin',(67.,-67.,28.825));
#43537=CARTESIAN_POINT('',(70.,-67.,28.825));
#43538=CARTESIAN_POINT('Origin',(69.75,-35.,29.075));
#43539=CARTESIAN_POINT('',(70.,67.,28.825));
#43540=CARTESIAN_POINT('',(70.,67.,28.825));
#43541=CARTESIAN_POINT('',(70.,-35.,28.825));
#43542=CARTESIAN_POINT('Origin',(67.,67.,29.075));
#43543=CARTESIAN_POINT('',(67.,70.,28.825));
#43544=CARTESIAN_POINT('Origin',(67.,67.,28.825));
#43545=CARTESIAN_POINT('',(67.,70.,28.825));
#43546=CARTESIAN_POINT('Origin',(35.,69.75,29.075));
#43547=CARTESIAN_POINT('',(-67.,70.,28.825));
#43548=CARTESIAN_POINT('',(-67.,70.,28.825));
#43549=CARTESIAN_POINT('',(35.,70.,28.825));
#43550=CARTESIAN_POINT('Origin',(-67.,67.,29.075));
#43551=CARTESIAN_POINT('',(-70.,67.,28.825));
#43552=CARTESIAN_POINT('Origin',(-67.,67.,28.825));
#43553=CARTESIAN_POINT('',(-70.,67.,28.825));
#43554=CARTESIAN_POINT('Origin',(-69.75,35.,29.075));
#43555=CARTESIAN_POINT('',(-70.,-51.,28.825));
#43556=CARTESIAN_POINT('',(-70.,-51.,28.825));
#43557=CARTESIAN_POINT('',(-70.,35.,28.825));
#43558=CARTESIAN_POINT('Origin',(-73.,-51.,29.075));
#43559=CARTESIAN_POINT('',(-73.,-54.,28.825));
#43560=CARTESIAN_POINT('Origin',(-73.,-51.,28.825));
#43561=CARTESIAN_POINT('',(-73.,-54.,28.825));
#43562=CARTESIAN_POINT('Origin',(-27.,-54.25,29.075));
#43563=CARTESIAN_POINT('',(-81.,-54.,28.825));
#43564=CARTESIAN_POINT('',(-81.,-54.,28.825));
#43565=CARTESIAN_POINT('',(-27.,-54.,28.825));
#43566=CARTESIAN_POINT('Origin',(-81.,-57.,29.075));
#43567=CARTESIAN_POINT('',(-84.,-57.,28.825));
#43568=CARTESIAN_POINT('Origin',(-81.,-57.,28.825));
#43569=CARTESIAN_POINT('',(-84.,-57.,28.825));
#43570=CARTESIAN_POINT('Origin',(-83.75,-27.,29.075));
#43571=CARTESIAN_POINT('',(-84.,-82.5,28.825));
#43572=CARTESIAN_POINT('',(-84.,-27.,28.825));
#43573=CARTESIAN_POINT('Origin',(-81.,-82.5,29.075));
#43574=CARTESIAN_POINT('',(-81.,-85.5,28.825));
#43575=CARTESIAN_POINT('Origin',(-42.,-85.25,29.075));
#43576=CARTESIAN_POINT('',(-57.,-85.5,28.825));
#43577=CARTESIAN_POINT('Origin',(-57.,-82.5,29.075));
#43578=CARTESIAN_POINT('',(-54.,-82.5,28.825));
#43579=CARTESIAN_POINT('Origin',(-54.25,-35.,29.075));
#43580=CARTESIAN_POINT('Origin',(-84.,-54.,1.));
#43581=CARTESIAN_POINT('',(-84.,-57.,1.));
#43582=CARTESIAN_POINT('Origin',(-81.,-57.,1.));
#43583=CARTESIAN_POINT('',(-81.,-54.,1.));
#43584=CARTESIAN_POINT('Origin',(-54.,-54.,1.));
#43585=CARTESIAN_POINT('',(-73.,-54.,10.4));
#43586=CARTESIAN_POINT('',(-57.,-54.,10.4));
#43587=CARTESIAN_POINT('Origin',(-73.,-51.,10.4));
#43588=CARTESIAN_POINT('',(-70.,-51.,10.4));
#43589=CARTESIAN_POINT('Origin',(-70.,70.,19.8));
#43590=CARTESIAN_POINT('',(-70.,67.,19.8));
#43591=CARTESIAN_POINT('Origin',(-67.,67.,19.8));
#43592=CARTESIAN_POINT('',(-67.,70.,19.8));
#43593=CARTESIAN_POINT('Origin',(70.,70.,19.8));
#43594=CARTESIAN_POINT('',(67.,70.,19.8));
#43595=CARTESIAN_POINT('Origin',(67.,67.,19.8));
#43596=CARTESIAN_POINT('',(70.,67.,19.8));
#43597=CARTESIAN_POINT('Origin',(70.,-70.,19.8));
#43598=CARTESIAN_POINT('',(70.,-67.,19.8));
#43599=CARTESIAN_POINT('Origin',(67.,-67.,19.8));
#43600=CARTESIAN_POINT('',(67.,-70.,19.8));
#43601=CARTESIAN_POINT('Origin',(42.,-70.,19.8));
#43602=CARTESIAN_POINT('',(45.,-70.,19.8));
#43603=CARTESIAN_POINT('Origin',(45.,-67.,19.8));
#43604=CARTESIAN_POINT('',(42.,-67.,19.8));
#43605=CARTESIAN_POINT('Origin',(42.,-40.,19.8));
#43606=CARTESIAN_POINT('',(42.,-43.,19.8));
#43607=CARTESIAN_POINT('Origin',(39.,-43.,19.8));
#43608=CARTESIAN_POINT('',(39.,-40.,19.8));
#43609=CARTESIAN_POINT('Origin',(-46.,-40.,19.8));
#43610=CARTESIAN_POINT('Origin',(37.5,0.,29.075));
#43611=CARTESIAN_POINT('',(25.25,-1.50019232895551E-15,29.075));
#43612=CARTESIAN_POINT('Origin',(-37.5,0.,29.075));
#43613=CARTESIAN_POINT('',(-49.75,-1.50019232895551E-15,29.075));
#43614=CARTESIAN_POINT('Origin',(0.,37.5,29.075));
#43615=CARTESIAN_POINT('',(-12.25,37.5,29.075));
#43616=CARTESIAN_POINT('Origin',(0.,0.,29.025));
#43617=CARTESIAN_POINT('',(-5.025,6.15385016571545E-16,28.725));
#43618=CARTESIAN_POINT('',(-5.325,-6.52124420545966E-16,29.025));
#43619=CARTESIAN_POINT('Origin',(0.,0.,28.725));
#43620=CARTESIAN_POINT('Origin',(0.,0.,29.325));
#43621=CARTESIAN_POINT('',(-5.025,6.15385016571545E-16,29.325));
#43622=CARTESIAN_POINT('Origin',(-60.,-79.,29.325));
#43623=CARTESIAN_POINT('',(-61.5,-79.,24.5));
#43624=CARTESIAN_POINT('',(-61.5,-79.,29.325));
#43625=CARTESIAN_POINT('',(-58.5,-79.,24.5));
#43626=CARTESIAN_POINT('Ctrl Pts',(-58.5,-79.,24.5));
#43627=CARTESIAN_POINT('Ctrl Pts',(-58.5,-78.810119017199,24.5));
#43628=CARTESIAN_POINT('Ctrl Pts',(-58.5382433687954,-78.6085507941687,
24.4868035691518));
#43629=CARTESIAN_POINT('Ctrl Pts',(-58.6917847708251,-78.2393832820639,
24.4391554329551));
#43630=CARTESIAN_POINT('Ctrl Pts',(-58.8070056851579,-78.0716739712825,
24.4053096652352));
#43631=CARTESIAN_POINT('Ctrl Pts',(-59.0717353764399,-77.8069442800004,
24.3411032840945));
#43632=CARTESIAN_POINT('Ctrl Pts',(-59.2394202300634,-77.6917706385605,
24.3063956191435));
#43633=CARTESIAN_POINT('Ctrl Pts',(-59.6084970398047,-77.5382644910968,
24.2567401743069));
#43634=CARTESIAN_POINT('Ctrl Pts',(-59.8100309093881,-77.5,24.2426406871193));
#43635=CARTESIAN_POINT('Ctrl Pts',(-60.1899690906119,-77.5,24.2426406871193));
#43636=CARTESIAN_POINT('Ctrl Pts',(-60.3915029601953,-77.5382644910968,
24.2567401743069));
#43637=CARTESIAN_POINT('Ctrl Pts',(-60.7605797699366,-77.6917706385605,
24.3063956191435));
#43638=CARTESIAN_POINT('Ctrl Pts',(-60.9282646235601,-77.8069442800004,
24.3411032840945));
#43639=CARTESIAN_POINT('Ctrl Pts',(-61.1929943148421,-78.0716739712825,
24.4053096652352));
#43640=CARTESIAN_POINT('Ctrl Pts',(-61.3082152291749,-78.2393832820639,
24.4391554329551));
#43641=CARTESIAN_POINT('Ctrl Pts',(-61.4617566312046,-78.6085507941687,
24.4868035691518));
#43642=CARTESIAN_POINT('Ctrl Pts',(-61.5,-78.810119017199,24.5));
#43643=CARTESIAN_POINT('Ctrl Pts',(-61.5,-79.,24.5));
#43644=CARTESIAN_POINT('',(-60.,-80.5,24.2426406871193));
#43645=CARTESIAN_POINT('Ctrl Pts',(-60.,-80.5,24.2426406871193));
#43646=CARTESIAN_POINT('Ctrl Pts',(-59.8100309093881,-80.5,24.2426406871193));
#43647=CARTESIAN_POINT('Ctrl Pts',(-59.6084970398047,-80.4617355089032,
24.2567401743069));
#43648=CARTESIAN_POINT('Ctrl Pts',(-59.2394202300634,-80.3082293614395,
24.3063956191435));
#43649=CARTESIAN_POINT('Ctrl Pts',(-59.0717353764399,-80.1930557199996,
24.3411032840945));
#43650=CARTESIAN_POINT('Ctrl Pts',(-58.8070056851579,-79.9283260287175,
24.4053096652352));
#43651=CARTESIAN_POINT('Ctrl Pts',(-58.6917847708251,-79.7606167179361,
24.4391554329551));
#43652=CARTESIAN_POINT('Ctrl Pts',(-58.5382433687954,-79.3914492058313,
24.4868035691518));
#43653=CARTESIAN_POINT('Ctrl Pts',(-58.5,-79.189880982801,24.5));
#43654=CARTESIAN_POINT('Ctrl Pts',(-58.5,-79.,24.5));
#43655=CARTESIAN_POINT('Ctrl Pts',(-61.5,-79.,24.5));
#43656=CARTESIAN_POINT('Ctrl Pts',(-61.5,-79.189880982801,24.5));
#43657=CARTESIAN_POINT('Ctrl Pts',(-61.4617566312046,-79.3914492058313,
24.4868035691518));
#43658=CARTESIAN_POINT('Ctrl Pts',(-61.3082152291749,-79.7606167179361,
24.4391554329551));
#43659=CARTESIAN_POINT('Ctrl Pts',(-61.1929943148421,-79.9283260287175,
24.4053096652352));
#43660=CARTESIAN_POINT('Ctrl Pts',(-60.9282646235601,-80.1930557199996,
24.3411032840945));
#43661=CARTESIAN_POINT('Ctrl Pts',(-60.7605797699366,-80.3082293614395,
24.3063956191435));
#43662=CARTESIAN_POINT('Ctrl Pts',(-60.3915029601953,-80.4617355089032,
24.2567401743069));
#43663=CARTESIAN_POINT('Ctrl Pts',(-60.1899690906119,-80.5,24.2426406871193));
#43664=CARTESIAN_POINT('Ctrl Pts',(-60.,-80.5,24.2426406871193));
#43665=CARTESIAN_POINT('Origin',(-60.,-79.,29.325));
#43666=CARTESIAN_POINT('',(-60.,-80.5,15.7573593128807));
#43667=CARTESIAN_POINT('',(-61.5,-79.,15.5));
#43668=CARTESIAN_POINT('Ctrl Pts',(-60.,-80.5,15.7573593128807));
#43669=CARTESIAN_POINT('Ctrl Pts',(-60.1899690906119,-80.5,15.7573593128807));
#43670=CARTESIAN_POINT('Ctrl Pts',(-60.3915029601953,-80.4617355089032,
15.7432598256931));
#43671=CARTESIAN_POINT('Ctrl Pts',(-60.7605797699366,-80.3082293614395,
15.6936043808565));
#43672=CARTESIAN_POINT('Ctrl Pts',(-60.9282646235601,-80.1930557199996,
15.6588967159055));
#43673=CARTESIAN_POINT('Ctrl Pts',(-61.1929943148421,-79.9283260287175,
15.5946903347648));
#43674=CARTESIAN_POINT('Ctrl Pts',(-61.3082152291749,-79.7606167179361,
15.5608445670449));
#43675=CARTESIAN_POINT('Ctrl Pts',(-61.4617566312046,-79.3914492058313,
15.5131964308482));
#43676=CARTESIAN_POINT('Ctrl Pts',(-61.5,-79.189880982801,15.5));
#43677=CARTESIAN_POINT('Ctrl Pts',(-61.5,-79.,15.5));
#43678=CARTESIAN_POINT('Ctrl Pts',(-61.5,-79.,15.5));
#43679=CARTESIAN_POINT('Ctrl Pts',(-61.5,-78.810119017199,15.5));
#43680=CARTESIAN_POINT('Ctrl Pts',(-61.4617566312046,-78.6085507941687,
15.5131964308482));
#43681=CARTESIAN_POINT('Ctrl Pts',(-61.3082152291749,-78.2393832820639,
15.5608445670449));
#43682=CARTESIAN_POINT('Ctrl Pts',(-61.1929943148421,-78.0716739712825,
15.5946903347648));
#43683=CARTESIAN_POINT('Ctrl Pts',(-60.9282646235601,-77.8069442800004,
15.6588967159055));
#43684=CARTESIAN_POINT('Ctrl Pts',(-60.7605797699366,-77.6917706385605,
15.6936043808565));
#43685=CARTESIAN_POINT('Ctrl Pts',(-60.3915029601953,-77.5382644910968,
15.7432598256931));
#43686=CARTESIAN_POINT('Ctrl Pts',(-60.1899690906119,-77.5,15.7573593128807));
#43687=CARTESIAN_POINT('Ctrl Pts',(-59.8100309093881,-77.5,15.7573593128807));
#43688=CARTESIAN_POINT('Ctrl Pts',(-59.6084970398047,-77.5382644910968,
15.7432598256931));
#43689=CARTESIAN_POINT('Ctrl Pts',(-59.2394202300634,-77.6917706385605,
15.6936043808565));
#43690=CARTESIAN_POINT('Ctrl Pts',(-59.0717353764399,-77.8069442800004,
15.6588967159055));
#43691=CARTESIAN_POINT('Ctrl Pts',(-58.8070056851579,-78.0716739712825,
15.5946903347648));
#43692=CARTESIAN_POINT('Ctrl Pts',(-58.6917847708251,-78.2393832820639,
15.5608445670449));
#43693=CARTESIAN_POINT('Ctrl Pts',(-58.5382433687954,-78.6085507941687,
15.5131964308482));
#43694=CARTESIAN_POINT('Ctrl Pts',(-58.5,-78.810119017199,15.5));
#43695=CARTESIAN_POINT('Ctrl Pts',(-58.5,-79.189880982801,15.5));
#43696=CARTESIAN_POINT('Ctrl Pts',(-58.5382433687954,-79.3914492058313,
15.5131964308482));
#43697=CARTESIAN_POINT('Ctrl Pts',(-58.6917847708251,-79.7606167179361,
15.5608445670449));
#43698=CARTESIAN_POINT('Ctrl Pts',(-58.8070056851579,-79.9283260287175,
15.5946903347648));
#43699=CARTESIAN_POINT('Ctrl Pts',(-59.0717353764399,-80.1930557199995,
15.6588967159055));
#43700=CARTESIAN_POINT('Ctrl Pts',(-59.2394202300634,-80.3082293614395,
15.6936043808565));
#43701=CARTESIAN_POINT('Ctrl Pts',(-59.6084970398047,-80.4617355089032,
15.7432598256931));
#43702=CARTESIAN_POINT('Ctrl Pts',(-59.8100309093881,-80.5,15.7573593128807));
#43703=CARTESIAN_POINT('Ctrl Pts',(-60.,-80.5,15.7573593128807));
#43704=CARTESIAN_POINT('',(-61.5,-79.,11.325));
#43705=CARTESIAN_POINT('',(-61.5,-79.,29.325));
#43706=CARTESIAN_POINT('Origin',(-60.,-79.,11.325));
#43707=CARTESIAN_POINT('Origin',(-60.,-79.,11.325));
#43708=CARTESIAN_POINT('Origin',(-54.,-79.,20.));
#43709=CARTESIAN_POINT('',(-54.,-79.,24.5));
#43710=CARTESIAN_POINT('',(-64.,-79.,24.5));
#43711=CARTESIAN_POINT('',(-54.,-79.,24.5));
#43712=CARTESIAN_POINT('Origin',(-64.,-79.,20.));
#43713=CARTESIAN_POINT('Origin',(-64.,-79.,20.));
#43714=CARTESIAN_POINT('Origin',(-54.,-66.,20.));
#43715=CARTESIAN_POINT('',(-58.5,-66.,25.));
#43716=CARTESIAN_POINT('',(-54.,-66.,25.));
#43717=CARTESIAN_POINT('Origin',(-58.5,-66.,20.));
#43718=CARTESIAN_POINT('Origin',(-58.5,-66.,20.));
#43719=CARTESIAN_POINT('Origin',(-18.75,56.25,20.825));
#43720=CARTESIAN_POINT('Origin',(-56.25,18.75,20.825));
#43721=CARTESIAN_POINT('Origin',(-52.425,52.425,29.325));
#43722=CARTESIAN_POINT('',(-56.6629,52.425,25.325));
#43723=CARTESIAN_POINT('',(-56.6629,52.425,29.325));
#43724=CARTESIAN_POINT('Origin',(-52.425,52.425,25.325));
#43725=CARTESIAN_POINT('Origin',(-52.425,52.425,25.325));
#43726=CARTESIAN_POINT('Origin',(-52.425,-52.425,29.325));
#43727=CARTESIAN_POINT('',(-57.425,-52.425,24.825));
#43728=CARTESIAN_POINT('',(-57.425,-52.425,29.325));
#43729=CARTESIAN_POINT('Origin',(-52.425,-52.425,24.825));
#43730=CARTESIAN_POINT('Origin',(-52.425,-52.425,24.825));
#43731=CARTESIAN_POINT('Origin',(52.425,52.425,29.325));
#43732=CARTESIAN_POINT('',(47.425,52.425,24.825));
#43733=CARTESIAN_POINT('',(47.425,52.425,29.325));
#43734=CARTESIAN_POINT('Origin',(52.425,52.425,24.825));
#43735=CARTESIAN_POINT('Origin',(52.425,52.425,24.825));
#43736=CARTESIAN_POINT('Origin',(-49.,-55.5,19.8));
#43737=CARTESIAN_POINT('',(-49.,-58.5,19.8));
#43738=CARTESIAN_POINT('Origin',(-54.,-58.5,19.8));
#43739=CARTESIAN_POINT('Origin',(-57.,-57.,10.4));
#43740=CARTESIAN_POINT('',(0.,0.,0.));
#43741=CARTESIAN_POINT('Origin',(18.75,18.75,48.25));
#43742=CARTESIAN_POINT('',(14.25,18.75,48.));
#43743=CARTESIAN_POINT('Origin',(18.75,18.75,48.));
#43744=CARTESIAN_POINT('',(13.75,18.75,48.5));
#43745=CARTESIAN_POINT('',(14.,18.75,48.25));
#43746=CARTESIAN_POINT('Origin',(18.75,18.75,48.5));
#43747=CARTESIAN_POINT('Origin',(18.75,18.75,57.));
#43748=CARTESIAN_POINT('',(14.25,18.75,43.25));
#43749=CARTESIAN_POINT('',(14.25,18.75,57.));
#43750=CARTESIAN_POINT('Origin',(18.75,18.75,43.25));
#43751=CARTESIAN_POINT('Origin',(18.75,18.75,48.5));
#43752=CARTESIAN_POINT('',(11.75,18.75,48.5));
#43753=CARTESIAN_POINT('Origin',(18.75,18.75,48.5));
#43754=CARTESIAN_POINT('Origin',(-56.25,-18.75,48.25));
#43755=CARTESIAN_POINT('',(-60.75,-18.75,48.));
#43756=CARTESIAN_POINT('Origin',(-56.25,-18.75,48.));
#43757=CARTESIAN_POINT('',(-61.25,-18.75,48.5));
#43758=CARTESIAN_POINT('',(-61.,-18.75,48.25));
#43759=CARTESIAN_POINT('Origin',(-56.25,-18.75,48.5));
#43760=CARTESIAN_POINT('Origin',(-56.25,-18.75,57.));
#43761=CARTESIAN_POINT('',(-60.75,-18.75,43.25));
#43762=CARTESIAN_POINT('',(-60.75,-18.75,57.));
#43763=CARTESIAN_POINT('Origin',(-56.25,-18.75,43.25));
#43764=CARTESIAN_POINT('Origin',(-56.25,-18.75,48.5));
#43765=CARTESIAN_POINT('',(-63.25,-18.75,48.5));
#43766=CARTESIAN_POINT('Origin',(-56.25,-18.75,48.5));
#43767=CARTESIAN_POINT('Origin',(-18.75,18.75,48.25));
#43768=CARTESIAN_POINT('',(-23.25,18.75,48.));
#43769=CARTESIAN_POINT('Origin',(-18.75,18.75,48.));
#43770=CARTESIAN_POINT('',(-23.75,18.75,48.5));
#43771=CARTESIAN_POINT('',(-23.5,18.75,48.25));
#43772=CARTESIAN_POINT('Origin',(-18.75,18.75,48.5));
#43773=CARTESIAN_POINT('Origin',(-18.75,18.75,57.));
#43774=CARTESIAN_POINT('',(-23.25,18.75,43.25));
#43775=CARTESIAN_POINT('',(-23.25,18.75,57.));
#43776=CARTESIAN_POINT('Origin',(-18.75,18.75,43.25));
#43777=CARTESIAN_POINT('Origin',(-18.75,18.75,48.5));
#43778=CARTESIAN_POINT('',(-25.75,18.75,48.5));
#43779=CARTESIAN_POINT('Origin',(-18.75,18.75,48.5));
#43780=CARTESIAN_POINT('Origin',(-18.75,-56.25,48.25));
#43781=CARTESIAN_POINT('',(-23.25,-56.25,48.));
#43782=CARTESIAN_POINT('Origin',(-18.75,-56.25,48.));
#43783=CARTESIAN_POINT('',(-23.75,-56.25,48.5));
#43784=CARTESIAN_POINT('',(-23.5,-56.25,48.25));
#43785=CARTESIAN_POINT('Origin',(-18.75,-56.25,48.5));
#43786=CARTESIAN_POINT('Origin',(-18.75,-56.25,57.));
#43787=CARTESIAN_POINT('',(-23.25,-56.25,43.25));
#43788=CARTESIAN_POINT('',(-23.25,-56.25,57.));
#43789=CARTESIAN_POINT('Origin',(-18.75,-56.25,43.25));
#43790=CARTESIAN_POINT('Origin',(-18.75,-56.25,48.5));
#43791=CARTESIAN_POINT('',(-25.75,-56.25,48.5));
#43792=CARTESIAN_POINT('Origin',(-18.75,-56.25,48.5));
#43793=CARTESIAN_POINT('Origin',(-18.75,-18.75,48.25));
#43794=CARTESIAN_POINT('',(-23.25,-18.75,48.));
#43795=CARTESIAN_POINT('Origin',(-18.75,-18.75,48.));
#43796=CARTESIAN_POINT('',(-23.75,-18.75,48.5));
#43797=CARTESIAN_POINT('',(-23.5,-18.75,48.25));
#43798=CARTESIAN_POINT('Origin',(-18.75,-18.75,48.5));
#43799=CARTESIAN_POINT('Origin',(-18.75,-18.75,57.));
#43800=CARTESIAN_POINT('',(-23.25,-18.75,43.25));
#43801=CARTESIAN_POINT('',(-23.25,-18.75,57.));
#43802=CARTESIAN_POINT('Origin',(-18.75,-18.75,43.25));
#43803=CARTESIAN_POINT('Origin',(-18.75,-18.75,48.5));
#43804=CARTESIAN_POINT('',(-25.75,-18.75,48.5));
#43805=CARTESIAN_POINT('Origin',(-18.75,-18.75,48.5));
#43806=CARTESIAN_POINT('Origin',(18.75,-56.25,48.25));
#43807=CARTESIAN_POINT('',(14.25,-56.25,48.));
#43808=CARTESIAN_POINT('Origin',(18.75,-56.25,48.));
#43809=CARTESIAN_POINT('',(13.75,-56.25,48.5));
#43810=CARTESIAN_POINT('',(14.,-56.25,48.25));
#43811=CARTESIAN_POINT('Origin',(18.75,-56.25,48.5));
#43812=CARTESIAN_POINT('Origin',(18.75,-56.25,57.));
#43813=CARTESIAN_POINT('',(14.25,-56.25,43.25));
#43814=CARTESIAN_POINT('',(14.25,-56.25,57.));
#43815=CARTESIAN_POINT('Origin',(18.75,-56.25,43.25));
#43816=CARTESIAN_POINT('Origin',(18.75,-56.25,48.5));
#43817=CARTESIAN_POINT('',(11.75,-56.25,48.5));
#43818=CARTESIAN_POINT('Origin',(18.75,-56.25,48.5));
#43819=CARTESIAN_POINT('Origin',(18.75,-18.75,48.25));
#43820=CARTESIAN_POINT('',(14.25,-18.75,48.));
#43821=CARTESIAN_POINT('Origin',(18.75,-18.75,48.));
#43822=CARTESIAN_POINT('',(13.75,-18.75,48.5));
#43823=CARTESIAN_POINT('',(14.,-18.75,48.25));
#43824=CARTESIAN_POINT('Origin',(18.75,-18.75,48.5));
#43825=CARTESIAN_POINT('Origin',(18.75,-18.75,57.));
#43826=CARTESIAN_POINT('',(14.25,-18.75,43.25));
#43827=CARTESIAN_POINT('',(14.25,-18.75,57.));
#43828=CARTESIAN_POINT('Origin',(18.75,-18.75,43.25));
#43829=CARTESIAN_POINT('Origin',(18.75,-18.75,48.5));
#43830=CARTESIAN_POINT('',(11.75,-18.75,48.5));
#43831=CARTESIAN_POINT('Origin',(18.75,-18.75,48.5));
#43832=CARTESIAN_POINT('Origin',(56.25,-18.75,48.25));
#43833=CARTESIAN_POINT('',(51.75,-18.75,48.));
#43834=CARTESIAN_POINT('Origin',(56.25,-18.75,48.));
#43835=CARTESIAN_POINT('',(51.25,-18.75,48.5));
#43836=CARTESIAN_POINT('',(51.5,-18.75,48.25));
#43837=CARTESIAN_POINT('Origin',(56.25,-18.75,48.5));
#43838=CARTESIAN_POINT('Origin',(56.25,-18.75,57.));
#43839=CARTESIAN_POINT('',(51.75,-18.75,43.25));
#43840=CARTESIAN_POINT('',(51.75,-18.75,57.));
#43841=CARTESIAN_POINT('Origin',(56.25,-18.75,43.25));
#43842=CARTESIAN_POINT('Origin',(56.25,-18.75,48.5));
#43843=CARTESIAN_POINT('',(49.25,-18.75,48.5));
#43844=CARTESIAN_POINT('Origin',(56.25,-18.75,48.5));
#43845=CARTESIAN_POINT('Origin',(-52.425,52.425,47.));
#43846=CARTESIAN_POINT('',(-54.425,52.425,47.25));
#43847=CARTESIAN_POINT('Origin',(-52.425,52.425,47.25));
#43848=CARTESIAN_POINT('',(-54.925,52.425,46.75));
#43849=CARTESIAN_POINT('',(-54.675,52.425,47.));
#43850=CARTESIAN_POINT('Origin',(-52.425,52.425,46.75));
#43851=CARTESIAN_POINT('Origin',(-52.425,52.425,57.));
#43852=CARTESIAN_POINT('',(-54.425,52.425,56.5));
#43853=CARTESIAN_POINT('Origin',(-52.425,52.425,56.5));
#43854=CARTESIAN_POINT('',(-54.425,52.425,57.));
#43855=CARTESIAN_POINT('Origin',(-52.425,52.425,46.75));
#43856=CARTESIAN_POINT('',(-56.6629,52.425,46.75));
#43857=CARTESIAN_POINT('Origin',(-52.425,52.425,46.75));
#43858=CARTESIAN_POINT('Origin',(85.475,-85.475,42.75));
#43859=CARTESIAN_POINT('',(85.475,-85.475,56.75));
#43860=CARTESIAN_POINT('',(85.225,-85.725,56.5));
#43861=CARTESIAN_POINT('',(61.7520833333331,-109.197916666667,33.0270833333335));
#43862=CARTESIAN_POINT('',(85.225,-85.725,43.25));
#43863=CARTESIAN_POINT('',(85.225,-85.725,42.75));
#43864=CARTESIAN_POINT('',(85.475,-85.475,43.));
#43865=CARTESIAN_POINT('',(64.1270833333331,-106.822916666667,64.3479166666665));
#43866=CARTESIAN_POINT('',(85.725,-85.225,43.25));
#43867=CARTESIAN_POINT('',(92.5354166666667,-78.4145833333332,50.0604166666666));
#43868=CARTESIAN_POINT('',(85.725,-85.225,56.5));
#43869=CARTESIAN_POINT('',(85.725,-85.225,42.75));
#43870=CARTESIAN_POINT('',(94.9104166666667,-76.0395833333332,47.3145833333334));
#43871=CARTESIAN_POINT('Origin',(85.475,-42.8625,56.75));
#43872=CARTESIAN_POINT('',(85.725,85.225,56.5));
#43873=CARTESIAN_POINT('',(85.725,-42.8625,56.5));
#43874=CARTESIAN_POINT('',(85.475,85.475,56.75));
#43875=CARTESIAN_POINT('',(109.197916666667,61.7520833333331,33.0270833333335));
#43876=CARTESIAN_POINT('',(85.225,85.225,57.));
#43877=CARTESIAN_POINT('',(85.225,85.225,57.));
#43878=CARTESIAN_POINT('',(85.225,-85.225,57.));
#43879=CARTESIAN_POINT('',(85.225,-42.8625,57.));
#43880=CARTESIAN_POINT('',(85.225,-85.225,57.));
#43881=CARTESIAN_POINT('Origin',(85.725,-85.725,42.75));
#43882=CARTESIAN_POINT('',(85.725,85.225,43.25));
#43883=CARTESIAN_POINT('',(85.725,-42.8625,43.25));
#43884=CARTESIAN_POINT('',(85.725,85.225,42.75));
#43885=CARTESIAN_POINT('Origin',(85.475,-42.8625,43.));
#43886=CARTESIAN_POINT('',(85.225,-85.225,42.75));
#43887=CARTESIAN_POINT('',(85.225,-85.225,42.75));
#43888=CARTESIAN_POINT('',(85.225,85.225,42.75));
#43889=CARTESIAN_POINT('',(85.225,-42.8625,42.75));
#43890=CARTESIAN_POINT('',(85.475,85.475,43.));
#43891=CARTESIAN_POINT('',(85.225,85.225,42.75));
#43892=CARTESIAN_POINT('',(106.822916666667,64.1270833333331,64.3479166666665));
#43893=CARTESIAN_POINT('Origin',(-18.75,56.25,45.75));
#43894=CARTESIAN_POINT('',(-22.25,56.25,45.5));
#43895=CARTESIAN_POINT('Origin',(-18.75,56.25,45.5));
#43896=CARTESIAN_POINT('',(-22.75,56.25,46.));
#43897=CARTESIAN_POINT('',(-22.5,56.25,45.75));
#43898=CARTESIAN_POINT('Origin',(-18.75,56.25,46.));
#43899=CARTESIAN_POINT('Origin',(-18.75,56.25,57.));
#43900=CARTESIAN_POINT('',(-22.25,56.25,43.25));
#43901=CARTESIAN_POINT('',(-22.25,56.25,57.));
#43902=CARTESIAN_POINT('Origin',(-18.75,56.25,43.25));
#43903=CARTESIAN_POINT('Origin',(-18.75,56.25,46.));
#43904=CARTESIAN_POINT('',(-25.25,56.25,46.));
#43905=CARTESIAN_POINT('Origin',(-18.75,56.25,46.));
#43906=CARTESIAN_POINT('Origin',(-56.25,18.75,45.75));
#43907=CARTESIAN_POINT('',(-59.75,18.75,45.5));
#43908=CARTESIAN_POINT('Origin',(-56.25,18.75,45.5));
#43909=CARTESIAN_POINT('',(-60.25,18.75,46.));
#43910=CARTESIAN_POINT('',(-60.,18.75,45.75));
#43911=CARTESIAN_POINT('Origin',(-56.25,18.75,46.));
#43912=CARTESIAN_POINT('Origin',(-56.25,18.75,57.));
#43913=CARTESIAN_POINT('',(-59.75,18.75,43.25));
#43914=CARTESIAN_POINT('',(-59.75,18.75,57.));
#43915=CARTESIAN_POINT('Origin',(-56.25,18.75,43.25));
#43916=CARTESIAN_POINT('Origin',(-56.25,18.75,46.));
#43917=CARTESIAN_POINT('',(-62.75,18.75,46.));
#43918=CARTESIAN_POINT('Origin',(-56.25,18.75,46.));
#43919=CARTESIAN_POINT('Origin',(-85.475,-85.475,42.75));
#43920=CARTESIAN_POINT('',(-85.475,-85.475,56.75));
#43921=CARTESIAN_POINT('',(-85.725,-85.225,56.5));
#43922=CARTESIAN_POINT('',(-109.197916666667,-61.7520833333331,33.0270833333335));
#43923=CARTESIAN_POINT('',(-85.725,-85.225,43.25));
#43924=CARTESIAN_POINT('',(-85.725,-85.225,42.75));
#43925=CARTESIAN_POINT('',(-85.475,-85.475,43.));
#43926=CARTESIAN_POINT('',(-106.822916666667,-64.1270833333331,64.3479166666665));
#43927=CARTESIAN_POINT('',(-85.225,-85.725,43.25));
#43928=CARTESIAN_POINT('',(-78.4145833333332,-92.5354166666667,50.0604166666666));
#43929=CARTESIAN_POINT('',(-85.225,-85.725,56.5));
#43930=CARTESIAN_POINT('',(-85.225,-85.725,42.75));
#43931=CARTESIAN_POINT('',(-76.0395833333332,-94.9104166666667,47.3145833333334));
#43932=CARTESIAN_POINT('Origin',(-85.475,42.8625,43.));
#43933=CARTESIAN_POINT('',(-85.725,85.225,43.25));
#43934=CARTESIAN_POINT('',(-85.725,42.8625,43.25));
#43935=CARTESIAN_POINT('',(-85.475,85.475,43.));
#43936=CARTESIAN_POINT('',(-92.5354166666667,78.4145833333332,50.0604166666666));
#43937=CARTESIAN_POINT('',(-85.225,85.225,42.75));
#43938=CARTESIAN_POINT('',(-85.725,85.725,43.25));
#43939=CARTESIAN_POINT('',(-85.225,-85.225,42.75));
#43940=CARTESIAN_POINT('',(-85.225,42.8625,42.75));
#43941=CARTESIAN_POINT('',(-85.225,-85.225,42.75));
#43942=CARTESIAN_POINT('Origin',(-85.725,85.725,42.75));
#43943=CARTESIAN_POINT('',(-85.725,85.225,56.5));
#43944=CARTESIAN_POINT('',(-85.725,42.8625,56.5));
#43945=CARTESIAN_POINT('',(-85.725,85.225,42.75));
#43946=CARTESIAN_POINT('Origin',(-85.475,42.8625,56.75));
#43947=CARTESIAN_POINT('',(-85.225,-85.225,57.));
#43948=CARTESIAN_POINT('',(-85.225,-85.225,57.));
#43949=CARTESIAN_POINT('',(-85.225,85.225,57.));
#43950=CARTESIAN_POINT('',(-85.225,42.8625,57.));
#43951=CARTESIAN_POINT('',(-85.475,85.475,56.75));
#43952=CARTESIAN_POINT('',(-85.225,85.225,57.));
#43953=CARTESIAN_POINT('',(-94.9104166666667,76.0395833333332,47.3145833333334));
#43954=CARTESIAN_POINT('Origin',(85.475,85.475,42.75));
#43955=CARTESIAN_POINT('',(85.225,85.725,43.25));
#43956=CARTESIAN_POINT('',(78.4145833333332,92.5354166666667,50.0604166666666));
#43957=CARTESIAN_POINT('',(85.225,85.725,56.5));
#43958=CARTESIAN_POINT('',(85.225,85.725,42.75));
#43959=CARTESIAN_POINT('',(76.0395833333332,94.9104166666667,47.3145833333334));
#43960=CARTESIAN_POINT('Origin',(-85.475,85.475,42.75));
#43961=CARTESIAN_POINT('',(-85.225,85.725,56.5));
#43962=CARTESIAN_POINT('',(-61.7520833333331,109.197916666667,33.0270833333335));
#43963=CARTESIAN_POINT('',(-85.225,85.725,43.25));
#43964=CARTESIAN_POINT('',(-85.225,85.725,42.75));
#43965=CARTESIAN_POINT('',(-64.1270833333331,106.822916666667,64.3479166666665));
#43966=CARTESIAN_POINT('Origin',(56.25,18.75,48.25));
#43967=CARTESIAN_POINT('',(51.75,18.75,48.));
#43968=CARTESIAN_POINT('Origin',(56.25,18.75,48.));
#43969=CARTESIAN_POINT('',(51.25,18.75,48.5));
#43970=CARTESIAN_POINT('',(51.5,18.75,48.25));
#43971=CARTESIAN_POINT('Origin',(56.25,18.75,48.5));
#43972=CARTESIAN_POINT('Origin',(56.25,18.75,57.));
#43973=CARTESIAN_POINT('',(51.75,18.75,43.25));
#43974=CARTESIAN_POINT('',(51.75,18.75,57.));
#43975=CARTESIAN_POINT('Origin',(56.25,18.75,43.25));
#43976=CARTESIAN_POINT('Origin',(56.25,18.75,48.5));
#43977=CARTESIAN_POINT('',(49.25,18.75,48.5));
#43978=CARTESIAN_POINT('Origin',(56.25,18.75,48.5));
#43979=CARTESIAN_POINT('Origin',(18.75,56.25,48.25));
#43980=CARTESIAN_POINT('',(14.25,56.25,48.));
#43981=CARTESIAN_POINT('Origin',(18.75,56.25,48.));
#43982=CARTESIAN_POINT('',(13.75,56.25,48.5));
#43983=CARTESIAN_POINT('',(14.,56.25,48.25));
#43984=CARTESIAN_POINT('Origin',(18.75,56.25,48.5));
#43985=CARTESIAN_POINT('Origin',(18.75,56.25,57.));
#43986=CARTESIAN_POINT('',(14.25,56.25,43.25));
#43987=CARTESIAN_POINT('',(14.25,56.25,57.));
#43988=CARTESIAN_POINT('Origin',(18.75,56.25,43.25));
#43989=CARTESIAN_POINT('Origin',(18.75,56.25,48.5));
#43990=CARTESIAN_POINT('',(11.75,56.25,48.5));
#43991=CARTESIAN_POINT('Origin',(18.75,56.25,48.5));
#43992=CARTESIAN_POINT('Origin',(18.75,-18.75,43.));
#43993=CARTESIAN_POINT('',(13.75,-18.75,42.75));
#43994=CARTESIAN_POINT('Origin',(18.75,-18.75,42.75));
#43995=CARTESIAN_POINT('',(14.,-18.75,43.));
#43996=CARTESIAN_POINT('Origin',(0.,0.,42.75));
#43997=CARTESIAN_POINT('',(42.8625,85.225,42.75));
#43998=CARTESIAN_POINT('',(-42.8625,-85.225,42.75));
#43999=CARTESIAN_POINT('',(13.75,-56.25,42.75));
#44000=CARTESIAN_POINT('Origin',(18.75,-56.25,42.75));
#44001=CARTESIAN_POINT('',(-23.75,-56.25,42.75));
#44002=CARTESIAN_POINT('Origin',(-18.75,-56.25,42.75));
#44003=CARTESIAN_POINT('',(-61.25,-18.75,42.75));
#44004=CARTESIAN_POINT('Origin',(-56.25,-18.75,42.75));
#44005=CARTESIAN_POINT('',(51.25,-18.75,42.75));
#44006=CARTESIAN_POINT('Origin',(56.25,-18.75,42.75));
#44007=CARTESIAN_POINT('',(-59.975,-52.425,42.75));
#44008=CARTESIAN_POINT('Origin',(-52.425,-52.425,42.75));
#44009=CARTESIAN_POINT('',(51.25,18.75,42.75));
#44010=CARTESIAN_POINT('Origin',(56.25,18.75,42.75));
#44011=CARTESIAN_POINT('',(-42.05,56.25,42.75));
#44012=CARTESIAN_POINT('Origin',(-37.5,56.25,42.75));
#44013=CARTESIAN_POINT('',(-60.8,37.5,42.75));
#44014=CARTESIAN_POINT('Origin',(-56.25,37.5,42.75));
#44015=CARTESIAN_POINT('',(-23.3,-37.5,42.75));
#44016=CARTESIAN_POINT('Origin',(-18.75,-37.5,42.75));
#44017=CARTESIAN_POINT('',(-4.55,-18.75,42.75));
#44018=CARTESIAN_POINT('Origin',(0.,-18.75,42.75));
#44019=CARTESIAN_POINT('',(14.2,-37.5,42.75));
#44020=CARTESIAN_POINT('Origin',(18.75,-37.5,42.75));
#44021=CARTESIAN_POINT('',(32.95,-18.75,42.75));
#44022=CARTESIAN_POINT('Origin',(37.5,-18.75,42.75));
#44023=CARTESIAN_POINT('',(-60.25,18.75,42.75));
#44024=CARTESIAN_POINT('Origin',(-56.25,18.75,42.75));
#44025=CARTESIAN_POINT('',(-23.3,5.57214293612046E-16,42.75));
#44026=CARTESIAN_POINT('Origin',(-18.75,0.,42.75));
#44027=CARTESIAN_POINT('',(-60.8,5.57214293612046E-16,42.75));
#44028=CARTESIAN_POINT('Origin',(-56.25,0.,42.75));
#44029=CARTESIAN_POINT('',(14.2,5.57214293612045E-16,42.75));
#44030=CARTESIAN_POINT('Origin',(18.75,0.,42.75));
#44031=CARTESIAN_POINT('',(32.95,18.75,42.75));
#44032=CARTESIAN_POINT('Origin',(37.5,18.75,42.75));
#44033=CARTESIAN_POINT('',(29.5,-37.5,42.75));
#44034=CARTESIAN_POINT('Origin',(37.5,-37.5,42.75));
#44035=CARTESIAN_POINT('',(-8.,-37.5,42.75));
#44036=CARTESIAN_POINT('Origin',(0.,-37.5,42.75));
#44037=CARTESIAN_POINT('',(-8.,9.79717439317883E-16,42.75));
#44038=CARTESIAN_POINT('Origin',(0.,0.,42.75));
#44039=CARTESIAN_POINT('',(29.5,9.79717439317882E-16,42.75));
#44040=CARTESIAN_POINT('Origin',(37.5,0.,42.75));
#44041=CARTESIAN_POINT('',(-56.6629,52.425,42.75));
#44042=CARTESIAN_POINT('Origin',(-52.425,52.425,42.75));
#44043=CARTESIAN_POINT('',(-8.,37.5,42.75));
#44044=CARTESIAN_POINT('Origin',(0.,37.5,42.75));
#44045=CARTESIAN_POINT('',(-45.5,37.5,42.75));
#44046=CARTESIAN_POINT('Origin',(-37.5,37.5,42.75));
#44047=CARTESIAN_POINT('',(-45.5,9.79717439317882E-16,42.75));
#44048=CARTESIAN_POINT('Origin',(-37.5,0.,42.75));
#44049=CARTESIAN_POINT('',(51.7,5.57214293612046E-16,42.75));
#44050=CARTESIAN_POINT('Origin',(56.25,0.,42.75));
#44051=CARTESIAN_POINT('',(32.95,-56.25,42.75));
#44052=CARTESIAN_POINT('Origin',(37.5,-56.25,42.75));
#44053=CARTESIAN_POINT('',(-4.55,56.25,42.75));
#44054=CARTESIAN_POINT('Origin',(0.,56.25,42.75));
#44055=CARTESIAN_POINT('',(-4.55,-56.25,42.75));
#44056=CARTESIAN_POINT('Origin',(0.,-56.25,42.75));
#44057=CARTESIAN_POINT('',(-22.75,56.25,42.75));
#44058=CARTESIAN_POINT('Origin',(-18.75,56.25,42.75));
#44059=CARTESIAN_POINT('',(51.7,-37.5,42.75));
#44060=CARTESIAN_POINT('Origin',(56.25,-37.5,42.75));
#44061=CARTESIAN_POINT('',(14.2,37.5,42.75));
#44062=CARTESIAN_POINT('Origin',(18.75,37.5,42.75));
#44063=CARTESIAN_POINT('',(-4.55,18.75,42.75));
#44064=CARTESIAN_POINT('Origin',(0.,18.75,42.75));
#44065=CARTESIAN_POINT('',(-23.3,37.5,42.75));
#44066=CARTESIAN_POINT('Origin',(-18.75,37.5,42.75));
#44067=CARTESIAN_POINT('',(-42.05,18.75,42.75));
#44068=CARTESIAN_POINT('Origin',(-37.5,18.75,42.75));
#44069=CARTESIAN_POINT('',(-42.05,-18.75,42.75));
#44070=CARTESIAN_POINT('Origin',(-37.5,-18.75,42.75));
#44071=CARTESIAN_POINT('',(13.75,56.25,42.75));
#44072=CARTESIAN_POINT('Origin',(18.75,56.25,42.75));
#44073=CARTESIAN_POINT('',(44.875,52.425,42.75));
#44074=CARTESIAN_POINT('Origin',(52.425,52.425,42.75));
#44075=CARTESIAN_POINT('',(13.75,18.75,42.75));
#44076=CARTESIAN_POINT('Origin',(18.75,18.75,42.75));
#44077=CARTESIAN_POINT('',(-23.75,18.75,42.75));
#44078=CARTESIAN_POINT('Origin',(-18.75,18.75,42.75));
#44079=CARTESIAN_POINT('',(-23.75,-18.75,42.75));
#44080=CARTESIAN_POINT('Origin',(-18.75,-18.75,42.75));
#44081=CARTESIAN_POINT('Origin',(18.75,-56.25,43.));
#44082=CARTESIAN_POINT('',(14.,-56.25,43.));
#44083=CARTESIAN_POINT('Origin',(-18.75,-18.75,43.));
#44084=CARTESIAN_POINT('',(-23.5,-18.75,43.));
#44085=CARTESIAN_POINT('Origin',(-18.75,-56.25,43.));
#44086=CARTESIAN_POINT('',(-23.5,-56.25,43.));
#44087=CARTESIAN_POINT('Origin',(-18.75,18.75,43.));
#44088=CARTESIAN_POINT('',(-23.5,18.75,43.));
#44089=CARTESIAN_POINT('Origin',(-56.25,-18.75,43.));
#44090=CARTESIAN_POINT('',(-61.,-18.75,43.));
#44091=CARTESIAN_POINT('Origin',(18.75,18.75,43.));
#44092=CARTESIAN_POINT('',(14.,18.75,43.));
#44093=CARTESIAN_POINT('Origin',(56.25,-18.75,43.));
#44094=CARTESIAN_POINT('',(51.5,-18.75,43.));
#44095=CARTESIAN_POINT('Origin',(52.425,52.425,43.));
#44096=CARTESIAN_POINT('',(45.375,52.425,43.25));
#44097=CARTESIAN_POINT('',(45.125,52.425,43.));
#44098=CARTESIAN_POINT('Origin',(52.425,52.425,43.25));
#44099=CARTESIAN_POINT('Origin',(52.425,52.425,57.));
#44100=CARTESIAN_POINT('',(45.375,52.425,56.5));
#44101=CARTESIAN_POINT('Origin',(52.425,52.425,56.5));
#44102=CARTESIAN_POINT('',(45.375,52.425,57.));
#44103=CARTESIAN_POINT('Origin',(-52.425,-52.425,43.));
#44104=CARTESIAN_POINT('',(-59.475,-52.425,43.25));
#44105=CARTESIAN_POINT('',(-59.725,-52.425,43.));
#44106=CARTESIAN_POINT('Origin',(-52.425,-52.425,43.25));
#44107=CARTESIAN_POINT('Origin',(-52.425,-52.425,57.));
#44108=CARTESIAN_POINT('',(-59.475,-52.425,56.5));
#44109=CARTESIAN_POINT('Origin',(-52.425,-52.425,56.5));
#44110=CARTESIAN_POINT('',(-59.475,-52.425,57.));
#44111=CARTESIAN_POINT('Origin',(18.75,56.25,43.));
#44112=CARTESIAN_POINT('',(14.,56.25,43.));
#44113=CARTESIAN_POINT('Origin',(56.25,18.75,43.));
#44114=CARTESIAN_POINT('',(51.5,18.75,43.));
#44115=CARTESIAN_POINT('Origin',(42.8625,85.475,43.));
#44116=CARTESIAN_POINT('',(42.8625,85.725,43.25));
#44117=CARTESIAN_POINT('Origin',(-42.8625,-85.475,43.));
#44118=CARTESIAN_POINT('',(-42.8625,-85.725,43.25));
#44119=CARTESIAN_POINT('Origin',(85.725,85.725,42.75));
#44120=CARTESIAN_POINT('',(42.8625,85.725,56.5));
#44121=CARTESIAN_POINT('Origin',(-37.5,56.25,43.));
#44122=CARTESIAN_POINT('',(-41.55,56.25,43.25));
#44123=CARTESIAN_POINT('',(-41.8,56.25,43.));
#44124=CARTESIAN_POINT('Origin',(-37.5,56.25,43.25));
#44125=CARTESIAN_POINT('Origin',(-37.5,56.25,57.));
#44126=CARTESIAN_POINT('',(-41.55,56.25,56.5));
#44127=CARTESIAN_POINT('Origin',(-37.5,56.25,56.5));
#44128=CARTESIAN_POINT('',(-41.55,56.25,57.));
#44129=CARTESIAN_POINT('Origin',(-37.5,-18.75,43.));
#44130=CARTESIAN_POINT('',(-41.55,-18.75,43.25));
#44131=CARTESIAN_POINT('',(-41.8,-18.75,43.));
#44132=CARTESIAN_POINT('Origin',(-37.5,-18.75,43.25));
#44133=CARTESIAN_POINT('Origin',(-37.5,-18.75,57.));
#44134=CARTESIAN_POINT('',(-41.55,-18.75,56.5));
#44135=CARTESIAN_POINT('Origin',(-37.5,-18.75,56.5));
#44136=CARTESIAN_POINT('',(-41.55,-18.75,57.));
#44137=CARTESIAN_POINT('Origin',(-56.25,37.5,43.));
#44138=CARTESIAN_POINT('',(-60.3,37.5,43.25));
#44139=CARTESIAN_POINT('',(-60.55,37.5,43.));
#44140=CARTESIAN_POINT('Origin',(-56.25,37.5,43.25));
#44141=CARTESIAN_POINT('Origin',(-56.25,37.5,57.));
#44142=CARTESIAN_POINT('',(-60.3,37.5,56.5));
#44143=CARTESIAN_POINT('Origin',(-56.25,37.5,56.5));
#44144=CARTESIAN_POINT('',(-60.3,37.5,57.));
#44145=CARTESIAN_POINT('Origin',(-37.5,18.75,43.));
#44146=CARTESIAN_POINT('',(-41.55,18.75,43.25));
#44147=CARTESIAN_POINT('',(-41.8,18.75,43.));
#44148=CARTESIAN_POINT('Origin',(-37.5,18.75,43.25));
#44149=CARTESIAN_POINT('Origin',(-37.5,18.75,57.));
#44150=CARTESIAN_POINT('',(-41.55,18.75,56.5));
#44151=CARTESIAN_POINT('Origin',(-37.5,18.75,56.5));
#44152=CARTESIAN_POINT('',(-41.55,18.75,57.));
#44153=CARTESIAN_POINT('Origin',(-18.75,-37.5,43.));
#44154=CARTESIAN_POINT('',(-22.8,-37.5,43.25));
#44155=CARTESIAN_POINT('',(-23.05,-37.5,43.));
#44156=CARTESIAN_POINT('Origin',(-18.75,-37.5,43.25));
#44157=CARTESIAN_POINT('Origin',(-18.75,-37.5,57.));
#44158=CARTESIAN_POINT('',(-22.8,-37.5,56.5));
#44159=CARTESIAN_POINT('Origin',(-18.75,-37.5,56.5));
#44160=CARTESIAN_POINT('',(-22.8,-37.5,57.));
#44161=CARTESIAN_POINT('Origin',(-18.75,37.5,43.));
#44162=CARTESIAN_POINT('',(-22.8,37.5,43.25));
#44163=CARTESIAN_POINT('',(-23.05,37.5,43.));
#44164=CARTESIAN_POINT('Origin',(-18.75,37.5,43.25));
#44165=CARTESIAN_POINT('Origin',(-18.75,37.5,57.));
#44166=CARTESIAN_POINT('',(-22.8,37.5,56.5));
#44167=CARTESIAN_POINT('Origin',(-18.75,37.5,56.5));
#44168=CARTESIAN_POINT('',(-22.8,37.5,57.));
#44169=CARTESIAN_POINT('Origin',(0.,-18.75,43.));
#44170=CARTESIAN_POINT('',(-4.05,-18.75,43.25));
#44171=CARTESIAN_POINT('',(-4.3,-18.75,43.));
#44172=CARTESIAN_POINT('Origin',(0.,-18.75,43.25));
#44173=CARTESIAN_POINT('Origin',(0.,-18.75,57.));
#44174=CARTESIAN_POINT('',(-4.05,-18.75,56.5));
#44175=CARTESIAN_POINT('Origin',(0.,-18.75,56.5));
#44176=CARTESIAN_POINT('',(-4.05,-18.75,57.));
#44177=CARTESIAN_POINT('Origin',(0.,18.75,43.));
#44178=CARTESIAN_POINT('',(-4.05,18.75,43.25));
#44179=CARTESIAN_POINT('',(-4.3,18.75,43.));
#44180=CARTESIAN_POINT('Origin',(0.,18.75,43.25));
#44181=CARTESIAN_POINT('Origin',(0.,18.75,57.));
#44182=CARTESIAN_POINT('',(-4.05,18.75,56.5));
#44183=CARTESIAN_POINT('Origin',(0.,18.75,56.5));
#44184=CARTESIAN_POINT('',(-4.05,18.75,57.));
#44185=CARTESIAN_POINT('Origin',(18.75,-37.5,43.));
#44186=CARTESIAN_POINT('',(14.7,-37.5,43.25));
#44187=CARTESIAN_POINT('',(14.45,-37.5,43.));
#44188=CARTESIAN_POINT('Origin',(18.75,-37.5,43.25));
#44189=CARTESIAN_POINT('Origin',(18.75,-37.5,57.));
#44190=CARTESIAN_POINT('',(14.7,-37.5,56.5));
#44191=CARTESIAN_POINT('Origin',(18.75,-37.5,56.5));
#44192=CARTESIAN_POINT('',(14.7,-37.5,57.));
#44193=CARTESIAN_POINT('Origin',(18.75,37.5,43.));
#44194=CARTESIAN_POINT('',(14.7,37.5,43.25));
#44195=CARTESIAN_POINT('',(14.45,37.5,43.));
#44196=CARTESIAN_POINT('Origin',(18.75,37.5,43.25));
#44197=CARTESIAN_POINT('Origin',(18.75,37.5,57.));
#44198=CARTESIAN_POINT('',(14.7,37.5,56.5));
#44199=CARTESIAN_POINT('Origin',(18.75,37.5,56.5));
#44200=CARTESIAN_POINT('',(14.7,37.5,57.));
#44201=CARTESIAN_POINT('Origin',(37.5,-18.75,43.));
#44202=CARTESIAN_POINT('',(33.45,-18.75,43.25));
#44203=CARTESIAN_POINT('',(33.2,-18.75,43.));
#44204=CARTESIAN_POINT('Origin',(37.5,-18.75,43.25));
#44205=CARTESIAN_POINT('Origin',(37.5,-18.75,57.));
#44206=CARTESIAN_POINT('',(33.45,-18.75,56.5));
#44207=CARTESIAN_POINT('Origin',(37.5,-18.75,56.5));
#44208=CARTESIAN_POINT('',(33.45,-18.75,57.));
#44209=CARTESIAN_POINT('Origin',(56.25,-37.5,43.));
#44210=CARTESIAN_POINT('',(52.2,-37.5,43.25));
#44211=CARTESIAN_POINT('',(51.95,-37.5,43.));
#44212=CARTESIAN_POINT('Origin',(56.25,-37.5,43.25));
#44213=CARTESIAN_POINT('Origin',(56.25,-37.5,57.));
#44214=CARTESIAN_POINT('',(52.2,-37.5,56.5));
#44215=CARTESIAN_POINT('Origin',(56.25,-37.5,56.5));
#44216=CARTESIAN_POINT('',(52.2,-37.5,57.));
#44217=CARTESIAN_POINT('Origin',(-56.25,18.75,43.));
#44218=CARTESIAN_POINT('',(-60.,18.75,43.));
#44219=CARTESIAN_POINT('Origin',(-18.75,56.25,43.));
#44220=CARTESIAN_POINT('',(-22.5,56.25,43.));
#44221=CARTESIAN_POINT('Origin',(-18.75,0.,43.));
#44222=CARTESIAN_POINT('',(-22.8,-4.95981953654678E-16,43.25));
#44223=CARTESIAN_POINT('',(-23.05,5.26598123633362E-16,43.));
#44224=CARTESIAN_POINT('Origin',(-18.75,0.,43.25));
#44225=CARTESIAN_POINT('Origin',(-18.75,0.,57.));
#44226=CARTESIAN_POINT('',(-22.8,4.95981953654678E-16,56.5));
#44227=CARTESIAN_POINT('Origin',(-18.75,0.,56.5));
#44228=CARTESIAN_POINT('',(-22.8,4.95981953654678E-16,57.));
#44229=CARTESIAN_POINT('Origin',(0.,-56.25,43.));
#44230=CARTESIAN_POINT('',(-4.05,-56.25,43.25));
#44231=CARTESIAN_POINT('',(-4.3,-56.25,43.));
#44232=CARTESIAN_POINT('Origin',(0.,-56.25,43.25));
#44233=CARTESIAN_POINT('Origin',(0.,-56.25,57.));
#44234=CARTESIAN_POINT('',(-4.05,-56.25,56.5));
#44235=CARTESIAN_POINT('Origin',(0.,-56.25,56.5));
#44236=CARTESIAN_POINT('',(-4.05,-56.25,57.));
#44237=CARTESIAN_POINT('Origin',(-56.25,0.,43.));
#44238=CARTESIAN_POINT('',(-60.3,-4.95981953654678E-16,43.25));
#44239=CARTESIAN_POINT('',(-60.55,5.26598123633362E-16,43.));
#44240=CARTESIAN_POINT('Origin',(-56.25,0.,43.25));
#44241=CARTESIAN_POINT('Origin',(-56.25,0.,57.));
#44242=CARTESIAN_POINT('',(-60.3,4.95981953654678E-16,56.5));
#44243=CARTESIAN_POINT('Origin',(-56.25,0.,56.5));
#44244=CARTESIAN_POINT('',(-60.3,4.95981953654678E-16,57.));
#44245=CARTESIAN_POINT('Origin',(0.,56.25,43.));
#44246=CARTESIAN_POINT('',(-4.05,56.25,43.25));
#44247=CARTESIAN_POINT('',(-4.3,56.25,43.));
#44248=CARTESIAN_POINT('Origin',(0.,56.25,43.25));
#44249=CARTESIAN_POINT('Origin',(0.,56.25,57.));
#44250=CARTESIAN_POINT('',(-4.05,56.25,56.5));
#44251=CARTESIAN_POINT('Origin',(0.,56.25,56.5));
#44252=CARTESIAN_POINT('',(-4.05,56.25,57.));
#44253=CARTESIAN_POINT('Origin',(18.75,0.,43.));
#44254=CARTESIAN_POINT('',(14.7,-4.95981953654678E-16,43.25));
#44255=CARTESIAN_POINT('',(14.45,5.26598123633362E-16,43.));
#44256=CARTESIAN_POINT('Origin',(18.75,0.,43.25));
#44257=CARTESIAN_POINT('Origin',(18.75,0.,57.));
#44258=CARTESIAN_POINT('',(14.7,4.95981953654678E-16,56.5));
#44259=CARTESIAN_POINT('Origin',(18.75,0.,56.5));
#44260=CARTESIAN_POINT('',(14.7,4.95981953654678E-16,57.));
#44261=CARTESIAN_POINT('Origin',(37.5,-56.25,43.));
#44262=CARTESIAN_POINT('',(33.45,-56.25,43.25));
#44263=CARTESIAN_POINT('',(33.2,-56.25,43.));
#44264=CARTESIAN_POINT('Origin',(37.5,-56.25,43.25));
#44265=CARTESIAN_POINT('Origin',(37.5,-56.25,57.));
#44266=CARTESIAN_POINT('',(33.45,-56.25,56.5));
#44267=CARTESIAN_POINT('Origin',(37.5,-56.25,56.5));
#44268=CARTESIAN_POINT('',(33.45,-56.25,57.));
#44269=CARTESIAN_POINT('Origin',(37.5,18.75,43.));
#44270=CARTESIAN_POINT('',(33.45,18.75,43.25));
#44271=CARTESIAN_POINT('',(33.2,18.75,43.));
#44272=CARTESIAN_POINT('Origin',(37.5,18.75,43.25));
#44273=CARTESIAN_POINT('Origin',(37.5,18.75,57.));
#44274=CARTESIAN_POINT('',(33.45,18.75,56.5));
#44275=CARTESIAN_POINT('Origin',(37.5,18.75,56.5));
#44276=CARTESIAN_POINT('',(33.45,18.75,57.));
#44277=CARTESIAN_POINT('Origin',(56.25,0.,43.));
#44278=CARTESIAN_POINT('',(52.2,-4.95981953654678E-16,43.25));
#44279=CARTESIAN_POINT('',(51.95,5.26598123633362E-16,43.));
#44280=CARTESIAN_POINT('Origin',(56.25,0.,43.25));
#44281=CARTESIAN_POINT('Origin',(56.25,0.,57.));
#44282=CARTESIAN_POINT('',(52.2,4.95981953654678E-16,56.5));
#44283=CARTESIAN_POINT('Origin',(56.25,0.,56.5));
#44284=CARTESIAN_POINT('',(52.2,4.95981953654678E-16,57.));
#44285=CARTESIAN_POINT('Origin',(37.5,-37.5,43.));
#44286=CARTESIAN_POINT('',(30.,-37.5,43.25));
#44287=CARTESIAN_POINT('',(29.75,-37.5,43.));
#44288=CARTESIAN_POINT('Origin',(37.5,-37.5,43.25));
#44289=CARTESIAN_POINT('Origin',(37.5,-37.5,57.));
#44290=CARTESIAN_POINT('',(30.,-37.5,56.5));
#44291=CARTESIAN_POINT('Origin',(37.5,-37.5,56.5));
#44292=CARTESIAN_POINT('',(30.,-37.5,57.));
#44293=CARTESIAN_POINT('Origin',(-37.5,0.,43.));
#44294=CARTESIAN_POINT('',(-45.,-9.18485099360515E-16,43.25));
#44295=CARTESIAN_POINT('',(-45.25,9.49101269339199E-16,43.));
#44296=CARTESIAN_POINT('Origin',(-37.5,0.,43.25));
#44297=CARTESIAN_POINT('Origin',(-37.5,0.,57.));
#44298=CARTESIAN_POINT('',(-45.,9.18485099360515E-16,56.5));
#44299=CARTESIAN_POINT('Origin',(-37.5,0.,56.5));
#44300=CARTESIAN_POINT('',(-45.,9.18485099360515E-16,57.));
#44301=CARTESIAN_POINT('Origin',(0.,-37.5,43.));
#44302=CARTESIAN_POINT('',(-7.5,-37.5,43.25));
#44303=CARTESIAN_POINT('',(-7.75,-37.5,43.));
#44304=CARTESIAN_POINT('Origin',(0.,-37.5,43.25));
#44305=CARTESIAN_POINT('Origin',(0.,-37.5,57.));
#44306=CARTESIAN_POINT('',(-7.5,-37.5,56.5));
#44307=CARTESIAN_POINT('Origin',(0.,-37.5,56.5));
#44308=CARTESIAN_POINT('',(-7.5,-37.5,57.));
#44309=CARTESIAN_POINT('Origin',(-37.5,37.5,43.));
#44310=CARTESIAN_POINT('',(-45.,37.5,43.25));
#44311=CARTESIAN_POINT('',(-45.25,37.5,43.));
#44312=CARTESIAN_POINT('Origin',(-37.5,37.5,43.25));
#44313=CARTESIAN_POINT('Origin',(-37.5,37.5,57.));
#44314=CARTESIAN_POINT('',(-45.,37.5,56.5));
#44315=CARTESIAN_POINT('Origin',(-37.5,37.5,56.5));
#44316=CARTESIAN_POINT('',(-45.,37.5,57.));
#44317=CARTESIAN_POINT('Origin',(0.,0.,43.));
#44318=CARTESIAN_POINT('',(-7.5,-9.18485099360515E-16,43.25));
#44319=CARTESIAN_POINT('',(-7.75,9.49101269339199E-16,43.));
#44320=CARTESIAN_POINT('Origin',(0.,0.,43.25));
#44321=CARTESIAN_POINT('Origin',(0.,0.,57.));
#44322=CARTESIAN_POINT('',(-7.5,9.18485099360515E-16,56.5));
#44323=CARTESIAN_POINT('Origin',(0.,0.,56.5));
#44324=CARTESIAN_POINT('',(-7.5,9.18485099360515E-16,57.));
#44325=CARTESIAN_POINT('Origin',(0.,37.5,43.));
#44326=CARTESIAN_POINT('',(-7.5,37.5,43.25));
#44327=CARTESIAN_POINT('',(-7.75,37.5,43.));
#44328=CARTESIAN_POINT('Origin',(0.,37.5,43.25));
#44329=CARTESIAN_POINT('Origin',(0.,37.5,57.));
#44330=CARTESIAN_POINT('',(-7.5,37.5,56.5));
#44331=CARTESIAN_POINT('Origin',(0.,37.5,56.5));
#44332=CARTESIAN_POINT('',(-7.5,37.5,57.));
#44333=CARTESIAN_POINT('Origin',(37.5,0.,43.));
#44334=CARTESIAN_POINT('',(30.,-9.18485099360515E-16,43.25));
#44335=CARTESIAN_POINT('',(29.75,9.49101269339199E-16,43.));
#44336=CARTESIAN_POINT('Origin',(37.5,0.,43.25));
#44337=CARTESIAN_POINT('Origin',(37.5,0.,57.));
#44338=CARTESIAN_POINT('',(30.,9.18485099360515E-16,56.5));
#44339=CARTESIAN_POINT('Origin',(37.5,0.,56.5));
#44340=CARTESIAN_POINT('',(30.,9.18485099360515E-16,57.));
#44341=CARTESIAN_POINT('Origin',(-42.8625,-85.475,56.75));
#44342=CARTESIAN_POINT('',(-42.8625,-85.225,57.));
#44343=CARTESIAN_POINT('',(-42.8625,-85.725,56.5));
#44344=CARTESIAN_POINT('Origin',(42.8625,85.475,56.75));
#44345=CARTESIAN_POINT('',(42.8625,85.225,57.));
#44346=CARTESIAN_POINT('Origin',(0.,0.,57.));
#44347=CARTESIAN_POINT('',(-54.925,52.425,57.));
#44348=CARTESIAN_POINT('Origin',(-52.425,52.425,57.));
#44349=CARTESIAN_POINT('',(-8.,37.5,57.));
#44350=CARTESIAN_POINT('Origin',(0.,37.5,57.));
#44351=CARTESIAN_POINT('',(-45.5,37.5,57.));
#44352=CARTESIAN_POINT('Origin',(-37.5,37.5,57.));
#44353=CARTESIAN_POINT('',(-45.5,-9.79717439317882E-16,57.));
#44354=CARTESIAN_POINT('Origin',(-37.5,0.,57.));
#44355=CARTESIAN_POINT('',(48.75,18.75,57.));
#44356=CARTESIAN_POINT('Origin',(56.25,18.75,57.));
#44357=CARTESIAN_POINT('',(11.25,-18.75,57.));
#44358=CARTESIAN_POINT('Origin',(18.75,-18.75,57.));
#44359=CARTESIAN_POINT('',(-26.25,-18.75,57.));
#44360=CARTESIAN_POINT('Origin',(-18.75,-18.75,57.));
#44361=CARTESIAN_POINT('',(-26.25,18.75,57.));
#44362=CARTESIAN_POINT('Origin',(-18.75,18.75,57.));
#44363=CARTESIAN_POINT('',(11.25,18.75,57.));
#44364=CARTESIAN_POINT('Origin',(18.75,18.75,57.));
#44365=CARTESIAN_POINT('',(51.7,-5.57214293612046E-16,57.));
#44366=CARTESIAN_POINT('Origin',(56.25,0.,57.));
#44367=CARTESIAN_POINT('',(32.95,-56.25,57.));
#44368=CARTESIAN_POINT('Origin',(37.5,-56.25,57.));
#44369=CARTESIAN_POINT('',(-4.55,56.25,57.));
#44370=CARTESIAN_POINT('Origin',(0.,56.25,57.));
#44371=CARTESIAN_POINT('',(-4.55,-56.25,57.));
#44372=CARTESIAN_POINT('Origin',(0.,-56.25,57.));
#44373=CARTESIAN_POINT('',(-42.05,56.25,57.));
#44374=CARTESIAN_POINT('Origin',(-37.5,56.25,57.));
#44375=CARTESIAN_POINT('',(-60.8,37.5,57.));
#44376=CARTESIAN_POINT('Origin',(-56.25,37.5,57.));
#44377=CARTESIAN_POINT('',(-23.3,-37.5,57.));
#44378=CARTESIAN_POINT('Origin',(-18.75,-37.5,57.));
#44379=CARTESIAN_POINT('',(-4.55,-18.75,57.));
#44380=CARTESIAN_POINT('Origin',(0.,-18.75,57.));
#44381=CARTESIAN_POINT('',(14.2,-37.5,57.));
#44382=CARTESIAN_POINT('Origin',(18.75,-37.5,57.));
#44383=CARTESIAN_POINT('',(32.95,-18.75,57.));
#44384=CARTESIAN_POINT('Origin',(37.5,-18.75,57.));
#44385=CARTESIAN_POINT('',(44.875,52.425,57.));
#44386=CARTESIAN_POINT('Origin',(52.425,52.425,57.));
#44387=CARTESIAN_POINT('',(-63.25,18.75,57.));
#44388=CARTESIAN_POINT('Origin',(-56.25,18.75,57.));
#44389=CARTESIAN_POINT('',(-25.75,56.25,57.));
#44390=CARTESIAN_POINT('Origin',(-18.75,56.25,57.));
#44391=CARTESIAN_POINT('',(-59.975,-52.425,57.));
#44392=CARTESIAN_POINT('Origin',(-52.425,-52.425,57.));
#44393=CARTESIAN_POINT('',(51.7,-37.5,57.));
#44394=CARTESIAN_POINT('Origin',(56.25,-37.5,57.));
#44395=CARTESIAN_POINT('',(14.2,37.5,57.));
#44396=CARTESIAN_POINT('Origin',(18.75,37.5,57.));
#44397=CARTESIAN_POINT('',(-4.55,18.75,57.));
#44398=CARTESIAN_POINT('Origin',(0.,18.75,57.));
#44399=CARTESIAN_POINT('',(-23.3,37.5,57.));
#44400=CARTESIAN_POINT('Origin',(-18.75,37.5,57.));
#44401=CARTESIAN_POINT('',(-42.05,18.75,57.));
#44402=CARTESIAN_POINT('Origin',(-37.5,18.75,57.));
#44403=CARTESIAN_POINT('',(-42.05,-18.75,57.));
#44404=CARTESIAN_POINT('Origin',(-37.5,-18.75,57.));
#44405=CARTESIAN_POINT('',(-23.3,-5.57214293612046E-16,57.));
#44406=CARTESIAN_POINT('Origin',(-18.75,0.,57.));
#44407=CARTESIAN_POINT('',(-60.8,-5.57214293612046E-16,57.));
#44408=CARTESIAN_POINT('Origin',(-56.25,0.,57.));
#44409=CARTESIAN_POINT('',(14.2,-5.57214293612045E-16,57.));
#44410=CARTESIAN_POINT('Origin',(18.75,0.,57.));
#44411=CARTESIAN_POINT('',(32.95,18.75,57.));
#44412=CARTESIAN_POINT('Origin',(37.5,18.75,57.));
#44413=CARTESIAN_POINT('',(48.75,-18.75,57.));
#44414=CARTESIAN_POINT('Origin',(56.25,-18.75,57.));
#44415=CARTESIAN_POINT('',(-63.75,-18.75,57.));
#44416=CARTESIAN_POINT('Origin',(-56.25,-18.75,57.));
#44417=CARTESIAN_POINT('',(-26.25,-56.25,57.));
#44418=CARTESIAN_POINT('Origin',(-18.75,-56.25,57.));
#44419=CARTESIAN_POINT('',(11.25,-56.25,57.));
#44420=CARTESIAN_POINT('Origin',(18.75,-56.25,57.));
#44421=CARTESIAN_POINT('',(11.25,56.25,57.));
#44422=CARTESIAN_POINT('Origin',(18.75,56.25,57.));
#44423=CARTESIAN_POINT('',(29.5,-37.5,57.));
#44424=CARTESIAN_POINT('Origin',(37.5,-37.5,57.));
#44425=CARTESIAN_POINT('',(-8.,-37.5,57.));
#44426=CARTESIAN_POINT('Origin',(0.,-37.5,57.));
#44427=CARTESIAN_POINT('',(-8.,-9.79717439317883E-16,57.));
#44428=CARTESIAN_POINT('Origin',(0.,0.,57.));
#44429=CARTESIAN_POINT('',(29.5,-9.79717439317882E-16,57.));
#44430=CARTESIAN_POINT('Origin',(37.5,0.,57.));
#44431=CARTESIAN_POINT('Origin',(-52.425,52.425,56.75));
#44432=CARTESIAN_POINT('',(-54.675,52.425,56.75));
#44433=CARTESIAN_POINT('Origin',(37.5,0.,56.75));
#44434=CARTESIAN_POINT('',(29.75,-9.49101269339199E-16,56.75));
#44435=CARTESIAN_POINT('Origin',(0.,37.5,56.75));
#44436=CARTESIAN_POINT('',(-7.75,37.5,56.75));
#44437=CARTESIAN_POINT('Origin',(0.,0.,56.75));
#44438=CARTESIAN_POINT('',(-7.75,-9.49101269339199E-16,56.75));
#44439=CARTESIAN_POINT('Origin',(-37.5,37.5,56.75));
#44440=CARTESIAN_POINT('',(-45.25,37.5,56.75));
#44441=CARTESIAN_POINT('Origin',(0.,-37.5,56.75));
#44442=CARTESIAN_POINT('',(-7.75,-37.5,56.75));
#44443=CARTESIAN_POINT('Origin',(-37.5,0.,56.75));
#44444=CARTESIAN_POINT('',(-45.25,-9.49101269339199E-16,56.75));
#44445=CARTESIAN_POINT('Origin',(37.5,-37.5,56.75));
#44446=CARTESIAN_POINT('',(29.75,-37.5,56.75));
#44447=CARTESIAN_POINT('Origin',(56.25,18.75,56.75));
#44448=CARTESIAN_POINT('',(49.25,18.75,56.5));
#44449=CARTESIAN_POINT('',(49.,18.75,56.75));
#44450=CARTESIAN_POINT('Origin',(56.25,18.75,56.5));
#44451=CARTESIAN_POINT('Origin',(56.25,18.75,57.));
#44452=CARTESIAN_POINT('',(49.25,18.75,57.));
#44453=CARTESIAN_POINT('Origin',(18.75,56.25,56.75));
#44454=CARTESIAN_POINT('',(11.75,56.25,56.5));
#44455=CARTESIAN_POINT('',(11.5,56.25,56.75));
#44456=CARTESIAN_POINT('Origin',(18.75,56.25,56.5));
#44457=CARTESIAN_POINT('Origin',(18.75,56.25,57.));
#44458=CARTESIAN_POINT('',(11.75,56.25,57.));
#44459=CARTESIAN_POINT('Origin',(18.75,-18.75,56.75));
#44460=CARTESIAN_POINT('',(11.75,-18.75,56.5));
#44461=CARTESIAN_POINT('',(11.5,-18.75,56.75));
#44462=CARTESIAN_POINT('Origin',(18.75,-18.75,56.5));
#44463=CARTESIAN_POINT('Origin',(18.75,-18.75,57.));
#44464=CARTESIAN_POINT('',(11.75,-18.75,57.));
#44465=CARTESIAN_POINT('Origin',(18.75,-56.25,56.75));
#44466=CARTESIAN_POINT('',(11.75,-56.25,56.5));
#44467=CARTESIAN_POINT('',(11.5,-56.25,56.75));
#44468=CARTESIAN_POINT('Origin',(18.75,-56.25,56.5));
#44469=CARTESIAN_POINT('Origin',(18.75,-56.25,57.));
#44470=CARTESIAN_POINT('',(11.75,-56.25,57.));
#44471=CARTESIAN_POINT('Origin',(-18.75,-18.75,56.75));
#44472=CARTESIAN_POINT('',(-25.75,-18.75,56.5));
#44473=CARTESIAN_POINT('',(-26.,-18.75,56.75));
#44474=CARTESIAN_POINT('Origin',(-18.75,-18.75,56.5));
#44475=CARTESIAN_POINT('Origin',(-18.75,-18.75,57.));
#44476=CARTESIAN_POINT('',(-25.75,-18.75,57.));
#44477=CARTESIAN_POINT('Origin',(-18.75,-56.25,56.75));
#44478=CARTESIAN_POINT('',(-25.75,-56.25,56.5));
#44479=CARTESIAN_POINT('',(-26.,-56.25,56.75));
#44480=CARTESIAN_POINT('Origin',(-18.75,-56.25,56.5));
#44481=CARTESIAN_POINT('Origin',(-18.75,-56.25,57.));
#44482=CARTESIAN_POINT('',(-25.75,-56.25,57.));
#44483=CARTESIAN_POINT('Origin',(-18.75,18.75,56.75));
#44484=CARTESIAN_POINT('',(-25.75,18.75,56.5));
#44485=CARTESIAN_POINT('',(-26.,18.75,56.75));
#44486=CARTESIAN_POINT('Origin',(-18.75,18.75,56.5));
#44487=CARTESIAN_POINT('Origin',(-18.75,18.75,57.));
#44488=CARTESIAN_POINT('',(-25.75,18.75,57.));
#44489=CARTESIAN_POINT('Origin',(-56.25,-18.75,56.75));
#44490=CARTESIAN_POINT('',(-63.25,-18.75,56.5));
#44491=CARTESIAN_POINT('',(-63.5,-18.75,56.75));
#44492=CARTESIAN_POINT('Origin',(-56.25,-18.75,56.5));
#44493=CARTESIAN_POINT('Origin',(-56.25,-18.75,57.));
#44494=CARTESIAN_POINT('',(-63.25,-18.75,57.));
#44495=CARTESIAN_POINT('Origin',(18.75,18.75,56.75));
#44496=CARTESIAN_POINT('',(11.75,18.75,56.5));
#44497=CARTESIAN_POINT('',(11.5,18.75,56.75));
#44498=CARTESIAN_POINT('Origin',(18.75,18.75,56.5));
#44499=CARTESIAN_POINT('Origin',(18.75,18.75,57.));
#44500=CARTESIAN_POINT('',(11.75,18.75,57.));
#44501=CARTESIAN_POINT('Origin',(56.25,-18.75,56.75));
#44502=CARTESIAN_POINT('',(49.25,-18.75,56.5));
#44503=CARTESIAN_POINT('',(49.,-18.75,56.75));
#44504=CARTESIAN_POINT('Origin',(56.25,-18.75,56.5));
#44505=CARTESIAN_POINT('Origin',(56.25,-18.75,57.));
#44506=CARTESIAN_POINT('',(49.25,-18.75,57.));
#44507=CARTESIAN_POINT('Origin',(56.25,0.,56.75));
#44508=CARTESIAN_POINT('',(51.95,-5.26598123633362E-16,56.75));
#44509=CARTESIAN_POINT('Origin',(37.5,18.75,56.75));
#44510=CARTESIAN_POINT('',(33.2,18.75,56.75));
#44511=CARTESIAN_POINT('Origin',(37.5,-56.25,56.75));
#44512=CARTESIAN_POINT('',(33.2,-56.25,56.75));
#44513=CARTESIAN_POINT('Origin',(18.75,0.,56.75));
#44514=CARTESIAN_POINT('',(14.45,-5.26598123633362E-16,56.75));
#44515=CARTESIAN_POINT('Origin',(0.,56.25,56.75));
#44516=CARTESIAN_POINT('',(-4.3,56.25,56.75));
#44517=CARTESIAN_POINT('Origin',(-56.25,0.,56.75));
#44518=CARTESIAN_POINT('',(-60.55,-5.26598123633362E-16,56.75));
#44519=CARTESIAN_POINT('Origin',(0.,-56.25,56.75));
#44520=CARTESIAN_POINT('',(-4.3,-56.25,56.75));
#44521=CARTESIAN_POINT('Origin',(-18.75,0.,56.75));
#44522=CARTESIAN_POINT('',(-23.05,-5.26598123633362E-16,56.75));
#44523=CARTESIAN_POINT('Origin',(-37.5,56.25,56.75));
#44524=CARTESIAN_POINT('',(-41.8,56.25,56.75));
#44525=CARTESIAN_POINT('Origin',(-37.5,-18.75,56.75));
#44526=CARTESIAN_POINT('',(-41.8,-18.75,56.75));
#44527=CARTESIAN_POINT('Origin',(-56.25,37.5,56.75));
#44528=CARTESIAN_POINT('',(-60.55,37.5,56.75));
#44529=CARTESIAN_POINT('Origin',(-37.5,18.75,56.75));
#44530=CARTESIAN_POINT('',(-41.8,18.75,56.75));
#44531=CARTESIAN_POINT('Origin',(-18.75,-37.5,56.75));
#44532=CARTESIAN_POINT('',(-23.05,-37.5,56.75));
#44533=CARTESIAN_POINT('Origin',(-18.75,37.5,56.75));
#44534=CARTESIAN_POINT('',(-23.05,37.5,56.75));
#44535=CARTESIAN_POINT('Origin',(0.,-18.75,56.75));
#44536=CARTESIAN_POINT('',(-4.3,-18.75,56.75));
#44537=CARTESIAN_POINT('Origin',(0.,18.75,56.75));
#44538=CARTESIAN_POINT('',(-4.3,18.75,56.75));
#44539=CARTESIAN_POINT('Origin',(18.75,-37.5,56.75));
#44540=CARTESIAN_POINT('',(14.45,-37.5,56.75));
#44541=CARTESIAN_POINT('Origin',(18.75,37.5,56.75));
#44542=CARTESIAN_POINT('',(14.45,37.5,56.75));
#44543=CARTESIAN_POINT('Origin',(37.5,-18.75,56.75));
#44544=CARTESIAN_POINT('',(33.2,-18.75,56.75));
#44545=CARTESIAN_POINT('Origin',(56.25,-37.5,56.75));
#44546=CARTESIAN_POINT('',(51.95,-37.5,56.75));
#44547=CARTESIAN_POINT('Origin',(52.425,52.425,56.75));
#44548=CARTESIAN_POINT('',(45.125,52.425,56.75));
#44549=CARTESIAN_POINT('Origin',(-52.425,-52.425,56.75));
#44550=CARTESIAN_POINT('',(-59.725,-52.425,56.75));
#44551=CARTESIAN_POINT('Origin',(-56.25,18.75,56.75));
#44552=CARTESIAN_POINT('',(-62.75,18.75,56.5));
#44553=CARTESIAN_POINT('',(-63.,18.75,56.75));
#44554=CARTESIAN_POINT('Origin',(-56.25,18.75,56.5));
#44555=CARTESIAN_POINT('Origin',(-56.25,18.75,57.));
#44556=CARTESIAN_POINT('',(-62.75,18.75,57.));
#44557=CARTESIAN_POINT('Origin',(-18.75,56.25,56.75));
#44558=CARTESIAN_POINT('',(-25.25,56.25,56.5));
#44559=CARTESIAN_POINT('',(-25.5,56.25,56.75));
#44560=CARTESIAN_POINT('Origin',(-18.75,56.25,56.5));
#44561=CARTESIAN_POINT('Origin',(-18.75,56.25,57.));
#44562=CARTESIAN_POINT('',(-25.25,56.25,57.));
#44563=CARTESIAN_POINT('Origin',(-52.425,52.425,42.75));
#44564=CARTESIAN_POINT('',(-56.6629,52.425,42.75));
#44565=CARTESIAN_POINT('Origin',(-85.725,-85.725,42.75));
#44566=CARTESIAN_POINT('',(0.,0.,0.));
#44567=CARTESIAN_POINT('Origin',(-33.475,-85.475,10.75));
#44568=CARTESIAN_POINT('',(-34.8212912017836,-85.725,7.25));
#44569=CARTESIAN_POINT('',(-32.1287087982164,-85.725,7.25));
#44570=CARTESIAN_POINT('Ctrl Pts',(-34.8212912017836,-85.725,7.25));
#44571=CARTESIAN_POINT('Ctrl Pts',(-34.4096238271454,-85.5772068894569,
7.25));
#44572=CARTESIAN_POINT('Ctrl Pts',(-33.9716586462892,-85.475,7.25));
#44573=CARTESIAN_POINT('Ctrl Pts',(-32.9783413537108,-85.475,7.25));
#44574=CARTESIAN_POINT('Ctrl Pts',(-32.5403761728546,-85.5772068894569,
7.25));
#44575=CARTESIAN_POINT('Ctrl Pts',(-32.1287087982164,-85.725,7.25));
#44576=CARTESIAN_POINT('',(-37.225,-85.725,10.75));
#44577=CARTESIAN_POINT('Origin',(-33.475,-85.725,10.75));
#44578=CARTESIAN_POINT('',(-36.725,-85.225,10.75));
#44579=CARTESIAN_POINT('',(-36.975,-85.475,10.75));
#44580=CARTESIAN_POINT('Origin',(-33.475,-85.225,10.75));
#44581=CARTESIAN_POINT('Origin',(-33.475,-85.725,10.75));
#44582=CARTESIAN_POINT('Origin',(-33.475,-85.475,3.75));
#44583=CARTESIAN_POINT('',(-37.225,-85.725,3.75));
#44584=CARTESIAN_POINT('Origin',(-33.475,-85.725,3.75));
#44585=CARTESIAN_POINT('',(-36.725,-85.225,3.75));
#44586=CARTESIAN_POINT('',(-36.975,-85.475,3.75));
#44587=CARTESIAN_POINT('Origin',(-33.475,-85.225,3.75));
#44588=CARTESIAN_POINT('',(-35.345828693387,-85.725,0.5));
#44589=CARTESIAN_POINT('Origin',(-33.475,-85.725,3.75));
#44590=CARTESIAN_POINT('',(-31.604171306613,-85.725,0.5));
#44591=CARTESIAN_POINT('Ctrl Pts',(-35.345828693387,-85.725,0.500000000000002));
#44592=CARTESIAN_POINT('Ctrl Pts',(-33.475,-85.225,-9.0205620750794E-16));
#44593=CARTESIAN_POINT('Ctrl Pts',(-31.604171306613,-85.725,0.500000000000002));
#44594=CARTESIAN_POINT('Origin',(-33.475,-85.725,3.75));
#44595=CARTESIAN_POINT('Origin',(-33.475,-85.725,10.75));
#44596=CARTESIAN_POINT('',(-36.725,-73.225,10.75));
#44597=CARTESIAN_POINT('',(-36.725,-85.725,10.75));
#44598=CARTESIAN_POINT('Origin',(-33.475,-73.225,10.75));
#44599=CARTESIAN_POINT('Origin',(-37.05,-85.475,0.25));
#44600=CARTESIAN_POINT('',(-40.125,-85.725,0.5));
#44601=CARTESIAN_POINT('',(-37.05,-85.725,0.5));
#44602=CARTESIAN_POINT('',(-40.125,-85.225,0.));
#44603=CARTESIAN_POINT('',(-40.125,-85.725,0.5));
#44604=CARTESIAN_POINT('',(-26.825,-85.225,0.));
#44605=CARTESIAN_POINT('',(-37.05,-85.225,0.));
#44606=CARTESIAN_POINT('',(-26.575,-85.475,0.250000000000002));
#44607=CARTESIAN_POINT('',(-29.9041666666666,-82.1458333333333,-3.07916666666666));
#44608=CARTESIAN_POINT('',(-26.825,-85.725,0.5));
#44609=CARTESIAN_POINT('',(-28.2791666666666,-87.1791666666667,1.95416666666665));
#44610=CARTESIAN_POINT('',(-37.05,-85.725,0.5));
#44611=CARTESIAN_POINT('Origin',(-33.475,-85.725,3.75));
#44612=CARTESIAN_POINT('',(-36.725,-73.225,3.75));
#44613=CARTESIAN_POINT('',(-36.725,-85.725,3.75));
#44614=CARTESIAN_POINT('Origin',(-33.475,-73.225,3.75));
#44615=CARTESIAN_POINT('Origin',(-40.125,-85.225,0.));
#44616=CARTESIAN_POINT('',(-40.625,-85.225,0.5));
#44617=CARTESIAN_POINT('',(-40.625,-85.225,0.5));
#44618=CARTESIAN_POINT('',(-40.125,-85.225,0.));
#44619=CARTESIAN_POINT('Origin',(-40.625,-47.225,0.5));
#44620=CARTESIAN_POINT('',(-40.125,-47.225,0.));
#44621=CARTESIAN_POINT('',(-40.125,-46.725,0.5));
#44622=CARTESIAN_POINT('',(-40.125,-47.225,0.));
#44623=CARTESIAN_POINT('',(-40.625,-47.225,0.5));
#44624=CARTESIAN_POINT('',(-40.625,-47.225,0.5));
#44625=CARTESIAN_POINT('',(-40.125,-46.725,0.5));
#44626=CARTESIAN_POINT('Origin',(-40.375,-56.475,0.25));
#44627=CARTESIAN_POINT('',(-40.625,-56.475,0.5));
#44628=CARTESIAN_POINT('',(-40.125,-56.475,0.));
#44629=CARTESIAN_POINT('Origin',(-40.375,-46.975,0.));
#44630=CARTESIAN_POINT('',(-40.375,-46.975,31.75));
#44631=CARTESIAN_POINT('',(-40.125,-46.725,31.5));
#44632=CARTESIAN_POINT('',(-33.3375,-39.9375,24.7125));
#44633=CARTESIAN_POINT('',(-40.125,-46.725,0.));
#44634=CARTESIAN_POINT('',(-40.625,-47.225,31.5));
#44635=CARTESIAN_POINT('',(-40.625,-47.225,0.));
#44636=CARTESIAN_POINT('',(-47.25,-53.85,24.875));
#44637=CARTESIAN_POINT('Origin',(-26.825,-47.225,0.));
#44638=CARTESIAN_POINT('',(-26.325,-47.225,0.5));
#44639=CARTESIAN_POINT('',(-26.825,-46.725,0.5));
#44640=CARTESIAN_POINT('',(-26.325,-47.225,0.5));
#44641=CARTESIAN_POINT('',(-26.825,-47.225,0.));
#44642=CARTESIAN_POINT('',(-26.825,-47.225,0.));
#44643=CARTESIAN_POINT('',(-26.825,-46.725,0.5));
#44644=CARTESIAN_POINT('Origin',(-26.575,-75.975,0.25));
#44645=CARTESIAN_POINT('',(-26.825,-75.975,0.));
#44646=CARTESIAN_POINT('',(-26.325,-85.225,0.5));
#44647=CARTESIAN_POINT('',(-26.325,-75.975,0.5));
#44648=CARTESIAN_POINT('',(-25.0333333333333,-83.9333333333333,1.79166666666668));
#44649=CARTESIAN_POINT('Origin',(-29.9,-46.975,0.25));
#44650=CARTESIAN_POINT('',(-29.9,-46.725,0.5));
#44651=CARTESIAN_POINT('',(-29.9,-47.225,0.));
#44652=CARTESIAN_POINT('Origin',(-26.575,-46.975,0.));
#44653=CARTESIAN_POINT('',(-26.575,-46.975,31.75));
#44654=CARTESIAN_POINT('',(-26.325,-47.225,31.5));
#44655=CARTESIAN_POINT('',(-16.45,-57.1,21.625));
#44656=CARTESIAN_POINT('',(-26.325,-47.225,0.));
#44657=CARTESIAN_POINT('',(-26.825,-46.725,31.5));
#44658=CARTESIAN_POINT('',(-26.825,-46.725,0.));
#44659=CARTESIAN_POINT('',(-32.4208333333333,-41.1291666666667,25.9041666666667));
#44660=CARTESIAN_POINT('Origin',(-40.375,-85.475,0.));
#44661=CARTESIAN_POINT('',(-40.375,-85.475,31.75));
#44662=CARTESIAN_POINT('',(-40.625,-85.225,31.5));
#44663=CARTESIAN_POINT('',(-50.5,-75.35,21.625));
#44664=CARTESIAN_POINT('',(-40.625,-85.225,0.));
#44665=CARTESIAN_POINT('',(-40.125,-85.725,31.5));
#44666=CARTESIAN_POINT('',(-40.125,-85.725,0.));
#44667=CARTESIAN_POINT('',(-34.5291666666667,-91.3208333333333,25.9041666666668));
#44668=CARTESIAN_POINT('Origin',(-26.325,-46.725,0.));
#44669=CARTESIAN_POINT('',(-29.9,-46.725,31.5));
#44670=CARTESIAN_POINT('',(-35.175,-46.725,10.75));
#44671=CARTESIAN_POINT('Origin',(-33.475,-46.725,10.75));
#44672=CARTESIAN_POINT('',(-35.175,-46.725,3.75));
#44673=CARTESIAN_POINT('Origin',(-33.475,-46.725,3.75));
#44674=CARTESIAN_POINT('Origin',(-40.625,-46.725,0.));
#44675=CARTESIAN_POINT('',(-40.625,-56.475,31.5));
#44676=CARTESIAN_POINT('',(-40.625,-66.,27.05));
#44677=CARTESIAN_POINT('Origin',(-40.625,-66.,20.));
#44678=CARTESIAN_POINT('',(-40.625,-79.,24.5));
#44679=CARTESIAN_POINT('Origin',(-40.625,-79.,20.));
#44680=CARTESIAN_POINT('Origin',(-40.375,-56.475,31.75));
#44681=CARTESIAN_POINT('',(-40.125,-85.225,32.));
#44682=CARTESIAN_POINT('',(-40.125,-85.225,32.));
#44683=CARTESIAN_POINT('',(-40.125,-47.225,32.));
#44684=CARTESIAN_POINT('',(-40.125,-56.475,32.));
#44685=CARTESIAN_POINT('',(-40.125,-47.225,32.));
#44686=CARTESIAN_POINT('Origin',(-37.05,-85.475,31.75));
#44687=CARTESIAN_POINT('',(-26.825,-85.725,31.5));
#44688=CARTESIAN_POINT('',(-37.05,-85.725,31.5));
#44689=CARTESIAN_POINT('',(-26.825,-85.225,32.));
#44690=CARTESIAN_POINT('',(-26.825,-85.725,31.5));
#44691=CARTESIAN_POINT('',(-37.05,-85.225,32.));
#44692=CARTESIAN_POINT('Origin',(-33.475,-66.225,0.));
#44693=CARTESIAN_POINT('Origin',(-26.325,-85.225,31.5));
#44694=CARTESIAN_POINT('',(-26.325,-85.225,31.5));
#44695=CARTESIAN_POINT('',(-26.325,-85.225,31.5));
#44696=CARTESIAN_POINT('',(-26.825,-85.225,32.));
#44697=CARTESIAN_POINT('Origin',(-26.575,-85.475,0.));
#44698=CARTESIAN_POINT('',(-26.325,-85.225,0.));
#44699=CARTESIAN_POINT('',(-26.825,-85.725,0.));
#44700=CARTESIAN_POINT('Origin',(-29.9,-46.975,31.75));
#44701=CARTESIAN_POINT('',(-26.825,-47.225,32.));
#44702=CARTESIAN_POINT('',(-29.9,-47.225,32.));
#44703=CARTESIAN_POINT('',(-26.825,-47.225,32.));
#44704=CARTESIAN_POINT('Origin',(-26.575,-75.975,31.75));
#44705=CARTESIAN_POINT('',(-26.825,-75.975,32.));
#44706=CARTESIAN_POINT('',(-26.325,-75.975,31.5));
#44707=CARTESIAN_POINT('Origin',(-26.325,-85.725,0.));
#44708=CARTESIAN_POINT('',(-26.325,-66.,27.05));
#44709=CARTESIAN_POINT('Origin',(-26.325,-66.,20.));
#44710=CARTESIAN_POINT('Origin',(-33.475,-66.225,32.));
#44711=CARTESIAN_POINT('',(-40.1,-79.,32.));
#44712=CARTESIAN_POINT('Origin',(-38.6,-79.,32.));
#44713=CARTESIAN_POINT('Origin',(-33.475,-73.225,3.75));
#44714=CARTESIAN_POINT('',(-35.175,-73.225,3.75));
#44715=CARTESIAN_POINT('Origin',(-33.475,-73.225,3.75));
#44716=CARTESIAN_POINT('Origin',(-33.475,-73.225,10.75));
#44717=CARTESIAN_POINT('',(-35.175,-73.225,10.75));
#44718=CARTESIAN_POINT('Origin',(-33.475,-73.225,10.75));
#44719=CARTESIAN_POINT('Origin',(-33.475,-85.725,3.75));
#44720=CARTESIAN_POINT('',(-35.175,-85.725,3.75));
#44721=CARTESIAN_POINT('Origin',(-33.475,-85.725,10.75));
#44722=CARTESIAN_POINT('',(-35.175,-85.725,10.75));
#44723=CARTESIAN_POINT('Origin',(-38.6,-79.,32.));
#44724=CARTESIAN_POINT('',(-40.1,-79.,24.5));
#44725=CARTESIAN_POINT('',(-40.1,-79.,32.));
#44726=CARTESIAN_POINT('',(-38.6,-77.5,24.2426406871193));
#44727=CARTESIAN_POINT('Ctrl Pts',(-38.6,-77.5,24.2426406871193));
#44728=CARTESIAN_POINT('Ctrl Pts',(-38.7899690906118,-77.5,24.2426406871193));
#44729=CARTESIAN_POINT('Ctrl Pts',(-38.9915029601953,-77.5382644910968,
24.2567401743069));
#44730=CARTESIAN_POINT('Ctrl Pts',(-39.3605797699365,-77.6917706385605,
24.3063956191435));
#44731=CARTESIAN_POINT('Ctrl Pts',(-39.5282646235601,-77.8069442800005,
24.3411032840945));
#44732=CARTESIAN_POINT('Ctrl Pts',(-39.7929943148421,-78.0716739712825,
24.4053096652352));
#44733=CARTESIAN_POINT('Ctrl Pts',(-39.9082152291749,-78.2393832820639,
24.4391554329551));
#44734=CARTESIAN_POINT('Ctrl Pts',(-40.0617566312046,-78.6085507941687,
24.4868035691518));
#44735=CARTESIAN_POINT('Ctrl Pts',(-40.1,-78.810119017199,24.5));
#44736=CARTESIAN_POINT('Ctrl Pts',(-40.1,-79.,24.5));
#44737=CARTESIAN_POINT('',(-37.1,-79.,24.5));
#44738=CARTESIAN_POINT('Ctrl Pts',(-37.1,-79.,24.5));
#44739=CARTESIAN_POINT('Ctrl Pts',(-37.1,-78.810119017199,24.5));
#44740=CARTESIAN_POINT('Ctrl Pts',(-37.1382433687954,-78.6085507941687,
24.4868035691518));
#44741=CARTESIAN_POINT('Ctrl Pts',(-37.2917847708251,-78.2393832820639,
24.4391554329551));
#44742=CARTESIAN_POINT('Ctrl Pts',(-37.4070056851579,-78.0716739712825,
24.4053096652352));
#44743=CARTESIAN_POINT('Ctrl Pts',(-37.6717353764399,-77.8069442800005,
24.3411032840945));
#44744=CARTESIAN_POINT('Ctrl Pts',(-37.8394202300635,-77.6917706385605,
24.3063956191435));
#44745=CARTESIAN_POINT('Ctrl Pts',(-38.2084970398047,-77.5382644910968,
24.2567401743069));
#44746=CARTESIAN_POINT('Ctrl Pts',(-38.4100309093882,-77.5,24.2426406871193));
#44747=CARTESIAN_POINT('Ctrl Pts',(-38.6,-77.5,24.2426406871193));
#44748=CARTESIAN_POINT('Ctrl Pts',(-40.1,-79.,24.5));
#44749=CARTESIAN_POINT('Ctrl Pts',(-40.1,-79.189880982801,24.5));
#44750=CARTESIAN_POINT('Ctrl Pts',(-40.0617566312046,-79.3914492058313,
24.4868035691518));
#44751=CARTESIAN_POINT('Ctrl Pts',(-39.9082152291749,-79.7606167179361,
24.4391554329551));
#44752=CARTESIAN_POINT('Ctrl Pts',(-39.7929943148421,-79.9283260287175,
24.4053096652352));
#44753=CARTESIAN_POINT('Ctrl Pts',(-39.5282646235601,-80.1930557199996,
24.3411032840945));
#44754=CARTESIAN_POINT('Ctrl Pts',(-39.3605797699365,-80.3082293614395,
24.3063956191435));
#44755=CARTESIAN_POINT('Ctrl Pts',(-38.9915029601953,-80.4617355089032,
24.2567401743069));
#44756=CARTESIAN_POINT('Ctrl Pts',(-38.7899690906118,-80.5,24.2426406871193));
#44757=CARTESIAN_POINT('Ctrl Pts',(-38.4100309093882,-80.5,24.2426406871193));
#44758=CARTESIAN_POINT('Ctrl Pts',(-38.2084970398047,-80.4617355089032,
24.2567401743069));
#44759=CARTESIAN_POINT('Ctrl Pts',(-37.8394202300634,-80.3082293614395,
24.3063956191435));
#44760=CARTESIAN_POINT('Ctrl Pts',(-37.6717353764399,-80.1930557199996,
24.3411032840945));
#44761=CARTESIAN_POINT('Ctrl Pts',(-37.4070056851579,-79.9283260287175,
24.4053096652352));
#44762=CARTESIAN_POINT('Ctrl Pts',(-37.2917847708251,-79.7606167179361,
24.4391554329551));
#44763=CARTESIAN_POINT('Ctrl Pts',(-37.1382433687954,-79.3914492058313,
24.4868035691518));
#44764=CARTESIAN_POINT('Ctrl Pts',(-37.1,-79.189880982801,24.5));
#44765=CARTESIAN_POINT('Ctrl Pts',(-37.1,-79.,24.5));
#44766=CARTESIAN_POINT('Origin',(-38.6,-79.,32.));
#44767=CARTESIAN_POINT('',(-38.6,-77.5,15.7573593128807));
#44768=CARTESIAN_POINT('',(-40.1,-79.,15.5));
#44769=CARTESIAN_POINT('Ctrl Pts',(-38.6,-77.5,15.7573593128807));
#44770=CARTESIAN_POINT('Ctrl Pts',(-38.4100309093882,-77.5,15.7573593128807));
#44771=CARTESIAN_POINT('Ctrl Pts',(-38.2084970398047,-77.5382644910968,
15.7432598256931));
#44772=CARTESIAN_POINT('Ctrl Pts',(-37.8394202300635,-77.6917706385605,
15.6936043808565));
#44773=CARTESIAN_POINT('Ctrl Pts',(-37.6717353764399,-77.8069442800005,
15.6588967159055));
#44774=CARTESIAN_POINT('Ctrl Pts',(-37.4070056851579,-78.0716739712825,
15.5946903347648));
#44775=CARTESIAN_POINT('Ctrl Pts',(-37.2917847708251,-78.2393832820639,
15.5608445670449));
#44776=CARTESIAN_POINT('Ctrl Pts',(-37.1382433687954,-78.6085507941687,
15.5131964308482));
#44777=CARTESIAN_POINT('Ctrl Pts',(-37.1,-78.810119017199,15.5));
#44778=CARTESIAN_POINT('Ctrl Pts',(-37.1,-79.189880982801,15.5));
#44779=CARTESIAN_POINT('Ctrl Pts',(-37.1382433687954,-79.3914492058313,
15.5131964308482));
#44780=CARTESIAN_POINT('Ctrl Pts',(-37.2917847708251,-79.7606167179361,
15.5608445670449));
#44781=CARTESIAN_POINT('Ctrl Pts',(-37.4070056851579,-79.9283260287175,
15.5946903347648));
#44782=CARTESIAN_POINT('Ctrl Pts',(-37.6717353764399,-80.1930557199996,
15.6588967159055));
#44783=CARTESIAN_POINT('Ctrl Pts',(-37.8394202300635,-80.3082293614395,
15.6936043808565));
#44784=CARTESIAN_POINT('Ctrl Pts',(-38.2084970398047,-80.4617355089032,
15.7432598256931));
#44785=CARTESIAN_POINT('Ctrl Pts',(-38.4100309093882,-80.5,15.7573593128807));
#44786=CARTESIAN_POINT('Ctrl Pts',(-38.7899690906118,-80.5,15.7573593128807));
#44787=CARTESIAN_POINT('Ctrl Pts',(-38.9915029601953,-80.4617355089032,
15.7432598256931));
#44788=CARTESIAN_POINT('Ctrl Pts',(-39.3605797699366,-80.3082293614395,
15.6936043808565));
#44789=CARTESIAN_POINT('Ctrl Pts',(-39.5282646235601,-80.1930557199995,
15.6588967159055));
#44790=CARTESIAN_POINT('Ctrl Pts',(-39.7929943148421,-79.9283260287175,
15.5946903347648));
#44791=CARTESIAN_POINT('Ctrl Pts',(-39.9082152291749,-79.7606167179361,
15.5608445670449));
#44792=CARTESIAN_POINT('Ctrl Pts',(-40.0617566312046,-79.3914492058313,
15.5131964308482));
#44793=CARTESIAN_POINT('Ctrl Pts',(-40.1,-79.189880982801,15.5));
#44794=CARTESIAN_POINT('Ctrl Pts',(-40.1,-79.,15.5));
#44795=CARTESIAN_POINT('Ctrl Pts',(-40.1,-79.,15.5));
#44796=CARTESIAN_POINT('Ctrl Pts',(-40.1,-78.810119017199,15.5));
#44797=CARTESIAN_POINT('Ctrl Pts',(-40.0617566312046,-78.6085507941687,
15.5131964308482));
#44798=CARTESIAN_POINT('Ctrl Pts',(-39.9082152291749,-78.2393832820639,
15.5608445670449));
#44799=CARTESIAN_POINT('Ctrl Pts',(-39.7929943148421,-78.0716739712825,
15.5946903347648));
#44800=CARTESIAN_POINT('Ctrl Pts',(-39.5282646235601,-77.8069442800005,
15.6588967159055));
#44801=CARTESIAN_POINT('Ctrl Pts',(-39.3605797699365,-77.6917706385605,
15.6936043808565));
#44802=CARTESIAN_POINT('Ctrl Pts',(-38.9915029601953,-77.5382644910968,
15.7432598256931));
#44803=CARTESIAN_POINT('Ctrl Pts',(-38.7899690906118,-77.5,15.7573593128807));
#44804=CARTESIAN_POINT('Ctrl Pts',(-38.6,-77.5,15.7573593128807));
#44805=CARTESIAN_POINT('',(-40.1,-79.,14.));
#44806=CARTESIAN_POINT('',(-40.1,-79.,32.));
#44807=CARTESIAN_POINT('Origin',(-38.6,-79.,14.));
#44808=CARTESIAN_POINT('Origin',(-38.6,-79.,14.));
#44809=CARTESIAN_POINT('Origin',(-40.625,-79.,20.));
#44810=CARTESIAN_POINT('',(-40.625,-79.,24.5));
#44811=CARTESIAN_POINT('',(-30.625,-79.,24.5));
#44812=CARTESIAN_POINT('',(-40.625,-79.,24.5));
#44813=CARTESIAN_POINT('Origin',(-30.625,-79.,20.));
#44814=CARTESIAN_POINT('Origin',(-30.625,-79.,20.));
#44815=CARTESIAN_POINT('Origin',(-26.325,-66.,20.));
#44816=CARTESIAN_POINT('',(-26.325,-66.,27.05));
#44817=CARTESIAN_POINT('Origin',(-40.625,-85.725,0.));
#44818=CARTESIAN_POINT('',(0.,0.,0.));
#44819=CARTESIAN_POINT('Origin',(-40.0142135623731,-80.4142135623731,20.));
#44820=CARTESIAN_POINT('',(-41.6670038745204,-81.5013243192465,20.0018221889518));
#44821=CARTESIAN_POINT('',(-41.6824373695361,-81.5175532542339,19.9794877782846));
#44822=CARTESIAN_POINT('Ctrl Pts',(-41.667003992987,-81.501323636858,20.0018258382422));
#44823=CARTESIAN_POINT('Ctrl Pts',(-41.6723036980297,-81.5065761360697,
19.9943901405908));
#44824=CARTESIAN_POINT('Ctrl Pts',(-41.6774508057097,-81.5119900511825,
19.9869413272942));
#44825=CARTESIAN_POINT('Ctrl Pts',(-41.6824371476317,-81.5175534133105,
19.9794877942845));
#44826=CARTESIAN_POINT('',(-41.1175295141106,-82.0824704858893,20.0205146094984));
#44827=CARTESIAN_POINT('Ctrl Pts',(-41.1175295141106,-82.0824704858894,
20.0205146094973));
#44828=CARTESIAN_POINT('Ctrl Pts',(-41.1169315617889,-82.0818012262451,
20.0214964568026));
#44829=CARTESIAN_POINT('Ctrl Pts',(-41.1163360655611,-82.0811293124528,
20.022477994219));
#44830=CARTESIAN_POINT('Ctrl Pts',(-41.0898149851225,-82.050962453584,20.0663587246604));
#44831=CARTESIAN_POINT('Ctrl Pts',(-41.0684925512851,-82.0163047514998,
20.1087879830725));
#44832=CARTESIAN_POINT('Ctrl Pts',(-41.0371790069056,-81.9399561963918,
20.1880837226203));
#44833=CARTESIAN_POINT('Ctrl Pts',(-41.026715172619,-81.8981742709483,20.2254321238237));
#44834=CARTESIAN_POINT('Ctrl Pts',(-41.017874801645,-81.8053693573189,20.2952495938576));
#44835=CARTESIAN_POINT('Ctrl Pts',(-41.0203629078659,-81.7532119643487,
20.3276528784673));
#44836=CARTESIAN_POINT('Ctrl Pts',(-41.0413539676923,-81.6607507752854,
20.3707052159476));
#44837=CARTESIAN_POINT('Ctrl Pts',(-41.0555000619675,-81.6208986488143,
20.3848443838584));
#44838=CARTESIAN_POINT('Ctrl Pts',(-41.093188372277,-81.5507282918097,20.3994995890491));
#44839=CARTESIAN_POINT('Ctrl Pts',(-41.1144544593006,-81.5206896773008,
20.401675192587));
#44840=CARTESIAN_POINT('Ctrl Pts',(-41.165653789439,-81.4669930646739,20.3956510376664));
#44841=CARTESIAN_POINT('Ctrl Pts',(-41.1944668468356,-81.4447737703187,
20.387440961117));
#44842=CARTESIAN_POINT('Ctrl Pts',(-41.2629514740271,-81.406840654893,20.3593672352608));
#44843=CARTESIAN_POINT('Ctrl Pts',(-41.3018885474464,-81.394495024668,20.3381091044114));
#44844=CARTESIAN_POINT('Ctrl Pts',(-41.3929538579519,-81.3809801263275,
20.2795382731015));
#44845=CARTESIAN_POINT('Ctrl Pts',(-41.4471194419021,-81.3855135588177,
20.2374603554904));
#44846=CARTESIAN_POINT('Ctrl Pts',(-41.5618160326496,-81.4200211943617,
20.1322968488021));
#44847=CARTESIAN_POINT('Ctrl Pts',(-41.6199733871036,-81.4547186766113,
20.0677665047026));
#44848=CARTESIAN_POINT('Ctrl Pts',(-41.6670038745197,-81.5013243192459,
20.0018221889509));
#44849=CARTESIAN_POINT('',(-41.4,-81.8,19.6));
#44850=CARTESIAN_POINT('Origin',(-41.4,-81.8,20.));
#44851=CARTESIAN_POINT('',(-40.0142135623731,-80.4142135623731,19.6));
#44852=CARTESIAN_POINT('',(-40.0142135623731,-80.4142135623731,19.6));
#44853=CARTESIAN_POINT('',(-40.0142135623731,-80.4142135623731,20.4));
#44854=CARTESIAN_POINT('Ctrl Pts',(-40.0142135623731,-80.4142135623731,
20.4));
#44855=CARTESIAN_POINT('Ctrl Pts',(-40.0142135623731,-80.4153831419304,
20.4));
#44856=CARTESIAN_POINT('Ctrl Pts',(-40.0142131996467,-80.4165527237652,
20.3999974351574));
#44857=CARTESIAN_POINT('Ctrl Pts',(-40.0141778904501,-80.4735319741397,
20.3997472920084));
#44858=CARTESIAN_POINT('Ctrl Pts',(-40.013302136999,-80.5295473343443,20.3936524317683));
#44859=CARTESIAN_POINT('Ctrl Pts',(-40.0100460838861,-80.6429937614698,
20.3672982573464));
#44860=CARTESIAN_POINT('Ctrl Pts',(-40.0075166610327,-80.7005682273989,
20.3457022349177));
#44861=CARTESIAN_POINT('Ctrl Pts',(-40.0022566529727,-80.7962497320611,
20.2899515263984));
#44862=CARTESIAN_POINT('Ctrl Pts',(-39.999637895333,-80.836023977406,20.2585158351079));
#44863=CARTESIAN_POINT('Ctrl Pts',(-39.9953022634654,-80.8963784968088,
20.1894129105366));
#44864=CARTESIAN_POINT('Ctrl Pts',(-39.9935403080928,-80.9187129635945,
20.1540514056522));
#44865=CARTESIAN_POINT('Ctrl Pts',(-39.991131445458,-80.9484928880337,20.0784645960831));
#44866=CARTESIAN_POINT('Ctrl Pts',(-39.9904773405935,-80.9561627655428,
20.039614799918));
#44867=CARTESIAN_POINT('Ctrl Pts',(-39.9904773405935,-80.9561627655428,
19.960385200082));
#44868=CARTESIAN_POINT('Ctrl Pts',(-39.991131445458,-80.9484928880337,19.9215354039169));
#44869=CARTESIAN_POINT('Ctrl Pts',(-39.9935403080928,-80.9187129635945,
19.8459485943478));
#44870=CARTESIAN_POINT('Ctrl Pts',(-39.9953022634654,-80.8963784968088,
19.8105870894634));
#44871=CARTESIAN_POINT('Ctrl Pts',(-39.999637895333,-80.8360239774059,19.741484164892));
#44872=CARTESIAN_POINT('Ctrl Pts',(-40.0022566529728,-80.796249732061,19.7100484736016));
#44873=CARTESIAN_POINT('Ctrl Pts',(-40.0075166610327,-80.7005682273989,
19.6542977650823));
#44874=CARTESIAN_POINT('Ctrl Pts',(-40.0100460838861,-80.6429937614698,
19.6327017426536));
#44875=CARTESIAN_POINT('Ctrl Pts',(-40.013302136999,-80.5295473343452,19.6063475682319));
#44876=CARTESIAN_POINT('Ctrl Pts',(-40.0141778904501,-80.473531974145,19.6002527079916));
#44877=CARTESIAN_POINT('Ctrl Pts',(-40.0142131996467,-80.4165527237649,
19.6000025648426));
#44878=CARTESIAN_POINT('Ctrl Pts',(-40.0142135623731,-80.4153831419307,
19.6));
#44879=CARTESIAN_POINT('Ctrl Pts',(-40.0142135623731,-80.4142135623731,
19.6));
#44880=CARTESIAN_POINT('Ctrl Pts',(-40.0142135623731,-80.4142135623731,
19.6));
#44881=CARTESIAN_POINT('Ctrl Pts',(-40.0153831419306,-80.4142135623731,
19.6));
#44882=CARTESIAN_POINT('Ctrl Pts',(-40.016552723765,-80.4142131996467,19.6000025648426));
#44883=CARTESIAN_POINT('Ctrl Pts',(-40.0735319741399,-80.4141778904502,
19.6002527079916));
#44884=CARTESIAN_POINT('Ctrl Pts',(-40.1295473343444,-80.413302136999,19.6063475682317));
#44885=CARTESIAN_POINT('Ctrl Pts',(-40.2429937614698,-80.4100460838861,
19.6327017426536));
#44886=CARTESIAN_POINT('Ctrl Pts',(-40.300568227399,-80.4075166610327,19.6542977650823));
#44887=CARTESIAN_POINT('Ctrl Pts',(-40.396249732061,-80.4022566529727,19.7100484736016));
#44888=CARTESIAN_POINT('Ctrl Pts',(-40.436023977406,-80.399637895333,19.741484164892));
#44889=CARTESIAN_POINT('Ctrl Pts',(-40.4963784968088,-80.3953022634654,
19.8105870894634));
#44890=CARTESIAN_POINT('Ctrl Pts',(-40.5187129635945,-80.3935403080928,
19.8459485943478));
#44891=CARTESIAN_POINT('Ctrl Pts',(-40.5484928880337,-80.391131445458,19.9215354039169));
#44892=CARTESIAN_POINT('Ctrl Pts',(-40.5561627655428,-80.3904773405935,
19.960385200082));
#44893=CARTESIAN_POINT('Ctrl Pts',(-40.5561627655428,-80.3904773405935,
20.039614799918));
#44894=CARTESIAN_POINT('Ctrl Pts',(-40.5484928880337,-80.391131445458,20.0784645960831));
#44895=CARTESIAN_POINT('Ctrl Pts',(-40.5187129635945,-80.3935403080928,
20.1540514056522));
#44896=CARTESIAN_POINT('Ctrl Pts',(-40.4963784968088,-80.3953022634654,
20.1894129105366));
#44897=CARTESIAN_POINT('Ctrl Pts',(-40.436023977406,-80.399637895333,20.258515835108));
#44898=CARTESIAN_POINT('Ctrl Pts',(-40.396249732061,-80.4022566529727,20.2899515263984));
#44899=CARTESIAN_POINT('Ctrl Pts',(-40.300568227399,-80.4075166610327,20.3457022349177));
#44900=CARTESIAN_POINT('Ctrl Pts',(-40.2429937614698,-80.4100460838861,
20.3672982573464));
#44901=CARTESIAN_POINT('Ctrl Pts',(-40.1295473343444,-80.413302136999,20.3936524317682));
#44902=CARTESIAN_POINT('Ctrl Pts',(-40.0735319741399,-80.4141778904502,
20.3997472920084));
#44903=CARTESIAN_POINT('Ctrl Pts',(-40.016552723765,-80.4142131996467,20.3999974351574));
#44904=CARTESIAN_POINT('Ctrl Pts',(-40.0153831419306,-80.4142135623731,
20.4));
#44905=CARTESIAN_POINT('Ctrl Pts',(-40.0142135623731,-80.4142135623731,
20.4));
#44906=CARTESIAN_POINT('Origin',(-41.4,-81.8,20.));
#44907=CARTESIAN_POINT('Origin',(-41.4,-81.8,20.));
#44908=CARTESIAN_POINT('',(-41.4,-81.8,20.));
#44909=CARTESIAN_POINT('Origin',(-38.6,-79.,20.));
#44910=CARTESIAN_POINT('',(-40.2,-79.,20.));
#44911=CARTESIAN_POINT('Origin',(-40.6,-79.,20.));
#44912=CARTESIAN_POINT('Origin',(-38.6,-79.,20.));
#44913=CARTESIAN_POINT('Origin',(-41.4,-81.8,20.));
#44914=CARTESIAN_POINT('Origin',(-41.4,-81.8,20.));
#44915=CARTESIAN_POINT('Origin',(-58.4561395287659,-80.2714145057222,20.));
#44916=CARTESIAN_POINT('',(-56.9777960240775,-81.7949165950883,19.6772168703845));
#44917=CARTESIAN_POINT('',(-56.9042068273237,-81.5494766841245,19.5999999999999));
#44918=CARTESIAN_POINT('Ctrl Pts',(-56.9777960279009,-81.7949165905344,
19.6772168782191));
#44919=CARTESIAN_POINT('Ctrl Pts',(-56.9774534269664,-81.7748789883664,
19.6657367803573));
#44920=CARTESIAN_POINT('Ctrl Pts',(-56.9758685115415,-81.7543927701849,
19.6551784083702));
#44921=CARTESIAN_POINT('Ctrl Pts',(-56.9671441435283,-81.6939687882869,
19.6278056262105));
#44922=CARTESIAN_POINT('Ctrl Pts',(-56.9562678019039,-81.6532801182632,
19.6140483572685));
#44923=CARTESIAN_POINT('Ctrl Pts',(-56.929299784212,-81.591434225957,19.6022201311171));
#44924=CARTESIAN_POINT('Ctrl Pts',(-56.9177055635009,-81.5698776231775,
19.5999999978021));
#44925=CARTESIAN_POINT('Ctrl Pts',(-56.904206824217,-81.5494766861803,19.6000000000003));
#44926=CARTESIAN_POINT('',(-56.8540093738152,-82.1084399539185,19.9814518777033));
#44927=CARTESIAN_POINT('Ctrl Pts',(-56.8540093738153,-82.1084399539186,
19.981451877705));
#44928=CARTESIAN_POINT('Ctrl Pts',(-56.8546684208551,-82.1078379696138,
19.9804667706938));
#44929=CARTESIAN_POINT('Ctrl Pts',(-56.8553252506811,-82.1072330983662,
19.9794819412701));
#44930=CARTESIAN_POINT('Ctrl Pts',(-56.885259036188,-82.0794420009762,19.9344611450319));
#44931=CARTESIAN_POINT('Ctrl Pts',(-56.9102018414315,-82.0463986825325,
19.8908548938768));
#44932=CARTESIAN_POINT('Ctrl Pts',(-56.9487731320942,-81.971873545886,19.8095675441362));
#44933=CARTESIAN_POINT('Ctrl Pts',(-56.9629285185929,-81.9303820655268,
19.7713797660207));
#44934=CARTESIAN_POINT('Ctrl Pts',(-56.9758152663889,-81.8565882282959,
19.7154512870322));
#44935=CARTESIAN_POINT('Ctrl Pts',(-56.9783326975642,-81.8263046345426,
19.6951999589232));
#44936=CARTESIAN_POINT('Ctrl Pts',(-56.9777960279009,-81.7949165905344,
19.6772168782191));
#44937=CARTESIAN_POINT('',(-56.3459906261847,-81.4915600460814,20.0185481222946));
#44938=CARTESIAN_POINT('Origin',(-56.6,-81.8,20.));
#44939=CARTESIAN_POINT('Ctrl Pts',(-56.904206824217,-81.5494766861803,19.6000000000003));
#44940=CARTESIAN_POINT('Ctrl Pts',(-56.8973970622138,-81.5391849453983,
19.6000000011092));
#44941=CARTESIAN_POINT('Ctrl Pts',(-56.8901026392551,-81.5291872963679,
19.6005647878238));
#44942=CARTESIAN_POINT('Ctrl Pts',(-56.8585917514376,-81.4901248771223,
19.6052302094125));
#44943=CARTESIAN_POINT('Ctrl Pts',(-56.8314688441805,-81.4653796121322,
19.6140191854886));
#44944=CARTESIAN_POINT('Ctrl Pts',(-56.7680758300491,-81.4230398883288,
19.642457690764));
#44945=CARTESIAN_POINT('Ctrl Pts',(-56.7324621427979,-81.4078826250911,
19.6628251782062));
#44946=CARTESIAN_POINT('Ctrl Pts',(-56.6455280686385,-81.3857136829775,
19.720036209981));
#44947=CARTESIAN_POINT('Ctrl Pts',(-56.5917170173975,-81.3846886026211,
19.7618502488057));
#44948=CARTESIAN_POINT('Ctrl Pts',(-56.4686735219491,-81.4084196738685,
19.8721932058865));
#44949=CARTESIAN_POINT('Ctrl Pts',(-56.4020317358757,-81.4415416401364,
19.9435530185242));
#44950=CARTESIAN_POINT('Ctrl Pts',(-56.3473237567345,-81.4903583244829,
20.016756128899));
#44951=CARTESIAN_POINT('Ctrl Pts',(-56.3466561735294,-81.4909580671593,
20.0176521239571));
#44952=CARTESIAN_POINT('Ctrl Pts',(-56.3459906261847,-81.4915600460814,
20.018548122295));
#44953=CARTESIAN_POINT('',(-58.4561395287659,-80.2714145057222,19.6));
#44954=CARTESIAN_POINT('',(-58.4561395287659,-80.2714145057222,19.6));
#44955=CARTESIAN_POINT('',(-58.4561395287659,-80.2714145057222,20.4));
#44956=CARTESIAN_POINT('Ctrl Pts',(-58.4561395287659,-80.2714145057222,
20.4));
#44957=CARTESIAN_POINT('Ctrl Pts',(-58.4549779405932,-80.2713020939635,
20.4));
#44958=CARTESIAN_POINT('Ctrl Pts',(-58.4538163849693,-80.2711893225306,
20.399997446394));
#44959=CARTESIAN_POINT('Ctrl Pts',(-58.3971341356222,-80.2656685650122,
20.3997479784273));
#44960=CARTESIAN_POINT('Ctrl Pts',(-58.3414898505613,-80.2594046889495,
20.3936592925489));
#44961=CARTESIAN_POINT('Ctrl Pts',(-58.2289948837902,-80.2452515766898,
20.3673459197356));
#44962=CARTESIAN_POINT('Ctrl Pts',(-58.1720125290647,-80.2372017088335,
20.3458022795996));
#44963=CARTESIAN_POINT('Ctrl Pts',(-58.0772658128868,-80.2227516349081,
20.2901288280491));
#44964=CARTESIAN_POINT('Ctrl Pts',(-58.0378581810609,-80.2163033472798,
20.258674501957));
#44965=CARTESIAN_POINT('Ctrl Pts',(-57.9781037597976,-80.2061585356058,
20.189514384551));
#44966=CARTESIAN_POINT('Ctrl Pts',(-57.9560095763437,-80.2022476217727,
20.1541222320853));
#44967=CARTESIAN_POINT('Ctrl Pts',(-57.9265724533894,-80.1969765246161,
20.0784874840272));
#44968=CARTESIAN_POINT('Ctrl Pts',(-57.9189967544966,-80.1955858364017,
20.0396265746691));
#44969=CARTESIAN_POINT('Ctrl Pts',(-57.9189967544966,-80.1955858364017,
19.9603734253309));
#44970=CARTESIAN_POINT('Ctrl Pts',(-57.9265724533894,-80.1969765246161,
19.9215125159728));
#44971=CARTESIAN_POINT('Ctrl Pts',(-57.9560095763437,-80.2022476217727,
19.8458777679147));
#44972=CARTESIAN_POINT('Ctrl Pts',(-57.9781037597976,-80.2061585356058,
19.810485615449));
#44973=CARTESIAN_POINT('Ctrl Pts',(-58.0378581810609,-80.2163033472798,
19.741325498043));
#44974=CARTESIAN_POINT('Ctrl Pts',(-58.0772658128868,-80.2227516349081,
19.7098711719509));
#44975=CARTESIAN_POINT('Ctrl Pts',(-58.1720125290647,-80.2372017088335,
19.6541977204004));
#44976=CARTESIAN_POINT('Ctrl Pts',(-58.2289948837902,-80.2452515766898,
19.6326540802644));
#44977=CARTESIAN_POINT('Ctrl Pts',(-58.3414898505845,-80.2594046889524,
19.6063407074457));
#44978=CARTESIAN_POINT('Ctrl Pts',(-58.3971341357726,-80.2656685650308,
19.6002520215721));
#44979=CARTESIAN_POINT('Ctrl Pts',(-58.4538163849616,-80.2711893225295,
19.600002553606));
#44980=CARTESIAN_POINT('Ctrl Pts',(-58.4549779406011,-80.2713020939643,
19.6));
#44981=CARTESIAN_POINT('Ctrl Pts',(-58.4561395287659,-80.2714145057222,
19.6));
#44982=CARTESIAN_POINT('Ctrl Pts',(-58.4561395287659,-80.2714145057222,
19.6));
#44983=CARTESIAN_POINT('Ctrl Pts',(-58.456027117008,-80.2725760938874,19.6));
#44984=CARTESIAN_POINT('Ctrl Pts',(-58.4559150644895,-80.2737377190986,
19.600002553606));
#44985=CARTESIAN_POINT('Ctrl Pts',(-58.4504644075707,-80.3304267522263,
19.6002520215721));
#44986=CARTESIAN_POINT('Ctrl Pts',(-58.4459421116762,-80.3862395774228,
19.6063407074461));
#44987=CARTESIAN_POINT('Ctrl Pts',(-58.4382613890477,-80.4993609045025,
19.6326540802644));
#44988=CARTESIAN_POINT('Ctrl Pts',(-58.4352353645325,-80.5568294376158,
19.6541977204004));
#44989=CARTESIAN_POINT('Ctrl Pts',(-58.4312493657365,-80.6525888062256,
19.7098711719509));
#44990=CARTESIAN_POINT('Ctrl Pts',(-58.4300214794505,-80.6925016381814,
19.741325498043));
#44991=CARTESIAN_POINT('Ctrl Pts',(-58.4285199726038,-80.753092508299,19.810485615449));
#44992=CARTESIAN_POINT('Ctrl Pts',(-58.4281216961571,-80.7755266244031,
19.8458777679147));
#44993=CARTESIAN_POINT('Ctrl Pts',(-58.4276503349443,-80.8054282379327,
19.9215125159728));
#44994=CARTESIAN_POINT('Ctrl Pts',(-58.4275625567855,-80.8131300248954,
19.9603734253309));
#44995=CARTESIAN_POINT('Ctrl Pts',(-58.4275625567855,-80.8131300248954,
20.0396265746691));
#44996=CARTESIAN_POINT('Ctrl Pts',(-58.4276503349443,-80.8054282379327,
20.0784874840272));
#44997=CARTESIAN_POINT('Ctrl Pts',(-58.4281216961571,-80.7755266244031,
20.1541222320853));
#44998=CARTESIAN_POINT('Ctrl Pts',(-58.4285199726038,-80.753092508299,20.189514384551));
#44999=CARTESIAN_POINT('Ctrl Pts',(-58.4300214794505,-80.6925016381814,
20.258674501957));
#45000=CARTESIAN_POINT('Ctrl Pts',(-58.4312493657365,-80.6525888062256,
20.2901288280491));
#45001=CARTESIAN_POINT('Ctrl Pts',(-58.4352353645325,-80.5568294376159,
20.3458022795996));
#45002=CARTESIAN_POINT('Ctrl Pts',(-58.4382613890477,-80.4993609045026,
20.3673459197356));
#45003=CARTESIAN_POINT('Ctrl Pts',(-58.4459421116747,-80.3862395774449,
20.3936592925487));
#45004=CARTESIAN_POINT('Ctrl Pts',(-58.4504644075606,-80.3304267523694,
20.3997479784273));
#45005=CARTESIAN_POINT('Ctrl Pts',(-58.4559150644899,-80.2737377190912,
20.399997446394));
#45006=CARTESIAN_POINT('Ctrl Pts',(-58.4560271170072,-80.272576093895,20.4));
#45007=CARTESIAN_POINT('Ctrl Pts',(-58.4561395287659,-80.2714145057222,
20.4));
#45008=CARTESIAN_POINT('Origin',(-56.6,-81.8,20.));
#45009=CARTESIAN_POINT('',(-56.6,-81.8,20.));
#45010=CARTESIAN_POINT('Origin',(-60.,-79.,20.));
#45011=CARTESIAN_POINT('',(-61.6,-79.,20.));
#45012=CARTESIAN_POINT('Origin',(-62.,-79.,20.));
#45013=CARTESIAN_POINT('Origin',(-60.,-79.,20.));
#45014=CARTESIAN_POINT('Origin',(-56.6,-81.8,20.));
#45015=CARTESIAN_POINT('Origin',(-56.6,-81.8,20.));
#45016=CARTESIAN_POINT('Ctrl Pts',(-56.998865393003,-81.8104071381607,19.971749517882));
#45017=CARTESIAN_POINT('Ctrl Pts',(-56.9761215679777,-81.8098137095668,
19.6504133876692));
#45018=CARTESIAN_POINT('Ctrl Pts',(-56.9306422269741,-81.702749946835,19.0272055496801));
#45019=CARTESIAN_POINT('Ctrl Pts',(-56.8393882333594,-81.0832286625891,
17.8952792144066));
#45020=CARTESIAN_POINT('Ctrl Pts',(-56.7246941823819,-79.659154025169,16.9983829421965));
#45021=CARTESIAN_POINT('Ctrl Pts',(-56.5861632252162,-77.6335534097869,
17.2233006398626));
#45022=CARTESIAN_POINT('Ctrl Pts',(-56.4467017882273,-76.1835978989143,
18.6719551219413));
#45023=CARTESIAN_POINT('Ctrl Pts',(-56.3063357852564,-75.9481362494154,
20.7219582178088));
#45024=CARTESIAN_POINT('Ctrl Pts',(-56.1650671343952,-77.0524010984881,
22.4820287706829));
#45025=CARTESIAN_POINT('Ctrl Pts',(-56.022913716882,-79.0240846877592,23.1743286974061));
#45026=CARTESIAN_POINT('Ctrl Pts',(-55.8798883483141,-81.0099417524087,
22.4819069016305));
#45027=CARTESIAN_POINT('Ctrl Pts',(-55.736009170698,-82.1371435389622,20.6919014148508));
#45028=CARTESIAN_POINT('Ctrl Pts',(-55.5912948188564,-81.9011989467447,
18.5773811983794));
#45029=CARTESIAN_POINT('Ctrl Pts',(-55.4457664679998,-80.3895075735084,
17.0631066199702));
#45030=CARTESIAN_POINT('Ctrl Pts',(-55.2994467925014,-78.2525981471427,
16.8201567755944));
#45031=CARTESIAN_POINT('Ctrl Pts',(-55.1523606723563,-76.4194586046196,
17.9695089930655));
#45032=CARTESIAN_POINT('Ctrl Pts',(-55.0291720750146,-75.8221765197523,
19.6778401981353));
#45033=CARTESIAN_POINT('Ctrl Pts',(-54.9302657004888,-76.0582767873485,
21.0517631272575));
#45034=CARTESIAN_POINT('Ctrl Pts',(-54.855911693957,-76.563774636797,21.9689095801494));
#45035=CARTESIAN_POINT('Ctrl Pts',(-54.7813873081152,-77.3470208623382,
22.6677199767267));
#45036=CARTESIAN_POINT('Ctrl Pts',(-54.6817995343713,-78.6425182874698,
23.2077559592215));
#45037=CARTESIAN_POINT('Ctrl Pts',(-54.5569085657542,-80.4660663250115,
23.0055515481889));
#45038=CARTESIAN_POINT('Ctrl Pts',(-54.4064224477222,-82.0323869212294,
21.4408137908159));
#45039=CARTESIAN_POINT('Ctrl Pts',(-54.2553538136249,-82.282138366727,19.2347828818201));
#45040=CARTESIAN_POINT('Ctrl Pts',(-54.1037383696759,-81.0976521492529,
17.3450468644423));
#45041=CARTESIAN_POINT('Ctrl Pts',(-53.9516134654316,-78.9865131673676,
16.6079479997978));
#45042=CARTESIAN_POINT('Ctrl Pts',(-53.799017300736,-76.8685737480114,17.3474746287888));
#45043=CARTESIAN_POINT('Ctrl Pts',(-53.6459896567803,-75.6706931696044,
19.2519276595415));
#45044=CARTESIAN_POINT('Ctrl Pts',(-53.4925710331048,-75.9223549441939,
21.4933728414198));
#45045=CARTESIAN_POINT('Ctrl Pts',(-53.3388026326536,-77.5204065688237,
23.0925152589881));
#45046=CARTESIAN_POINT('Ctrl Pts',(-53.1847265069516,-79.7714109640732,
23.3467986618763));
#45047=CARTESIAN_POINT('Ctrl Pts',(-53.03038548168,-81.6931375902356,22.1399790200489));
#45048=CARTESIAN_POINT('Ctrl Pts',(-52.875823002085,-82.4441600599385,19.9951637320667));
#45049=CARTESIAN_POINT('Ctrl Pts',(-52.7210833439104,-81.6931147568403,
17.847607587344));
#45050=CARTESIAN_POINT('Ctrl Pts',(-52.5662111784277,-79.7652472072559,
16.6359089985643));
#45051=CARTESIAN_POINT('Ctrl Pts',(-52.411251276088,-77.5012356580149,16.8908255535852));
#45052=CARTESIAN_POINT('Ctrl Pts',(-52.256248453475,-75.8897320482582,18.5022380823304));
#45053=CARTESIAN_POINT('Ctrl Pts',(-52.1012476567581,-75.6346189430596,
20.7668255842009));
#45054=CARTESIAN_POINT('Ctrl Pts',(-51.946293812071,-76.8468283649895,22.6957639240306));
#45055=CARTESIAN_POINT('Ctrl Pts',(-51.7914318627055,-78.9959989264195,
23.4475029895662));
#45056=CARTESIAN_POINT('Ctrl Pts',(-51.6367067716067,-81.143023685764,22.6958068198001));
#45057=CARTESIAN_POINT('Ctrl Pts',(-51.4821631962239,-82.3514430242135,
20.7716237421131));
#45058=CARTESIAN_POINT('Ctrl Pts',(-51.3278450629361,-82.0966921870304,
18.5171370441619));
#45059=CARTESIAN_POINT('Ctrl Pts',(-51.173795763927,-80.494660275846,16.9160818675009));
#45060=CARTESIAN_POINT('Ctrl Pts',(-51.0200579736735,-78.2481247248837,
16.6640082062395));
#45061=CARTESIAN_POINT('Ctrl Pts',(-50.8666737295509,-76.3395049302381,
17.8643638570452));
#45062=CARTESIAN_POINT('Ctrl Pts',(-50.713684168159,-75.5963279226902,19.9885708308413));
#45063=CARTESIAN_POINT('Ctrl Pts',(-50.561130291697,-76.3404917399077,22.103826159149));
#45064=CARTESIAN_POINT('Ctrl Pts',(-50.4090511127719,-78.2340315759714,
23.2925880511682));
#45065=CARTESIAN_POINT('Ctrl Pts',(-50.2574850343491,-80.4481760005255,
23.0417916058766));
#45066=CARTESIAN_POINT('Ctrl Pts',(-50.1064690255066,-82.01705159905,21.4708528285098));
#45067=CARTESIAN_POINT('Ctrl Pts',(-49.9560387185426,-82.2630418039423,
19.2728709293431));
#45068=CARTESIAN_POINT('Ctrl Pts',(-49.8062283566168,-81.0898252948096,
17.4088059239318));
#45069=CARTESIAN_POINT('Ctrl Pts',(-49.6570709537323,-79.019024315676,16.68592863221));
#45070=CARTESIAN_POINT('Ctrl Pts',(-49.5085980443133,-76.9595196408508,
17.4088734508976));
#45071=CARTESIAN_POINT('Ctrl Pts',(-49.3608396229039,-75.8040867405457,
19.24850872357));
#45072=CARTESIAN_POINT('Ctrl Pts',(-49.2138236838193,-76.0501675357259,
21.3978373023004));
#45073=CARTESIAN_POINT('Ctrl Pts',(-49.0675767596914,-77.5665861446786,
22.9130985070277));
#45074=CARTESIAN_POINT('Ctrl Pts',(-48.9059614999196,-79.9400679445208,
23.1852360004509));
#45075=CARTESIAN_POINT('Ctrl Pts',(-48.7614602181023,-81.6648094897616,
21.8082179781191));
#45076=CARTESIAN_POINT('Ctrl Pts',(-48.641745504212,-82.0326853928027,20.1333807208566));
#45077=CARTESIAN_POINT('Ctrl Pts',(-48.5622130344089,-81.8465385109611,
19.0326778475393));
#45078=CARTESIAN_POINT('Ctrl Pts',(-48.4670622745342,-81.1987085058851,
17.8562669615047));
#45079=CARTESIAN_POINT('Ctrl Pts',(-48.3486693000866,-79.7268341045547,
16.9318783271684));
#45080=CARTESIAN_POINT('Ctrl Pts',(-48.2074855512855,-77.6628755974866,
17.1663816685728));
#45081=CARTESIAN_POINT('Ctrl Pts',(-48.0672023078574,-76.206752176544,18.626431849987));
#45082=CARTESIAN_POINT('Ctrl Pts',(-47.927830219219,-75.9792981345661,20.6628912290644));
#45083=CARTESIAN_POINT('Ctrl Pts',(-47.7893778161085,-77.0643886294908,
22.3852565245146));
#45084=CARTESIAN_POINT('Ctrl Pts',(-47.6518515237459,-78.9735990241534,
23.0508787165266));
#45085=CARTESIAN_POINT('Ctrl Pts',(-47.5152556014389,-80.8684432520523,
22.3853788812134));
#45086=CARTESIAN_POINT('Ctrl Pts',(-47.3795921088708,-81.9276134623547,
20.6952758178572));
#45087=CARTESIAN_POINT('Ctrl Pts',(-47.2448609079158,-81.7034807862736,
18.7270982413631));
#45088=CARTESIAN_POINT('Ctrl Pts',(-47.1110596886693,-80.3107425715779,
17.3377494473466));
#45089=CARTESIAN_POINT('Ctrl Pts',(-46.9781840026693,-78.3691181398569,
17.1212491527646));
#45090=CARTESIAN_POINT('Ctrl Pts',(-46.8462272430603,-76.7274568500113,
18.1555514656259));
#45091=CARTESIAN_POINT('Ctrl Pts',(-46.7151806507337,-76.0932466642441,
19.9745644839421));
#45092=CARTESIAN_POINT('Ctrl Pts',(-46.5850332874596,-76.72689365866,21.7807592120224));
#45093=CARTESIAN_POINT('Ctrl Pts',(-46.4773155913697,-78.0692304834685,
22.6203028484064));
#45094=CARTESIAN_POINT('Ctrl Pts',(-46.3915770038462,-79.2743999206746,
22.6845333353118));
#45095=CARTESIAN_POINT('Ctrl Pts',(-46.306125933356,-80.4347163011863,22.3540877308873));
#45096=CARTESIAN_POINT('Ctrl Pts',(-46.2140165472685,-81.3855756228331,
21.3981264795911));
#45097=CARTESIAN_POINT('Ctrl Pts',(-46.0871761509613,-81.7920886092443,
19.6302877304961));
#45098=CARTESIAN_POINT('Ctrl Pts',(-45.9979124562317,-81.2080139528857,
18.4010685232934));
#45099=CARTESIAN_POINT('Ctrl Pts',(-45.931706785465,-80.4609863771443,17.8600692258404));
#45100=CARTESIAN_POINT('Ctrl Pts',(-45.8899254264441,-79.9656081265692,
17.5575209097683));
#45101=CARTESIAN_POINT('Ctrl Pts',(-45.8118000032237,-78.880763795498,17.2764338892227));
#45102=CARTESIAN_POINT('Ctrl Pts',(-45.6978306326569,-77.2975836321059,
17.8314065963964));
#45103=CARTESIAN_POINT('Ctrl Pts',(-45.5742396517875,-76.3354201599197,
19.3681907346036));
#45104=CARTESIAN_POINT('Ctrl Pts',(-45.437706343548,-76.5552758080846,21.3715656944865));
#45105=CARTESIAN_POINT('Ctrl Pts',(-45.3020562393531,-78.1821308742347,
22.6659223685449));
#45106=CARTESIAN_POINT('Ctrl Pts',(-45.1941987227426,-79.758928297719,22.475534026443));
#45107=CARTESIAN_POINT('Ctrl Pts',(-45.0866996199815,-81.0338356970261,
21.6807000396746));
#45108=CARTESIAN_POINT('Ctrl Pts',(-44.9662578644687,-81.8333475233177,
20.012518703382));
#45109=CARTESIAN_POINT('Ctrl Pts',(-44.8243750512167,-80.8834891862673,
18.0522457056093));
#45110=CARTESIAN_POINT('Ctrl Pts',(-44.7007996247099,-79.204627825654,17.4066536628875));
#45111=CARTESIAN_POINT('Ctrl Pts',(-44.5952423985192,-77.7129206082217,
17.7439551046314));
#45112=CARTESIAN_POINT('Ctrl Pts',(-44.4900223228441,-76.6730225954323,
18.8674759604783));
#45113=CARTESIAN_POINT('Ctrl Pts',(-44.3851107070103,-76.4459242852341,
20.3731595407077));
#45114=CARTESIAN_POINT('Ctrl Pts',(-44.280478717402,-77.1066399045476,21.7436998539951));
#45115=CARTESIAN_POINT('Ctrl Pts',(-44.1847949217249,-78.3107241896412,
22.4370140832109));
#45116=CARTESIAN_POINT('Ctrl Pts',(-44.0979705969536,-79.5480359338008,
22.4357585099148));
#45117=CARTESIAN_POINT('Ctrl Pts',(-44.0199391969229,-80.5493767638303,
21.9538965049427));
#45118=CARTESIAN_POINT('Ctrl Pts',(-43.9549950707645,-81.1260138276735,
21.230332507434));
#45119=CARTESIAN_POINT('Ctrl Pts',(-43.9030819779796,-81.3650788043183,
20.5453498510557));
#45120=CARTESIAN_POINT('Ctrl Pts',(-43.8511952002441,-81.4469675514213,
19.8246440252031));
#45121=CARTESIAN_POINT('Ctrl Pts',(-43.786381545381,-81.2412693616971,18.9250357363984));
#45122=CARTESIAN_POINT('Ctrl Pts',(-43.7086639057346,-80.5513181773471,
18.058939887935));
#45123=CARTESIAN_POINT('Ctrl Pts',(-43.6309915965552,-79.554575354439,17.5802369898606));
#45124=CARTESIAN_POINT('Ctrl Pts',(-43.5404114400028,-78.2638755524742,
17.5781557379155));
#45125=CARTESIAN_POINT('Ctrl Pts',(-43.4369226415031,-76.9748964799918,
18.3837836136963));
#45126=CARTESIAN_POINT('Ctrl Pts',(-43.3204955018513,-76.409902299744,20.0015897439));
#45127=CARTESIAN_POINT('Ctrl Pts',(-43.2040204721867,-76.9752002181154,
21.6172377254714));
#45128=CARTESIAN_POINT('Ctrl Pts',(-43.0874525410452,-78.4262949071933,
22.5297854402615));
#45129=CARTESIAN_POINT('Ctrl Pts',(-42.9707470684933,-80.1313821068561,
22.3379694555197));
#45130=CARTESIAN_POINT('Ctrl Pts',(-42.8538596468785,-81.3469559099921,
21.1232848086745));
#45131=CARTESIAN_POINT('Ctrl Pts',(-42.7367469025614,-81.5402924255104,
19.4123612569526));
#45132=CARTESIAN_POINT('Ctrl Pts',(-42.6193646471204,-80.6227499332965,
17.950746393619));
#45133=CARTESIAN_POINT('Ctrl Pts',(-42.5016723128577,-78.9894841983059,
17.3785603509998));
#45134=CARTESIAN_POINT('Ctrl Pts',(-42.3836228189166,-77.3512439815465,
17.9509054109146));
#45135=CARTESIAN_POINT('Ctrl Pts',(-42.2651858183516,-76.4228942839963,
19.4252147114051));
#45136=CARTESIAN_POINT('Ctrl Pts',(-42.1462969423314,-76.6193425219703,
21.1617531840419));
#45137=CARTESIAN_POINT('Ctrl Pts',(-42.0269611323496,-77.8579790787978,
22.4041645790426));
#45138=CARTESIAN_POINT('Ctrl Pts',(-41.9070542715169,-79.6104428558897,
22.601547445429));
#45139=CARTESIAN_POINT('Ctrl Pts',(-41.8067886921112,-80.8577927602762,
21.8204122976217));
#45140=CARTESIAN_POINT('Ctrl Pts',(-41.7260879027667,-81.4058116777841,
20.8193752889488));
#45141=CARTESIAN_POINT('Ctrl Pts',(-41.6858137213157,-81.5009183081234,
20.2675948162325));
#45142=CARTESIAN_POINT('Ctrl Pts',(-41.6655045384048,-81.5014482121737,
19.980656523783));
#45143=CARTESIAN_POINT('Ctrl Pts',(-57.0019869965663,-81.6907681353096,
19.971749517882));
#45144=CARTESIAN_POINT('Ctrl Pts',(-56.9801545695107,-81.6901984867797,
19.663290073818));
#45145=CARTESIAN_POINT('Ctrl Pts',(-56.9366454549946,-81.5877436991947,
19.0670363519488));
#45146=CARTESIAN_POINT('Ctrl Pts',(-56.8491846045637,-80.9941573968246,
17.9820163561888));
#45147=CARTESIAN_POINT('Ctrl Pts',(-56.7393118494271,-79.6295959629488,
17.1227663162549));
#45148=CARTESIAN_POINT('Ctrl Pts',(-56.6064781904435,-77.6872334681487,
17.3380508628845));
#45149=CARTESIAN_POINT('Ctrl Pts',(-56.4726828633942,-76.2958461360222,
18.7279994719948));
#45150=CARTESIAN_POINT('Ctrl Pts',(-56.3379160681303,-76.0694886906288,
20.6963932339323));
#45151=CARTESIAN_POINT('Ctrl Pts',(-56.2021929256842,-77.1304743295524,
22.3880320262854));
#45152=CARTESIAN_POINT('Ctrl Pts',(-56.0654858506924,-79.0269074027327,
23.0542475046959));
#45153=CARTESIAN_POINT('Ctrl Pts',(-55.9278104502865,-80.9390721595663,
22.3879092034606));
#45154=CARTESIAN_POINT('Ctrl Pts',(-55.7891657233314,-82.0258490619999,
20.6628380569866));
#45155=CARTESIAN_POINT('Ctrl Pts',(-55.6495621609665,-81.7986045584916,
18.6224539012947));
#45156=CARTESIAN_POINT('Ctrl Pts',(-55.5090063278671,-80.3385390793215,
17.15925969508));
#45157=CARTESIAN_POINT('Ctrl Pts',(-55.367513994765,-78.2716513700982,16.9237976938686));
#45158=CARTESIAN_POINT('Ctrl Pts',(-55.2250902663515,-76.4959591428919,
18.0365569888073));
#45159=CARTESIAN_POINT('Ctrl Pts',(-55.1056572247686,-75.9163181618903,
19.6932190528411));
#45160=CARTESIAN_POINT('Ctrl Pts',(-55.0096417192807,-76.1454620591887,
21.0271736310102));
#45161=CARTESIAN_POINT('Ctrl Pts',(-54.9374115962142,-76.6365391415173,
21.918279169925));
#45162=CARTESIAN_POINT('Ctrl Pts',(-54.8649633201778,-77.398040791451,22.5977776331588));
#45163=CARTESIAN_POINT('Ctrl Pts',(-54.7680757073581,-78.6585216738225,
23.1233216086256));
#45164=CARTESIAN_POINT('Ctrl Pts',(-54.6464650009296,-80.4348314338745,
22.9268255090038));
#45165=CARTESIAN_POINT('Ctrl Pts',(-54.4996934767181,-81.9633416794487,
21.4007041190596));
#45166=CARTESIAN_POINT('Ctrl Pts',(-54.3521194914096,-82.207945805232,19.2451779007863));
#45167=CARTESIAN_POINT('Ctrl Pts',(-54.2037864512958,-81.0491986386383,
17.3953506314354));
#45168=CARTESIAN_POINT('Ctrl Pts',(-54.0546726002324,-78.9797161272989,
16.6721627753971));
#45169=CARTESIAN_POINT('Ctrl Pts',(-53.9048744917015,-76.8997385794412,
17.3977515494516));
#45170=CARTESIAN_POINT('Ctrl Pts',(-53.7543943945856,-75.7208910787165,
19.2707235463476));
#45171=CARTESIAN_POINT('Ctrl Pts',(-53.6032700366971,-75.9682122953648,
21.4793965483087));
#45172=CARTESIAN_POINT('Ctrl Pts',(-53.4515364940605,-77.5451237531408,
23.0583259880909));
#45173=CARTESIAN_POINT('Ctrl Pts',(-53.2992315669793,-79.7708514113732,
23.3104301280262));
#45174=CARTESIAN_POINT('Ctrl Pts',(-53.1463938538412,-81.674796438284,22.1155785760537));
#45175=CARTESIAN_POINT('Ctrl Pts',(-52.9930634292223,-82.4207031937924,
19.9874447955775));
#45176=CARTESIAN_POINT('Ctrl Pts',(-52.8392816877573,-81.674734243082,17.8523154647485));
#45177=CARTESIAN_POINT('Ctrl Pts',(-52.685091115623,-79.7551482890924,16.6450035815774));
#45178=CARTESIAN_POINT('Ctrl Pts',(-52.5305349248319,-77.4962905952853,
16.8986406907687));
#45179=CARTESIAN_POINT('Ctrl Pts',(-52.3756570363291,-75.8851236735628,
18.5087336570864));
#45180=CARTESIAN_POINT('Ctrl Pts',(-52.2205021178324,-75.6289937996702,
20.7761504419683));
#45181=CARTESIAN_POINT('Ctrl Pts',(-52.0651155111308,-76.8443509963939,
22.7113962588161));
#45182=CARTESIAN_POINT('Ctrl Pts',(-51.9095431202422,-79.0037626673798,
23.4674453589518));
#45183=CARTESIAN_POINT('Ctrl Pts',(-51.7538317605233,-81.1653007981464,
22.7113908580931));
#45184=CARTESIAN_POINT('Ctrl Pts',(-51.5980280916369,-82.3844800346085,
20.7713497617126));
#45185=CARTESIAN_POINT('Ctrl Pts',(-51.4421798125795,-82.1278008744938,
18.4938138332471));
#45186=CARTESIAN_POINT('Ctrl Pts',(-51.2863321673339,-80.5071214327334,
16.8731800143954));
#45187=CARTESIAN_POINT('Ctrl Pts',(-51.130536019338,-78.2299651325731,16.6170046250107));
#45188=CARTESIAN_POINT('Ctrl Pts',(-50.9748294395751,-76.2916779025706,
17.8352675022703));
#45189=CARTESIAN_POINT('Ctrl Pts',(-50.8192788139203,-75.535222425711,19.9954618233132));
#45190=CARTESIAN_POINT('Ctrl Pts',(-50.6638867930748,-76.2927555227092,
22.1505393874449));
#45191=CARTESIAN_POINT('Ctrl Pts',(-50.5087514726537,-78.2244666356574,
23.3639881816775));
#45192=CARTESIAN_POINT('Ctrl Pts',(-50.3538945398054,-80.4872358031265,
23.1082751603607));
#45193=CARTESIAN_POINT('Ctrl Pts',(-50.1993628432606,-82.0933694651835,
21.5008310722846));
#45194=CARTESIAN_POINT('Ctrl Pts',(-50.0451997389494,-82.3460604904031,
19.2479176258722));
#45195=CARTESIAN_POINT('Ctrl Pts',(-49.8914483697448,-81.1422016319754,
17.3341629878747));
#45196=CARTESIAN_POINT('Ctrl Pts',(-49.7381512549702,-79.0137037469387,
16.5905910347466));
#45197=CARTESIAN_POINT('Ctrl Pts',(-49.5853491463611,-76.8936172217032,
17.3342716101559));
#45198=CARTESIAN_POINT('Ctrl Pts',(-49.4330838300899,-75.7023254250077,
19.23006834526));
#45199=CARTESIAN_POINT('Ctrl Pts',(-49.2813906500908,-75.9558173014907,
21.4481635243258));
#45200=CARTESIAN_POINT('Ctrl Pts',(-49.1303147410793,-77.5222584825662,
23.0139808902264));
#45201=CARTESIAN_POINT('Ctrl Pts',(-48.9631599505202,-79.9772604688309,
23.2959931188457));
#45202=CARTESIAN_POINT('Ctrl Pts',(-48.8135053288752,-81.7639158613361,
21.8703489536029));
#45203=CARTESIAN_POINT('Ctrl Pts',(-48.6894028260435,-82.1454765472973,
20.1340332249349));
#45204=CARTESIAN_POINT('Ctrl Pts',(-48.606909800781,-81.9524122938921,18.9923151182377));
#45205=CARTESIAN_POINT('Ctrl Pts',(-48.508170467145,-81.2801964984991,17.7714890537002));
#45206=CARTESIAN_POINT('Ctrl Pts',(-48.3852366463024,-79.7519113147864,
16.811404479291));
#45207=CARTESIAN_POINT('Ctrl Pts',(-48.2385155735682,-77.6069227684042,
17.0548447507493));
#45208=CARTESIAN_POINT('Ctrl Pts',(-48.0926237391039,-76.0923857542406,
18.5731419517954));
#45209=CARTESIAN_POINT('Ctrl Pts',(-47.947583021408,-75.855478330155,20.6924131824904));
#45210=CARTESIAN_POINT('Ctrl Pts',(-47.8034159184779,-76.9851960001735,
22.4859469609739));
#45211=CARTESIAN_POINT('Ctrl Pts',(-47.6601418264662,-78.9740985729673,
23.1795079552557));
#45212=CARTESIAN_POINT('Ctrl Pts',(-47.5177785879326,-80.9488982642021,
22.4860500718809));
#45213=CARTESIAN_POINT('Ctrl Pts',(-47.3763417219138,-82.0531474374999,
20.7241762413299));
#45214=CARTESIAN_POINT('Ctrl Pts',(-47.235844434292,-81.8194952609905,18.6719275218613));
#45215=CARTESIAN_POINT('Ctrl Pts',(-47.0962979916432,-80.3671156551725,
17.2230535256656));
#45216=CARTESIAN_POINT('Ctrl Pts',(-46.9577106913804,-78.3422825162418,
16.9972911628132));
#45217=CARTESIAN_POINT('Ctrl Pts',(-46.8200902726817,-76.6304302822888,
18.075883028566));
#45218=CARTESIAN_POINT('Ctrl Pts',(-46.6834384403178,-75.9693039379864,
19.9724034084133));
#45219=CARTESIAN_POINT('Ctrl Pts',(-46.5477630195146,-76.6298878847089,
21.8549661590069));
#45220=CARTESIAN_POINT('Ctrl Pts',(-46.4355022701039,-78.0285744887402,
22.7295728438287));
#45221=CARTESIAN_POINT('Ctrl Pts',(-46.3461948648046,-79.2837766671998,
22.7964336666031));
#45222=CARTESIAN_POINT('Ctrl Pts',(-46.2572098972965,-80.491947115071,22.4523137524949));
#45223=CARTESIAN_POINT('Ctrl Pts',(-46.1613273153243,-81.4814786400232,
21.4572593980856));
#45224=CARTESIAN_POINT('Ctrl Pts',(-46.029379168661,-81.9042028287135,19.6183514631787));
#45225=CARTESIAN_POINT('Ctrl Pts',(-45.9365841068927,-81.2968358878326,
18.3408380995742));
#45226=CARTESIAN_POINT('Ctrl Pts',(-45.8678105576775,-80.5209218669219,
17.7789311757114));
#45227=CARTESIAN_POINT('Ctrl Pts',(-45.8244172040792,-80.0064507564458,
17.4647228951126));
#45228=CARTESIAN_POINT('Ctrl Pts',(-45.7433029268672,-78.8802013286524,
17.1730202319442));
#45229=CARTESIAN_POINT('Ctrl Pts',(-45.625023158468,-77.238153925619,17.749002446988));
#45230=CARTESIAN_POINT('Ctrl Pts',(-45.4969734702573,-76.2416278070243,
19.3413279722522));
#45231=CARTESIAN_POINT('Ctrl Pts',(-45.3556138735636,-76.4696516892768,
21.4144303969982));
#45232=CARTESIAN_POINT('Ctrl Pts',(-45.2154337533091,-78.1509909287844,
22.7510113308197));
#45233=CARTESIAN_POINT('Ctrl Pts',(-45.1041545433855,-79.77719143669,22.5542299247681));
#45234=CARTESIAN_POINT('Ctrl Pts',(-44.9933799101428,-81.0907403963799,
21.7352269105764));
#45235=CARTESIAN_POINT('Ctrl Pts',(-44.8694102564831,-81.9125541069559,
20.0183583220098));
#45236=CARTESIAN_POINT('Ctrl Pts',(-44.7237191663694,-80.9363612867671,
18.0064421148482));
#45237=CARTESIAN_POINT('Ctrl Pts',(-44.5970462847396,-79.2162221332394,
17.3455095591394));
#45238=CARTESIAN_POINT('Ctrl Pts',(-44.4890652688093,-77.6906315220753,
17.6908462673951));
#45239=CARTESIAN_POINT('Ctrl Pts',(-44.3815708076311,-76.6292107816859,
18.8382383324711));
#45240=CARTESIAN_POINT('Ctrl Pts',(-44.2746354502652,-76.3982162105429,
20.3727555213266));
#45241=CARTESIAN_POINT('Ctrl Pts',(-44.1681351294007,-77.0707409099873,
21.7667200651887));
#45242=CARTESIAN_POINT('Ctrl Pts',(-44.0709442472466,-78.2934511464485,
22.4702571756528));
#45243=CARTESIAN_POINT('Ctrl Pts',(-43.982911287045,-79.5475054890082,22.4687580004392));
#45244=CARTESIAN_POINT('Ctrl Pts',(-43.9039153234828,-80.560817283634,21.9809254218161));
#45245=CARTESIAN_POINT('Ctrl Pts',(-43.8382577690521,-81.1433928581717,
21.2496464767121));
#45246=CARTESIAN_POINT('Ctrl Pts',(-43.7858541652558,-81.384655107603,20.5582833734644));
#45247=CARTESIAN_POINT('Ctrl Pts',(-43.7335111620554,-81.46720801557,19.8314057389319));
#45248=CARTESIAN_POINT('Ctrl Pts',(-43.668205947399,-81.2598502135044,18.9251965418744));
#45249=CARTESIAN_POINT('Ctrl Pts',(-43.5900171832591,-80.5657229312084,
18.0541956163639));
#45250=CARTESIAN_POINT('Ctrl Pts',(-43.5119949360051,-79.5647038944138,
17.5736303297245));
#45251=CARTESIAN_POINT('Ctrl Pts',(-43.4211637692904,-78.2706023916298,
17.5717877335082));
#45252=CARTESIAN_POINT('Ctrl Pts',(-43.3175670029884,-76.9810666086263,
18.3784566755502));
#45253=CARTESIAN_POINT('Ctrl Pts',(-43.2012797062853,-76.4177083926015,
19.9937013177312));
#45254=CARTESIAN_POINT('Ctrl Pts',(-43.0852342760176,-76.9813003440223,
21.602448212408));
#45255=CARTESIAN_POINT('Ctrl Pts',(-42.9693708727529,-78.4233112003797,
22.5084979989942));
#45256=CARTESIAN_POINT('Ctrl Pts',(-42.8536484379065,-80.1132146170046,
22.3177218418165));
#45257=CARTESIAN_POINT('Ctrl Pts',(-42.7380174315994,-81.3147326529136,
21.1161627237155));
#45258=CARTESIAN_POINT('Ctrl Pts',(-42.622431553402,-81.5048285111816,19.4282173657));
#45259=CARTESIAN_POINT('Ctrl Pts',(-42.5068436055692,-80.6011664819877,
17.9899070717688));
#45260=CARTESIAN_POINT('Ctrl Pts',(-42.3912050559913,-78.9969340372162,
17.4285740592569));
#45261=CARTESIAN_POINT('Ctrl Pts',(-42.275471116222,-77.3917022239558,17.9900550824597));
#45262=CARTESIAN_POINT('Ctrl Pts',(-42.1595879125518,-76.484399288327,19.4322227612078));
#45263=CARTESIAN_POINT('Ctrl Pts',(-42.0435230131546,-76.6767317876591,
21.126904131581));
#45264=CARTESIAN_POINT('Ctrl Pts',(-41.9272646554307,-77.8836619438754,
22.3367466196967));
#45265=CARTESIAN_POINT('Ctrl Pts',(-41.8106510944935,-79.5876128552717,
22.5280006580125));
#45266=CARTESIAN_POINT('Ctrl Pts',(-41.7133341547954,-80.7980091014391,
21.7698238788751));
#45267=CARTESIAN_POINT('Ctrl Pts',(-41.6350706349544,-81.3292252397651,
20.7991118311558));
#45268=CARTESIAN_POINT('Ctrl Pts',(-41.596096236417,-81.4212850362297,20.2652300023777));
#45269=CARTESIAN_POINT('Ctrl Pts',(-41.5763904523584,-81.4217991964907,
19.9868168306642));
#45270=CARTESIAN_POINT('Ctrl Pts',(-56.8938806655278,-81.449218908126,19.9798472493564));
#45271=CARTESIAN_POINT('Ctrl Pts',(-56.8739034306165,-81.4486976650013,
19.6975988873676));
#45272=CARTESIAN_POINT('Ctrl Pts',(-56.834388516913,-81.3555481289854,19.1561130599078));
#45273=CARTESIAN_POINT('Ctrl Pts',(-56.754710817907,-80.81511613009,18.1675547779568));
#45274=CARTESIAN_POINT('Ctrl Pts',(-56.6548967662929,-79.5747336327388,
17.3876045355145));
#45275=CARTESIAN_POINT('Ctrl Pts',(-56.5342263208108,-77.8106208453556,
17.5830023129393));
#45276=CARTESIAN_POINT('Ctrl Pts',(-56.4128097095029,-76.5479937245359,
18.8448683450199));
#45277=CARTESIAN_POINT('Ctrl Pts',(-56.2905391787879,-76.3427409187718,
20.6305435185828));
#45278=CARTESIAN_POINT('Ctrl Pts',(-56.1674316415267,-77.3051540077992,
22.1650049810762));
#45279=CARTESIAN_POINT('Ctrl Pts',(-56.0434183804932,-79.0253682692881,
22.7693699258002));
#45280=CARTESIAN_POINT('Ctrl Pts',(-55.9184902021531,-80.76041430407,22.1649257307675));
#45281=CARTESIAN_POINT('Ctrl Pts',(-55.7926139794339,-81.7471752563372,
20.5989990927192));
#45282=CARTESIAN_POINT('Ctrl Pts',(-55.665770759842,-81.5409899392144,18.7453244956607));
#45283=CARTESIAN_POINT('Ctrl Pts',(-55.5379380211753,-80.2134922663367,
17.4145335706771));
#45284=CARTESIAN_POINT('Ctrl Pts',(-55.4090994105114,-78.3317895941842,
17.199794799748));
#45285=CARTESIAN_POINT('Ctrl Pts',(-55.2792362147139,-76.7126809740671,
18.2138816022247));
#45286=CARTESIAN_POINT('Ctrl Pts',(-55.1701567495123,-76.1829937999486,
19.7264829493925));
#45287=CARTESIAN_POINT('Ctrl Pts',(-55.0823625588476,-76.3924030320099,
20.9461543340251));
#45288=CARTESIAN_POINT('Ctrl Pts',(-55.0162545425101,-76.8417463674681,
21.7616744562217));
#45289=CARTESIAN_POINT('Ctrl Pts',(-54.9498823613353,-77.539261345362,22.3841725264662));
#45290=CARTESIAN_POINT('Ctrl Pts',(-54.8610323667072,-78.6949935525488,
22.8661593057298));
#45291=CARTESIAN_POINT('Ctrl Pts',(-54.7493114127749,-80.3264380739757,
22.6862663557752));
#45292=CARTESIAN_POINT('Ctrl Pts',(-54.6141770440791,-81.7339723863005,
21.282048149325));
#45293=CARTESIAN_POINT('Ctrl Pts',(-54.4779752619141,-81.9605162195905,
19.2931923197602));
#45294=CARTESIAN_POINT('Ctrl Pts',(-54.3407073175252,-80.8893439419391,
17.5814556098495));
#45295=CARTESIAN_POINT('Ctrl Pts',(-54.2023736536333,-78.9700251318391,
16.9097214459956));
#45296=CARTESIAN_POINT('Ctrl Pts',(-54.0629841015741,-77.0348423863016,
17.5837533254939));
#45297=CARTESIAN_POINT('Ctrl Pts',(-53.9225461836219,-75.9341039807705,
19.3306551916095));
#45298=CARTESIAN_POINT('Ctrl Pts',(-53.7810707929938,-76.1644712152157,
21.397800765737));
#45299=CARTESIAN_POINT('Ctrl Pts',(-53.6385714735097,-77.6441441078143,
22.8809897524166));
#45300=CARTESIAN_POINT('Ctrl Pts',(-53.4950639676803,-79.740509330956,23.1196407622332));
#45301=CARTESIAN_POINT('Ctrl Pts',(-53.3505664751887,-81.5406299938883,
21.9913998749732));
#45302=CARTESIAN_POINT('Ctrl Pts',(-53.2050994521972,-82.2492481514294,
19.9734896793798));
#45303=CARTESIAN_POINT('Ctrl Pts',(-53.0586858006082,-81.540488114762,17.9409077358488));
#45304=CARTESIAN_POINT('Ctrl Pts',(-52.9113506491857,-79.7075778778228,
16.7865308434111));
#45305=CARTESIAN_POINT('Ctrl Pts',(-52.7631211786402,-77.5417692000642,
17.0283429800463));
#45306=CARTESIAN_POINT('Ctrl Pts',(-52.6140265379999,-75.9903067164397,
18.5767943577803));
#45307=CARTESIAN_POINT('Ctrl Pts',(-52.4640979081661,-75.7414723756217,
20.7669193990113));
#45308=CARTESIAN_POINT('Ctrl Pts',(-52.3133683735114,-76.9187653495364,
22.6442841363996));
#45309=CARTESIAN_POINT('Ctrl Pts',(-52.1618730139186,-79.0203650036271,
23.381653056446));
#45310=CARTESIAN_POINT('Ctrl Pts',(-52.0096487974204,-81.1332438312709,
22.6441978412598));
#45311=CARTESIAN_POINT('Ctrl Pts',(-51.8567346701536,-82.3306671274323,
20.7416040561834));
#45312=CARTESIAN_POINT('Ctrl Pts',(-51.703170408764,-82.0793436505482,18.4980732665105));
#45313=CARTESIAN_POINT('Ctrl Pts',(-51.548998435844,-80.4777166500322,16.8943328305896));
#45314=CARTESIAN_POINT('Ctrl Pts',(-51.3942599140222,-78.2170100179401,
16.6384668010765));
#45315=CARTESIAN_POINT('Ctrl Pts',(-51.2390031714738,-76.2840963807832,
17.8515302441033));
#45316=CARTESIAN_POINT('Ctrl Pts',(-51.0832647073186,-75.5255777659518,
20.0128901467821));
#45317=CARTESIAN_POINT('Ctrl Pts',(-50.9271121506165,-76.2852475855935,
22.1787168558586));
#45318=CARTESIAN_POINT('Ctrl Pts',(-50.77056825008,-78.2330104312193,23.4040514047276));
#45319=CARTESIAN_POINT('Ctrl Pts',(-50.6136938502426,-80.524688911548,23.1466211054636));
#45320=CARTESIAN_POINT('Ctrl Pts',(-50.4565368618462,-82.1586749532148,
21.5134827334387));
#45321=CARTESIAN_POINT('Ctrl Pts',(-50.2991475798848,-82.4180954974584,
19.2143218707712));
#45322=CARTESIAN_POINT('Ctrl Pts',(-50.1415762807599,-81.1860035174916,
17.2528324014937));
#45323=CARTESIAN_POINT('Ctrl Pts',(-49.9838738197086,-78.9975177621074,
16.486714827865));
#45324=CARTESIAN_POINT('Ctrl Pts',(-49.8260923486205,-76.8085272901581,
17.253030288183));
#45325=CARTESIAN_POINT('Ctrl Pts',(-49.6682820790183,-75.5730195227687,
19.216469125723));
#45326=CARTESIAN_POINT('Ctrl Pts',(-49.5104978361797,-75.8352207050452,
21.5232288242989));
#45327=CARTESIAN_POINT('Ctrl Pts',(-49.3527832636632,-77.4690060053744,
23.1581845435753));
#45328=CARTESIAN_POINT('Ctrl Pts',(-49.1776977284958,-80.0397589837405,
23.4552962194859));
#45329=CARTESIAN_POINT('Ctrl Pts',(-49.0203423715508,-81.9195835809123,
21.9580643192054));
#45330=CARTESIAN_POINT('Ctrl Pts',(-48.8894100336456,-82.3227846164501,
20.1263666907));
#45331=CARTESIAN_POINT('Ctrl Pts',(-48.8022107925218,-82.1188190468183,
18.9196473910859));
#45332=CARTESIAN_POINT('Ctrl Pts',(-48.6976764064176,-81.4074504860157,
17.6271971643817));
#45333=CARTESIAN_POINT('Ctrl Pts',(-48.5671956740568,-79.7862474292538,
16.6075671275254));
#45334=CARTESIAN_POINT('Ctrl Pts',(-48.4110057336366,-77.5030478338066,
16.86546764075));
#45335=CARTESIAN_POINT('Ctrl Pts',(-48.2552376689688,-75.8854225102068,
18.4854612464013));
#45336=CARTESIAN_POINT('Ctrl Pts',(-48.0999434436653,-75.6307100332678,
20.7541124518367));
#45337=CARTESIAN_POINT('Ctrl Pts',(-47.9451661206175,-76.8425294742725,
22.6799565976964));
#45338=CARTESIAN_POINT('Ctrl Pts',(-47.7909512523896,-78.9827633245282,
23.4273301176066));
#45339=CARTESIAN_POINT('Ctrl Pts',(-47.6373416660037,-81.1136922956471,
22.6800260682271));
#45340=CARTESIAN_POINT('Ctrl Pts',(-47.4843795207015,-82.3085819854583,
20.7751611932815));
#45341=CARTESIAN_POINT('Ctrl Pts',(-47.3321048269705,-82.0561553777343,
18.5508802879414));
#45342=CARTESIAN_POINT('Ctrl Pts',(-47.1805562855874,-80.4794196831413,
16.9768948333079));
#45343=CARTESIAN_POINT('Ctrl Pts',(-47.029770256272,-78.2764296948284,16.7305760045727));
#45344=CARTESIAN_POINT('Ctrl Pts',(-46.8797825692249,-76.4103691501619,
17.9055895262826));
#45345=CARTESIAN_POINT('Ctrl Pts',(-46.7306246774405,-75.6881729894422,
19.9755811261626));
#45346=CARTESIAN_POINT('Ctrl Pts',(-46.5823318642751,-76.4097535506971,
22.0334906631283));
#45347=CARTESIAN_POINT('Ctrl Pts',(-46.4594923341318,-77.9402056822882,
22.9909089774758));
#45348=CARTESIAN_POINT('Ctrl Pts',(-46.3616909254776,-79.314859900965,23.0641907370176));
#45349=CARTESIAN_POINT('Ctrl Pts',(-46.2641995052703,-80.6385976410735,
22.6872274238976));
#45350=CARTESIAN_POINT('Ctrl Pts',(-46.1590932556085,-81.7235437390656,
21.596478187795));
#45351=CARTESIAN_POINT('Ctrl Pts',(-46.014372674255,-82.1873157419008,19.5794806256373));
#45352=CARTESIAN_POINT('Ctrl Pts',(-45.9125554805191,-81.5209695292361,
18.1775553804498));
#45353=CARTESIAN_POINT('Ctrl Pts',(-45.8370809471352,-80.6693842884602,
17.5608521824556));
#45354=CARTESIAN_POINT('Ctrl Pts',(-45.7894563496702,-80.104733110141,17.2159936869747));
#45355=CARTESIAN_POINT('Ctrl Pts',(-45.7004335623306,-78.8685673337143,
16.8958075847323));
#45356=CARTESIAN_POINT('Ctrl Pts',(-45.5706717427821,-77.0663809967464,
17.5279735658841));
#45357=CARTESIAN_POINT('Ctrl Pts',(-45.430169690343,-75.9729867562349,19.2752779146581));
#45358=CARTESIAN_POINT('Ctrl Pts',(-45.2752021281552,-76.2233068312271,
21.5489130349393));
#45359=CARTESIAN_POINT('Ctrl Pts',(-45.1216158714685,-78.0661371879358,
23.0131504465605));
#45360=CARTESIAN_POINT('Ctrl Pts',(-44.9998479620023,-79.8459952382941,
22.7973970035329));
#45361=CARTESIAN_POINT('Ctrl Pts',(-44.8787164843353,-81.2825728142914,
21.9016562184237));
#45362=CARTESIAN_POINT('Ctrl Pts',(-44.7433295404188,-82.1794770296741,
20.0257518112265));
#45363=CARTESIAN_POINT('Ctrl Pts',(-44.5845594999856,-81.1142670786869,
17.8332659205346));
#45364=CARTESIAN_POINT('Ctrl Pts',(-44.4468550226416,-79.2432620245245,
17.1150869676367));
#45365=CARTESIAN_POINT('Ctrl Pts',(-44.3296591566119,-77.5872330042658,
17.4904086854693));
#45366=CARTESIAN_POINT('Ctrl Pts',(-44.2132882540016,-76.4379280034599,
18.733713586435));
#45367=CARTESIAN_POINT('Ctrl Pts',(-44.0977385940157,-76.1888336362038,
20.3922467063092));
#45368=CARTESIAN_POINT('Ctrl Pts',(-43.9829982620799,-76.9144258896296,
21.8947108508307));
#45369=CARTESIAN_POINT('Ctrl Pts',(-43.8785525781174,-78.2292942545683,
22.6506000135548));
#45370=CARTESIAN_POINT('Ctrl Pts',(-43.7841753116354,-79.5742350057765,
22.6486678392791));
#45371=CARTESIAN_POINT('Ctrl Pts',(-43.699672217088,-80.6584337764255,22.1263780555366));
#45372=CARTESIAN_POINT('Ctrl Pts',(-43.6296126732069,-81.2801642158414,
21.3455317785918));
#45373=CARTESIAN_POINT('Ctrl Pts',(-43.5737753994274,-81.5372170176451,
20.6087512726784));
#45374=CARTESIAN_POINT('Ctrl Pts',(-43.518078981982,-81.6250338077328,19.8350853592833));
#45375=CARTESIAN_POINT('Ctrl Pts',(-43.4487183634687,-81.404469536385,18.8724557081866));
#45376=CARTESIAN_POINT('Ctrl Pts',(-43.3658959085869,-80.6687217128354,
17.949784241022));
#45377=CARTESIAN_POINT('Ctrl Pts',(-43.283474596072,-79.610792793437,17.4423031492366));
#45378=CARTESIAN_POINT('Ctrl Pts',(-43.1877734173518,-78.2470216501346,
17.4407977672363));
#45379=CARTESIAN_POINT('Ctrl Pts',(-43.0790453443284,-76.8935395063061,
18.2888255232695));
#45380=CARTESIAN_POINT('Ctrl Pts',(-42.9575637604258,-76.3060155363263,
19.9777434791269));
#45381=CARTESIAN_POINT('Ctrl Pts',(-42.8368801969012,-76.8937775828933,
21.6512107701672));
#45382=CARTESIAN_POINT('Ctrl Pts',(-42.7169622778929,-78.3878970389899,
22.5882669368956));
#45383=CARTESIAN_POINT('Ctrl Pts',(-42.5977722059908,-80.1292261653996,
22.3901838052404));
#45384=CARTESIAN_POINT('Ctrl Pts',(-42.4792718279229,-81.3601746061652,
21.1570532288566));
#45385=CARTESIAN_POINT('Ctrl Pts',(-42.3614218706137,-81.5525719695301,
19.434897660521));
#45386=CARTESIAN_POINT('Ctrl Pts',(-42.2441791418002,-80.6341360625486,
17.9759923568351));
#45387=CARTESIAN_POINT('Ctrl Pts',(-42.1275051232798,-79.0140156775564,
17.4107380824392));
#45388=CARTESIAN_POINT('Ctrl Pts',(-42.0113456022818,-77.4024665017815,
17.9760297721319));
#45389=CARTESIAN_POINT('Ctrl Pts',(-41.8956771393597,-76.4973982517658,
19.41739241847));
#45390=CARTESIAN_POINT('Ctrl Pts',(-41.7804045126007,-76.6899507198097,
21.1009365038956));
#45391=CARTESIAN_POINT('Ctrl Pts',(-41.665545375653,-77.8837303342628,22.2956049805917));
#45392=CARTESIAN_POINT('Ctrl Pts',(-41.5509433179345,-79.5588532573537,
22.4820346193826));
#45393=CARTESIAN_POINT('Ctrl Pts',(-41.4558302779412,-80.7416595080358,
21.73980621753));
#45394=CARTESIAN_POINT('Ctrl Pts',(-41.3795913853863,-81.2587963541492,
20.7938974313728));
#45395=CARTESIAN_POINT('Ctrl Pts',(-41.3417721331875,-81.3480515793144,
20.2756857792622));
#45396=CARTESIAN_POINT('Ctrl Pts',(-41.322588188277,-81.3485521238293,20.0046454119954));
#45397=CARTESIAN_POINT('Ctrl Pts',(-56.5102053539837,-81.351600589951,20.0071836514217));
#45398=CARTESIAN_POINT('Ctrl Pts',(-56.4910244219711,-81.3511001238464,
19.7361858548797));
#45399=CARTESIAN_POINT('Ctrl Pts',(-56.4531917437032,-81.261737846479,19.2178972242685));
#45400=CARTESIAN_POINT('Ctrl Pts',(-56.3770585424072,-80.7451754499662,
18.2734918738261));
#45401=CARTESIAN_POINT('Ctrl Pts',(-56.2823212194466,-79.56681271122,17.5350771162317));
#45402=CARTESIAN_POINT('Ctrl Pts',(-56.168557869964,-77.9044015600755,17.7210078702458));
#45403=CARTESIAN_POINT('Ctrl Pts',(-56.054932665963,-76.7242923839595,18.9032627799536));
#45404=CARTESIAN_POINT('Ctrl Pts',(-55.9412690897771,-76.5353583257392,
20.5629616301326));
#45405=CARTESIAN_POINT('Ctrl Pts',(-55.8275659899422,-77.425346150383,21.9786754829479));
#45406=CARTESIAN_POINT('Ctrl Pts',(-55.7137625672808,-79.0039247999209,
22.5314527230236));
#45407=CARTESIAN_POINT('Ctrl Pts',(-55.5998114833368,-80.5853579566487,
21.9787611516442));
#45408=CARTESIAN_POINT('Ctrl Pts',(-55.4856598482461,-81.4785333921862,
20.5583160012619));
#45409=CARTESIAN_POINT('Ctrl Pts',(-55.3712576510193,-81.2910980626486,
18.8871689581471));
#45410=CARTESIAN_POINT('Ctrl Pts',(-55.2565556248424,-80.0992808803953,
17.6944405340721));
#45411=CARTESIAN_POINT('Ctrl Pts',(-55.141503164892,-78.4192425544493,17.5040643664775));
#45412=CARTESIAN_POINT('Ctrl Pts',(-55.026055868874,-76.9808732902402,18.4064154466049));
#45413=CARTESIAN_POINT('Ctrl Pts',(-54.9294735631935,-76.5128630966309,
19.7455891929516));
#45414=CARTESIAN_POINT('Ctrl Pts',(-54.8519729228635,-76.6978592561223,
20.8220799878041));
#45415=CARTESIAN_POINT('Ctrl Pts',(-54.7937180120044,-77.0938776199365,
21.540591026434));
#45416=CARTESIAN_POINT('Ctrl Pts',(-54.7353290651632,-77.7074901235831,
22.0880670558696));
#45417=CARTESIAN_POINT('Ctrl Pts',(-54.6572920452478,-78.7225626158952,
22.5112243584038));
#45418=CARTESIAN_POINT('Ctrl Pts',(-54.5593711005937,-80.1520967756301,
22.3529289346277));
#45419=CARTESIAN_POINT('Ctrl Pts',(-54.4412482204883,-81.3817174297985,
21.1251765148885));
#45420=CARTESIAN_POINT('Ctrl Pts',(-54.3224612626691,-81.5786773319245,
19.3908351414342));
#45421=CARTESIAN_POINT('Ctrl Pts',(-54.2029675645252,-80.6459478261372,
17.9012773774753));
#45422=CARTESIAN_POINT('Ctrl Pts',(-54.0827425677814,-78.9778893097759,
17.317885726257));
#45423=CARTESIAN_POINT('Ctrl Pts',(-53.9617333429526,-77.2981755739033,
17.9032403007292));
#45424=CARTESIAN_POINT('Ctrl Pts',(-53.8399125595789,-76.3436028630065,
19.4185080130129));
#45425=CARTESIAN_POINT('Ctrl Pts',(-53.7172473194658,-76.5433947171594,
21.2106545999253));
#45426=CARTESIAN_POINT('Ctrl Pts',(-53.5937073203965,-77.8260881060579,
22.4964442551405));
#45427=CARTESIAN_POINT('Ctrl Pts',(-53.4692641471014,-79.6438496446738,
22.7035183202107));
#45428=CARTESIAN_POINT('Ctrl Pts',(-53.3438915061289,-81.2057871862013,
21.7248460212009));
#45429=CARTESIAN_POINT('Ctrl Pts',(-53.2175652348102,-81.8214765038056,
19.9726072217714));
#45430=CARTESIAN_POINT('Ctrl Pts',(-53.0902632570463,-81.2056586657804,
18.2052063703588));
#45431=CARTESIAN_POINT('Ctrl Pts',(-52.9619658262281,-79.6098641790913,
17.1995187197679));
#45432=CARTESIAN_POINT('Ctrl Pts',(-52.8326556330999,-77.7203742313896,
17.4098298281602));
#45433=CARTESIAN_POINT('Ctrl Pts',(-52.7023177766159,-76.3635187904908,
18.7630035707443));
#45434=CARTESIAN_POINT('Ctrl Pts',(-52.570939721051,-76.1446314012751,20.6821481924982));
#45435=CARTESIAN_POINT('Ctrl Pts',(-52.4385113642502,-77.1782614510524,
22.3321665597262));
#45436=CARTESIAN_POINT('Ctrl Pts',(-52.3050249835528,-79.0298407796912,
22.9828907354959));
#45437=CARTESIAN_POINT('Ctrl Pts',(-52.1704753824066,-80.8979297239154,
22.3320439848364));
#45438=CARTESIAN_POINT('Ctrl Pts',(-52.0348597424323,-81.9610122222982,
20.6451414911034));
#45439=CARTESIAN_POINT('Ctrl Pts',(-51.8981780948215,-81.7385564317577,
18.6478788175736));
#45440=CARTESIAN_POINT('Ctrl Pts',(-51.7604321945898,-80.3083549963098,
17.2138695348548));
#45441=CARTESIAN_POINT('Ctrl Pts',(-51.6216279436362,-78.2802930883723,
16.9828845462497));
#45442=CARTESIAN_POINT('Ctrl Pts',(-51.4817699615281,-76.5380718994072,
18.0745070683019));
#45443=CARTESIAN_POINT('Ctrl Pts',(-51.3408736679231,-75.8501788412933,
20.0297405359875));
#45444=CARTESIAN_POINT('Ctrl Pts',(-51.1989382729077,-76.5392195094218,
21.9991175294759));
#45445=CARTESIAN_POINT('Ctrl Pts',(-51.0559946652494,-78.3171890144164,
23.1196650869329));
#45446=CARTESIAN_POINT('Ctrl Pts',(-50.9120515053575,-80.4205653742962,
22.8851695343114));
#45447=CARTESIAN_POINT('Ctrl Pts',(-50.7671291242161,-81.9289478457697,
21.380149508053));
#45448=CARTESIAN_POINT('Ctrl Pts',(-50.6212487099078,-82.1713186731815,
19.248852229337));
#45449=CARTESIAN_POINT('Ctrl Pts',(-50.474433980975,-81.0247130386606,17.4198125584412));
#45450=CARTESIAN_POINT('Ctrl Pts',(-50.3267111772793,-78.9748712348568,
16.7000982510701));
#45451=CARTESIAN_POINT('Ctrl Pts',(-50.1781079176229,-76.9120299405903,
17.420093293127));
#45452=CARTESIAN_POINT('Ctrl Pts',(-50.0286560537834,-75.7398510408867,
19.2788548996711));
#45453=CARTESIAN_POINT('Ctrl Pts',(-49.8783844328933,-75.9874937562904,
21.476647216806));
#45454=CARTESIAN_POINT('Ctrl Pts',(-49.7273345651342,-77.5512046364284,
23.0443219045335));
#45455=CARTESIAN_POINT('Ctrl Pts',(-49.5586585240247,-80.0279089996088,
23.3334401353208));
#45456=CARTESIAN_POINT('Ctrl Pts',(-49.4060082642688,-81.8538210133292,
21.8837856461858));
#45457=CARTESIAN_POINT('Ctrl Pts',(-49.2782581021314,-82.2484807046217,
20.0963040292974));
#45458=CARTESIAN_POINT('Ctrl Pts',(-49.1928885669734,-82.0489182365846,
18.914665854516));
#45459=CARTESIAN_POINT('Ctrl Pts',(-49.0902384690458,-81.3507219395805,
17.6452269478581));
#45460=CARTESIAN_POINT('Ctrl Pts',(-48.9615765066383,-79.7525096231734,
16.6379188946829));
#45461=CARTESIAN_POINT('Ctrl Pts',(-48.8066280268286,-77.4866354369491,
16.8915282252642));
#45462=CARTESIAN_POINT('Ctrl Pts',(-48.6511833135857,-75.870236297486,18.5070672541726));
#45463=CARTESIAN_POINT('Ctrl Pts',(-48.4952829185379,-75.6121761854611,
20.7849669355286));
#45464=CARTESIAN_POINT('Ctrl Pts',(-48.3389764832945,-76.8343636892977,
22.731649389924));
#45465=CARTESIAN_POINT('Ctrl Pts',(-48.1823111553132,-79.0084616600531,
23.4933056118749));
#45466=CARTESIAN_POINT('Ctrl Pts',(-48.0253367390954,-81.1874456640624,
22.7316029756924));
#45467=CARTESIAN_POINT('Ctrl Pts',(-47.8681030052212,-82.4179904745334,
20.7742238673546));
#45468=CARTESIAN_POINT('Ctrl Pts',(-47.7106605343791,-82.1591871711449,
18.4735616689089));
#45469=CARTESIAN_POINT('Ctrl Pts',(-47.5530598605685,-80.5206179988346,
16.8346671108224));
#45470=CARTESIAN_POINT('Ctrl Pts',(-47.3953525426489,-78.2160956239723,
16.5747442943651));
#45471=CARTESIAN_POINT('Ctrl Pts',(-47.2375889524593,-76.2515474551307,
17.8091507733092));
#45472=CARTESIAN_POINT('Ctrl Pts',(-47.0798232077956,-75.48537779457,19.9985379877705));
#45473=CARTESIAN_POINT('Ctrl Pts',(-46.9221018381816,-76.250966995779,22.1885862850942));
#45474=CARTESIAN_POINT('Ctrl Pts',(-46.7907582490246,-77.887069828226,23.2141549060391));
#45475=CARTESIAN_POINT('Ctrl Pts',(-46.6857437519368,-79.3633599628629,
23.2931678430071));
#45476=CARTESIAN_POINT('Ctrl Pts',(-46.5807886964194,-80.7886728129746,
22.8877056847724));
#45477=CARTESIAN_POINT('Ctrl Pts',(-46.467199813299,-81.9623024203698,21.7095989845971));
#45478=CARTESIAN_POINT('Ctrl Pts',(-46.3101244066264,-82.4667648192415,
19.5204885422792));
#45479=CARTESIAN_POINT('Ctrl Pts',(-46.1990680734046,-81.7418829913271,
17.9904302358176));
#45480=CARTESIAN_POINT('Ctrl Pts',(-46.1164515816408,-80.8095926681598,
17.3151909175046));
#45481=CARTESIAN_POINT('Ctrl Pts',(-46.0642853611533,-80.1910909998415,
16.9374483432803));
#45482=CARTESIAN_POINT('Ctrl Pts',(-45.9665775630929,-78.8344213924405,
16.5853757174044));
#45483=CARTESIAN_POINT('Ctrl Pts',(-45.8236196285692,-76.8476963089672,
17.2805323474208));
#45484=CARTESIAN_POINT('Ctrl Pts',(-45.668075484254,-75.6358728708552,19.2140995275267));
#45485=CARTESIAN_POINT('Ctrl Pts',(-45.4958299283901,-75.9121578661318,
21.7421177773414));
#45486=CARTESIAN_POINT('Ctrl Pts',(-45.3242577516971,-77.9692102287361,
23.38035508761));
#45487=CARTESIAN_POINT('Ctrl Pts',(-45.1876221856116,-79.9670552350402,
23.139500775403));
#45488=CARTESIAN_POINT('Ctrl Pts',(-45.0513558128287,-81.5832325086694,
22.1319648181091));
#45489=CARTESIAN_POINT('Ctrl Pts',(-44.8986075069025,-82.5974332632258,
20.0161637774792));
#45490=CARTESIAN_POINT('Ctrl Pts',(-44.7186795070239,-81.3925086591267,
17.5302291648947));
#45491=CARTESIAN_POINT('Ctrl Pts',(-44.5621230479846,-79.2651609763857,
16.712655372227));
#45492=CARTESIAN_POINT('Ctrl Pts',(-44.4285417889314,-77.3774483800612,
17.139881442109));
#45493=CARTESIAN_POINT('Ctrl Pts',(-44.2956173863613,-76.0640042276617,
18.5597990145458));
#45494=CARTESIAN_POINT('Ctrl Pts',(-44.1633484646108,-75.7783293923941,
20.4582768445098));
#45495=CARTESIAN_POINT('Ctrl Pts',(-44.031779218605,-76.6099851009247,22.1814794461785));
#45496=CARTESIAN_POINT('Ctrl Pts',(-43.91182076343,-78.1200466389143,23.0500041168154));
#45497=CARTESIAN_POINT('Ctrl Pts',(-43.8032972503512,-79.6666485186877,
23.0479392254152));
#45498=CARTESIAN_POINT('Ctrl Pts',(-43.7060427882043,-80.9145301144203,
22.4469274515336));
#45499=CARTESIAN_POINT('Ctrl Pts',(-43.6253519025163,-81.6306856242157,
21.5476182586661));
#45500=CARTESIAN_POINT('Ctrl Pts',(-43.5610123031743,-81.9268920837325,
20.6986435448477));
#45501=CARTESIAN_POINT('Ctrl Pts',(-43.4968178170664,-82.0281189549035,
19.806937944391));
#45502=CARTESIAN_POINT('Ctrl Pts',(-43.4168479041046,-81.7738600390164,
18.6970519690361));
#45503=CARTESIAN_POINT('Ctrl Pts',(-43.3213263793924,-80.9253416906861,
17.6329077834861));
#45504=CARTESIAN_POINT('Ctrl Pts',(-43.2262532956317,-79.7050475580838,
17.0475327158774));
#45505=CARTESIAN_POINT('Ctrl Pts',(-43.1158616470016,-78.1319653479767,
17.0458078617628));
#45506=CARTESIAN_POINT('Ctrl Pts',(-42.9904623873872,-76.5711141945366,
18.0239064285819));
#45507=CARTESIAN_POINT('Ctrl Pts',(-42.8504284292441,-75.8942100281233,
19.9706479680719));
#45508=CARTESIAN_POINT('Ctrl Pts',(-42.7114451655225,-76.5714158474922,
21.8975344967549));
#45509=CARTESIAN_POINT('Ctrl Pts',(-42.5735200918022,-78.2899803626415,
22.9747252284951));
#45510=CARTESIAN_POINT('Ctrl Pts',(-42.4366584097288,-80.2891630255458,
22.7466550039197));
#45511=CARTESIAN_POINT('Ctrl Pts',(-42.300862738502,-81.6990410530149,21.3332139952526));
#45512=CARTESIAN_POINT('Ctrl Pts',(-42.1661332961441,-81.9181163628249,
19.3646257221592));
#45513=CARTESIAN_POINT('Ctrl Pts',(-42.0324677389737,-80.8704178528976,
17.7021871370045));
#45514=CARTESIAN_POINT('Ctrl Pts',(-41.8998614427592,-79.0291889851441,
17.060906941546));
#45515=CARTESIAN_POINT('Ctrl Pts',(-41.768306817613,-77.204873422229,17.7021299380875));
#45516=CARTESIAN_POINT('Ctrl Pts',(-41.6377947505436,-76.1852713423579,
19.3284903687226));
#45517=CARTESIAN_POINT('Ctrl Pts',(-41.5083116255931,-76.4029798468466,
21.2192502585522));
#45518=CARTESIAN_POINT('Ctrl Pts',(-41.3798598292886,-77.7388493644985,
22.5535329081885));
#45519=CARTESIAN_POINT('Ctrl Pts',(-41.252378015881,-79.6025795576068,22.7597660265109));
#45520=CARTESIAN_POINT('Ctrl Pts',(-41.1470144444954,-80.9111847600037,
21.93603750269));
#45521=CARTESIAN_POINT('Ctrl Pts',(-41.0631067409177,-81.4804422184361,
20.8951581990914));
#45522=CARTESIAN_POINT('Ctrl Pts',(-41.0214391827265,-81.5786120505805,
20.3242243526537));
#45523=CARTESIAN_POINT('Ctrl Pts',(-41.0004636061353,-81.5791593420714,
20.0278709170366));
#45524=CARTESIAN_POINT('Ctrl Pts',(-56.1931710509147,-81.5904762192943,
20.0291818533745));
#45525=CARTESIAN_POINT('Ctrl Pts',(-56.1721965566912,-81.5899289558238,
19.7328437132649));
#45526=CARTESIAN_POINT('Ctrl Pts',(-56.1304803139095,-81.4914160150344,
19.1612770147036));
#45527=CARTESIAN_POINT('Ctrl Pts',(-56.047109678892,-80.9249724047485,18.1271447389076));
#45528=CARTESIAN_POINT('Ctrl Pts',(-55.9436715369273,-79.6379237377103,
17.3216367798175));
#45529=CARTESIAN_POINT('Ctrl Pts',(-55.8203317637762,-77.8351613950806,
17.5256562815028));
#45530=CARTESIAN_POINT('Ctrl Pts',(-55.69790582868,-76.5650422099848,18.8008040261662));
#45531=CARTESIAN_POINT('Ctrl Pts',(-55.5762992644413,-76.3649861666019,
20.5773747368897));
#45532=CARTESIAN_POINT('Ctrl Pts',(-55.4555213165667,-77.312671536182,22.0805289509775));
#45533=CARTESIAN_POINT('Ctrl Pts',(-55.3355023408405,-78.9788215337353,
22.661615143053));
#45534=CARTESIAN_POINT('Ctrl Pts',(-55.2162218985695,-80.6341462766125,
22.0806902291229));
#45535=CARTESIAN_POINT('Ctrl Pts',(-55.0976344395572,-81.5604707585099,
20.6032956261243));
#45536=CARTESIAN_POINT('Ctrl Pts',(-54.9797037858124,-81.3649349503641,
18.8802080061892));
#45537=CARTESIAN_POINT('Ctrl Pts',(-54.8623863490237,-80.1439213865375,
17.6614773952729));
#45538=CARTESIAN_POINT('Ctrl Pts',(-54.7456423816505,-78.438301885998,17.4704950427283));
#45539=CARTESIAN_POINT('Ctrl Pts',(-54.6294225574966,-76.9911289094193,
18.381155317716));
#45540=CARTESIAN_POINT('Ctrl Pts',(-54.5329814401706,-76.5254042740319,
19.719510916299));
#45541=CARTESIAN_POINT('Ctrl Pts',(-54.4560325840395,-76.709489835983,20.788354755425));
#45542=CARTESIAN_POINT('Ctrl Pts',(-54.3984251024622,-77.1014268283988,
21.4989031483612));
#45543=CARTESIAN_POINT('Ctrl Pts',(-54.3409144108848,-77.7060790817609,
22.0380321813387));
#45544=CARTESIAN_POINT('Ctrl Pts',(-54.2643529957864,-78.7023284793725,
22.4529267891116));
#45545=CARTESIAN_POINT('Ctrl Pts',(-54.1688795115049,-80.0965435535358,
22.2967139321817));
#45546=CARTESIAN_POINT('Ctrl Pts',(-54.0545941116151,-81.2849959119691,
21.1068835663603));
#45547=CARTESIAN_POINT('Ctrl Pts',(-53.9405474572273,-81.4719923932769,
19.441012695379));
#45548=CARTESIAN_POINT('Ctrl Pts',(-53.8266972060701,-80.5811209890118,
18.0223892278746));
#45549=CARTESIAN_POINT('Ctrl Pts',(-53.7129653055039,-79.0022844568973,
17.472401568245));
#45550=CARTESIAN_POINT('Ctrl Pts',(-53.599334468734,-77.4251558030463,18.0241320621135));
#45551=CARTESIAN_POINT('Ctrl Pts',(-53.4857367540597,-76.5364154437238,
19.4385659324685));
#45552=CARTESIAN_POINT('Ctrl Pts',(-53.3721220169306,-76.7233926686843,
21.0987319736096));
#45553=CARTESIAN_POINT('Ctrl Pts',(-53.2584384574455,-77.9053472090669,
22.2809672747817));
#45554=CARTESIAN_POINT('Ctrl Pts',(-53.1446349951865,-79.568314662251,22.4686541503725));
#45555=CARTESIAN_POINT('Ctrl Pts',(-53.030660482889,-80.9877176287472,21.577332089441));
#45556=CARTESIAN_POINT('Ctrl Pts',(-52.9164642736675,-81.5429354152238,
19.9924518303138));
#45557=CARTESIAN_POINT('Ctrl Pts',(-52.8019958227748,-80.9876773944488,
18.4033565400404));
#45558=CARTESIAN_POINT('Ctrl Pts',(-52.6872052811913,-79.5588434690807,
17.5045277438755));
#45559=CARTESIAN_POINT('Ctrl Pts',(-52.5720437782595,-77.8759033624557,
17.6931479297474));
#45560=CARTESIAN_POINT('Ctrl Pts',(-52.456463479153,-76.6732981208235,18.8941780160138));
#45561=CARTESIAN_POINT('Ctrl Pts',(-52.3404174742245,-76.4810117294207,
20.5897747255326));
#45562=CARTESIAN_POINT('Ctrl Pts',(-52.2238599700478,-77.3917589649615,
22.0417537639404));
#45563=CARTESIAN_POINT('Ctrl Pts',(-52.1067461880084,-79.0167757404078,
22.6119079176574));
#45564=CARTESIAN_POINT('Ctrl Pts',(-51.9890325238844,-80.6510816764256,
22.0416788272352));
#45565=CARTESIAN_POINT('Ctrl Pts',(-51.8706765682083,-81.5784074709173,
20.5689210739554));
#45566=CARTESIAN_POINT('Ctrl Pts',(-51.7516381842611,-81.3840761178566,
18.8293385290052));
#45567=CARTESIAN_POINT('Ctrl Pts',(-51.6318777612795,-80.1401644139924,
17.5827772497869));
#45568=CARTESIAN_POINT('Ctrl Pts',(-51.5113598466867,-78.3790893485887,
17.3825631025712));
#45569=CARTESIAN_POINT('Ctrl Pts',(-51.3900453226883,-76.8679002321331,
18.3297321532828));
#45570=CARTESIAN_POINT('Ctrl Pts',(-51.2679089636746,-76.2716995874448,
20.0248007634938));
#45571=CARTESIAN_POINT('Ctrl Pts',(-51.1448999383953,-76.8689071318202,
21.731599205865));
#45572=CARTESIAN_POINT('Ctrl Pts',(-51.021010641651,-78.4098824882715,22.7028590477005));
#45573=CARTESIAN_POINT('Ctrl Pts',(-50.8962035466111,-80.2336798734102,
22.4997020368517));
#45574=CARTESIAN_POINT('Ctrl Pts',(-50.7704540538976,-81.5427020047577,
21.1939832796085));
#45575=CARTESIAN_POINT('Ctrl Pts',(-50.6437387988144,-81.753601597011,19.3427496141414));
#45576=CARTESIAN_POINT('Ctrl Pts',(-50.5160369129462,-80.7566939083138,
17.7516096622113));
#45577=CARTESIAN_POINT('Ctrl Pts',(-50.3873296992986,-78.9709799251651,
17.1240176730073));
#45578=CARTESIAN_POINT('Ctrl Pts',(-50.2576005805652,-77.1700135782155,
17.75191180977));
#45579=CARTESIAN_POINT('Ctrl Pts',(-50.1268359834938,-76.1438312789394,
19.3777143443819));
#45580=CARTESIAN_POINT('Ctrl Pts',(-49.9950235011709,-76.3601822381745,
21.3055450852728));
#45581=CARTESIAN_POINT('Ctrl Pts',(-49.8621562390858,-77.7348938688194,
22.6849411190031));
#45582=CARTESIAN_POINT('Ctrl Pts',(-49.7133415381469,-79.9195947555483,
22.9413584111036));
#45583=CARTESIAN_POINT('Ctrl Pts',(-49.5781602668827,-81.5376672860394,
21.6590948623266));
#45584=CARTESIAN_POINT('Ctrl Pts',(-49.4646197181616,-81.8890632572599,
20.0705481237758));
#45585=CARTESIAN_POINT('Ctrl Pts',(-49.3885799052481,-81.7114130509256,
19.0181107772552));
#45586=CARTESIAN_POINT('Ctrl Pts',(-49.2969766628829,-81.0886388482757,
17.8852892572052));
#45587=CARTESIAN_POINT('Ctrl Pts',(-49.181806776448,-79.6588985177388,16.9828625133814));
#45588=CARTESIAN_POINT('Ctrl Pts',(-49.0425442242264,-77.6225755834458,
17.2092920570815));
#45589=CARTESIAN_POINT('Ctrl Pts',(-48.9022309275819,-76.1626933241173,
18.6662194328442));
#45590=CARTESIAN_POINT('Ctrl Pts',(-48.7608776813598,-75.9271678115608,
20.7310072076683));
#45591=CARTESIAN_POINT('Ctrl Pts',(-48.6184974980409,-77.038831411295,22.5047935543629));
#45592=CARTESIAN_POINT('Ctrl Pts',(-48.4751059278121,-79.0277630066599,
23.2034124271523));
#45593=CARTESIAN_POINT('Ctrl Pts',(-48.3307209130028,-81.0321747592271,
22.5046334535624));
#45594=CARTESIAN_POINT('Ctrl Pts',(-48.1853628100416,-82.1711101595149,
20.6964577220007));
#45595=CARTESIAN_POINT('Ctrl Pts',(-48.0390540416698,-81.9325628945093,
18.5587419776551));
#45596=CARTESIAN_POINT('Ctrl Pts',(-47.8918194155008,-80.4035068057025,
17.0266017125607));
#45597=CARTESIAN_POINT('Ctrl Pts',(-47.7436853224969,-78.2396309977359,
16.7805121138364));
#45598=CARTESIAN_POINT('Ctrl Pts',(-47.5946813664555,-76.3835179295052,
17.9443525134594));
#45599=CARTESIAN_POINT('Ctrl Pts',(-47.4448367983989,-75.6540675159799,
20.02254637128));
#45600=CARTESIAN_POINT('Ctrl Pts',(-47.2941883295031,-76.3830994404273,
22.114567621428));
#45601=CARTESIAN_POINT('Ctrl Pts',(-47.1679999676535,-77.9535609675346,
23.1010714787732));
#45602=CARTESIAN_POINT('Ctrl Pts',(-47.0666921451397,-79.3776145525847,
23.1776099822803));
#45603=CARTESIAN_POINT('Ctrl Pts',(-46.9651456325947,-80.7564776023867,
22.7858153407833));
#45604=CARTESIAN_POINT('Ctrl Pts',(-46.8547566881906,-81.8978095452959,
21.6420721310674));
#45605=CARTESIAN_POINT('Ctrl Pts',(-46.7013715271651,-82.3915913662202,
19.5050054644041));
#45606=CARTESIAN_POINT('Ctrl Pts',(-46.5922746342819,-81.6820066722275,
18.0013720242213));
#45607=CARTESIAN_POINT('Ctrl Pts',(-46.5107702934997,-80.762347045538,17.3351375612649));
#45608=CARTESIAN_POINT('Ctrl Pts',(-46.4592725150514,-80.1518069976578,
16.962269556289));
#45609=CARTESIAN_POINT('Ctrl Pts',(-46.362556488097,-78.8093578228561,16.6130383905039));
#45610=CARTESIAN_POINT('Ctrl Pts',(-46.220252885875,-76.8319457334074,17.3026718943654));
#45611=CARTESIAN_POINT('Ctrl Pts',(-46.0645726816584,-75.6173234870341,
19.2366771428804));
#45612=CARTESIAN_POINT('Ctrl Pts',(-45.8910714666791,-75.8925338508242,
21.7821315892937));
#45613=CARTESIAN_POINT('Ctrl Pts',(-45.7170955988033,-77.9753043773735,
23.4465775524674));
#45614=CARTESIAN_POINT('Ctrl Pts',(-45.5775759501255,-80.0153755859992,
23.2028167937863));
#45615=CARTESIAN_POINT('Ctrl Pts',(-45.4379062168885,-81.6717237264668,
22.1705201271916));
#45616=CARTESIAN_POINT('Ctrl Pts',(-45.2805526561883,-82.7200865632941,
19.9931079900749));
#45617=CARTESIAN_POINT('Ctrl Pts',(-45.0937704500736,-81.4738598243379,
17.4107654017481));
#45618=CARTESIAN_POINT('Ctrl Pts',(-44.9301776981165,-79.2519774158652,
16.5546323280892));
#45619=CARTESIAN_POINT('Ctrl Pts',(-44.7899176784637,-77.2699004358815,
17.0018364132725));
#45620=CARTESIAN_POINT('Ctrl Pts',(-44.6496109849249,-75.8827842307996,
18.4989471414362));
#45621=CARTESIAN_POINT('Ctrl Pts',(-44.5093442071425,-75.5784269695796,
20.5118097310074));
#45622=CARTESIAN_POINT('Ctrl Pts',(-44.3691027049655,-76.4632134679003,
22.3486394697955));
#45623=CARTESIAN_POINT('Ctrl Pts',(-44.2406353839749,-78.0793884615202,
23.2797044070866));
#45624=CARTESIAN_POINT('Ctrl Pts',(-44.1239394431124,-79.7421639402498,
23.2781543264229));
#45625=CARTESIAN_POINT('Ctrl Pts',(-44.0189993614293,-81.0886776635895,
22.6302737684353));
#45626=CARTESIAN_POINT('Ctrl Pts',(-43.9316263801741,-81.8643428824872,
21.6570022286492));
#45627=CARTESIAN_POINT('Ctrl Pts',(-43.8617948533705,-82.1859028857951,
20.7356337027876));
#45628=CARTESIAN_POINT('Ctrl Pts',(-43.7920004881958,-82.2960384222753,
19.7662775164889));
#45629=CARTESIAN_POINT('Ctrl Pts',(-43.7048391513216,-82.0193817005433,
18.5565903493298));
#45630=CARTESIAN_POINT('Ctrl Pts',(-43.6003869534277,-81.0920630654462,
17.3927421594966));
#45631=CARTESIAN_POINT('Ctrl Pts',(-43.4960916257064,-79.7537507355311,
16.7501788420722));
#45632=CARTESIAN_POINT('Ctrl Pts',(-43.3746208877838,-78.0229433571945,
16.7476551770101));
#45633=CARTESIAN_POINT('Ctrl Pts',(-43.2360946688018,-76.2982193406305,
17.8266391512518));
#45634=CARTESIAN_POINT('Ctrl Pts',(-43.0807103498632,-75.5455686337531,
19.9858138830528));
#45635=CARTESIAN_POINT('Ctrl Pts',(-42.9258436987913,-76.2985455065884,
22.1331261217648));
#45636=CARTESIAN_POINT('Ctrl Pts',(-42.77153307093,-78.2201494104768,23.3393944253305));
#45637=CARTESIAN_POINT('Ctrl Pts',(-42.6178242859543,-80.4652865043261,
23.0847085443991));
#45638=CARTESIAN_POINT('Ctrl Pts',(-42.4647580213375,-82.0552277538098,
21.4926381936908));
#45639=CARTESIAN_POINT('Ctrl Pts',(-42.3123743467156,-82.3042292356101,
19.2664619793303));
#45640=CARTESIAN_POINT('Ctrl Pts',(-42.1607129706379,-81.1165722086679,
17.3797443302913));
#45641=CARTESIAN_POINT('Ctrl Pts',(-42.0098077521494,-79.0218319254807,
16.6489801585146));
#45642=CARTESIAN_POINT('Ctrl Pts',(-41.8597011624017,-76.9400588245036,
17.3796589230168));
#45643=CARTESIAN_POINT('Ctrl Pts',(-41.710410410155,-75.7731819376884,19.2391358645968));
#45644=CARTESIAN_POINT('Ctrl Pts',(-41.5620024200472,-76.021931806847,21.4065209298965));
#45645=CARTESIAN_POINT('Ctrl Pts',(-41.41446762267,-77.5555540696917,22.938792418932));
#45646=CARTESIAN_POINT('Ctrl Pts',(-41.267888073828,-79.69889898891,23.1771584642698));
#45647=CARTESIAN_POINT('Ctrl Pts',(-41.1464403049599,-81.2063623988802,
22.2273394788785));
#45648=CARTESIAN_POINT('Ctrl Pts',(-41.049904311213,-81.8619881545566,21.0300427262042));
#45649=CARTESIAN_POINT('Ctrl Pts',(-41.0016934823989,-81.975435692595,20.3694323176616));
#45650=CARTESIAN_POINT('Ctrl Pts',(-40.977684131746,-81.9760621408481,20.030216204962));
#45651=CARTESIAN_POINT('Ctrl Pts',(-56.1840163481737,-81.9875883200479,
20.0290964452435));
#45652=CARTESIAN_POINT('Ctrl Pts',(-56.1600105776776,-81.9869619649552,
19.6899309185389));
#45653=CARTESIAN_POINT('Ctrl Pts',(-56.1117529637962,-81.8731652833032,
19.0287333656979));
#45654=CARTESIAN_POINT('Ctrl Pts',(-56.0157840520367,-81.2205270484806,
17.8385771112663));
#45655=CARTESIAN_POINT('Ctrl Pts',(-55.896346951956,-79.7356206089475,16.9078031975861));
#45656=CARTESIAN_POINT('Ctrl Pts',(-55.7540857207524,-77.6558823397947,
17.1438436556406));
#45657=CARTESIAN_POINT('Ctrl Pts',(-55.6128283938031,-76.1907775976361,
18.6144681707804));
#45658=CARTESIAN_POINT('Ctrl Pts',(-55.4726208861106,-75.9604020090565,
20.6628992338605));
#45659=CARTESIAN_POINT('Ctrl Pts',(-55.3334578707361,-77.0523722890483,
22.3940848262856));
#45660=CARTESIAN_POINT('Ctrl Pts',(-55.1953542744678,-78.9694706157036,
23.0621619556173));
#45661=CARTESIAN_POINT('Ctrl Pts',(-55.0583124323056,-80.8706958719993,
22.3942275308775));
#45662=CARTESIAN_POINT('Ctrl Pts',(-54.9223368518524,-81.9320218793108,
20.7000997936462));
#45663=CARTESIAN_POINT('Ctrl Pts',(-54.7874272612403,-81.7075151506292,
18.7294034487537));
#45664=CARTESIAN_POINT('Ctrl Pts',(-54.6535823409156,-80.3140723860071,
17.3399419744697));
#45665=CARTESIAN_POINT('Ctrl Pts',(-54.5207967868566,-78.374400120103,17.1238400380949));
#45666=CARTESIAN_POINT('Ctrl Pts',(-54.3890655740886,-76.7350629052144,
18.1568592070291));
#45667=CARTESIAN_POINT('Ctrl Pts',(-54.2801569414996,-76.2103002516481,
19.668090987021));
#45668=CARTESIAN_POINT('Ctrl Pts',(-54.1935510059906,-76.4176946207056,
20.8708526855492));
#45669=CARTESIAN_POINT('Ctrl Pts',(-54.128852397298,-76.857964212694,21.6686798646502));
#45670=CARTESIAN_POINT('Ctrl Pts',(-54.0644082411501,-77.5355178162316,
22.2725716773656));
#45671=CARTESIAN_POINT('Ctrl Pts',(-53.9788200417259,-78.6492334202541,
22.7361008606065));
#45672=CARTESIAN_POINT('Ctrl Pts',(-53.8724521289787,-80.2018795945108,
22.5608064996248));
#45673=CARTESIAN_POINT('Ctrl Pts',(-53.7457963218449,-81.5173535677004,
21.2413375034754));
#45674=CARTESIAN_POINT('Ctrl Pts',(-53.6201029336044,-81.721643630464,19.4056787875082));
#45675=CARTESIAN_POINT('Ctrl Pts',(-53.4953423172526,-80.7441720245738,
17.8527194339666));
#45676=CARTESIAN_POINT('Ctrl Pts',(-53.3715075050393,-79.024792546053,17.2558018189766));
#45677=CARTESIAN_POINT('Ctrl Pts',(-53.2485467601093,-77.3194469011662,
17.8545268954824));
#45678=CARTESIAN_POINT('Ctrl Pts',(-53.1264418459081,-76.3662466418217,
19.3754622160036));
#45679=CARTESIAN_POINT('Ctrl Pts',(-53.005159492876,-76.5678911164086,21.1467949273089));
#45680=CARTESIAN_POINT('Ctrl Pts',(-52.8846665013463,-77.8217327869644,
22.3978467499115));
#45681=CARTESIAN_POINT('Ctrl Pts',(-52.7649271902849,-79.5710431464096,
22.5930405834681));
#45682=CARTESIAN_POINT('Ctrl Pts',(-52.6459043559135,-81.0515632714903,
21.6606738718825));
#45683=CARTESIAN_POINT('Ctrl Pts',(-52.527559012935,-81.6245808941478,20.0180744750991));
#45684=CARTESIAN_POINT('Ctrl Pts',(-52.4098503630411,-81.0516487109053,
18.3853810869962));
#45685=CARTESIAN_POINT('Ctrl Pts',(-52.2927360961711,-79.59321937671,17.4706707303658));
#45686=CARTESIAN_POINT('Ctrl Pts',(-52.1761727220418,-77.8907123681399,
17.6638192609241));
#45687=CARTESIAN_POINT('Ctrl Pts',(-52.0601156179322,-76.6852554675414,
18.870974293838));
#45688=CARTESIAN_POINT('Ctrl Pts',(-51.9445189762202,-76.4960826665638,
20.5596055972846));
#45689=CARTESIAN_POINT('Ctrl Pts',(-51.8293359020739,-77.3976800945512,
21.99268490099));
#45690=CARTESIAN_POINT('Ctrl Pts',(-51.7145184824162,-78.9909626260138,
22.5493032765671));
#45691=CARTESIAN_POINT('Ctrl Pts',(-51.6000175219678,-80.5793083717327,
21.9927446344126));
#45692=CARTESIAN_POINT('Ctrl Pts',(-51.4857834151221,-81.4721331834413,
20.5706570604428));
#45693=CARTESIAN_POINT('Ctrl Pts',(-51.3717654497242,-81.2839320663009,
18.9053328706095));
#45694=CARTESIAN_POINT('Ctrl Pts',(-51.2579142567362,-80.1003468389221,
17.7222119598947));
#45695=CARTESIAN_POINT('Ctrl Pts',(-51.1441760738262,-78.4387785300752,
17.5353834584123));
#45696=CARTESIAN_POINT('Ctrl Pts',(-51.0305059559029,-77.0243269868296,
18.4242496721567));
#45697=CARTESIAN_POINT('Ctrl Pts',(-50.9168383295718,-76.4715635155443,
20.0017362886162));
#45698=CARTESIAN_POINT('Ctrl Pts',(-50.8031528501867,-77.0251058898071,
21.5782322028432));
#45699=CARTESIAN_POINT('Ctrl Pts',(-50.6893600620005,-78.4409437964808,
22.4685167016839));
#45700=CARTESIAN_POINT('Ctrl Pts',(-50.5754265208159,-80.1051012370473,
22.281444116521));
#45701=CARTESIAN_POINT('Ctrl Pts',(-50.4612995336001,-81.2916130994061,
21.0956690984439));
#45702=CARTESIAN_POINT('Ctrl Pts',(-50.3469292478256,-81.4804026348622,
19.4251616901667));
#45703=CARTESIAN_POINT('Ctrl Pts',(-50.2322658318771,-80.5843542802,17.9976877444011));
#45704=CARTESIAN_POINT('Ctrl Pts',(-50.1172596710639,-78.9887878135073,
17.4383486295407));
#45705=CARTESIAN_POINT('Ctrl Pts',(-50.0018627971402,-77.3876668209355,
17.9978807978644));
#45706=CARTESIAN_POINT('Ctrl Pts',(-49.8860256103752,-76.4798823834744,
19.4383054994183));
#45707=CARTESIAN_POINT('Ctrl Pts',(-49.7697055460028,-76.6717902993605,
21.1389672456695));
#45708=CARTESIAN_POINT('Ctrl Pts',(-49.6528483461859,-77.8811686925252,
22.3512019911516));
#45709=CARTESIAN_POINT('Ctrl Pts',(-49.5223825436566,-79.7962746252137,
22.5748992760119));
#45710=CARTESIAN_POINT('Ctrl Pts',(-49.4042570362098,-81.2094493464976,
21.4535078840428));
#45711=CARTESIAN_POINT('Ctrl Pts',(-49.3052520376841,-81.5155121502254,
20.0685103690615));
#45712=CARTESIAN_POINT('Ctrl Pts',(-49.2390213385448,-81.3607622132748,
19.1519212626098));
#45713=CARTESIAN_POINT('Ctrl Pts',(-49.1593082369371,-80.8187609382315,
18.1662414366685));
#45714=CARTESIAN_POINT('Ctrl Pts',(-49.0591919240773,-79.5759523510137,
17.3821693816316));
#45715=CARTESIAN_POINT('Ctrl Pts',(-48.9382874011232,-77.8082989807897,
17.5790252757248));
#45716=CARTESIAN_POINT('Ctrl Pts',(-48.8165729896642,-76.5422165483546,
18.8427933888379));
#45717=CARTESIAN_POINT('Ctrl Pts',(-48.6940204727097,-76.3381158557561,
20.6327850920547));
#45718=CARTESIAN_POINT('Ctrl Pts',(-48.5705971077618,-77.3016688744965,
22.1702805692189));
#45719=CARTESIAN_POINT('Ctrl Pts',(-48.4462749687256,-79.0259411160725,
22.7760661916481));
#45720=CARTESIAN_POINT('Ctrl Pts',(-48.3210268594155,-80.7646781227256,
22.1701438364573));
#45721=CARTESIAN_POINT('Ctrl Pts',(-48.194828354645,-81.7537397700009,20.600520392927));
#45722=CARTESIAN_POINT('Ctrl Pts',(-48.067657124948,-81.5468220181871,18.7423903191848));
#45723=CARTESIAN_POINT('Ctrl Pts',(-47.939493283709,-80.2161779802247,17.408315588859));
#45724=CARTESIAN_POINT('Ctrl Pts',(-47.8103191852242,-78.3292737794169,
17.1930918886314));
#45725=CARTESIAN_POINT('Ctrl Pts',(-47.6801196014556,-76.7069354904978,
18.2094845308307));
#45726=CARTESIAN_POINT('Ctrl Pts',(-47.5488814434326,-76.0672383673362,
20.0294810068135));
#45727=CARTESIAN_POINT('Ctrl Pts',(-47.416594505357,-76.7065669191,21.8669523450674));
#45728=CARTESIAN_POINT('Ctrl Pts',(-47.3054739921019,-78.0892405398055,
22.7364966500394));
#45729=CARTESIAN_POINT('Ctrl Pts',(-47.2160471510534,-79.3463826256051,
22.8042334163218));
#45730=CARTESIAN_POINT('Ctrl Pts',(-47.1262652329036,-80.5655791894923,
22.4580413955535));
#45731=CARTESIAN_POINT('Ctrl Pts',(-47.028424926471,-81.5778068418593,21.4447201314267));
#45732=CARTESIAN_POINT('Ctrl Pts',(-46.8920633743752,-82.0174655355277,
19.5449713709624));
#45733=CARTESIAN_POINT('Ctrl Pts',(-46.7947208039299,-81.3856409780859,
18.2026916859546));
#45734=CARTESIAN_POINT('Ctrl Pts',(-46.7217816589043,-80.5625621836747,
17.6063431295216));
#45735=CARTESIAN_POINT('Ctrl Pts',(-46.6756703161032,-80.0158736768733,
17.2724754919093));
#45736=CARTESIAN_POINT('Ctrl Pts',(-46.5889231063328,-78.8118838311396,
16.9587472215029));
#45737=CARTESIAN_POINT('Ctrl Pts',(-46.4608607449701,-77.0312443703412,
17.5782509142251));
#45738=CARTESIAN_POINT('Ctrl Pts',(-46.320096662837,-75.9317484370967,19.3262399513567));
#45739=CARTESIAN_POINT('Ctrl Pts',(-46.1625627274249,-76.1796390782523,
21.6382820870331));
#45740=CARTESIAN_POINT('Ctrl Pts',(-46.0036976824358,-78.0797604735648,
23.161043382435));
#45741=CARTESIAN_POINT('Ctrl Pts',(-45.875575120692,-79.9539900307661,22.9387587305178));
#45742=CARTESIAN_POINT('Ctrl Pts',(-45.7468693842732,-81.4804681301568,
21.9876429965309));
#45743=CARTESIAN_POINT('Ctrl Pts',(-45.6012748321095,-82.4538170148249,
19.9738849325405));
#45744=CARTESIAN_POINT('Ctrl Pts',(-45.427232277001,-81.2961720285109,17.5655039599756));
#45745=CARTESIAN_POINT('Ctrl Pts',(-45.2739171720439,-79.2134585556205,
16.7610475026127));
#45746=CARTESIAN_POINT('Ctrl Pts',(-45.1417971188088,-77.3459353550754,
17.1811310509974));
#45747=CARTESIAN_POINT('Ctrl Pts',(-45.0090220243129,-76.0316098470263,
18.5974518633508));
#45748=CARTESIAN_POINT('Ctrl Pts',(-44.8755781232189,-75.7405809030124,
20.5124323793354));
#45749=CARTESIAN_POINT('Ctrl Pts',(-44.7415271801667,-76.5852722717957,
22.2695961253322));
#45750=CARTESIAN_POINT('Ctrl Pts',(-44.6180902998809,-78.1379907426961,
23.1657114909166));
#45751=CARTESIAN_POINT('Ctrl Pts',(-44.5054512296313,-79.7434195908802,
23.164944985583));
#45752=CARTESIAN_POINT('Ctrl Pts',(-44.403762511972,-81.0487736199286,22.5375621623098));
#45753=CARTESIAN_POINT('Ctrl Pts',(-44.3187755095097,-81.803927310347,21.5908894911752));
#45754=CARTESIAN_POINT('Ctrl Pts',(-44.2506328752899,-82.1178415065376,
20.6917295984092));
#45755=CARTESIAN_POINT('Ctrl Pts',(-44.182398840638,-82.2256429773631,19.7439125803809));
#45756=CARTESIAN_POINT('Ctrl Pts',(-44.0969322192952,-81.9548232044274,
18.5574476942815));
#45757=CARTESIAN_POINT('Ctrl Pts',(-43.9941104782232,-81.0423485897149,
17.4111483979706));
#45758=CARTESIAN_POINT('Ctrl Pts',(-43.8910383941689,-79.7196940350006,
16.775424120007));
#45759=CARTESIAN_POINT('Ctrl Pts',(-43.7705035162583,-78.002099182994,16.7721223788263));
#45760=CARTESIAN_POINT('Ctrl Pts',(-43.6323887221455,-76.2810481647922,
17.8464747635074));
#45761=CARTESIAN_POINT('Ctrl Pts',(-43.4765588968987,-75.523682339802,20.0119147314719));
#45762=CARTESIAN_POINT('Ctrl Pts',(-43.3203104399421,-76.2814825700852,
22.1798824763609));
#45763=CARTESIAN_POINT('Ctrl Pts',(-43.1636988788655,-78.231183283665,23.4065011857406));
#45764=CARTESIAN_POINT('Ctrl Pts',(-43.0067701275799,-80.5243831967142,
23.1486711821189));
#45765=CARTESIAN_POINT('Ctrl Pts',(-42.8495752732181,-82.1593690722874,
21.5147059359154));
#45766=CARTESIAN_POINT('Ctrl Pts',(-42.692163877366,-82.4189200513296,19.2145330104326));
#45767=CARTESIAN_POINT('Ctrl Pts',(-42.5345870339397,-81.186419702914,17.252341889947));
#45768=CARTESIAN_POINT('Ctrl Pts',(-42.3768955999956,-78.9974076189623,
16.4862760606958));
#45769=CARTESIAN_POINT('Ctrl Pts',(-42.2191420853598,-76.8080962266395,
17.2523251227454));
#45770=CARTESIAN_POINT('Ctrl Pts',(-42.0613769172934,-75.5725384440266,
19.2168395004127));
#45771=CARTESIAN_POINT('Ctrl Pts',(-41.9036550552319,-75.8347814351827,
21.521221016026));
#45772=CARTESIAN_POINT('Ctrl Pts',(-41.7459807111963,-77.472413483267,23.1602525911309));
#45773=CARTESIAN_POINT('Ctrl Pts',(-41.5885306559279,-79.775140966077,23.418780464454));
#45774=CARTESIAN_POINT('Ctrl Pts',(-41.4573307056616,-81.4042927804752,
22.3935048251252));
#45775=CARTESIAN_POINT('Ctrl Pts',(-41.352752520906,-82.115291034017,21.0964799172088));
#45776=CARTESIAN_POINT('Ctrl Pts',(-41.3002494256406,-82.2388355933261,
20.376965989901));
#45777=CARTESIAN_POINT('Ctrl Pts',(-41.2742555650807,-82.2395138211038,
20.0097117288145));
#45778=CARTESIAN_POINT('Ctrl Pts',(-56.4864851473071,-82.244406184525,20.0072137503139));
#45779=CARTESIAN_POINT('Ctrl Pts',(-56.4604905643926,-82.2437279376262,
19.6399492874994));
#45780=CARTESIAN_POINT('Ctrl Pts',(-56.4079575497986,-82.1200108277759,
18.920179834268));
#45781=CARTESIAN_POINT('Ctrl Pts',(-56.3035124971059,-81.4097019511314,
17.6250516252384));
#45782=CARTESIAN_POINT('Ctrl Pts',(-56.1728276535228,-79.7866044363345,
16.6050341645054));
#45783=CARTESIAN_POINT('Ctrl Pts',(-56.0165510858122,-77.5016274012234,
16.8629024989691));
#45784=CARTESIAN_POINT('Ctrl Pts',(-55.860614787854,-75.8832484996987,18.4844935021406));
#45785=CARTESIAN_POINT('Ctrl Pts',(-55.7051693135572,-75.6261404352104,
20.7551980554146));
#45786=CARTESIAN_POINT('Ctrl Pts',(-55.5501938084122,-76.8403636413408,
22.6833784979432));
#45787=CARTESIAN_POINT('Ctrl Pts',(-55.3957875322177,-78.9829092901664,
23.4316620324926));
#45788=CARTESIAN_POINT('Ctrl Pts',(-55.24196914399,-81.1169629091852,22.6834289530792));
#45789=CARTESIAN_POINT('Ctrl Pts',(-55.0887919206184,-82.3135405021836,
20.775923098071));
#45790=CARTESIAN_POINT('Ctrl Pts',(-54.9362912020637,-82.0610299365338,
18.5483313129834));
#45791=CARTESIAN_POINT('Ctrl Pts',(-54.7845085300065,-80.4817755535852,
16.971919870799));
#45792=CARTESIAN_POINT('Ctrl Pts',(-54.6334788977311,-78.2758404106939,
16.725043392695));
#45793=CARTESIAN_POINT('Ctrl Pts',(-54.4832409733484,-76.4057062548225,
17.9022861782441));
#45794=CARTESIAN_POINT('Ctrl Pts',(-54.3587251945716,-75.8050582161101,
19.6298057588485));
#45795=CARTESIAN_POINT('Ctrl Pts',(-54.2595476624192,-76.0424269715925,
21.0072061434664));
#45796=CARTESIAN_POINT('Ctrl Pts',(-54.1853814487781,-76.5470394748316,
21.9218209716504));
#45797=CARTESIAN_POINT('Ctrl Pts',(-54.1114367342337,-77.3244395716799,
22.6148156691908));
#45798=CARTESIAN_POINT('Ctrl Pts',(-54.0131440892721,-78.603436095196,23.1472615029114));
#45799=CARTESIAN_POINT('Ctrl Pts',(-53.89084487041,-80.3887986905675,22.9461526703339));
#45800=CARTESIAN_POINT('Ctrl Pts',(-53.7450274334933,-81.9037455172806,
21.4272424575567));
#45801=CARTESIAN_POINT('Ctrl Pts',(-53.6001717997465,-82.1395116153914,
19.3115740408835));
#45802=CARTESIAN_POINT('Ctrl Pts',(-53.4563014930413,-81.0123159195144,
17.5203471528416));
#45803=CARTESIAN_POINT('Ctrl Pts',(-53.3134327675242,-79.0285454948578,
16.8315743124168));
#45804=CARTESIAN_POINT('Ctrl Pts',(-53.1715865117443,-77.0609306911321,
17.5224129170849));
#45805=CARTESIAN_POINT('Ctrl Pts',(-53.0307741778491,-75.9616236346913,
19.2767822365058));
#45806=CARTESIAN_POINT('Ctrl Pts',(-52.8910084417059,-76.1943323645279,
21.3184594913424));
#45807=CARTESIAN_POINT('Ctrl Pts',(-52.7522984009004,-77.6383558894365,
22.7586903987038));
#45808=CARTESIAN_POINT('Ctrl Pts',(-52.6146512025417,-79.6498424442095,
22.9826023867588));
#45809=CARTESIAN_POINT('Ctrl Pts',(-52.4780713027781,-81.3488556804301,
21.9118659023322));
#45810=CARTESIAN_POINT('Ctrl Pts',(-52.3425607834635,-82.0044406266488,
20.0302316483582));
#45811=CARTESIAN_POINT('Ctrl Pts',(-52.2081191771091,-81.3490236341856,
18.1651768258721));
#45812=CARTESIAN_POINT('Ctrl Pts',(-52.0747434976663,-79.6870258617311,
17.1239828634592));
#45813=CARTESIAN_POINT('Ctrl Pts',(-51.9424282544566,-77.7539297691834,
17.3444231983787));
#45814=CARTESIAN_POINT('Ctrl Pts',(-51.811165533831,-76.3909322893194,18.7110902501839));
#45815=CARTESIAN_POINT('Ctrl Pts',(-51.6809449612247,-76.1790859877837,
20.6141953273701));
#45816=CARTESIAN_POINT('Ctrl Pts',(-51.5517537883029,-77.191947419427,22.2214040979907));
#45817=CARTESIAN_POINT('Ctrl Pts',(-51.4235767560169,-78.9718377059214,
22.841571824978));
#45818=CARTESIAN_POINT('Ctrl Pts',(-51.2963963326679,-80.736261721788,22.22157134421));
#45819=CARTESIAN_POINT('Ctrl Pts',(-51.1701921675022,-81.7215941240923,
20.6488770320107));
#45820=CARTESIAN_POINT('Ctrl Pts',(-51.04494276267,-81.512959740282,18.81889422146));
#45821=CARTESIAN_POINT('Ctrl Pts',(-50.9206221929331,-80.2186251867107,
17.5277455362834));
#45822=CARTESIAN_POINT('Ctrl Pts',(-50.7972074154033,-78.4146002994715,
17.3268756024418));
#45823=CARTESIAN_POINT('Ctrl Pts',(-50.6746620991811,-76.890151497893,18.2872664763635));
#45824=CARTESIAN_POINT('Ctrl Pts',(-50.5529729373044,-76.3000175094954,
19.9778077309354));
#45825=CARTESIAN_POINT('Ctrl Pts',(-50.4320678326896,-76.8908632778512,
21.6540392745149));
#45826=CARTESIAN_POINT('Ctrl Pts',(-50.3119596915113,-78.3872184931367,
22.5923847015876));
#45827=CARTESIAN_POINT('Ctrl Pts',(-50.1925891892237,-80.1314109391504,
22.3940639393699));
#45828=CARTESIAN_POINT('Ctrl Pts',(-50.0739208360292,-81.364151714832,21.1588635538291));
#45829=CARTESIAN_POINT('Ctrl Pts',(-49.9559142964183,-81.5567499157273,
19.4340963825786));
#45830=CARTESIAN_POINT('Ctrl Pts',(-49.8385286442904,-80.6369710758383,
17.9731922877536));
#45831=CARTESIAN_POINT('Ctrl Pts',(-49.7217215196508,-79.0147721014308,
17.4069911561483));
#45832=CARTESIAN_POINT('Ctrl Pts',(-49.6054475819526,-77.4013710218261,
17.9732338854577));
#45833=CARTESIAN_POINT('Ctrl Pts',(-49.4896640315131,-76.4954328808651,
19.4150710735183));
#45834=CARTESIAN_POINT('Ctrl Pts',(-49.3743185623355,-76.6880905927546,
21.1019689204466));
#45835=CARTESIAN_POINT('Ctrl Pts',(-49.2593775009166,-77.8799327853689,
22.293670540459));
#45836=CARTESIAN_POINT('Ctrl Pts',(-49.1320281323078,-79.7504014899488,
22.5091749028563));
#45837=CARTESIAN_POINT('Ctrl Pts',(-49.0177356327972,-81.1156454492951,
21.4212181211584));
#45838=CARTESIAN_POINT('Ctrl Pts',(-48.9226956524205,-81.4083679794129,
20.0913953086005));
#45839=CARTESIAN_POINT('Ctrl Pts',(-48.8594012746119,-81.2602898532879,
19.2152150535946));
#45840=CARTESIAN_POINT('Ctrl Pts',(-48.7834990124813,-80.743690351567,18.2765978302752));
#45841=CARTESIAN_POINT('Ctrl Pts',(-48.6887409077433,-79.5658058177838,
17.5354801724578));
#45842=CARTESIAN_POINT('Ctrl Pts',(-48.5751083143484,-77.9040028995463,
17.7226483218797));
#45843=CARTESIAN_POINT('Ctrl Pts',(-48.4615222697365,-76.7233535485495,
18.9039803371791));
#45844=CARTESIAN_POINT('Ctrl Pts',(-48.3479226073069,-76.5359862699538,
20.5641246869877));
#45845=CARTESIAN_POINT('Ctrl Pts',(-48.2342619825293,-77.4252520533088,
21.9796151711007));
#45846=CARTESIAN_POINT('Ctrl Pts',(-48.1204872312989,-79.004419957339,22.5325711539792));
#45847=CARTESIAN_POINT('Ctrl Pts',(-48.0065478245435,-80.5861911385054,
21.9795902880699));
#45848=CARTESIAN_POINT('Ctrl Pts',(-47.8923923883356,-81.4798322178271,
20.5584387533152));
#45849=CARTESIAN_POINT('Ctrl Pts',(-47.7779709658212,-81.2921160797888,
18.8862371910536));
#45850=CARTESIAN_POINT('Ctrl Pts',(-47.6632337755331,-80.0995238430424,
17.692561192887));
#45851=CARTESIAN_POINT('Ctrl Pts',(-47.5481326792351,-78.4175602791118,
17.5020376251063));
#45852=CARTESIAN_POINT('Ctrl Pts',(-47.4326186963439,-76.9784793998031,
18.4050558861712));
#45853=CARTESIAN_POINT('Ctrl Pts',(-47.3166472249995,-76.4140883364296,
20.0141330991597));
#45854=CARTESIAN_POINT('Ctrl Pts',(-47.2001668836196,-76.9781174597249,
21.6320696043394));
#45855=CARTESIAN_POINT('Ctrl Pts',(-47.102648679663,-78.1922506890227,22.3947478975612));
#45856=CARTESIAN_POINT('Ctrl Pts',(-47.0243227633107,-79.2934240076467,
22.4539599055311));
#45857=CARTESIAN_POINT('Ctrl Pts',(-46.9457927494229,-80.3599158358455,
22.1509640171201));
#45858=CARTESIAN_POINT('Ctrl Pts',(-46.8603764354211,-81.2434007966227,
21.2659119848418));
#45859=CARTESIAN_POINT('Ctrl Pts',(-46.741537508699,-81.6262476288813,19.6101004829355));
#45860=CARTESIAN_POINT('Ctrl Pts',(-46.6568637398311,-81.0760751285665,
18.442619615091));
#45861=CARTESIAN_POINT('Ctrl Pts',(-46.5934814534038,-80.3608237881132,
17.9244206785242));
#45862=CARTESIAN_POINT('Ctrl Pts',(-46.5534170582025,-79.8858191183262,
17.634331035083));
#45863=CARTESIAN_POINT('Ctrl Pts',(-46.4780913513627,-78.8402806753656,
17.3620372339516));
#45864=CARTESIAN_POINT('Ctrl Pts',(-46.3669961151747,-77.2955789649705,
17.8997405417894));
#45865=CARTESIAN_POINT('Ctrl Pts',(-46.244957124377,-76.3424755180359,19.4152946981647));
#45866=CARTESIAN_POINT('Ctrl Pts',(-46.1084247765798,-76.557423872972,21.4190561415109));
#45867=CARTESIAN_POINT('Ctrl Pts',(-45.9707329691292,-78.2041668358601,
22.7389476836005));
#45868=CARTESIAN_POINT('Ctrl Pts',(-45.8596256684999,-79.8294782506187,
22.5463669763199));
#45869=CARTESIAN_POINT('Ctrl Pts',(-45.7479534244289,-81.1538676554818,
21.7211828863017));
#45870=CARTESIAN_POINT('Ctrl Pts',(-45.6215284524728,-81.9995992769805,
19.9729588911492));
#45871=CARTESIAN_POINT('Ctrl Pts',(-45.4701335388581,-80.9935962179004,
17.8777328348881));
#45872=CARTESIAN_POINT('Ctrl Pts',(-45.3364999414446,-79.1787132506225,
17.1761128984294));
#45873=CARTESIAN_POINT('Ctrl Pts',(-45.2211494416365,-77.5482952105881,
17.5424430554541));
#45874=CARTESIAN_POINT('Ctrl Pts',(-45.1049770492795,-76.3982092929863,
18.7809644843786));
#45875=CARTESIAN_POINT('Ctrl Pts',(-44.9879827710476,-76.1425303947159,
20.4596334384395));
#45876=CARTESIAN_POINT('Ctrl Pts',(-44.8701487351934,-76.8842395494568,
22.0040483067461));
#45877=CARTESIAN_POINT('Ctrl Pts',(-44.7613669966606,-78.2519997258415,
22.7941158256609));
#45878=CARTESIAN_POINT('Ctrl Pts',(-44.6618625928431,-79.6699579690279,
22.7937774228697));
#45879=CARTESIAN_POINT('Ctrl Pts',(-44.5718347215401,-80.8255497018144,
22.238718741254));
#45880=CARTESIAN_POINT('Ctrl Pts',(-44.4964128977026,-81.4957557167802,
21.3989808934452));
#45881=CARTESIAN_POINT('Ctrl Pts',(-44.4358432233994,-81.7748194347551,
20.5998204980552));
#45882=CARTESIAN_POINT('Ctrl Pts',(-44.3751132847541,-81.8708038494031,
19.756384583514));
#45883=CARTESIAN_POINT('Ctrl Pts',(-44.2989055206723,-81.6296514379495,
18.6985105124891));
#45884=CARTESIAN_POINT('Ctrl Pts',(-44.2069805398381,-80.8143272807318,
17.6736395231787));
#45885=CARTESIAN_POINT('Ctrl Pts',(-44.1145834563323,-79.6290317450135,
17.1034965275683));
#45886=CARTESIAN_POINT('Ctrl Pts',(-44.0062428609622,-78.0854298017345,
17.1000390392989));
#45887=CARTESIAN_POINT('Ctrl Pts',(-43.8816346938952,-76.5325285282763,
18.067897428711));
#45888=CARTESIAN_POINT('Ctrl Pts',(-43.7403998945461,-75.8448247700219,
20.0291730208815));
#45889=CARTESIAN_POINT('Ctrl Pts',(-43.5981411706491,-76.5329789950227,
22.002878837303));
#45890=CARTESIAN_POINT('Ctrl Pts',(-43.4548672770674,-78.3150063887284,
23.126063236142));
#45891=CARTESIAN_POINT('Ctrl Pts',(-43.3105981900307,-80.4226136408398,
22.8909180049375));
#45892=CARTESIAN_POINT('Ctrl Pts',(-43.1653527245271,-81.9340396600559,
21.3830760708777));
#45893=CARTESIAN_POINT('Ctrl Pts',(-43.0191522761607,-82.17692827644,19.2478221178909));
#45894=CARTESIAN_POINT('Ctrl Pts',(-42.8720229653157,-81.0283119211314,
17.4154508680147));
#45895=CARTESIAN_POINT('Ctrl Pts',(-42.72398589125,-78.9749522023299,16.6947394827832));
#45896=CARTESIAN_POINT('Ctrl Pts',(-42.5750811952544,-76.9086922943806,
17.4156052640251));
#45897=CARTESIAN_POINT('Ctrl Pts',(-42.4253130086118,-75.7347412322853,
19.2784528703265));
#45898=CARTESIAN_POINT('Ctrl Pts',(-42.2747717246015,-75.9829440186284,
21.4774728284354));
#45899=CARTESIAN_POINT('Ctrl Pts',(-42.1234329434898,-77.5530085323627,
23.0518956352805));
#45900=CARTESIAN_POINT('Ctrl Pts',(-41.9714093758298,-79.7755362218638,
23.3034733604654));
#45901=CARTESIAN_POINT('Ctrl Pts',(-41.8440182230729,-81.3582430385855,
22.3099349163572));
#45902=CARTESIAN_POINT('Ctrl Pts',(-41.7419838188056,-82.0522110516402,
21.0447471654702));
#45903=CARTESIAN_POINT('Ctrl Pts',(-41.6906401481783,-82.173201565315,20.3413153591936));
#45904=CARTESIAN_POINT('Ctrl Pts',(-41.6652025102081,-82.1738652802192,
19.9819196890115));
#45905=CARTESIAN_POINT('Ctrl Pts',(-56.8752592603261,-82.1647273768201,
19.9798438846464));
#45906=CARTESIAN_POINT('Ctrl Pts',(-56.849820483618,-82.1640636319366,19.6204321297793));
#45907=CARTESIAN_POINT('Ctrl Pts',(-56.7985225143976,-82.0433810770499,
18.9174518831814));
#45908=CARTESIAN_POINT('Ctrl Pts',(-56.6961514981416,-81.3476586777129,
17.6477773877481));
#45909=CARTESIAN_POINT('Ctrl Pts',(-56.5675242515753,-79.750819824018,16.6421258544651));
#45910=CARTESIAN_POINT('Ctrl Pts',(-56.4127777672657,-77.4877184491089,
16.8951938814764));
#45911=CARTESIAN_POINT('Ctrl Pts',(-56.2574474727138,-75.8738250468064,
18.5092015929225));
#45912=CARTESIAN_POINT('Ctrl Pts',(-56.1016864083364,-75.6139448078687,
20.7846026649799));
#45913=CARTESIAN_POINT('Ctrl Pts',(-55.9454946697642,-76.8362502840664,
22.7298037295438));
#45914=CARTESIAN_POINT('Ctrl Pts',(-55.7889342465819,-79.0084823141423,
23.4908597602889));
#45915=CARTESIAN_POINT('Ctrl Pts',(-55.6320475439178,-81.1864409267459,
22.7296922749762));
#45916=CARTESIAN_POINT('Ctrl Pts',(-55.4748870696447,-82.4163634726471,
20.7734068870129));
#45917=CARTESIAN_POINT('Ctrl Pts',(-55.3175017283399,-82.1580193500458,
18.4737774574898));
#45918=CARTESIAN_POINT('Ctrl Pts',(-55.1599423980537,-80.5200128949239,
16.8354996081942));
#45919=CARTESIAN_POINT('Ctrl Pts',(-55.0022599601601,-78.2168457221201,
16.5754940197918));
#45920=CARTESIAN_POINT('Ctrl Pts',(-54.8445051279008,-76.2517211817873,
17.8098895741297));
#45921=CARTESIAN_POINT('Ctrl Pts',(-54.7130265903422,-75.6157428815775,
19.6337203952621));
#45922=CARTESIAN_POINT('Ctrl Pts',(-54.6078575942801,-75.8671226247866,
21.0945269420162));
#45923=CARTESIAN_POINT('Ctrl Pts',(-54.5289952123769,-76.4034892139563,
22.0671944258025));
#45924=CARTESIAN_POINT('Ctrl Pts',(-54.45015348062,-77.2322557766833,22.8063001739345));
#45925=CARTESIAN_POINT('Ctrl Pts',(-54.3450673578701,-78.5994774058443,
23.3758588243804));
#45926=CARTESIAN_POINT('Ctrl Pts',(-54.2137934297236,-80.5160729256162,
23.1616447909686));
#45927=CARTESIAN_POINT('Ctrl Pts',(-54.0564493591351,-82.1522391523417,
21.5241073076164));
#45928=CARTESIAN_POINT('Ctrl Pts',(-53.8993416236473,-82.4098810996251,
19.2296924343533));
#45929=CARTESIAN_POINT('Ctrl Pts',(-53.7425168108729,-81.182881687469,17.2762363265303));
#45930=CARTESIAN_POINT('Ctrl Pts',(-53.5860317510178,-79.0106245714821,
16.5200699813797));
#45931=CARTESIAN_POINT('Ctrl Pts',(-53.4299252093456,-76.8447807469938,
17.278626424945));
#45932=CARTESIAN_POINT('Ctrl Pts',(-53.2742504725809,-75.6280966857697,
19.2170863781129));
#45933=CARTESIAN_POINT('Ctrl Pts',(-53.119053328739,-75.8848398803048,21.4841287570035));
#45934=CARTESIAN_POINT('Ctrl Pts',(-52.9643793906807,-77.4937457201632,
23.0910239089316));
#45935=CARTESIAN_POINT('Ctrl Pts',(-52.8102726712708,-79.7452709481134,
23.3431554210652));
#45936=CARTESIAN_POINT('Ctrl Pts',(-52.6567761139084,-81.6551584863882,
22.1411843335501));
#45937=CARTESIAN_POINT('Ctrl Pts',(-52.503931172354,-82.3957109528423,20.0196751705757));
#45938=CARTESIAN_POINT('Ctrl Pts',(-52.351778100954,-81.6552494754696,17.9089395610088));
#45939=CARTESIAN_POINT('Ctrl Pts',(-52.2003554700587,-79.769380504285,16.7261729823972));
#45940=CARTESIAN_POINT('Ctrl Pts',(-52.0496999603813,-77.5687465705001,
16.9760925231193));
#45941=CARTESIAN_POINT('Ctrl Pts',(-51.8998463388462,-76.012452612391,18.5352706051618));
#45942=CARTESIAN_POINT('Ctrl Pts',(-51.7508275550648,-75.7692773993649,
20.7124125039816));
#45943=CARTESIAN_POINT('Ctrl Pts',(-51.6026745746877,-76.9298555111948,
22.5553551303563));
#45944=CARTESIAN_POINT('Ctrl Pts',(-51.4554165147952,-78.9738720391516,
23.268189846291));
#45945=CARTESIAN_POINT('Ctrl Pts',(-51.3090803638474,-81.0035379035248,
22.5555024258079));
#45946=CARTESIAN_POINT('Ctrl Pts',(-51.1636912979732,-82.1385729582828,
20.7445599295758));
#45947=CARTESIAN_POINT('Ctrl Pts',(-51.0192712722321,-81.8983414763417,
18.6352378679758));
#45948=CARTESIAN_POINT('Ctrl Pts',(-50.8758418420892,-80.4057039065717,
17.1460946436865));
#45949=CARTESIAN_POINT('Ctrl Pts',(-50.7334180548278,-78.3246929559324,
16.9143845079462));
#45950=CARTESIAN_POINT('Ctrl Pts',(-50.59202195101,-76.5664296105997,18.0221939935554));
#45951=CARTESIAN_POINT('Ctrl Pts',(-50.4516523555111,-75.8863075302345,
19.9712950019085));
#45952=CARTESIAN_POINT('Ctrl Pts',(-50.3123526988948,-76.567215386836,21.9020278716489));
#45953=CARTESIAN_POINT('Ctrl Pts',(-50.1740919754148,-78.2891689544036,
22.9812616932865));
#45954=CARTESIAN_POINT('Ctrl Pts',(-50.0368949024821,-80.2928434997237,
22.7528430998679));
#45955=CARTESIAN_POINT('Ctrl Pts',(-49.9007628172212,-81.7058263131614,
21.3360544397924));
#45956=CARTESIAN_POINT('Ctrl Pts',(-49.7656971633282,-81.9253505848977,
19.3628482967946));
#45957=CARTESIAN_POINT('Ctrl Pts',(-49.6316962630047,-80.875132507514,17.696518464657));
#45958=CARTESIAN_POINT('Ctrl Pts',(-49.4987557206264,-79.0295187448053,
17.0534789042926));
#45959=CARTESIAN_POINT('Ctrl Pts',(-49.3668698109708,-77.2008650160025,
17.6965257519911));
#45960=CARTESIAN_POINT('Ctrl Pts',(-49.2360272361897,-76.1788139886115,
19.3257142409972));
#45961=CARTESIAN_POINT('Ctrl Pts',(-49.1062212407889,-76.3969375716729,
21.2228970450781));
#45962=CARTESIAN_POINT('Ctrl Pts',(-48.9774270334425,-77.7326214921823,
22.5564587298384));
#45963=CARTESIAN_POINT('Ctrl Pts',(-48.8354545460198,-79.8173749253273,
22.7945675099833));
#45964=CARTESIAN_POINT('Ctrl Pts',(-48.7088470418068,-81.3278881573385,
21.5873043990266));
#45965=CARTESIAN_POINT('Ctrl Pts',(-48.6041290543196,-81.649373826429,20.1224911974117));
#45966=CARTESIAN_POINT('Ctrl Pts',(-48.534620354474,-81.4866810139768,19.1606355190012));
#45967=CARTESIAN_POINT('Ctrl Pts',(-48.4515237794181,-80.9208898398131,
18.1333862032429));
#45968=CARTESIAN_POINT('Ctrl Pts',(-48.3482038580319,-79.6366194811744,
17.3271167141711));
#45969=CARTESIAN_POINT('Ctrl Pts',(-48.2251202545579,-77.837643114993,17.5317437994423));
#45970=CARTESIAN_POINT('Ctrl Pts',(-48.1028920056514,-76.5693020567696,
18.8036614028563));
#45971=CARTESIAN_POINT('Ctrl Pts',(-47.9814941498671,-76.3712437839294,
20.5771187760201));
#45972=CARTESIAN_POINT('Ctrl Pts',(-47.8608902646939,-77.3161881337434,
22.0771677966622));
#45973=CARTESIAN_POINT('Ctrl Pts',(-47.7410462421363,-78.9795365673136,
22.6572563470884));
#45974=CARTESIAN_POINT('Ctrl Pts',(-47.621924133136,-80.6317614090933,22.0772596720609));
#45975=CARTESIAN_POINT('Ctrl Pts',(-47.5034851640459,-81.5566082922497,
20.6022109593297));
#45976=CARTESIAN_POINT('Ctrl Pts',(-47.3856887008372,-81.3611652480675,
18.8816656058404));
#45977=CARTESIAN_POINT('Ctrl Pts',(-47.2684930379886,-80.1418965970207,
17.6645313415393));
#45978=CARTESIAN_POINT('Ctrl Pts',(-47.1518546779662,-78.4378987159531,
17.4738303532817));
#45979=CARTESIAN_POINT('Ctrl Pts',(-47.035729680131,-76.9929991848448,18.3832266388075));
#45980=CARTESIAN_POINT('Ctrl Pts',(-46.9200707020022,-76.4325170788587,
19.9880981973879));
#45981=CARTESIAN_POINT('Ctrl Pts',(-46.8048338212136,-76.9925383820305,
21.5874694958995));
#45982=CARTESIAN_POINT('Ctrl Pts',(-46.7091081845317,-78.1847792549115,
22.334195828462));
#45983=CARTESIAN_POINT('Ctrl Pts',(-46.6326982675346,-79.2587887541768,
22.3916117914154));
#45984=CARTESIAN_POINT('Ctrl Pts',(-46.5563871527435,-80.2949437910353,
22.0967756284929));
#45985=CARTESIAN_POINT('Ctrl Pts',(-46.4738638160743,-81.1473553294667,
21.2409040031375));
#45986=CARTESIAN_POINT('Ctrl Pts',(-46.3597902157357,-81.513659560961,19.6513176505422));
#45987=CARTESIAN_POINT('Ctrl Pts',(-46.2791218208211,-80.9873379664293,
18.539972764432));
#45988=CARTESIAN_POINT('Ctrl Pts',(-46.2190639506903,-80.3096902111283,
18.0491241809696));
#45989=CARTESIAN_POINT('Ctrl Pts',(-46.1811383237244,-79.8600373014878,
17.7745096412059));
#45990=CARTESIAN_POINT('Ctrl Pts',(-46.110055836894,-78.8732147621218,17.5182574519196));
#45991=CARTESIAN_POINT('Ctrl Pts',(-46.0058525452064,-77.4252814529119,
18.0242139470201));
#45992=CARTESIAN_POINT('Ctrl Pts',(-45.8922026265434,-76.539210510756,19.4365393731754));
#45993=CARTESIAN_POINT('Ctrl Pts',(-45.7658834584667,-76.7403618945056,
21.2900242272622));
#45994=CARTESIAN_POINT('Ctrl Pts',(-45.6394596654201,-78.254383737651,22.4991687889416));
#45995=CARTESIAN_POINT('Ctrl Pts',(-45.5381619454123,-79.735719356395,22.3220960440989));
#45996=CARTESIAN_POINT('Ctrl Pts',(-45.4367445560468,-80.9384968216192,
21.5724769602265));
#45997=CARTESIAN_POINT('Ctrl Pts',(-45.3224673093312,-81.7004093138281,
19.9911131458827));
#45998=CARTESIAN_POINT('Ctrl Pts',(-45.1865750493327,-80.7945960871807,
18.1116772564183));
#45999=CARTESIAN_POINT('Ctrl Pts',(-45.067267809229,-79.1739536659866,17.4864162444988));
#46000=CARTESIAN_POINT('Ctrl Pts',(-44.9646874949972,-77.7240469630762,
17.8129469503058));
#46001=CARTESIAN_POINT('Ctrl Pts',(-44.8617690078026,-76.7056236007332,
18.910928891785));
#46002=CARTESIAN_POINT('Ctrl Pts',(-44.7584641908549,-76.480539316094,20.3933934365883));
#46003=CARTESIAN_POINT('Ctrl Pts',(-44.6547587194653,-77.1340685669796,
21.7526435901753));
#46004=CARTESIAN_POINT('Ctrl Pts',(-44.5592880723631,-78.3349402974165,
22.4457038177027));
#46005=CARTESIAN_POINT('Ctrl Pts',(-44.4721509081512,-79.576854086323,22.4451636374686));
#46006=CARTESIAN_POINT('Ctrl Pts',(-44.3934483384747,-80.5871463859038,
21.9596778440093));
#46007=CARTESIAN_POINT('Ctrl Pts',(-44.3276243811037,-81.1720812201823,
21.226542345069));
#46008=CARTESIAN_POINT('Ctrl Pts',(-44.274808294589,-81.4154125231196,20.5296318079551));
#46009=CARTESIAN_POINT('Ctrl Pts',(-44.2218917840583,-81.4990363304231,
19.7946015755715));
#46010=CARTESIAN_POINT('Ctrl Pts',(-44.1555489539339,-81.2889560814031,
18.8735938810967));
#46011=CARTESIAN_POINT('Ctrl Pts',(-44.0756146123583,-80.5797685906883,
17.9823336840274));
#46012=CARTESIAN_POINT('Ctrl Pts',(-43.9953446131058,-79.5498136667998,
17.4870332901371));
#46013=CARTESIAN_POINT('Ctrl Pts',(-43.9012877875629,-78.2095611820704,
17.4841349207429));
#46014=CARTESIAN_POINT('Ctrl Pts',(-43.7932102496733,-76.8623578132868,
18.3240159758579));
#46015=CARTESIAN_POINT('Ctrl Pts',(-43.6707955883791,-76.2661491824651,
20.024684650845));
#46016=CARTESIAN_POINT('Ctrl Pts',(-43.5475096262792,-76.8627315678271,
21.7357943752776));
#46017=CARTESIAN_POINT('Ctrl Pts',(-43.4233292629246,-78.4078293249966,
22.7097747478266));
#46018=CARTESIAN_POINT('Ctrl Pts',(-43.2982253749316,-80.2361879343779,
22.5059992916388));
#46019=CARTESIAN_POINT('Ctrl Pts',(-43.1721744015948,-81.5486128680076,
21.1971050757497));
#46020=CARTESIAN_POINT('Ctrl Pts',(-43.0451541452452,-81.7600970908285,
19.3412274997668));
#46021=CARTESIAN_POINT('Ctrl Pts',(-42.9171435660302,-80.7606861815771,
17.7460023752414));
#46022=CARTESIAN_POINT('Ctrl Pts',(-42.7881277014792,-78.9703896149554,
17.1170309454072));
#46023=CARTESIAN_POINT('Ctrl Pts',(-42.6580847566778,-77.1647690829171,
17.7461949009107));
#46024=CARTESIAN_POINT('Ctrl Pts',(-42.5270162280679,-76.1358663680163,
19.3771917235364));
#46025=CARTESIAN_POINT('Ctrl Pts',(-42.3948798007065,-76.3528431108269,
21.3079390832326));
#46026=CARTESIAN_POINT('Ctrl Pts',(-42.2616851225389,-77.7343788134307,
22.6951866504985));
#46027=CARTESIAN_POINT('Ctrl Pts',(-42.1274243440262,-79.6971490024854,
22.9179776480344));
#46028=CARTESIAN_POINT('Ctrl Pts',(-42.014670143851,-81.0996489509398,22.0396067694999));
#46029=CARTESIAN_POINT('Ctrl Pts',(-41.9239057210112,-81.7167415335571,
20.9138412402982));
#46030=CARTESIAN_POINT('Ctrl Pts',(-41.8783332471008,-81.8242677093701,
20.2893946603941));
#46031=CARTESIAN_POINT('Ctrl Pts',(-41.8555711999267,-81.8248616131743,
19.9678010749981));
#46032=CARTESIAN_POINT('Ctrl Pts',(-56.9957437894396,-81.9300461410118,
19.971749517882));
#46033=CARTESIAN_POINT('Ctrl Pts',(-56.9720878172747,-81.9294289128066,
19.6375261168725));
#46034=CARTESIAN_POINT('Ctrl Pts',(-56.9246413144741,-81.8177633897353,
18.9873413433035));
#46035=CARTESIAN_POINT('Ctrl Pts',(-56.8295978260608,-81.172295314983,17.8084446380066));
#46036=CARTESIAN_POINT('Ctrl Pts',(-56.7100918560198,-79.6886388558644,
16.8738035209148));
#46037=CARTESIAN_POINT('Ctrl Pts',(-56.5658678859323,-77.5795917259262,
17.1083394260631));
#46038=CARTESIAN_POINT('Ctrl Pts',(-56.4207376045591,-76.0708561854358,
18.615883976467));
#46039=CARTESIAN_POINT('Ctrl Pts',(-56.2747745518288,-75.8262259255696,
20.747841123805));
#46040=CARTESIAN_POINT('Ctrl Pts',(-56.1279819285444,-76.973974321702,22.5766823449522));
#46041=CARTESIAN_POINT('Ctrl Pts',(-55.9803900390286,-79.0213695189193,
23.2952423817352));
#46042=CARTESIAN_POINT('Ctrl Pts',(-55.832025105169,-81.0814642752292,22.5765597878218));
#46043=CARTESIAN_POINT('Ctrl Pts',(-55.682917594715,-82.2494586027885,20.7210911241734));
#46044=CARTESIAN_POINT('Ctrl Pts',(-55.5330991431064,-82.0047795818836,
18.5317276122314));
#46045=CARTESIAN_POINT('Ctrl Pts',(-55.3826016766804,-80.4409685466629,
16.9658035999932));
#46046=CARTESIAN_POINT('Ctrl Pts',(-55.2314623577778,-78.233256374022,16.715215318237));
#46047=CARTESIAN_POINT('Ctrl Pts',(-55.0797112113575,-76.3419404793175,
17.9015819532036));
#46048=CARTESIAN_POINT('Ctrl Pts',(-54.9527851585667,-75.7267686910698,
19.6622433798203));
#46049=CARTESIAN_POINT('Ctrl Pts',(-54.8509618033697,-75.9699335874656,
21.0767733443915));
#46050=CARTESIAN_POINT('Ctrl Pts',(-54.7744678880113,-76.4900881076259,
22.0203926993287));
#46051=CARTESIAN_POINT('Ctrl Pts',(-54.6978511000632,-77.2954494492304,
22.7388596335825));
#46052=CARTESIAN_POINT('Ctrl Pts',(-54.5955361546865,-78.626606066821,23.2936701301925));
#46053=CARTESIAN_POINT('Ctrl Pts',(-54.4673860500643,-80.4982210477155,
23.0857086092053));
#46054=CARTESIAN_POINT('Ctrl Pts',(-54.3131881300118,-82.1031550636772,
21.4816044105671));
#46055=CARTESIAN_POINT('Ctrl Pts',(-54.1586231171422,-82.3581618493084,
19.2239374375668));
#46056=CARTESIAN_POINT('Ctrl Pts',(-54.003750320265,-81.1473256829115,17.2932949130607));
#46057=CARTESIAN_POINT('Ctrl Pts',(-53.8485668683044,-78.9932739136752,
16.5418724180722));
#46058=CARTESIAN_POINT('Ctrl Pts',(-53.6931792503979,-76.836159548567,17.2957199364878));
#46059=CARTESIAN_POINT('Ctrl Pts',(-53.5376043604849,-75.6185266026793,
19.2327575977176));
#46060=CARTESIAN_POINT('Ctrl Pts',(-53.3818919303312,-75.874664526356,21.5083040823326));
#46061=CARTESIAN_POINT('Ctrl Pts',(-53.2260876155861,-77.4948156925005,
23.1286340455996));
#46062=CARTESIAN_POINT('Ctrl Pts',(-53.0702387399007,-79.7724813964587,
23.3852583119079));
#46063=CARTESIAN_POINT('Ctrl Pts',(-52.9143921490795,-81.713192088748,22.1657213517522));
#46064=CARTESIAN_POINT('Ctrl Pts',(-52.7585949551581,-82.46980977515,20.0028714955218));
#46065=CARTESIAN_POINT('Ctrl Pts',(-52.602894351696,-81.7132156482904,17.8415191196344));
#46066=CARTESIAN_POINT('Ctrl Pts',(-52.44733732548,-79.7758359678184,16.6246532457464));
#46067=CARTESIAN_POINT('Ctrl Pts',(-52.2919702655199,-77.5052173825921,
16.8810081968058));
#46068=CARTESIAN_POINT('Ctrl Pts',(-52.1368389777891,-75.8923408919337,
18.4947736518063));
#46069=CARTESIAN_POINT('Ctrl Pts',(-51.9819887183747,-75.6380824394838,
20.7579855405843));
#46070=CARTESIAN_POINT('Ctrl Pts',(-51.8274641395511,-76.8479253296823,
22.6818497208179));
#46071=CARTESIAN_POINT('Ctrl Pts',(-51.6733091246767,-78.9882310561524,
23.4297519524038));
#46072=CARTESIAN_POINT('Ctrl Pts',(-51.5195672315392,-81.1221058384755,
22.6819274088254));
#46073=CARTESIAN_POINT('Ctrl Pts',(-51.3662803627253,-82.3205231170056,
20.7723832742744));
#46074=CARTESIAN_POINT('Ctrl Pts',(-51.2134906309633,-82.067536758452,18.5395357722326));
#46075=CARTESIAN_POINT('Ctrl Pts',(-51.0612355077352,-80.4831665052501,
16.9570782370458));
#46076=CARTESIAN_POINT('Ctrl Pts',(-50.9095589525399,-78.2658943169774,
16.7089499791194));
#46077=CARTESIAN_POINT('Ctrl Pts',(-50.7584862188345,-76.3858276880046,
17.8921278081452));
#46078=CARTESIAN_POINT('Ctrl Pts',(-50.6080801931949,-75.6555081289303,
19.9815434149077));
#46079=CARTESIAN_POINT('Ctrl Pts',(-50.4583150157542,-76.3867863899377,
22.0582342796407));
#46080=CARTESIAN_POINT('Ctrl Pts',(-50.3092957305894,-78.2431770442968,
23.2229562447285));
#46081=CARTESIAN_POINT('Ctrl Pts',(-50.1610199298396,-80.4098753634881,
22.97691940353));
#46082=CARTESIAN_POINT('Ctrl Pts',(-50.0135202964699,-81.9422769935299,
21.4416476757106));
#46083=CARTESIAN_POINT('Ctrl Pts',(-49.8668235155934,-82.1816514238649,
19.2974799656789));
#46084=CARTESIAN_POINT('Ctrl Pts',(-49.7209554829974,-81.038468925659,17.4822050937547));
#46085=CARTESIAN_POINT('Ctrl Pts',(-49.5759405288341,-79.0243729605365,
16.7796992026714));
#46086=CARTESIAN_POINT('Ctrl Pts',(-49.4317994982005,-77.0245243396262,
17.4822411066595));
#46087=CARTESIAN_POINT('Ctrl Pts',(-49.2885552045132,-75.9044564152709,
19.2664840098316));
#46088=CARTESIAN_POINT('Ctrl Pts',(-49.1462191456824,-76.1432283129171,
21.3478786801514));
#46089=CARTESIAN_POINT('Ctrl Pts',(-49.0048212758934,-77.6101485651985,
22.813088681206));
#46090=CARTESIAN_POINT('Ctrl Pts',(-48.8487356825073,-79.9029287381131,
23.075400288994));
#46091=CARTESIAN_POINT('Ctrl Pts',(-48.7093468797834,-81.5663232868859,
21.746536954466));
#46092=CARTESIAN_POINT('Ctrl Pts',(-48.5940037608329,-81.9206064075348,
20.1326883641399));
#46093=CARTESIAN_POINT('Ctrl Pts',(-48.5174232874096,-81.741320931239,19.0727142447915));
#46094=CARTESIAN_POINT('Ctrl Pts',(-48.4258458131364,-81.1177007039368,
17.9404149812607));
#46095=CARTESIAN_POINT('Ctrl Pts',(-48.3120022564393,-79.7019158587733,
17.0515806518557));
#46096=CARTESIAN_POINT('Ctrl Pts',(-48.1763524335297,-77.7185967734674,
17.2772440131571));
#46097=CARTESIAN_POINT('Ctrl Pts',(-48.0416796916409,-76.320687388509,18.6793406519538));
#46098=CARTESIAN_POINT('Ctrl Pts',(-47.9079753617284,-76.1027042059027,
20.6332804614806));
#46099=CARTESIAN_POINT('Ctrl Pts',(-47.7752376830806,-77.1433202924972,
22.2846464781002));
#46100=CARTESIAN_POINT('Ctrl Pts',(-47.6434585171334,-78.972990052141,22.9223505322969));
#46101=CARTESIAN_POINT('Ctrl Pts',(-47.5126292328511,-80.7879405549371,
22.2847608704201));
#46102=CARTESIAN_POINT('Ctrl Pts',(-47.3827381427943,-81.8020110648646,
20.6664188218262));
#46103=CARTESIAN_POINT('Ctrl Pts',(-47.2537717088521,-81.5873850261729,
18.7823941819149));
#46104=CARTESIAN_POINT('Ctrl Pts',(-47.1257142248705,-80.2543820614397,
17.452698786342));
#46105=CARTESIAN_POINT('Ctrl Pts',(-46.9985476751261,-78.3961966011715,
17.2455162857473));
#46106=CARTESIAN_POINT('Ctrl Pts',(-46.8722525809472,-76.8250061389063,
18.2353999825299));
#46107=CARTESIAN_POINT('Ctrl Pts',(-46.7468058450621,-76.2178906475949,
19.976571843654));
#46108=CARTESIAN_POINT('Ctrl Pts',(-46.6221857531722,-76.8245123203334,
21.7059764500968));
#46109=CARTESIAN_POINT('Ctrl Pts',(-46.5189980363482,-78.1102171954823,
22.5102013483286));
#46110=CARTESIAN_POINT('Ctrl Pts',(-46.4368404123711,-79.264997126938,22.5717632225066));
#46111=CARTESIAN_POINT('Ctrl Pts',(-46.3549353191113,-80.3771028622425,
22.2550763842303));
#46112=CARTESIAN_POINT('Ctrl Pts',(-46.2666032496695,-81.2889540598721,
21.3384880705053));
#46113=CARTESIAN_POINT('Ctrl Pts',(-46.144898284069,-81.6791110052382,19.6423622368182));
#46114=CARTESIAN_POINT('Ctrl Pts',(-46.0591734169203,-81.1185247625248,
18.4619314156135));
#46115=CARTESIAN_POINT('Ctrl Pts',(-45.9955525435571,-80.4007191749686,
17.9420736696449));
#46116=CARTESIAN_POINT('Ctrl Pts',(-45.9553997199636,-79.9246659480749,
17.6513316937921));
#46117=CARTESIAN_POINT('Ctrl Pts',(-45.8802818055934,-78.8817219091746,
17.3809925802952));
#46118=CARTESIAN_POINT('Ctrl Pts',(-45.7705555090585,-77.3580643432502,
17.9148058039039));
#46119=CARTESIAN_POINT('Ctrl Pts',(-45.651478880851,-76.4308117831266,19.3952080057491));
#46120=CARTESIAN_POINT('Ctrl Pts',(-45.51970485512,-76.642423188315,21.327898472145));
#46121=CARTESIAN_POINT('Ctrl Pts',(-45.3886056079646,-78.2138816873341,
22.5792243900901));
#46122=CARTESIAN_POINT('Ctrl Pts',(-45.2841719635512,-79.7403108235408,
22.3953632331636));
#46123=CARTESIAN_POINT('Ctrl Pts',(-45.1799875089255,-80.9757148217796,
21.6251986126592));
#46124=CARTESIAN_POINT('Ctrl Pts',(-45.0630768128045,-81.7523990234054,
20.0067826286561));
#46125=CARTESIAN_POINT('Ctrl Pts',(-44.9250344935208,-80.8294906995215,
18.0995295298735));
#46126=CARTESIAN_POINT('Ctrl Pts',(-44.8045136744454,-79.1930650736379,
17.4696729318157));
#46127=CARTESIAN_POINT('Ctrl Pts',(-44.701419620499,-77.7364078840939,17.7986961941708));
#46128=CARTESIAN_POINT('Ctrl Pts',(-44.5984229179905,-76.7187699522523,
18.8974867189146));
#46129=CARTESIAN_POINT('Ctrl Pts',(-44.4955825943665,-76.4958138571141,
20.3731005520608));
#46130=CARTESIAN_POINT('Ctrl Pts',(-44.3927708776428,-77.1442359200327,
21.7191405627173));
#46131=CARTESIAN_POINT('Ctrl Pts',(-44.2985803436408,-78.3287975756668,
22.4016406217508));
#46132=CARTESIAN_POINT('Ctrl Pts',(-44.212968657307,-79.5483578860479,22.4006017235312));
#46133=CARTESIAN_POINT('Ctrl Pts',(-44.1359129289841,-80.5369158826798,
21.9250916588476));
#46134=CARTESIAN_POINT('Ctrl Pts',(-44.0716711057434,-81.1071613821891,
21.209794149862));
#46135=CARTESIAN_POINT('Ctrl Pts',(-44.0202796282341,-81.3438226977104,
20.5317985242787));
#46136=CARTESIAN_POINT('Ctrl Pts',(-43.9688671964135,-81.424967756689,19.8178776520423));
#46137=CARTESIAN_POINT('Ctrl Pts',(-43.9045730095602,-81.2211275084576,
18.9256365062025));
#46138=CARTESIAN_POINT('Ctrl Pts',(-43.8273513228911,-80.5359206811645,
18.0651935405777));
#46139=CARTESIAN_POINT('Ctrl Pts',(-43.7500498740938,-79.5443212242324,
17.5887321159173));
#46140=CARTESIAN_POINT('Ctrl Pts',(-43.6597723140765,-78.2581786621976,
17.5864270630418));
#46141=CARTESIAN_POINT('Ctrl Pts',(-43.5563922708837,-76.9708420771708,
18.3903159951276));
#46142=CARTESIAN_POINT('Ctrl Pts',(-43.4397879463254,-76.4046306882061,
20.0093689692673));
#46143=CARTESIAN_POINT('Ctrl Pts',(-43.3228698120996,-76.9711309491329,
21.6305633927173));
#46144=CARTESIAN_POINT('Ctrl Pts',(-43.2055779422275,-78.4300603274151,
22.5488750915416));
#46145=CARTESIAN_POINT('Ctrl Pts',(-43.0878753463866,-80.1489032046835,
22.3562127233884));
#46146=CARTESIAN_POINT('Ctrl Pts',(-42.9697167650604,-81.3775451817227,
21.1294459363969));
#46147=CARTESIAN_POINT('Ctrl Pts',(-42.8510614298393,-81.5740110412663,
19.3969759842311));
#46148=CARTESIAN_POINT('Ctrl Pts',(-42.7318700097782,-80.6433893673584,
17.9132545669706));
#46149=CARTESIAN_POINT('Ctrl Pts',(-42.6121001443425,-78.9824684567483,
17.3306920485745));
#46150=CARTESIAN_POINT('Ctrl Pts',(-42.4917212833099,-77.3125682663215,
17.9134664117972));
#46151=CARTESIAN_POINT('Ctrl Pts',(-42.370679651798,-76.3640214348811,19.4188706488154));
#46152=CARTESIAN_POINT('Ctrl Pts',(-42.2489781115364,-76.5645238873024,
21.1959821363472));
#46153=CARTESIAN_POINT('Ctrl Pts',(-42.1265944138874,-77.8341045341955,
22.4700397556397));
#46154=CARTESIAN_POINT('Ctrl Pts',(-42.0034115172595,-79.6340422101825,
22.6734170894833));
#46155=CARTESIAN_POINT('Ctrl Pts',(-41.9001966362758,-80.9177882354456,
21.8698096826426));
#46156=CARTESIAN_POINT('Ctrl Pts',(-41.817082010737,-81.4823776799116,20.8390969971333));
#46157=CARTESIAN_POINT('Ctrl Pts',(-41.7755178320191,-81.5805519289745,
20.2697706727669));
#46158=CARTESIAN_POINT('Ctrl Pts',(-41.7546186244511,-81.5810972278566,
19.9744962169019));
#46159=CARTESIAN_POINT('Ctrl Pts',(-56.998865393003,-81.8104071381607,19.971749517882));
#46160=CARTESIAN_POINT('Ctrl Pts',(-56.9761215679777,-81.8098137095668,
19.6504133876692));
#46161=CARTESIAN_POINT('Ctrl Pts',(-56.9306422269741,-81.702749946835,19.0272055496801));
#46162=CARTESIAN_POINT('Ctrl Pts',(-56.8393882333594,-81.0832286625891,
17.8952792144066));
#46163=CARTESIAN_POINT('Ctrl Pts',(-56.7246941823819,-79.659154025169,16.9983829421965));
#46164=CARTESIAN_POINT('Ctrl Pts',(-56.5861632252162,-77.6335534097869,
17.2233006398626));
#46165=CARTESIAN_POINT('Ctrl Pts',(-56.4467017882273,-76.1835978989143,
18.6719551219413));
#46166=CARTESIAN_POINT('Ctrl Pts',(-56.3063357852564,-75.9481362494154,
20.7219582178088));
#46167=CARTESIAN_POINT('Ctrl Pts',(-56.1650671343952,-77.0524010984881,
22.4820287706829));
#46168=CARTESIAN_POINT('Ctrl Pts',(-56.022913716882,-79.0240846877592,23.1743286974061));
#46169=CARTESIAN_POINT('Ctrl Pts',(-55.8798883483141,-81.0099417524087,
22.4819069016305));
#46170=CARTESIAN_POINT('Ctrl Pts',(-55.736009170698,-82.1371435389622,20.6919014148508));
#46171=CARTESIAN_POINT('Ctrl Pts',(-55.5912948188564,-81.9011989467447,
18.5773811983794));
#46172=CARTESIAN_POINT('Ctrl Pts',(-55.4457664679998,-80.3895075735084,
17.0631066199702));
#46173=CARTESIAN_POINT('Ctrl Pts',(-55.2994467925014,-78.2525981471427,
16.8201567755944));
#46174=CARTESIAN_POINT('Ctrl Pts',(-55.1523606723563,-76.4194586046196,
17.9695089930655));
#46175=CARTESIAN_POINT('Ctrl Pts',(-55.0291720750146,-75.8221765197523,
19.6778401981353));
#46176=CARTESIAN_POINT('Ctrl Pts',(-54.9302657004888,-76.0582767873485,
21.0517631272575));
#46177=CARTESIAN_POINT('Ctrl Pts',(-54.855911693957,-76.563774636797,21.9689095801494));
#46178=CARTESIAN_POINT('Ctrl Pts',(-54.7813873081152,-77.3470208623382,
22.6677199767267));
#46179=CARTESIAN_POINT('Ctrl Pts',(-54.6817995343713,-78.6425182874698,
23.2077559592215));
#46180=CARTESIAN_POINT('Ctrl Pts',(-54.5569085657542,-80.4660663250115,
23.0055515481889));
#46181=CARTESIAN_POINT('Ctrl Pts',(-54.4064224477222,-82.0323869212294,
21.4408137908159));
#46182=CARTESIAN_POINT('Ctrl Pts',(-54.2553538136249,-82.282138366727,19.2347828818201));
#46183=CARTESIAN_POINT('Ctrl Pts',(-54.1037383696759,-81.0976521492529,
17.3450468644423));
#46184=CARTESIAN_POINT('Ctrl Pts',(-53.9516134654316,-78.9865131673676,
16.6079479997978));
#46185=CARTESIAN_POINT('Ctrl Pts',(-53.799017300736,-76.8685737480114,17.3474746287888));
#46186=CARTESIAN_POINT('Ctrl Pts',(-53.6459896567803,-75.6706931696044,
19.2519276595415));
#46187=CARTESIAN_POINT('Ctrl Pts',(-53.4925710331048,-75.9223549441939,
21.4933728414198));
#46188=CARTESIAN_POINT('Ctrl Pts',(-53.3388026326536,-77.5204065688237,
23.0925152589881));
#46189=CARTESIAN_POINT('Ctrl Pts',(-53.1847265069516,-79.7714109640732,
23.3467986618763));
#46190=CARTESIAN_POINT('Ctrl Pts',(-53.03038548168,-81.6931375902356,22.1399790200489));
#46191=CARTESIAN_POINT('Ctrl Pts',(-52.875823002085,-82.4441600599385,19.9951637320667));
#46192=CARTESIAN_POINT('Ctrl Pts',(-52.7210833439104,-81.6931147568403,
17.847607587344));
#46193=CARTESIAN_POINT('Ctrl Pts',(-52.5662111784277,-79.7652472072559,
16.6359089985643));
#46194=CARTESIAN_POINT('Ctrl Pts',(-52.411251276088,-77.5012356580149,16.8908255535852));
#46195=CARTESIAN_POINT('Ctrl Pts',(-52.256248453475,-75.8897320482582,18.5022380823304));
#46196=CARTESIAN_POINT('Ctrl Pts',(-52.1012476567581,-75.6346189430596,
20.7668255842009));
#46197=CARTESIAN_POINT('Ctrl Pts',(-51.946293812071,-76.8468283649895,22.6957639240306));
#46198=CARTESIAN_POINT('Ctrl Pts',(-51.7914318627055,-78.9959989264195,
23.4475029895662));
#46199=CARTESIAN_POINT('Ctrl Pts',(-51.6367067716067,-81.143023685764,22.6958068198001));
#46200=CARTESIAN_POINT('Ctrl Pts',(-51.4821631962239,-82.3514430242135,
20.7716237421131));
#46201=CARTESIAN_POINT('Ctrl Pts',(-51.3278450629361,-82.0966921870304,
18.5171370441619));
#46202=CARTESIAN_POINT('Ctrl Pts',(-51.173795763927,-80.494660275846,16.9160818675009));
#46203=CARTESIAN_POINT('Ctrl Pts',(-51.0200579736735,-78.2481247248837,
16.6640082062395));
#46204=CARTESIAN_POINT('Ctrl Pts',(-50.8666737295509,-76.3395049302381,
17.8643638570452));
#46205=CARTESIAN_POINT('Ctrl Pts',(-50.713684168159,-75.5963279226902,19.9885708308413));
#46206=CARTESIAN_POINT('Ctrl Pts',(-50.561130291697,-76.3404917399077,22.103826159149));
#46207=CARTESIAN_POINT('Ctrl Pts',(-50.4090511127719,-78.2340315759714,
23.2925880511682));
#46208=CARTESIAN_POINT('Ctrl Pts',(-50.2574850343491,-80.4481760005255,
23.0417916058766));
#46209=CARTESIAN_POINT('Ctrl Pts',(-50.1064690255066,-82.01705159905,21.4708528285098));
#46210=CARTESIAN_POINT('Ctrl Pts',(-49.9560387185426,-82.2630418039423,
19.2728709293431));
#46211=CARTESIAN_POINT('Ctrl Pts',(-49.8062283566168,-81.0898252948096,
17.4088059239318));
#46212=CARTESIAN_POINT('Ctrl Pts',(-49.6570709537323,-79.019024315676,16.68592863221));
#46213=CARTESIAN_POINT('Ctrl Pts',(-49.5085980443133,-76.9595196408508,
17.4088734508976));
#46214=CARTESIAN_POINT('Ctrl Pts',(-49.3608396229039,-75.8040867405457,
19.24850872357));
#46215=CARTESIAN_POINT('Ctrl Pts',(-49.2138236838193,-76.0501675357259,
21.3978373023004));
#46216=CARTESIAN_POINT('Ctrl Pts',(-49.0675767596914,-77.5665861446786,
22.9130985070277));
#46217=CARTESIAN_POINT('Ctrl Pts',(-48.9059614999196,-79.9400679445208,
23.1852360004509));
#46218=CARTESIAN_POINT('Ctrl Pts',(-48.7614602181023,-81.6648094897616,
21.8082179781191));
#46219=CARTESIAN_POINT('Ctrl Pts',(-48.641745504212,-82.0326853928027,20.1333807208566));
#46220=CARTESIAN_POINT('Ctrl Pts',(-48.5622130344089,-81.8465385109611,
19.0326778475393));
#46221=CARTESIAN_POINT('Ctrl Pts',(-48.4670622745342,-81.1987085058851,
17.8562669615047));
#46222=CARTESIAN_POINT('Ctrl Pts',(-48.3486693000866,-79.7268341045547,
16.9318783271684));
#46223=CARTESIAN_POINT('Ctrl Pts',(-48.2074855512855,-77.6628755974866,
17.1663816685728));
#46224=CARTESIAN_POINT('Ctrl Pts',(-48.0672023078574,-76.206752176544,18.626431849987));
#46225=CARTESIAN_POINT('Ctrl Pts',(-47.927830219219,-75.9792981345661,20.6628912290644));
#46226=CARTESIAN_POINT('Ctrl Pts',(-47.7893778161085,-77.0643886294908,
22.3852565245146));
#46227=CARTESIAN_POINT('Ctrl Pts',(-47.6518515237459,-78.9735990241534,
23.0508787165266));
#46228=CARTESIAN_POINT('Ctrl Pts',(-47.5152556014389,-80.8684432520523,
22.3853788812134));
#46229=CARTESIAN_POINT('Ctrl Pts',(-47.3795921088708,-81.9276134623547,
20.6952758178572));
#46230=CARTESIAN_POINT('Ctrl Pts',(-47.2448609079158,-81.7034807862736,
18.7270982413631));
#46231=CARTESIAN_POINT('Ctrl Pts',(-47.1110596886693,-80.3107425715779,
17.3377494473466));
#46232=CARTESIAN_POINT('Ctrl Pts',(-46.9781840026693,-78.3691181398569,
17.1212491527646));
#46233=CARTESIAN_POINT('Ctrl Pts',(-46.8462272430603,-76.7274568500113,
18.1555514656259));
#46234=CARTESIAN_POINT('Ctrl Pts',(-46.7151806507337,-76.0932466642441,
19.9745644839421));
#46235=CARTESIAN_POINT('Ctrl Pts',(-46.5850332874596,-76.72689365866,21.7807592120224));
#46236=CARTESIAN_POINT('Ctrl Pts',(-46.4773155913697,-78.0692304834685,
22.6203028484064));
#46237=CARTESIAN_POINT('Ctrl Pts',(-46.3915770038462,-79.2743999206746,
22.6845333353118));
#46238=CARTESIAN_POINT('Ctrl Pts',(-46.306125933356,-80.4347163011863,22.3540877308873));
#46239=CARTESIAN_POINT('Ctrl Pts',(-46.2140165472685,-81.3855756228331,
21.3981264795911));
#46240=CARTESIAN_POINT('Ctrl Pts',(-46.0871761509613,-81.7920886092443,
19.6302877304961));
#46241=CARTESIAN_POINT('Ctrl Pts',(-45.9979124562317,-81.2080139528857,
18.4010685232934));
#46242=CARTESIAN_POINT('Ctrl Pts',(-45.931706785465,-80.4609863771443,17.8600692258404));
#46243=CARTESIAN_POINT('Ctrl Pts',(-45.8899254264441,-79.9656081265692,
17.5575209097683));
#46244=CARTESIAN_POINT('Ctrl Pts',(-45.8118000032237,-78.880763795498,17.2764338892227));
#46245=CARTESIAN_POINT('Ctrl Pts',(-45.6978306326569,-77.2975836321059,
17.8314065963964));
#46246=CARTESIAN_POINT('Ctrl Pts',(-45.5742396517875,-76.3354201599197,
19.3681907346036));
#46247=CARTESIAN_POINT('Ctrl Pts',(-45.437706343548,-76.5552758080846,21.3715656944865));
#46248=CARTESIAN_POINT('Ctrl Pts',(-45.3020562393531,-78.1821308742347,
22.6659223685449));
#46249=CARTESIAN_POINT('Ctrl Pts',(-45.1941987227426,-79.758928297719,22.475534026443));
#46250=CARTESIAN_POINT('Ctrl Pts',(-45.0866996199815,-81.0338356970261,
21.6807000396746));
#46251=CARTESIAN_POINT('Ctrl Pts',(-44.9662578644687,-81.8333475233177,
20.012518703382));
#46252=CARTESIAN_POINT('Ctrl Pts',(-44.8243750512167,-80.8834891862673,
18.0522457056093));
#46253=CARTESIAN_POINT('Ctrl Pts',(-44.7007996247099,-79.204627825654,17.4066536628875));
#46254=CARTESIAN_POINT('Ctrl Pts',(-44.5952423985192,-77.7129206082217,
17.7439551046314));
#46255=CARTESIAN_POINT('Ctrl Pts',(-44.4900223228441,-76.6730225954323,
18.8674759604783));
#46256=CARTESIAN_POINT('Ctrl Pts',(-44.3851107070103,-76.4459242852341,
20.3731595407077));
#46257=CARTESIAN_POINT('Ctrl Pts',(-44.280478717402,-77.1066399045476,21.7436998539951));
#46258=CARTESIAN_POINT('Ctrl Pts',(-44.1847949217249,-78.3107241896412,
22.4370140832109));
#46259=CARTESIAN_POINT('Ctrl Pts',(-44.0979705969536,-79.5480359338008,
22.4357585099148));
#46260=CARTESIAN_POINT('Ctrl Pts',(-44.0199391969229,-80.5493767638303,
21.9538965049427));
#46261=CARTESIAN_POINT('Ctrl Pts',(-43.9549950707645,-81.1260138276735,
21.230332507434));
#46262=CARTESIAN_POINT('Ctrl Pts',(-43.9030819779796,-81.3650788043183,
20.5453498510557));
#46263=CARTESIAN_POINT('Ctrl Pts',(-43.8511952002441,-81.4469675514213,
19.8246440252031));
#46264=CARTESIAN_POINT('Ctrl Pts',(-43.786381545381,-81.2412693616971,18.9250357363984));
#46265=CARTESIAN_POINT('Ctrl Pts',(-43.7086639057346,-80.5513181773471,
18.058939887935));
#46266=CARTESIAN_POINT('Ctrl Pts',(-43.6309915965552,-79.554575354439,17.5802369898606));
#46267=CARTESIAN_POINT('Ctrl Pts',(-43.5404114400028,-78.2638755524742,
17.5781557379155));
#46268=CARTESIAN_POINT('Ctrl Pts',(-43.4369226415031,-76.9748964799918,
18.3837836136963));
#46269=CARTESIAN_POINT('Ctrl Pts',(-43.3204955018513,-76.409902299744,20.0015897439));
#46270=CARTESIAN_POINT('Ctrl Pts',(-43.2040204721867,-76.9752002181154,
21.6172377254714));
#46271=CARTESIAN_POINT('Ctrl Pts',(-43.0874525410452,-78.4262949071933,
22.5297854402615));
#46272=CARTESIAN_POINT('Ctrl Pts',(-42.9707470684933,-80.1313821068561,
22.3379694555197));
#46273=CARTESIAN_POINT('Ctrl Pts',(-42.8538596468785,-81.3469559099921,
21.1232848086745));
#46274=CARTESIAN_POINT('Ctrl Pts',(-42.7367469025614,-81.5402924255104,
19.4123612569526));
#46275=CARTESIAN_POINT('Ctrl Pts',(-42.6193646471204,-80.6227499332965,
17.950746393619));
#46276=CARTESIAN_POINT('Ctrl Pts',(-42.5016723128577,-78.9894841983059,
17.3785603509998));
#46277=CARTESIAN_POINT('Ctrl Pts',(-42.3836228189166,-77.3512439815465,
17.9509054109146));
#46278=CARTESIAN_POINT('Ctrl Pts',(-42.2651858183516,-76.4228942839963,
19.4252147114051));
#46279=CARTESIAN_POINT('Ctrl Pts',(-42.1462969423314,-76.6193425219703,
21.1617531840419));
#46280=CARTESIAN_POINT('Ctrl Pts',(-42.0269611323496,-77.8579790787978,
22.4041645790426));
#46281=CARTESIAN_POINT('Ctrl Pts',(-41.9070542715169,-79.6104428558897,
22.601547445429));
#46282=CARTESIAN_POINT('Ctrl Pts',(-41.8067886921112,-80.8577927602762,
21.8204122976217));
#46283=CARTESIAN_POINT('Ctrl Pts',(-41.7260879027667,-81.4058116777841,
20.8193752889488));
#46284=CARTESIAN_POINT('Ctrl Pts',(-41.6858137213157,-81.5009183081234,
20.2675948162325));
#46285=CARTESIAN_POINT('Ctrl Pts',(-41.6655045384048,-81.5014482121737,
19.980656523783));
#46286=CARTESIAN_POINT('Ctrl Pts',(-56.9777992245686,-81.7947852592049,
19.6770343419626));
#46287=CARTESIAN_POINT('Ctrl Pts',(-56.9620765160291,-81.7719278227084,
19.4593650843275));
#46288=CARTESIAN_POINT('Ctrl Pts',(-56.923598666368,-81.6549313743044,18.9398363132408));
#46289=CARTESIAN_POINT('Ctrl Pts',(-56.8393882333594,-81.0832286625891,
17.8952792144066));
#46290=CARTESIAN_POINT('Ctrl Pts',(-56.7246941823819,-79.659154025169,16.9983829421965));
#46291=CARTESIAN_POINT('Ctrl Pts',(-56.5861632252162,-77.6335534097869,
17.2233006398626));
#46292=CARTESIAN_POINT('Ctrl Pts',(-56.4467017882273,-76.1835978989143,
18.6719551219413));
#46293=CARTESIAN_POINT('Ctrl Pts',(-56.3063357852564,-75.9481362494154,
20.7219582178088));
#46294=CARTESIAN_POINT('Ctrl Pts',(-56.1650671343952,-77.0524010984881,
22.4820287706829));
#46295=CARTESIAN_POINT('Ctrl Pts',(-56.022913716882,-79.0240846877592,23.1743286974061));
#46296=CARTESIAN_POINT('Ctrl Pts',(-55.8798883483141,-81.0099417524087,
22.4819069016305));
#46297=CARTESIAN_POINT('Ctrl Pts',(-55.736009170698,-82.1371435389622,20.6919014148508));
#46298=CARTESIAN_POINT('Ctrl Pts',(-55.5912948188564,-81.9011989467447,
18.5773811983794));
#46299=CARTESIAN_POINT('Ctrl Pts',(-55.4457664679998,-80.3895075735084,
17.0631066199702));
#46300=CARTESIAN_POINT('Ctrl Pts',(-55.2994467925014,-78.2525981471427,
16.8201567755944));
#46301=CARTESIAN_POINT('Ctrl Pts',(-55.1523606723563,-76.4194586046196,
17.9695089930655));
#46302=CARTESIAN_POINT('Ctrl Pts',(-55.0291720750146,-75.8221765197523,
19.6778401981353));
#46303=CARTESIAN_POINT('Ctrl Pts',(-54.9302657004888,-76.0582767873485,
21.0517631272575));
#46304=CARTESIAN_POINT('Ctrl Pts',(-54.855911693957,-76.563774636797,21.9689095801494));
#46305=CARTESIAN_POINT('Ctrl Pts',(-54.7813873081152,-77.3470208623382,
22.6677199767267));
#46306=CARTESIAN_POINT('Ctrl Pts',(-54.6817995343713,-78.6425182874698,
23.2077559592215));
#46307=CARTESIAN_POINT('Ctrl Pts',(-54.5569085657542,-80.4660663250115,
23.0055515481889));
#46308=CARTESIAN_POINT('Ctrl Pts',(-54.4064224477222,-82.0323869212294,
21.4408137908159));
#46309=CARTESIAN_POINT('Ctrl Pts',(-54.2553538136249,-82.282138366727,19.2347828818201));
#46310=CARTESIAN_POINT('Ctrl Pts',(-54.1037383696759,-81.0976521492529,
17.3450468644423));
#46311=CARTESIAN_POINT('Ctrl Pts',(-53.9516134654316,-78.9865131673676,
16.6079479997978));
#46312=CARTESIAN_POINT('Ctrl Pts',(-53.799017300736,-76.8685737480114,17.3474746287888));
#46313=CARTESIAN_POINT('Ctrl Pts',(-53.6459896567803,-75.6706931696044,
19.2519276595415));
#46314=CARTESIAN_POINT('Ctrl Pts',(-53.4925710331048,-75.9223549441939,
21.4933728414198));
#46315=CARTESIAN_POINT('Ctrl Pts',(-53.3388026326536,-77.5204065688237,
23.0925152589881));
#46316=CARTESIAN_POINT('Ctrl Pts',(-53.1847265069516,-79.7714109640732,
23.3467986618763));
#46317=CARTESIAN_POINT('Ctrl Pts',(-53.03038548168,-81.6931375902356,22.1399790200489));
#46318=CARTESIAN_POINT('Ctrl Pts',(-52.875823002085,-82.4441600599385,19.9951637320667));
#46319=CARTESIAN_POINT('Ctrl Pts',(-52.7210833439104,-81.6931147568403,
17.847607587344));
#46320=CARTESIAN_POINT('Ctrl Pts',(-52.5662111784277,-79.7652472072559,
16.6359089985643));
#46321=CARTESIAN_POINT('Ctrl Pts',(-52.411251276088,-77.5012356580149,16.8908255535852));
#46322=CARTESIAN_POINT('Ctrl Pts',(-52.256248453475,-75.8897320482582,18.5022380823304));
#46323=CARTESIAN_POINT('Ctrl Pts',(-52.1012476567581,-75.6346189430596,
20.7668255842009));
#46324=CARTESIAN_POINT('Ctrl Pts',(-51.946293812071,-76.8468283649895,22.6957639240306));
#46325=CARTESIAN_POINT('Ctrl Pts',(-51.7914318627055,-78.9959989264195,
23.4475029895662));
#46326=CARTESIAN_POINT('Ctrl Pts',(-51.6367067716067,-81.143023685764,22.6958068198001));
#46327=CARTESIAN_POINT('Ctrl Pts',(-51.4821631962239,-82.3514430242135,
20.7716237421131));
#46328=CARTESIAN_POINT('Ctrl Pts',(-51.3278450629361,-82.0966921870304,
18.5171370441619));
#46329=CARTESIAN_POINT('Ctrl Pts',(-51.173795763927,-80.494660275846,16.9160818675009));
#46330=CARTESIAN_POINT('Ctrl Pts',(-51.0200579736735,-78.2481247248837,
16.6640082062395));
#46331=CARTESIAN_POINT('Ctrl Pts',(-50.8666737295509,-76.3395049302381,
17.8643638570452));
#46332=CARTESIAN_POINT('Ctrl Pts',(-50.713684168159,-75.5963279226902,19.9885708308413));
#46333=CARTESIAN_POINT('Ctrl Pts',(-50.561130291697,-76.3404917399077,22.103826159149));
#46334=CARTESIAN_POINT('Ctrl Pts',(-50.4090511127719,-78.2340315759714,
23.2925880511682));
#46335=CARTESIAN_POINT('Ctrl Pts',(-50.2574850343491,-80.4481760005255,
23.0417916058766));
#46336=CARTESIAN_POINT('Ctrl Pts',(-50.1064690255066,-82.01705159905,21.4708528285098));
#46337=CARTESIAN_POINT('Ctrl Pts',(-49.9560387185426,-82.2630418039423,
19.2728709293431));
#46338=CARTESIAN_POINT('Ctrl Pts',(-49.8062283566168,-81.0898252948096,
17.4088059239318));
#46339=CARTESIAN_POINT('Ctrl Pts',(-49.6570709537323,-79.019024315676,16.68592863221));
#46340=CARTESIAN_POINT('Ctrl Pts',(-49.5085980443133,-76.9595196408508,
17.4088734508976));
#46341=CARTESIAN_POINT('Ctrl Pts',(-49.3608396229039,-75.8040867405457,
19.24850872357));
#46342=CARTESIAN_POINT('Ctrl Pts',(-49.2138236838193,-76.0501675357259,
21.3978373023004));
#46343=CARTESIAN_POINT('Ctrl Pts',(-49.0675767596914,-77.5665861446786,
22.9130985070277));
#46344=CARTESIAN_POINT('Ctrl Pts',(-48.9059614999196,-79.9400679445208,
23.1852360004509));
#46345=CARTESIAN_POINT('Ctrl Pts',(-48.7614602181023,-81.6648094897616,
21.8082179781191));
#46346=CARTESIAN_POINT('Ctrl Pts',(-48.641745504212,-82.0326853928027,20.1333807208566));
#46347=CARTESIAN_POINT('Ctrl Pts',(-48.5622130344089,-81.8465385109611,
19.0326778475393));
#46348=CARTESIAN_POINT('Ctrl Pts',(-48.4670622745342,-81.1987085058851,
17.8562669615047));
#46349=CARTESIAN_POINT('Ctrl Pts',(-48.3486693000866,-79.7268341045547,
16.9318783271684));
#46350=CARTESIAN_POINT('Ctrl Pts',(-48.2074855512855,-77.6628755974866,
17.1663816685728));
#46351=CARTESIAN_POINT('Ctrl Pts',(-48.0672023078574,-76.206752176544,18.626431849987));
#46352=CARTESIAN_POINT('Ctrl Pts',(-47.927830219219,-75.9792981345661,20.6628912290644));
#46353=CARTESIAN_POINT('Ctrl Pts',(-47.7893778161085,-77.0643886294908,
22.3852565245146));
#46354=CARTESIAN_POINT('Ctrl Pts',(-47.6518515237459,-78.9735990241534,
23.0508787165266));
#46355=CARTESIAN_POINT('Ctrl Pts',(-47.5152556014389,-80.8684432520523,
22.3853788812134));
#46356=CARTESIAN_POINT('Ctrl Pts',(-47.3795921088708,-81.9276134623547,
20.6952758178572));
#46357=CARTESIAN_POINT('Ctrl Pts',(-47.2448609079158,-81.7034807862736,
18.7270982413631));
#46358=CARTESIAN_POINT('Ctrl Pts',(-47.1110596886693,-80.3107425715779,
17.3377494473466));
#46359=CARTESIAN_POINT('Ctrl Pts',(-46.9781840026693,-78.3691181398569,
17.1212491527646));
#46360=CARTESIAN_POINT('Ctrl Pts',(-46.8462272430603,-76.7274568500113,
18.1555514656259));
#46361=CARTESIAN_POINT('Ctrl Pts',(-46.7151806507337,-76.0932466642441,
19.9745644839421));
#46362=CARTESIAN_POINT('Ctrl Pts',(-46.5850332874596,-76.72689365866,21.7807592120224));
#46363=CARTESIAN_POINT('Ctrl Pts',(-46.4773155913697,-78.0692304834685,
22.6203028484064));
#46364=CARTESIAN_POINT('Ctrl Pts',(-46.3915770038462,-79.2743999206746,
22.6845333353118));
#46365=CARTESIAN_POINT('Ctrl Pts',(-46.306125933356,-80.4347163011863,22.3540877308873));
#46366=CARTESIAN_POINT('Ctrl Pts',(-46.2140165472685,-81.3855756228331,
21.3981264795911));
#46367=CARTESIAN_POINT('Ctrl Pts',(-46.0871761509613,-81.7920886092443,
19.6302877304961));
#46368=CARTESIAN_POINT('Ctrl Pts',(-45.9979124562317,-81.2080139528857,
18.4010685232934));
#46369=CARTESIAN_POINT('Ctrl Pts',(-45.931706785465,-80.4609863771443,17.8600692258404));
#46370=CARTESIAN_POINT('Ctrl Pts',(-45.8899254264441,-79.9656081265692,
17.5575209097683));
#46371=CARTESIAN_POINT('Ctrl Pts',(-45.8118000032237,-78.880763795498,17.2764338892227));
#46372=CARTESIAN_POINT('Ctrl Pts',(-45.6978306326569,-77.2975836321059,
17.8314065963964));
#46373=CARTESIAN_POINT('Ctrl Pts',(-45.5742396517875,-76.3354201599197,
19.3681907346036));
#46374=CARTESIAN_POINT('Ctrl Pts',(-45.437706343548,-76.5552758080846,21.3715656944865));
#46375=CARTESIAN_POINT('Ctrl Pts',(-45.3020562393531,-78.1821308742347,
22.6659223685449));
#46376=CARTESIAN_POINT('Ctrl Pts',(-45.1941987227426,-79.758928297719,22.475534026443));
#46377=CARTESIAN_POINT('Ctrl Pts',(-45.0866996199815,-81.0338356970261,
21.6807000396746));
#46378=CARTESIAN_POINT('Ctrl Pts',(-44.9662578644687,-81.8333475233177,
20.012518703382));
#46379=CARTESIAN_POINT('Ctrl Pts',(-44.8243750512167,-80.8834891862673,
18.0522457056093));
#46380=CARTESIAN_POINT('Ctrl Pts',(-44.7007996247099,-79.204627825654,17.4066536628875));
#46381=CARTESIAN_POINT('Ctrl Pts',(-44.5952423985192,-77.7129206082217,
17.7439551046314));
#46382=CARTESIAN_POINT('Ctrl Pts',(-44.4900223228441,-76.6730225954323,
18.8674759604783));
#46383=CARTESIAN_POINT('Ctrl Pts',(-44.3851107070103,-76.4459242852341,
20.3731595407077));
#46384=CARTESIAN_POINT('Ctrl Pts',(-44.280478717402,-77.1066399045476,21.7436998539951));
#46385=CARTESIAN_POINT('Ctrl Pts',(-44.1847949217249,-78.3107241896412,
22.4370140832109));
#46386=CARTESIAN_POINT('Ctrl Pts',(-44.0979705969536,-79.5480359338008,
22.4357585099148));
#46387=CARTESIAN_POINT('Ctrl Pts',(-44.0199391969229,-80.5493767638303,
21.9538965049427));
#46388=CARTESIAN_POINT('Ctrl Pts',(-43.9549950707645,-81.1260138276735,
21.230332507434));
#46389=CARTESIAN_POINT('Ctrl Pts',(-43.9030819779796,-81.3650788043183,
20.5453498510557));
#46390=CARTESIAN_POINT('Ctrl Pts',(-43.8511952002441,-81.4469675514213,
19.8246440252031));
#46391=CARTESIAN_POINT('Ctrl Pts',(-43.786381545381,-81.2412693616971,18.9250357363984));
#46392=CARTESIAN_POINT('Ctrl Pts',(-43.7086639057346,-80.5513181773471,
18.058939887935));
#46393=CARTESIAN_POINT('Ctrl Pts',(-43.6309915965552,-79.554575354439,17.5802369898606));
#46394=CARTESIAN_POINT('Ctrl Pts',(-43.5404114400028,-78.2638755524742,
17.5781557379155));
#46395=CARTESIAN_POINT('Ctrl Pts',(-43.4369226415031,-76.9748964799918,
18.3837836136963));
#46396=CARTESIAN_POINT('Ctrl Pts',(-43.3204955018513,-76.409902299744,20.0015897439));
#46397=CARTESIAN_POINT('Ctrl Pts',(-43.2040204721867,-76.9752002181154,
21.6172377254714));
#46398=CARTESIAN_POINT('Ctrl Pts',(-43.0874525410452,-78.4262949071933,
22.5297854402615));
#46399=CARTESIAN_POINT('Ctrl Pts',(-42.9707470684933,-80.1313821068561,
22.3379694555197));
#46400=CARTESIAN_POINT('Ctrl Pts',(-42.8538596468785,-81.3469559099921,
21.1232848086745));
#46401=CARTESIAN_POINT('Ctrl Pts',(-42.7367469025614,-81.5402924255104,
19.4123612569526));
#46402=CARTESIAN_POINT('Ctrl Pts',(-42.6193646471204,-80.6227499332965,
17.950746393619));
#46403=CARTESIAN_POINT('Ctrl Pts',(-42.5016723128577,-78.9894841983059,
17.3785603509998));
#46404=CARTESIAN_POINT('Ctrl Pts',(-42.3836228189166,-77.3512439815465,
17.9509054109146));
#46405=CARTESIAN_POINT('Ctrl Pts',(-42.2651858183516,-76.4228942839963,
19.4252147114051));
#46406=CARTESIAN_POINT('Ctrl Pts',(-42.1462969423314,-76.6193425219703,
21.1617531840419));
#46407=CARTESIAN_POINT('Ctrl Pts',(-42.0269611323496,-77.8579790787978,
22.4041645790426));
#46408=CARTESIAN_POINT('Ctrl Pts',(-41.9070542715169,-79.6104428558897,
22.601547445429));
#46409=CARTESIAN_POINT('Ctrl Pts',(-41.8067886921112,-80.8577927602762,
21.8204122976217));
#46410=CARTESIAN_POINT('Ctrl Pts',(-41.7265845261587,-81.4024392322866,
20.8255355557661));
#46411=CARTESIAN_POINT('Ctrl Pts',(-41.6868051036148,-81.4985501065725,
20.281169425713));
#46412=CARTESIAN_POINT('Ctrl Pts',(-41.667003992989,-81.5013236368607,20.0018258382291));
#46413=CARTESIAN_POINT('',(0.,0.,0.));
#46414=CARTESIAN_POINT('Origin',(-20.1,0.,0.));
#46415=CARTESIAN_POINT('',(-25.862836477965,-3.93796551936703,0.00241968030858936));
#46416=CARTESIAN_POINT('',(-26.046163522035,-3.93691440463921,0.00389705969986015));
#46417=CARTESIAN_POINT('',(-20.1,-3.933,-4.81653586104654E-16));
#46418=CARTESIAN_POINT('',(-26.267,1.75076268474097,3.52556565592089));
#46419=CARTESIAN_POINT('Ctrl Pts',(-25.862836477965,-3.93796551936703,0.00241968030858936));
#46420=CARTESIAN_POINT('Ctrl Pts',(-25.8692092928874,-3.93880098183899,
0.127947404661549));
#46421=CARTESIAN_POINT('Ctrl Pts',(-25.8755821078097,-3.93332319567765,
0.253396721851654));
#46422=CARTESIAN_POINT('Ctrl Pts',(-25.881954922732,-3.92129417144253,0.378208920623738));
#46423=CARTESIAN_POINT('Ctrl Pts',(-25.948213931562,-3.79622679811926,1.67589803937646));
#46424=CARTESIAN_POINT('Ctrl Pts',(-26.014472940392,-2.96296803864307,2.90471440911298));
#46425=CARTESIAN_POINT('Ctrl Pts',(-26.080731949222,-1.80365763965045,3.50203017167187));
#46426=CARTESIAN_POINT('Ctrl Pts',(-26.1428212994813,-0.717302279173672,
4.06175704129799));
#46427=CARTESIAN_POINT('Ctrl Pts',(-26.2049106497407,0.655359278582525,
4.066962738484));
#46428=CARTESIAN_POINT('Ctrl Pts',(-26.267,1.75283089415091,3.52826931739086));
#46429=CARTESIAN_POINT('',(-26.267,-1.74869447533124,3.52286199445082));
#46430=CARTESIAN_POINT('Origin',(-26.267,0.,0.));
#46431=CARTESIAN_POINT('Ctrl Pts',(-26.267,-1.74869447533123,3.52286199445082));
#46432=CARTESIAN_POINT('Ctrl Pts',(-26.20074099117,-2.92199812251929,2.94045212175197));
#46433=CARTESIAN_POINT('Ctrl Pts',(-26.13448198234,-3.77113385184886,1.73058568782258));
#46434=CARTESIAN_POINT('Ctrl Pts',(-26.06822297351,-3.91479953860179,0.43684538414918));
#46435=CARTESIAN_POINT('Ctrl Pts',(-26.0608698230183,-3.93074296175041,
0.29327144125381));
#46436=CARTESIAN_POINT('Ctrl Pts',(-26.0535166725267,-3.93799806875422,
0.148664537846095));
#46437=CARTESIAN_POINT('Ctrl Pts',(-26.046163522035,-3.93691440463921,0.00389705969986015));
#46438=CARTESIAN_POINT('Origin',(-20.1,0.,0.));
#46439=CARTESIAN_POINT('',(-24.612836477965,-3.92791610626173,0.00232109521066254));
#46440=CARTESIAN_POINT('',(-24.796163522035,-3.92757907140906,0.00208605505030474));
#46441=CARTESIAN_POINT('',(-20.1,-3.933,-4.81653586104654E-16));
#46442=CARTESIAN_POINT('Ctrl Pts',(-24.612836477965,-3.92791610626173,0.00232109521066254));
#46443=CARTESIAN_POINT('Ctrl Pts',(-24.6383219065741,-3.9306200668013,0.507662989981787));
#46444=CARTESIAN_POINT('Ctrl Pts',(-24.6638073351831,-3.84018781632386,
1.01207323610777));
#46445=CARTESIAN_POINT('Ctrl Pts',(-24.6892927637922,-3.65215730231515,
1.47701096116609));
#46446=CARTESIAN_POINT('Ctrl Pts',(-24.7555517726221,-3.16330087854708,
2.68579239084588));
#46447=CARTESIAN_POINT('Ctrl Pts',(-24.8218107814521,-2.01474203513748,
3.62776458934148));
#46448=CARTESIAN_POINT('Ctrl Pts',(-24.8880697902821,-0.733655209919689,
3.87059482446554));
#46449=CARTESIAN_POINT('Ctrl Pts',(-24.9543287991121,0.547431615298105,
4.1134250595896));
#46450=CARTESIAN_POINT('Ctrl Pts',(-25.0205878079421,1.96104642232409,3.65711333134211));
#46451=CARTESIAN_POINT('Ctrl Pts',(-25.0868468167721,2.8583382289552,2.71105327307234));
#46452=CARTESIAN_POINT('Ctrl Pts',(-25.1531058256021,3.7556300355863,1.76499321480257));
#46453=CARTESIAN_POINT('Ctrl Pts',(-25.2193648344321,4.13659884182251,0.329184826510518));
#46454=CARTESIAN_POINT('Ctrl Pts',(-25.2856238432621,3.82640530464537,-0.937248424257726));
#46455=CARTESIAN_POINT('Ctrl Pts',(-25.3518828520921,3.51621176746824,-2.20368167502597));
#46456=CARTESIAN_POINT('Ctrl Pts',(-25.4181418609221,2.51485588687775,-3.30073978827041));
#46457=CARTESIAN_POINT('Ctrl Pts',(-25.4844008697521,1.28190902568355,-3.72506985025129));
#46458=CARTESIAN_POINT('Ctrl Pts',(-25.5506598785821,0.0489621644893422,
-4.14939991223217));
#46459=CARTESIAN_POINT('Ctrl Pts',(-25.616918887412,-1.41557567730859,-3.90100192294949));
#46460=CARTESIAN_POINT('Ctrl Pts',(-25.683177896242,-2.43940660462237,-3.0935219944237));
#46461=CARTESIAN_POINT('Ctrl Pts',(-25.7430640901497,-3.3647651109516,-2.36370577123936));
#46462=CARTESIAN_POINT('Ctrl Pts',(-25.8029502840574,-3.9301145668118,-1.17718112922547));
#46463=CARTESIAN_POINT('Ctrl Pts',(-25.862836477965,-3.93796551936703,0.00241968030858936));
#46464=CARTESIAN_POINT('Ctrl Pts',(-26.046163522035,-3.93691440463921,0.00389705969986015));
#46465=CARTESIAN_POINT('Ctrl Pts',(-25.9872576636967,-3.92823320534685,
-1.15583067459948));
#46466=CARTESIAN_POINT('Ctrl Pts',(-25.9283518053584,-3.38440620529298,
-2.32586339218745));
#46467=CARTESIAN_POINT('Ctrl Pts',(-25.86944594702,-2.48513760513297,-3.05769982285182));
#46468=CARTESIAN_POINT('Ctrl Pts',(-25.80318693819,-1.47361434073496,-3.88089055276197));
#46469=CARTESIAN_POINT('Ctrl Pts',(-25.73692792936,-0.0123721677626969,
-4.14965783916484));
#46470=CARTESIAN_POINT('Ctrl Pts',(-25.6706689205301,1.22684276968273,-3.74329298057656));
#46471=CARTESIAN_POINT('Ctrl Pts',(-25.6044099117001,2.46605770712816,-3.33692812198827));
#46472=CARTESIAN_POINT('Ctrl Pts',(-25.5381509028701,3.48324540904674,-2.25543111840884));
#46473=CARTESIAN_POINT('Ctrl Pts',(-25.4718918940401,3.81205929712905,-0.993876849486107));
#46474=CARTESIAN_POINT('Ctrl Pts',(-25.4056328852101,4.14087318521135,0.267677419436621));
#46475=CARTESIAN_POINT('Ctrl Pts',(-25.3393738763801,3.78131325945737,1.70928895370264));
#46476=CARTESIAN_POINT('Ctrl Pts',(-25.2731148675501,2.89813926393057,2.66858937313117));
#46477=CARTESIAN_POINT('Ctrl Pts',(-25.2068558587201,2.01496526840376,3.6278897925597));
#46478=CARTESIAN_POINT('Ctrl Pts',(-25.1405968498901,0.608177203104113,
4.10487909715074));
#46479=CARTESIAN_POINT('Ctrl Pts',(-25.0743378410601,-0.67637689196117,
3.88097217602644));
#46480=CARTESIAN_POINT('Ctrl Pts',(-25.0080788322301,-1.96093098702646,
3.65706525490214));
#46481=CARTESIAN_POINT('Ctrl Pts',(-24.9418198234001,-3.12325111185738,
2.73226210806249));
#46482=CARTESIAN_POINT('Ctrl Pts',(-24.8755608145702,-3.62991379199177,
1.53086062077391));
#46483=CARTESIAN_POINT('Ctrl Pts',(-24.8490950503918,-3.83228951790751,
1.0509861251));
#46484=CARTESIAN_POINT('Ctrl Pts',(-24.8226292862134,-3.93005938637917,
0.526982173100531));
#46485=CARTESIAN_POINT('Ctrl Pts',(-24.796163522035,-3.92757907140906,0.00208605505030474));
#46486=CARTESIAN_POINT('Origin',(-20.1,0.,0.));
#46487=CARTESIAN_POINT('',(-23.362836477965,-3.92954087356332,-0.00313358730535757));
#46488=CARTESIAN_POINT('',(-23.546163522035,-3.93003375797999,-0.00328548955642192));
#46489=CARTESIAN_POINT('',(-20.1,-3.933,-4.81653586104654E-16));
#46490=CARTESIAN_POINT('Ctrl Pts',(-23.362836477965,-3.92954087356332,-0.00313358730535757));
#46491=CARTESIAN_POINT('Ctrl Pts',(-23.4074345202608,-3.92297089886225,
0.880266467358495));
#46492=CARTESIAN_POINT('Ctrl Pts',(-23.4520325625565,-3.62843124950771,
1.76763631385351));
#46493=CARTESIAN_POINT('Ctrl Pts',(-23.4966306048523,-3.0816991297842,2.45416793101582));
#46494=CARTESIAN_POINT('Ctrl Pts',(-23.5628896136823,-2.26942292922431,
3.47414329634622));
#46495=CARTESIAN_POINT('Ctrl Pts',(-23.6291486225123,-0.900486241088972,
4.05081158553528));
#46496=CARTESIAN_POINT('Ctrl Pts',(-23.6954076313422,0.39677869711984,3.91948657984679));
#46497=CARTESIAN_POINT('Ctrl Pts',(-23.7616666401722,1.69404363532865,3.78816157415829));
#46498=CARTESIAN_POINT('Ctrl Pts',(-23.8279256490022,2.91963682361093,2.94884327359225));
#46499=CARTESIAN_POINT('Ctrl Pts',(-23.8941846578322,3.51101935415754,1.78677195511959));
#46500=CARTESIAN_POINT('Ctrl Pts',(-23.9604436666622,4.10240188470415,0.624700636646922));
#46501=CARTESIAN_POINT('Ctrl Pts',(-24.0267026754922,4.05957375751508,-0.860123699732376));
#46502=CARTESIAN_POINT('Ctrl Pts',(-24.0929616843222,3.40219320868621,-1.98617525416531));
#46503=CARTESIAN_POINT('Ctrl Pts',(-24.1592206931522,2.74481265985733,-3.11222680859825));
#46504=CARTESIAN_POINT('Ctrl Pts',(-24.2254797019822,1.47287968938866,-3.87950558108483));
#46505=CARTESIAN_POINT('Ctrl Pts',(-24.2917387108122,0.170201795278273,
-3.93583954010648));
#46506=CARTESIAN_POINT('Ctrl Pts',(-24.3579977196422,-1.13247609883211,
-3.99217349912814));
#46507=CARTESIAN_POINT('Ctrl Pts',(-24.4242567284722,-2.46589891658421,
-3.33756264468487));
#46508=CARTESIAN_POINT('Ctrl Pts',(-24.4905157373022,-3.21803332339699,
-2.27246188703126));
#46509=CARTESIAN_POINT('Ctrl Pts',(-24.5312893175231,-3.68087170740913,
-1.6170344673876));
#46510=CARTESIAN_POINT('Ctrl Pts',(-24.5720628977441,-3.92359009889234,
-0.806164357459004));
#46511=CARTESIAN_POINT('Ctrl Pts',(-24.612836477965,-3.92791610626173,0.00232109521066254));
#46512=CARTESIAN_POINT('Ctrl Pts',(-24.796163522035,-3.92757907140906,0.00208605505030474));
#46513=CARTESIAN_POINT('Ctrl Pts',(-24.7563702773834,-3.92384973339512,
-0.78713429398102));
#46514=CARTESIAN_POINT('Ctrl Pts',(-24.7165770327318,-3.69348120864786,
-1.57837159481464));
#46515=CARTESIAN_POINT('Ctrl Pts',(-24.6767837880802,-3.25127923682329,
-2.22465431953071));
#46516=CARTESIAN_POINT('Ctrl Pts',(-24.6105247792502,-2.51497676608259,
-3.30076794480929));
#46517=CARTESIAN_POINT('Ctrl Pts',(-24.5442657704202,-1.19136658916336,
-3.97499536762895));
#46518=CARTESIAN_POINT('Ctrl Pts',(-24.4780067615902,0.112003991582728,
-3.93791887508927));
#46519=CARTESIAN_POINT('Ctrl Pts',(-24.4117477527602,1.41537457232881,-3.9008423825496));
#46520=CARTESIAN_POINT('Ctrl Pts',(-24.3454887439302,2.69850555690174,-3.15246197465059));
#46521=CARTESIAN_POINT('Ctrl Pts',(-24.2792297351002,3.37245887007014,-2.03625428556874));
#46522=CARTESIAN_POINT('Ctrl Pts',(-24.2129707262702,4.04641218323854,-0.920046596486897));
#46523=CARTESIAN_POINT('Ctrl Pts',(-24.1467117174402,4.11118782500241,0.563988373777779));
#46524=CARTESIAN_POINT('Ctrl Pts',(-24.0804527086102,3.53704904185838,1.73467621447729));
#46525=CARTESIAN_POINT('Ctrl Pts',(-24.0141936997803,2.96291025871434,2.90536405517679));
#46526=CARTESIAN_POINT('Ctrl Pts',(-23.9479346909503,1.7498570506624,3.76270476631113));
#46527=CARTESIAN_POINT('Ctrl Pts',(-23.8816756821203,0.454675018478186,
3.91319154529663));
#46528=CARTESIAN_POINT('Ctrl Pts',(-23.8154166732903,-0.840507013706024,
4.06367832428214));
#46529=CARTESIAN_POINT('Ctrl Pts',(-23.7491576644603,-2.21781787002251,
3.50731117111882));
#46530=CARTESIAN_POINT('Ctrl Pts',(-23.6828986556303,-3.04508289517983,
2.4994553191023));
#46531=CARTESIAN_POINT('Ctrl Pts',(-23.6373202777652,-3.61414359465313,
1.80616944495611));
#46532=CARTESIAN_POINT('Ctrl Pts',(-23.5917418999001,-3.92293272121378,
0.899247420609198));
#46533=CARTESIAN_POINT('Ctrl Pts',(-23.546163522035,-3.93003375797999,-0.00328548955642192));
#46534=CARTESIAN_POINT('Origin',(-20.1,0.,0.));
#46535=CARTESIAN_POINT('',(-22.112836477965,-3.93925214816407,-0.000930796536843803));
#46536=CARTESIAN_POINT('',(-22.296163522035,-3.93941472965677,-0.000577549300834287));
#46537=CARTESIAN_POINT('',(-20.1,-3.933,-4.81653586104654E-16));
#46538=CARTESIAN_POINT('Ctrl Pts',(-22.112836477965,-3.93925214816407,-0.000930796536843803));
#46539=CARTESIAN_POINT('Ctrl Pts',(-22.1765471339475,-3.93525732598551,
1.25304394614318));
#46540=CARTESIAN_POINT('Ctrl Pts',(-22.24025778993,-3.28460955709606,2.51058367703939));
#46541=CARTESIAN_POINT('Ctrl Pts',(-22.3039684459124,-2.25702327318862,
3.22887835952372));
#46542=CARTESIAN_POINT('Ctrl Pts',(-22.3702274547424,-1.18833472165735,
3.97590400186476));
#46543=CARTESIAN_POINT('Ctrl Pts',(-22.4364864635724,0.288049624548706,
4.13968349190898));
#46544=CARTESIAN_POINT('Ctrl Pts',(-22.5027454724024,1.49447969449625,3.6450432001131));
#46545=CARTESIAN_POINT('Ctrl Pts',(-22.5690044812324,2.70090976444378,3.15040290831721));
#46546=CARTESIAN_POINT('Ctrl Pts',(-22.6352634900624,3.63738555813281,1.99734283468122));
#46547=CARTESIAN_POINT('Ctrl Pts',(-22.7015224988924,3.8740712420106,0.715109458270375));
#46548=CARTESIAN_POINT('Ctrl Pts',(-22.7677815077224,4.11075692588839,-0.567123918140469));
#46549=CARTESIAN_POINT('Ctrl Pts',(-22.8340405165524,3.64765249995493,-1.97853059732616));
#46550=CARTESIAN_POINT('Ctrl Pts',(-22.9002995253823,2.69731965973127,-2.87128476585916));
#46551=CARTESIAN_POINT('Ctrl Pts',(-22.9665585342123,1.74698681950761,-3.76403893439215));
#46552=CARTESIAN_POINT('Ctrl Pts',(-23.0328175430423,0.30942556499374,-4.13814059227245));
#46553=CARTESIAN_POINT('Ctrl Pts',(-23.0990765518723,-0.955533573395335,
-3.82187976573015));
#46554=CARTESIAN_POINT('Ctrl Pts',(-23.1653355607023,-2.22049271178442,
-3.50561893918785));
#46555=CARTESIAN_POINT('Ctrl Pts',(-23.2315945695323,-3.31284973404871,
-2.49899562822293));
#46556=CARTESIAN_POINT('Ctrl Pts',(-23.2978535783623,-3.73122038868862,
-1.26404275200461));
#46557=CARTESIAN_POINT('Ctrl Pts',(-23.3195145448965,-3.86799141664524,
-0.860319946676077));
#46558=CARTESIAN_POINT('Ctrl Pts',(-23.3411755114308,-3.93273186569672,
-0.432194999766649));
#46559=CARTESIAN_POINT('Ctrl Pts',(-23.362836477965,-3.92954087356332,-0.00313358730535757));
#46560=CARTESIAN_POINT('Ctrl Pts',(-23.546163522035,-3.93003375797999,-0.00328548955642192));
#46561=CARTESIAN_POINT('Ctrl Pts',(-23.5254828910701,-3.93325576647851,
-0.412798748322419));
#46562=CARTESIAN_POINT('Ctrl Pts',(-23.5048022601052,-3.87436684872067,
-0.821408385246961));
#46563=CARTESIAN_POINT('Ctrl Pts',(-23.4841216291403,-3.74949809732583,
-1.20874765734832));
#46564=CARTESIAN_POINT('Ctrl Pts',(-23.4178626203103,-3.34942908031632,
-2.44975023091271));
#46565=CARTESIAN_POINT('Ctrl Pts',(-23.3516036114803,-2.27207185229914,
-3.47241082717177));
#46566=CARTESIAN_POINT('Ctrl Pts',(-23.2853446026503,-1.01192620125752,
-3.80733629848171));
#46567=CARTESIAN_POINT('Ctrl Pts',(-23.2190855938203,0.248219449784087,
-4.14226176979165));
#46568=CARTESIAN_POINT('Ctrl Pts',(-23.1528265849903,1.69115352385012,-3.78945211615245));
#46569=CARTESIAN_POINT('Ctrl Pts',(-23.0865675761603,2.65457957778525,-2.91084403176621));
#46570=CARTESIAN_POINT('Ctrl Pts',(-23.0203085673304,3.61800563172037,-2.03223594737998));
#46571=CARTESIAN_POINT('Ctrl Pts',(-22.9540495585004,4.10192366552458,-0.627829432246697));
#46572=CARTESIAN_POINT('Ctrl Pts',(-22.8877905496704,3.88421859382125,0.657762520794241));
#46573=CARTESIAN_POINT('Ctrl Pts',(-22.8215315408404,3.66651352211792,1.94335447383518));
#46574=CARTESIAN_POINT('Ctrl Pts',(-22.7552725320104,2.74718534490704,3.11013186478378));
#46575=CARTESIAN_POINT('Ctrl Pts',(-22.6890135231804,1.54819930612708,3.62255216810003));
#46576=CARTESIAN_POINT('Ctrl Pts',(-22.6227545143504,0.349213267347125,
4.13497247141627));
#46577=CARTESIAN_POINT('Ctrl Pts',(-22.5564955055204,-1.12943063300191,
3.99303568710015));
#46578=CARTESIAN_POINT('Ctrl Pts',(-22.4902364966904,-2.20904522830817,
3.26188974105464));
#46579=CARTESIAN_POINT('Ctrl Pts',(-22.4255455051386,-3.26311077950542,
2.54804633992363));
#46580=CARTESIAN_POINT('Ctrl Pts',(-22.3608545135868,-3.93680958792955,
1.27255103296312));
#46581=CARTESIAN_POINT('Ctrl Pts',(-22.296163522035,-3.93941472965677,-0.000577549300834287));
#46582=CARTESIAN_POINT('Origin',(-20.1,0.,0.));
#46583=CARTESIAN_POINT('',(-20.862836477965,-3.93234356276048,0.00362164229294471));
#46584=CARTESIAN_POINT('',(-21.046163522035,-3.9317665782605,0.00358829654485505));
#46585=CARTESIAN_POINT('',(-20.1,-3.933,-4.81653586104654E-16));
#46586=CARTESIAN_POINT('Ctrl Pts',(-20.862836477965,-3.93234356276048,0.0036216422929447));
#46587=CARTESIAN_POINT('Ctrl Pts',(-20.8794007388042,-3.93531979599253,
0.331135104398647));
#46588=CARTESIAN_POINT('Ctrl Pts',(-20.8959649996434,-3.89783641446075,
0.657976746908121));
#46589=CARTESIAN_POINT('Ctrl Pts',(-20.9125292604826,-3.81726008563346,
0.973824906028897));
#46590=CARTESIAN_POINT('Ctrl Pts',(-20.9787882693126,-3.49494520934099,
2.23725502025529));
#46591=CARTESIAN_POINT('Ctrl Pts',(-21.0450472781426,-2.48310226931282,
3.32477896443637));
#46592=CARTESIAN_POINT('Ctrl Pts',(-21.1113062869725,-1.2461600872343,3.73723086604704));
#46593=CARTESIAN_POINT('Ctrl Pts',(-21.1775652958025,-0.00921790515579238,
4.1496827676577));
#46594=CARTESIAN_POINT('Ctrl Pts',(-21.2438243046325,1.45282351897305,3.88706262669794));
#46595=CARTESIAN_POINT('Ctrl Pts',(-21.3100833134625,2.46889741289712,3.06991124842487));
#46596=CARTESIAN_POINT('Ctrl Pts',(-21.3763423222925,3.48497130682118,2.2527598701518));
#46597=CARTESIAN_POINT('Ctrl Pts',(-21.4426013311225,4.05507767054045,0.881077254565418));
#46598=CARTESIAN_POINT('Ctrl Pts',(-21.5088603399525,3.91754167653988,-0.415543886543193));
#46599=CARTESIAN_POINT('Ctrl Pts',(-21.5751193487825,3.78000568253931,-1.7121650276518));
#46600=CARTESIAN_POINT('Ctrl Pts',(-21.6413783576125,2.93482733081889,-2.93372469428265));
#46601=CARTESIAN_POINT('Ctrl Pts',(-21.7076373664425,1.76993756462108,-3.51953555564859));
#46602=CARTESIAN_POINT('Ctrl Pts',(-21.7738963752725,0.605047798423272,
-4.10534641701454));
#46603=CARTESIAN_POINT('Ctrl Pts',(-21.8401553841025,-0.879553382251932,
-4.05540847311559));
#46604=CARTESIAN_POINT('Ctrl Pts',(-21.9064143929325,-2.00244443517383,
-3.39264289164551));
#46605=CARTESIAN_POINT('Ctrl Pts',(-21.9726734017624,-3.12533548809572,
-2.72987731017544));
#46606=CARTESIAN_POINT('Ctrl Pts',(-22.0389324105924,-3.8865164132643,-1.45428409113424));
#46607=CARTESIAN_POINT('Ctrl Pts',(-22.1051914194224,-3.93661049742035,
-0.151351584294707));
#46608=CARTESIAN_POINT('Ctrl Pts',(-22.10773977227,-3.93853713961222,-0.101240183255385));
#46609=CARTESIAN_POINT('Ctrl Pts',(-22.1102881251175,-3.93941193644936,
-0.0510883417224217));
#46610=CARTESIAN_POINT('Ctrl Pts',(-22.112836477965,-3.93925214816407,-0.000930796536843803));
#46611=CARTESIAN_POINT('Ctrl Pts',(-22.296163522035,-3.93941472965677,-0.000577549300834287));
#46612=CARTESIAN_POINT('Ctrl Pts',(-22.2945955047568,-3.93947787457297,
-0.0314363685343833));
#46613=CARTESIAN_POINT('Ctrl Pts',(-22.2930274874786,-3.93914674633027,
-0.0622937972973192));
#46614=CARTESIAN_POINT('Ctrl Pts',(-22.2914594702004,-3.93841720487129,
-0.0931418037587124));
#46615=CARTESIAN_POINT('Ctrl Pts',(-22.2252004613704,-3.90758929586465,
-1.39667229475164));
#46616=CARTESIAN_POINT('Ctrl Pts',(-22.1589414525405,-3.16534818758786,
-2.68337816896259));
#46617=CARTESIAN_POINT('Ctrl Pts',(-22.0926824437105,-2.05237735636058,
-3.36267046029439));
#46618=CARTESIAN_POINT('Ctrl Pts',(-22.0264234348805,-0.939406525133289,
-4.04196275162618));
#46619=CARTESIAN_POINT('Ctrl Pts',(-21.9601644260505,0.544294029044505,
-4.11384146007883));
#46620=CARTESIAN_POINT('Ctrl Pts',(-21.8939054172205,1.71771614846726,-3.54531475321241));
#46621=CARTESIAN_POINT('Ctrl Pts',(-21.8276464083905,2.89113826789002,-2.97678804634599));
#46622=CARTESIAN_POINT('Ctrl Pts',(-21.7613873995605,3.75428195255775,-1.76785592416049));
#46623=CARTESIAN_POINT('Ctrl Pts',(-21.6951283907305,3.91097029556221,-0.473409766869109));
#46624=CARTESIAN_POINT('Ctrl Pts',(-21.6288693819005,4.06765863856667,0.821036390422279));
#46625=CARTESIAN_POINT('Ctrl Pts',(-21.5626103730705,3.51789163990787,2.20099658281955));
#46626=CARTESIAN_POINT('Ctrl Pts',(-21.4963513642405,2.51400850188269,3.03307875075606));
#46627=CARTESIAN_POINT('Ctrl Pts',(-21.4300923554105,1.51012536385751,3.86516091869257));
#46628=CARTESIAN_POINT('Ctrl Pts',(-21.3638333465805,0.0521260864659473,
4.14936506216831));
#46629=CARTESIAN_POINT('Ctrl Pts',(-21.2975743377506,-1.19077787552372,
3.75524346893355));
#46630=CARTESIAN_POINT('Ctrl Pts',(-21.2313153289206,-2.43368183751338,
3.36112187569878));
#46631=CARTESIAN_POINT('Ctrl Pts',(-21.1650563200905,-3.46149048410115,
2.28867454575351));
#46632=CARTESIAN_POINT('Ctrl Pts',(-21.0987973112606,-3.80244684589627,
1.03014729183));
#46633=CARTESIAN_POINT('Ctrl Pts',(-21.081252714852,-3.89272802978727,0.696904263763043));
#46634=CARTESIAN_POINT('Ctrl Pts',(-21.0637081184435,-3.93485212301176,
0.350614663720363));
#46635=CARTESIAN_POINT('Ctrl Pts',(-21.046163522035,-3.9317665782605,0.00358829654485505));
#46636=CARTESIAN_POINT('Origin',(-20.1,0.,0.));
#46637=CARTESIAN_POINT('',(-19.612836477965,-3.92668363390084,-0.000828347603293866));
#46638=CARTESIAN_POINT('',(-19.796163522035,-3.92682791432394,-0.00113809054688487));
#46639=CARTESIAN_POINT('',(-20.1,-3.933,-4.81653586104654E-16));
#46640=CARTESIAN_POINT('Ctrl Pts',(-19.612836477965,-3.92668363390084,-0.000828347603293866));
#46641=CARTESIAN_POINT('Ctrl Pts',(-19.6485133524909,-3.92535470355143,
0.707150422160364));
#46642=CARTESIAN_POINT('Ctrl Pts',(-19.6841902270168,-3.7427691911929,1.41576831419161));
#46643=CARTESIAN_POINT('Ctrl Pts',(-19.7198671015427,-3.38301464948758,
2.01866822195352));
#46644=CARTESIAN_POINT('Ctrl Pts',(-19.7861261103727,-2.71487934693509,
3.13837253582242));
#46645=CARTESIAN_POINT('Ctrl Pts',(-19.8523851192027,-1.43565559653748,
3.89343614948163));
#46646=CARTESIAN_POINT('Ctrl Pts',(-19.9186441280327,-0.132498138932822,
3.93729015340666));
#46647=CARTESIAN_POINT('Ctrl Pts',(-19.9849031368627,1.17065931867184,3.98114415733169));
#46648=CARTESIAN_POINT('Ctrl Pts',(-20.0511621456927,2.49775048348358,3.31378855152255));
#46649=CARTESIAN_POINT('Ctrl Pts',(-20.1174211545226,3.23964980691583,2.24153488430273));
#46650=CARTESIAN_POINT('Ctrl Pts',(-20.1836801633526,3.98154913034808,1.1692812170829));
#46651=CARTESIAN_POINT('Ctrl Pts',(-20.2499391721826,4.13825661240085,-0.307870511547617));
#46652=CARTESIAN_POINT('Ctrl Pts',(-20.3161981810126,3.63784461652941,-1.51191800536888));
#46653=CARTESIAN_POINT('Ctrl Pts',(-20.3824571898426,3.13743262065797,-2.71596549919015));
#46654=CARTESIAN_POINT('Ctrl Pts',(-20.4487161986726,1.97990114686232,-3.64690875820217));
#46655=CARTESIAN_POINT('Ctrl Pts',(-20.5149752075026,0.696549033280147,
-3.8774513476293));
#46656=CARTESIAN_POINT('Ctrl Pts',(-20.5812342163326,-0.586803080302027,
-4.10799393705643));
#46657=CARTESIAN_POINT('Ctrl Pts',(-20.6474932251626,-1.99597583367073,
-3.63813585689868));
#46658=CARTESIAN_POINT('Ctrl Pts',(-20.7137522339926,-2.8841688040767,-2.68353867468395));
#46659=CARTESIAN_POINT('Ctrl Pts',(-20.7634469819834,-3.55032011860643,
-1.96758370885252));
#46660=CARTESIAN_POINT('Ctrl Pts',(-20.8131417299742,-3.92341450991201,
-0.97895760594279));
#46661=CARTESIAN_POINT('Ctrl Pts',(-20.862836477965,-3.93234356276048,0.0036216422929447));
#46662=CARTESIAN_POINT('Ctrl Pts',(-21.046163522035,-3.9317665782605,0.00358829654485505));
#46663=CARTESIAN_POINT('Ctrl Pts',(-20.9974491096135,-3.92319923957353,
-0.959966816269948));
#46664=CARTESIAN_POINT('Ctrl Pts',(-20.9487346971921,-3.56608662401112,
-1.92920206092837));
#46665=CARTESIAN_POINT('Ctrl Pts',(-20.9000202847706,-2.92352288274049,
-2.6406096667939));
#46666=CARTESIAN_POINT('Ctrl Pts',(-20.8337612759406,-2.0495384807871,-3.60823219359254));
#46667=CARTESIAN_POINT('Ctrl Pts',(-20.7675022671106,-0.64746559987786,
-4.09887006928808));
#46668=CARTESIAN_POINT('Ctrl Pts',(-20.7012432582806,0.639154129026382,
-3.88732394561629));
#46669=CARTESIAN_POINT('Ctrl Pts',(-20.6349842494506,1.92577385793062,-3.6757778219445));
#46670=CARTESIAN_POINT('Ctrl Pts',(-20.5687252406206,3.09694043482986,-2.7620476989054));
#46671=CARTESIAN_POINT('Ctrl Pts',(-20.5024662317906,3.61509660473914,-1.56552930251614));
#46672=CARTESIAN_POINT('Ctrl Pts',(-20.4362072229606,4.13325277464841,-0.369010906126889));
#46673=CARTESIAN_POINT('Ctrl Pts',(-20.3699482141306,3.99839853756772,1.11029576361251));
#46674=CARTESIAN_POINT('Ctrl Pts',(-20.3036892053006,3.27243104370014,2.19339930765503));
#46675=CARTESIAN_POINT('Ctrl Pts',(-20.2374301964706,2.54646354983257,3.27650285169755));
#46676=CARTESIAN_POINT('Ctrl Pts',(-20.1711711876407,1.2293827991781,3.96340327004319));
#46677=CARTESIAN_POINT('Ctrl Pts',(-20.1049121788107,-0.074280369672471,
3.93881808228536));
#46678=CARTESIAN_POINT('Ctrl Pts',(-20.0386531699807,-1.37794353852305,
3.91423289452753));
#46679=CARTESIAN_POINT('Ctrl Pts',(-19.9723941611507,-2.66818912556973,
3.17816210066622));
#46680=CARTESIAN_POINT('Ctrl Pts',(-19.9061351523207,-3.35280344433398,
2.06845703902532));
#46681=CARTESIAN_POINT('Ctrl Pts',(-19.8694779422255,-3.73156025582722,
1.45452253703641));
#46682=CARTESIAN_POINT('Ctrl Pts',(-19.8328207321302,-3.92494801200659,
0.726227639740267));
#46683=CARTESIAN_POINT('Ctrl Pts',(-19.796163522035,-3.92682791432394,-0.00113809054688487));
#46684=CARTESIAN_POINT('Origin',(-20.1,0.,0.));
#46685=CARTESIAN_POINT('',(-18.362836477965,-3.93539198680633,-0.00329798213515642));
#46686=CARTESIAN_POINT('',(-18.546163522035,-3.93595275298544,-0.00314060659151173));
#46687=CARTESIAN_POINT('',(-20.1,-3.933,-4.81653586104654E-16));
#46688=CARTESIAN_POINT('Ctrl Pts',(-18.362836477965,-3.93539198680633,-0.00329798213515642));
#46689=CARTESIAN_POINT('Ctrl Pts',(-18.4176259661776,-3.9256864189977,1.07786343746756));
#46690=CARTESIAN_POINT('Ctrl Pts',(-18.4724154543902,-3.46255938905757,
2.1663295974234));
#46691=CARTESIAN_POINT('Ctrl Pts',(-18.5272049426028,-2.6696961456285,2.89698671044328));
#46692=CARTESIAN_POINT('Ctrl Pts',(-18.5934639514328,-1.71085651486767,
3.78059810530474));
#46693=CARTESIAN_POINT('Ctrl Pts',(-18.6597229602628,-0.269778218465152,
4.1409143621431));
#46694=CARTESIAN_POINT('Ctrl Pts',(-18.7259819690928,0.992093901389918,
3.8125528451441));
#46695=CARTESIAN_POINT('Ctrl Pts',(-18.7922409779228,2.25396602124499,3.48419132814511));
#46696=CARTESIAN_POINT('Ctrl Pts',(-18.8584999867528,3.33663196455261,2.46715203730877));
#46697=CARTESIAN_POINT('Ctrl Pts',(-18.9247589955828,3.74315564656476,1.22824888183212));
#46698=CARTESIAN_POINT('Ctrl Pts',(-18.9910180044128,4.14967932857691,-0.0106542736445235));
#46699=CARTESIAN_POINT('Ctrl Pts',(-19.0572770132428,3.88006074929359,-1.47142129376147));
#46700=CARTESIAN_POINT('Ctrl Pts',(-19.1235360220728,3.05805294831981,-2.48357034817677));
#46701=CARTESIAN_POINT('Ctrl Pts',(-19.1897950309028,2.23604514734603,-3.49571940259206));
#46702=CARTESIAN_POINT('Ctrl Pts',(-19.2560540397328,0.861648124681792,
-4.0592504913057));
#46703=CARTESIAN_POINT('Ctrl Pts',(-19.3223130485627,-0.434299513895741,
-3.91550679233807));
#46704=CARTESIAN_POINT('Ctrl Pts',(-19.3885720573927,-1.73024715247327,
-3.77176309337043));
#46705=CARTESIAN_POINT('Ctrl Pts',(-19.4548310662227,-2.9477454069641,-2.92074460672151));
#46706=CARTESIAN_POINT('Ctrl Pts',(-19.5210900750527,-3.5279711068558,-1.75306285635774));
#46707=CARTESIAN_POINT('Ctrl Pts',(-19.5516722093568,-3.79577680745584,
-1.21411425533504));
#46708=CARTESIAN_POINT('Ctrl Pts',(-19.5822543436609,-3.92782278992184,
-0.607706111115191));
#46709=CARTESIAN_POINT('Ctrl Pts',(-19.612836477965,-3.92668363390084,-0.000828347603293866));
#46710=CARTESIAN_POINT('Ctrl Pts',(-19.796163522035,-3.92682791432394,-0.00113809054688487));
#46711=CARTESIAN_POINT('Ctrl Pts',(-19.7665617233002,-3.92834599193799,
-0.588507775762331));
#46712=CARTESIAN_POINT('Ctrl Pts',(-19.7369599245655,-3.80498088204029,
-1.17527154672688));
#46713=CARTESIAN_POINT('Ctrl Pts',(-19.7073581258307,-3.55349992886683,
-1.70071858759768));
#46714=CARTESIAN_POINT('Ctrl Pts',(-19.6410991170007,-2.9905990441536,-2.87684982315929));
#46715=CARTESIAN_POINT('Ctrl Pts',(-19.5748401081707,-1.78581422424533,
-3.74577296486201));
#46716=CARTESIAN_POINT('Ctrl Pts',(-19.5085810993407,-0.492133262158209,
-3.90865837735552));
#46717=CARTESIAN_POINT('Ctrl Pts',(-19.4423220905107,0.801547699928912,
-4.07154378984904));
#46718=CARTESIAN_POINT('Ctrl Pts',(-19.3760630816808,2.18412480419487,-3.52839147313334));
#46719=CARTESIAN_POINT('Ctrl Pts',(-19.3098040728508,3.02100484455689,-2.52850453584661));
#46720=CARTESIAN_POINT('Ctrl Pts',(-19.2435450640208,3.8578848849189,-1.52861759855989));
#46721=CARTESIAN_POINT('Ctrl Pts',(-19.1772860551908,4.14906786137697,-0.0719960407021211));
#46722=CARTESIAN_POINT('Ctrl Pts',(-19.1110270463608,3.76090282736967,1.17278104601673));
#46723=CARTESIAN_POINT('Ctrl Pts',(-19.0447680375308,3.37273779336236,2.4175581327356));
#46724=CARTESIAN_POINT('Ctrl Pts',(-18.9785090287008,2.3052247488897,3.45049074831555));
#46725=CARTESIAN_POINT('Ctrl Pts',(-18.9122500198708,1.04834470371331,3.79747005787655));
#46726=CARTESIAN_POINT('Ctrl Pts',(-18.8459910110408,-0.208535341463058,
4.14444936743754));
#46727=CARTESIAN_POINT('Ctrl Pts',(-18.7797320022108,-1.65478238734316,
3.80547537097956));
#46728=CARTESIAN_POINT('Ctrl Pts',(-18.7134729933808,-2.62657917083836,
2.93613475815557));
#46729=CARTESIAN_POINT('Ctrl Pts',(-18.6577031695989,-3.44453489224753,
2.20441580189885));
#46730=CARTESIAN_POINT('Ctrl Pts',(-18.6019333458169,-3.92636673554791,
1.0969590749087));
#46731=CARTESIAN_POINT('Ctrl Pts',(-18.546163522035,-3.93595275298544,-0.00314060659151173));
#46732=CARTESIAN_POINT('Origin',(-20.1,0.,0.));
#46733=CARTESIAN_POINT('',(-17.112836477965,-3.93744710033063,0.002522420057968));
#46734=CARTESIAN_POINT('',(-17.296163522035,-3.93695989693636,0.00276125700748165));
#46735=CARTESIAN_POINT('',(-20.1,-3.933,-4.81653586104654E-16));
#46736=CARTESIAN_POINT('Ctrl Pts',(-17.112836477965,-3.93744710033063,0.002522420057968));
#46737=CARTESIAN_POINT('Ctrl Pts',(-17.1204795710344,-3.93856978775161,
0.153138791280183));
#46738=CARTESIAN_POINT('Ctrl Pts',(-17.1281226641037,-3.93067892709947,
0.303636406391696));
#46739=CARTESIAN_POINT('Ctrl Pts',(-17.135765757173,-3.913382153674,0.453045118553371));
#46740=CARTESIAN_POINT('Ctrl Pts',(-17.202024766003,-3.76343408255482,1.74828947690608));
#46741=CARTESIAN_POINT('Ctrl Pts',(-17.268283774833,-2.90659489979499,2.96169852217127));
#46742=CARTESIAN_POINT('Ctrl Pts',(-17.334542783663,-1.73614792488526,3.5363257840275));
#46743=CARTESIAN_POINT('Ctrl Pts',(-17.4008017924929,-0.565700949975524,
4.11095304588373));
#46744=CARTESIAN_POINT('Ctrl Pts',(-17.467060801323,0.918353817084128,4.04679852433096));
#46745=CARTESIAN_POINT('Ctrl Pts',(-17.5333198101529,2.03484570423632,3.37330880791163));
#46746=CARTESIAN_POINT('Ctrl Pts',(-17.5995788189829,3.15133759138853,2.6998190914923));
#46747=CARTESIAN_POINT('Ctrl Pts',(-17.6658378278129,3.90026659863329,1.41699418020642));
#46748=CARTESIAN_POINT('Ctrl Pts',(-17.7320968366429,3.93787952146319,0.113641664316406));
#46749=CARTESIAN_POINT('Ctrl Pts',(-17.7983558454729,3.97549244429308,-1.18971085157359));
#46750=CARTESIAN_POINT('Ctrl Pts',(-17.8646148543029,3.30178928270808,-2.51359097206773));
#46751=CARTESIAN_POINT('Ctrl Pts',(-17.9308738631329,2.22599508740998,-3.25034696552659));
#46752=CARTESIAN_POINT('Ctrl Pts',(-17.9971328719629,1.15020089211187,-3.98710295898546));
#46753=CARTESIAN_POINT('Ctrl Pts',(-18.0633918807929,-0.327684336899324,
-4.13673482540907));
#46754=CARTESIAN_POINT('Ctrl Pts',(-18.1296508896229,-1.52932164152444,
-3.63056260167998));
#46755=CARTESIAN_POINT('Ctrl Pts',(-18.1959098984529,-2.73095894614955,
-3.1243903779509));
#46756=CARTESIAN_POINT('Ctrl Pts',(-18.2621689072829,-3.65634832638855,
-1.96241406406912));
#46757=CARTESIAN_POINT('Ctrl Pts',(-18.3284279161129,-3.8807425339485,-0.677972640685939));
#46758=CARTESIAN_POINT('Ctrl Pts',(-18.3398974367302,-3.91958546316641,
-0.455634159512376));
#46759=CARTESIAN_POINT('Ctrl Pts',(-18.3513669573476,-3.93742373073598,
-0.229626126408842));
#46760=CARTESIAN_POINT('Ctrl Pts',(-18.362836477965,-3.93539198680633,-0.00329798213515642));
#46761=CARTESIAN_POINT('Ctrl Pts',(-18.546163522035,-3.93595275298544,-0.00314060659151173));
#46762=CARTESIAN_POINT('Ctrl Pts',(-18.5356743369869,-3.93775569055916,
-0.210047287445732));
#46763=CARTESIAN_POINT('Ctrl Pts',(-18.5251851519389,-3.92285337434481,
-0.4166937197063));
#46764=CARTESIAN_POINT('Ctrl Pts',(-18.5146959668909,-3.89034016437652,
-0.62053111545171));
#46765=CARTESIAN_POINT('Ctrl Pts',(-18.4484369580609,-3.68495785330915,
-1.90814914704498));
#46766=CARTESIAN_POINT('Ctrl Pts',(-18.3821779492309,-2.7768467100641,-3.08367798104153));
#46767=CARTESIAN_POINT('Ctrl Pts',(-18.3159189404009,-1.58282338906351,
-3.60755811801555));
#46768=CARTESIAN_POINT('Ctrl Pts',(-18.2496599315709,-0.388800068062912,
-4.13143825498958));
#46769=CARTESIAN_POINT('Ctrl Pts',(-18.1834009227409,1.09113543069324,-4.00366969494108));
#46770=CARTESIAN_POINT('Ctrl Pts',(-18.1171419139109,2.17770308165872,-3.28289731004049));
#46771=CARTESIAN_POINT('Ctrl Pts',(-18.0508829050809,3.2642707326242,-2.56212492513991));
#46772=CARTESIAN_POINT('Ctrl Pts',(-17.9846238962509,3.95747053579902,-1.24834871538727));
#46773=CARTESIAN_POINT('Ctrl Pts',(-17.9183648874209,3.93912863407312,0.0554172380767894));
#46774=CARTESIAN_POINT('Ctrl Pts',(-17.8521058785909,3.92078673234721,1.35918319154085));
#46775=CARTESIAN_POINT('Ctrl Pts',(-17.7858468697609,3.19090312572055,2.65293888871631));
#46776=CARTESIAN_POINT('Ctrl Pts',(-17.7195878609309,2.08448928314013,3.34285953427781));
#46777=CARTESIAN_POINT('Ctrl Pts',(-17.6533288521009,0.978075440559705,
4.0327801798393));
#46778=CARTESIAN_POINT('Ctrl Pts',(-17.587069843271,-0.504868637974483,
4.11886577378683));
#46779=CARTESIAN_POINT('Ctrl Pts',(-17.520810834441,-1.68368202029562,3.5616036177215));
#46780=CARTESIAN_POINT('Ctrl Pts',(-17.454551825611,-2.86249540261677,3.00434146165616));
#46781=CARTESIAN_POINT('Ctrl Pts',(-17.388292816781,-3.73717808872487,1.80373155557796));
#46782=CARTESIAN_POINT('Ctrl Pts',(-17.322033807951,-3.90625682929457,0.510845463029787));
#46783=CARTESIAN_POINT('Ctrl Pts',(-17.3134103793123,-3.92826196458659,
0.34257987690214));
#46784=CARTESIAN_POINT('Ctrl Pts',(-17.3047869506736,-3.93831536149175,
0.172751288119817));
#46785=CARTESIAN_POINT('Ctrl Pts',(-17.296163522035,-3.93695989693636,0.00276125700748165));
#46786=CARTESIAN_POINT('Origin',(-20.1,0.,0.));
#46787=CARTESIAN_POINT('',(-15.862836477965,-3.92749965338984,0.00198301116285243));
#46788=CARTESIAN_POINT('',(-16.046163522035,-3.92722756002595,0.00170206837946952));
#46789=CARTESIAN_POINT('',(-20.1,-3.933,-4.81653586104654E-16));
#46790=CARTESIAN_POINT('Ctrl Pts',(-15.862836477965,-3.92749965338984,0.00198301116285243));
#46791=CARTESIAN_POINT('Ctrl Pts',(-15.8895921847211,-3.929911697341,0.532649718284621));
#46792=CARTESIAN_POINT('Ctrl Pts',(-15.9163478914771,-3.82991474772018,
1.06244554991683));
#46793=CARTESIAN_POINT('Ctrl Pts',(-15.9431035982331,-3.62319942873785,
1.54668685901589));
#46794=CARTESIAN_POINT('Ctrl Pts',(-16.0093626070631,-3.11128052221676,
2.74588333205284));
#46795=CARTESIAN_POINT('Ctrl Pts',(-16.0756216158931,-1.94488189277277,
3.66570417872142));
#46796=CARTESIAN_POINT('Ctrl Pts',(-16.1418806247231,-0.659379616892197,
3.88394644908117));
#46797=CARTESIAN_POINT('Ctrl Pts',(-16.2081396335531,0.626122658988377,
4.10218871944093));
#46798=CARTESIAN_POINT('Ctrl Pts',(-16.2743986423831,2.03072858130552,3.61885241349186));
#46799=CARTESIAN_POINT('Ctrl Pts',(-16.3406576512131,2.90973762197645,2.65579150308084));
#46800=CARTESIAN_POINT('Ctrl Pts',(-16.4069166600431,3.78874666264738,1.69273059266982));
#46801=CARTESIAN_POINT('Ctrl Pts',(-16.4731756688731,4.14215882167208,0.249945077796819));
#46802=CARTESIAN_POINT('Ctrl Pts',(-16.5394346777031,3.80775845969318,-1.0103396865036));
#46803=CARTESIAN_POINT('Ctrl Pts',(-16.605693686533,3.47335809771428,-2.27062445080401));
#46804=CARTESIAN_POINT('Ctrl Pts',(-16.671952695363,2.45114521473181,-3.34840846453186));
#46805=CARTESIAN_POINT('Ctrl Pts',(-16.738211704193,1.21030936065731,-3.74899482213246));
#46806=CARTESIAN_POINT('Ctrl Pts',(-16.804470713023,-0.0305264934171873,
-4.14958117973306));
#46807=CARTESIAN_POINT('Ctrl Pts',(-16.870729721853,-1.4899853185837,-3.87296988120641));
#46808=CARTESIAN_POINT('Ctrl Pts',(-16.936988730683,-2.4981862514277,-3.04612439622297));
#46809=CARTESIAN_POINT('Ctrl Pts',(-16.9956046464437,-3.39008943550714,
-2.31465699049648));
#46810=CARTESIAN_POINT('Ctrl Pts',(-17.0542205622044,-3.92883705846707,
-1.15257492700707));
#46811=CARTESIAN_POINT('Ctrl Pts',(-17.112836477965,-3.93744710033063,0.002522420057968));
#46812=CARTESIAN_POINT('Ctrl Pts',(-17.296163522035,-3.93695989693636,0.00276125700748165));
#46813=CARTESIAN_POINT('Ctrl Pts',(-17.2385279418436,-3.92790050891893,
-1.13338475642016));
#46814=CARTESIAN_POINT('Ctrl Pts',(-17.1808923616523,-3.40920089730388,
-2.27674248904084));
#46815=CARTESIAN_POINT('Ctrl Pts',(-17.123256781461,-2.54294257060525,-3.00886164266523));
#46816=CARTESIAN_POINT('Ctrl Pts',(-17.056997772631,-1.54707477631489,-3.85052037679398));
#46817=CARTESIAN_POINT('Ctrl Pts',(-16.990738763801,-0.0918643927028295,
-4.14867556603334));
#46818=CARTESIAN_POINT('Ctrl Pts',(-16.924479754971,1.15475729573842,-3.76647596650864));
#46819=CARTESIAN_POINT('Ctrl Pts',(-16.858220746141,2.40137898417968,-3.38427636698394));
#46820=CARTESIAN_POINT('Ctrl Pts',(-16.791961737311,3.43941197745014,-2.32172197869517));
#46821=CARTESIAN_POINT('Ctrl Pts',(-16.725702728481,3.7924062321702,-1.06651801778504));
#46822=CARTESIAN_POINT('Ctrl Pts',(-16.6594437196511,4.14540048689025,0.188685943125091));
#46823=CARTESIAN_POINT('Ctrl Pts',(-16.5931847108211,3.81335600305992,1.63653947665657));
#46824=CARTESIAN_POINT('Ctrl Pts',(-16.5269257019911,2.94867920387608,2.612488330913));
#46825=CARTESIAN_POINT('Ctrl Pts',(-16.4606666931611,2.08400240469223,3.58843718516944));
#46826=CARTESIAN_POINT('Ctrl Pts',(-16.3944076843311,0.686693290154852,
4.09248136015081));
#46827=CARTESIAN_POINT('Ctrl Pts',(-16.3281486755011,-0.601893685968137,
3.89326737738197));
#46828=CARTESIAN_POINT('Ctrl Pts',(-16.2618896666711,-1.89048066209112,
3.69405339461314));
#46829=CARTESIAN_POINT('Ctrl Pts',(-16.1956306578411,-3.07034549979972,
2.79158125409412));
#46830=CARTESIAN_POINT('Ctrl Pts',(-16.1293716490111,-3.59993725883069,
1.60008076770775));
#46831=CARTESIAN_POINT('Ctrl Pts',(-16.1016356066857,-3.82162453884031,
1.10131828235401));
#46832=CARTESIAN_POINT('Ctrl Pts',(-16.0738995643604,-3.92936691994989,
0.551910450100659));
#46833=CARTESIAN_POINT('Ctrl Pts',(-16.046163522035,-3.92722756002595,0.00170206837946952));
#46834=CARTESIAN_POINT('Origin',(-20.1,0.,0.));
#46835=CARTESIAN_POINT('',(-14.612836477965,-3.92993428904087,-0.00292452251886177));
#46836=CARTESIAN_POINT('',(-14.796163522035,-3.93066717675506,-0.00339337507098336));
#46837=CARTESIAN_POINT('',(-20.1,-3.933,-4.81653586104654E-16));
#46838=CARTESIAN_POINT('Ctrl Pts',(-14.612836477965,-3.92993428904087,-0.00292452251886177));
#46839=CARTESIAN_POINT('Ctrl Pts',(-14.6587047984078,-3.92274597267032,
0.905157682402563));
#46840=CARTESIAN_POINT('Ctrl Pts',(-14.7045731188505,-3.60989172825119,
1.81749520012196));
#46841=CARTESIAN_POINT('Ctrl Pts',(-14.7504414392932,-3.03423748762575,
2.51256698125943));
#46842=CARTESIAN_POINT('Ctrl Pts',(-14.8167004481232,-2.20267707633405,
3.51663180943119));
#46843=CARTESIAN_POINT('Ctrl Pts',(-14.8829594569532,-0.822726637212052,
4.06732386343745));
#46844=CARTESIAN_POINT('Ctrl Pts',(-14.9492184657832,0.471837982743719,
3.91125962200143));
#46845=CARTESIAN_POINT('Ctrl Pts',(-15.0154774746132,1.76640260269949,3.75519538056541));
#46846=CARTESIAN_POINT('Ctrl Pts',(-15.0817364834432,2.97558140348904,2.89237484368711));
#46847=CARTESIAN_POINT('Ctrl Pts',(-15.1479954922732,3.54456962503122,1.71914580902439));
#46848=CARTESIAN_POINT('Ctrl Pts',(-15.2142545011032,4.1135578465734,0.545916774361676));
#46849=CARTESIAN_POINT('Ctrl Pts',(-15.2805135099332,4.04235548886822,-0.937720758085456));
#46850=CARTESIAN_POINT('Ctrl Pts',(-15.3467725187632,3.36354093984507,-2.05095209846013));
#46851=CARTESIAN_POINT('Ctrl Pts',(-15.4130315275932,2.68472639082192,-3.1641834388348));
#46852=CARTESIAN_POINT('Ctrl Pts',(-15.4792905364232,1.39829965048081,-3.907008587137));
#46853=CARTESIAN_POINT('Ctrl Pts',(-15.5455495452532,0.0947746782110898,
-3.93839117418686));
#46854=CARTESIAN_POINT('Ctrl Pts',(-15.6118085540831,-1.20875029405863,
-3.96977376123672));
#46855=CARTESIAN_POINT('Ctrl Pts',(-15.6780675629131,-2.52937349825695,
-3.28971378703422));
#46856=CARTESIAN_POINT('Ctrl Pts',(-15.7443265717431,-3.26096550855702,
-2.21039775023031));
#46857=CARTESIAN_POINT('Ctrl Pts',(-15.7838298738171,-3.69713714299747,
-1.56691472523465));
#46858=CARTESIAN_POINT('Ctrl Pts',(-15.8233331758911,-3.92393840562737,
-0.781516652037125));
#46859=CARTESIAN_POINT('Ctrl Pts',(-15.862836477965,-3.92749965338984,0.00198301116285243));
#46860=CARTESIAN_POINT('Ctrl Pts',(-16.046163522035,-3.92722756002595,0.00170206837946952));
#46861=CARTESIAN_POINT('Ctrl Pts',(-16.0076405555304,-3.9242561739239,-0.762489837983766));
#46862=CARTESIAN_POINT('Ctrl Pts',(-15.9691175890257,-3.70931400904017,
-1.5282260691143));
#46863=CARTESIAN_POINT('Ctrl Pts',(-15.9305946225211,-3.29328759331302,
-2.16195612127992));
#46864=CARTESIAN_POINT('Ctrl Pts',(-15.8643356136911,-2.57772748841107,
-3.25196369162747));
#46865=CARTESIAN_POINT('Ctrl Pts',(-15.7980766048612,-1.26728859825383,
-3.95145000006882));
#46866=CARTESIAN_POINT('Ctrl Pts',(-15.7318175960312,0.0365514847583181,
-3.93935038839483));
#46867=CARTESIAN_POINT('Ctrl Pts',(-15.6655585872012,1.34039156777047,-3.92725077672083));
#46868=CARTESIAN_POINT('Ctrl Pts',(-15.5992995783712,2.63763284363753,-3.2035652449315));
#46869=CARTESIAN_POINT('Ctrl Pts',(-15.5330405695412,3.33284158193514,-2.10047074141391));
#46870=CARTESIAN_POINT('Ctrl Pts',(-15.4667815607112,4.02805032023276,-0.997376237896311));
#46871=CARTESIAN_POINT('Ctrl Pts',(-15.4005225518812,4.12122652096094,0.485127237349519));
#46872=CARTESIAN_POINT('Ctrl Pts',(-15.3342635430512,3.56962055023412,1.66660105852033));
#46873=CARTESIAN_POINT('Ctrl Pts',(-15.2680045342212,3.01801457950731,2.84807487969113));
#46874=CARTESIAN_POINT('Ctrl Pts',(-15.2017455253912,1.82162643732546,3.72851904678691));
#46875=CARTESIAN_POINT('Ctrl Pts',(-15.1354865165612,0.529555795411518,
3.90377691175494));
#46876=CARTESIAN_POINT('Ctrl Pts',(-15.0692275077312,-0.762514846502421,
4.07903477672298));
#46877=CARTESIAN_POINT('Ctrl Pts',(-15.0029684989012,-2.15026798814847,
3.5491063395633));
#46878=CARTESIAN_POINT('Ctrl Pts',(-14.9367094900712,-2.99666853050174,
2.55730054859198));
#46879=CARTESIAN_POINT('Ctrl Pts',(-14.8898608340592,-3.59511889306143,
1.85604091382695));
#46880=CARTESIAN_POINT('Ctrl Pts',(-14.8430121780471,-3.92293383932689,
0.923877483478437));
#46881=CARTESIAN_POINT('Ctrl Pts',(-14.796163522035,-3.93066717675506,-0.00339337507098336));
#46882=CARTESIAN_POINT('Origin',(-28.5777734492731,0.,0.));
#46883=CARTESIAN_POINT('',(-14.2027734492731,-3.22023791762178,-0.00239639078269415));
#46884=CARTESIAN_POINT('',(-13.9562265507269,-3.22274745212571,-5.48329643912382E-7));
#46885=CARTESIAN_POINT('',(-28.5777734492731,-3.22275,-1.83004677902795E-13));
#46886=CARTESIAN_POINT('',(-13.9553333333333,-1.03523973309624,-3.05194958305651));
#46887=CARTESIAN_POINT('Ctrl Pts',(-14.2027734492731,-3.22023791762178,
-0.00239639078269425));
#46888=CARTESIAN_POINT('Ctrl Pts',(-14.1823827608858,-3.22285639546545,
-0.333182212003909));
#46889=CARTESIAN_POINT('Ctrl Pts',(-14.0999027222393,-3.03322933916847,
-1.66841872358004));
#46890=CARTESIAN_POINT('Ctrl Pts',(-14.0174226835927,-1.98323022307269,
-2.73145967097912));
#46891=CARTESIAN_POINT('Ctrl Pts',(-13.9553333333333,-1.03598926702581,
-3.05747757600544));
#46892=CARTESIAN_POINT('',(-13.9553333333333,-3.22271751746272,-0.0144694553766564));
#46893=CARTESIAN_POINT('Origin',(-13.9553333333333,0.,0.));
#46894=CARTESIAN_POINT('Ctrl Pts',(-13.9562265507269,-3.22274745212571,
-5.48329644236558E-7));
#46895=CARTESIAN_POINT('Ctrl Pts',(-13.9559288115957,-3.22274914287197,
-0.00482335248839003));
#46896=CARTESIAN_POINT('Ctrl Pts',(-13.9556310724645,-3.2227391724512,-0.00964633599337804));
#46897=CARTESIAN_POINT('Ctrl Pts',(-13.9553333333333,-3.22271751746272,
-0.0144694553766564));
#46898=CARTESIAN_POINT('Origin',(-28.5777734492731,0.,0.));
#46899=CARTESIAN_POINT('',(-15.4527734492731,-3.21824294634175,0.00162490445582779));
#46900=CARTESIAN_POINT('',(-15.2062265507269,-3.22083845509468,-0.00278057450064706));
#46901=CARTESIAN_POINT('',(-28.5777734492731,-3.22275,-1.83004677902795E-13));
#46902=CARTESIAN_POINT('Ctrl Pts',(-15.4527734492731,-3.21824294634175,
0.00162490445582791));
#46903=CARTESIAN_POINT('Ctrl Pts',(-15.4132701471991,-3.21532481483233,
-0.640384640313474));
#46904=CARTESIAN_POINT('Ctrl Pts',(-15.3075078362952,-2.71776457270222,
-2.36340351127251));
#46905=CARTESIAN_POINT('Ctrl Pts',(-15.1354865165612,0.0916700791133597,
-3.81013263943217));
#46906=CARTESIAN_POINT('Ctrl Pts',(-14.9367094900712,3.25401315877339,-1.98409164271898));
#46907=CARTESIAN_POINT('Ctrl Pts',(-14.7379324635813,3.42904549919622,1.66304249739848));
#46908=CARTESIAN_POINT('Ctrl Pts',(-14.5391554370913,0.456596238902905,
3.78406071648658));
#46909=CARTESIAN_POINT('Ctrl Pts',(-14.3607690989886,-2.58767128823935,
2.56919539238608));
#46910=CARTESIAN_POINT('Ctrl Pts',(-14.2486417697158,-3.21434772016868,
0.74169766614858));
#46911=CARTESIAN_POINT('Ctrl Pts',(-14.2027734492731,-3.22023791762178,
-0.00239639078269425));
#46912=CARTESIAN_POINT('Ctrl Pts',(-15.2062265507269,-3.22083845509468,
-0.00278057450064713));
#46913=CARTESIAN_POINT('Ctrl Pts',(-15.186816197909,-3.22346391822557,-0.317588440328601));
#46914=CARTESIAN_POINT('Ctrl Pts',(-15.1011468362611,-3.03633781573977,
-1.70398423664175));
#46915=CARTESIAN_POINT('Ctrl Pts',(-14.9492184657832,-1.04956382363505,
-3.66415224416977));
#46916=CARTESIAN_POINT('Ctrl Pts',(-14.7504414392933,2.51414376359986,-2.86419653732846));
#46917=CARTESIAN_POINT('Ctrl Pts',(-14.5516644128032,3.76833505696647,0.563263663837553));
#46918=CARTESIAN_POINT('Ctrl Pts',(-14.3528873863133,1.56631945652084,3.47714249206992));
#46919=CARTESIAN_POINT('Ctrl Pts',(-14.1544080989545,-2.07437419278699,
3.19251685865474));
#46920=CARTESIAN_POINT('Ctrl Pts',(-14.0221878204257,-3.22237288338974,
1.0684457944476));
#46921=CARTESIAN_POINT('Ctrl Pts',(-13.9562265507269,-3.22274745212571,
-5.48329644236558E-7));
#46922=CARTESIAN_POINT('Origin',(-28.5777734492731,0.,0.));
#46923=CARTESIAN_POINT('',(-16.7027734492731,-3.2263940103205,0.00206690293443917));
#46924=CARTESIAN_POINT('',(-16.4562265507269,-3.21801998959411,0.00139469638163969));
#46925=CARTESIAN_POINT('',(-28.5777734492731,-3.22275,-1.83004677902795E-13));
#46926=CARTESIAN_POINT('Ctrl Pts',(-16.7027734492731,-3.2263940103205,0.002066902934439));
#46927=CARTESIAN_POINT('Ctrl Pts',(-16.6441575335124,-3.21933883299632,
-0.944434489197185));
#46928=CARTESIAN_POINT('Ctrl Pts',(-16.5192826089217,-2.27886282222011,
-2.97304725088416));
#46929=CARTESIAN_POINT('Ctrl Pts',(-16.3281486755011,1.17088524590524,-3.62687816153355));
#46930=CARTESIAN_POINT('Ctrl Pts',(-16.1293716490111,3.68372778490734,-0.977428557993123));
#46931=CARTESIAN_POINT('Ctrl Pts',(-15.9305946225211,2.81495659078308,2.56928160070777));
#46932=CARTESIAN_POINT('Ctrl Pts',(-15.7318175960312,-0.637899043196787,
3.75743726813516));
#46933=CARTESIAN_POINT('Ctrl Pts',(-15.5725438716151,-2.93536387380584,
1.94565869403867));
#46934=CARTESIAN_POINT('Ctrl Pts',(-15.4795291560291,-3.22021940569686,
0.436459923621029));
#46935=CARTESIAN_POINT('Ctrl Pts',(-15.4527734492731,-3.21824294634175,
0.00162490445582791));
#46936=CARTESIAN_POINT('Ctrl Pts',(-16.4562265507269,-3.21801998959411,
0.00139469638163962));
#46937=CARTESIAN_POINT('Ctrl Pts',(-16.4177035842223,-3.21558519819808,
-0.624793827959028));
#46938=CARTESIAN_POINT('Ctrl Pts',(-16.3129216088877,-2.73652383299444,
-2.3314605700088));
#46939=CARTESIAN_POINT('Ctrl Pts',(-16.1418806247231,0.0353578955585694,
-3.81103610176739));
#46940=CARTESIAN_POINT('Ctrl Pts',(-15.9431035982331,3.22428567725235,-2.0320448374088));
#46941=CARTESIAN_POINT('Ctrl Pts',(-15.7443265717431,3.45333495329863,1.6123015202179));
#46942=CARTESIAN_POINT('Ctrl Pts',(-15.5455495452532,0.512328175864222,
3.77664281656251));
#46943=CARTESIAN_POINT('Ctrl Pts',(-15.3661828715811,-2.56597725945458,
2.60115883494905));
#46944=CARTESIAN_POINT('Ctrl Pts',(-15.253075206739,-3.21450166048588,0.757036908181897));
#46945=CARTESIAN_POINT('Ctrl Pts',(-15.2062265507269,-3.22083845509468,
-0.00278057450064713));
#46946=CARTESIAN_POINT('Origin',(-28.5777734492731,0.,0.));
#46947=CARTESIAN_POINT('',(-17.9527734492731,-3.22471002427666,-0.0027024083209955));
#46948=CARTESIAN_POINT('',(-17.7062265507269,-3.22599478969022,0.00226260895499958));
#46949=CARTESIAN_POINT('',(-28.5777734492731,-3.22275,-1.83004677902795E-13));
#46950=CARTESIAN_POINT('Ctrl Pts',(-17.9527734492731,-3.22471002427666,
-0.00270240832099557));
#46951=CARTESIAN_POINT('Ctrl Pts',(-17.9413039286557,-3.22637486097873,
-0.188158555526165));
#46952=CARTESIAN_POINT('Ctrl Pts',(-17.8635753992083,-3.12731663875485,
-1.44321058791824));
#46953=CARTESIAN_POINT('Ctrl Pts',(-17.719587860931,-1.47950656459142,-3.51230314164857));
#46954=CARTESIAN_POINT('Ctrl Pts',(-17.520810834441,2.15348704471131,-3.14447240364953));
#46955=CARTESIAN_POINT('Ctrl Pts',(-17.322033807951,3.80960974798971,0.109939997816874));
#46956=CARTESIAN_POINT('Ctrl Pts',(-17.123256781461,1.96856401336108,3.2634289244733));
#46957=CARTESIAN_POINT('Ctrl Pts',(-16.924479754971,-1.67959578872999,3.42113600634526));
#46958=CARTESIAN_POINT('Ctrl Pts',(-16.7843186442417,-3.16479457102735,
1.31787827406947));
#46959=CARTESIAN_POINT('Ctrl Pts',(-16.7104165423424,-3.22731395460883,
0.125483864632017));
#46960=CARTESIAN_POINT('Ctrl Pts',(-16.7027734492731,-3.2263940103205,0.002066902934439));
#46961=CARTESIAN_POINT('Ctrl Pts',(-17.7062265507269,-3.22599478969022,
0.00226260895499947));
#46962=CARTESIAN_POINT('Ctrl Pts',(-17.6485909705356,-3.21857141243789,
-0.928709820430633));
#46963=CARTESIAN_POINT('Ctrl Pts',(-17.5246963815143,-2.30492056053424,
-2.94264957100572));
#46964=CARTESIAN_POINT('Ctrl Pts',(-17.334542783663,1.11714296776071,-3.64378942704172));
#46965=CARTESIAN_POINT('Ctrl Pts',(-17.135765757173,3.66887510281969,-1.03177786727233));
#46966=CARTESIAN_POINT('Ctrl Pts',(-16.936988730683,2.85263073953649,2.52739068741007));
#46967=CARTESIAN_POINT('Ctrl Pts',(-16.738211704193,-0.582287604380603,
3.76645122510734));
#46968=CARTESIAN_POINT('Ctrl Pts',(-16.5779576442077,-2.92058117340316,
1.97790330423196));
#46969=CARTESIAN_POINT('Ctrl Pts',(-16.4839625930523,-3.21977300820459,
0.452242411152104));
#46970=CARTESIAN_POINT('Ctrl Pts',(-16.4562265507269,-3.21801998959411,
0.00139469638163962));
#46971=CARTESIAN_POINT('Origin',(-28.5777734492731,0.,0.));
#46972=CARTESIAN_POINT('',(-19.2027734492731,-3.21757428963995,-0.000678758514853295));
#46973=CARTESIAN_POINT('',(-18.9562265507269,-3.22516952318429,-0.00257345280792048));
#46974=CARTESIAN_POINT('',(-28.5777734492731,-3.22275,-1.83004677902795E-13));
#46975=CARTESIAN_POINT('Ctrl Pts',(-19.2027734492731,-3.21757428963995,
-0.000678758514853252));
#46976=CARTESIAN_POINT('Ctrl Pts',(-19.172191314969,-3.21850772850764,-0.497962082277344));
#46977=CARTESIAN_POINT('Ctrl Pts',(-19.0753501718349,-2.87588199447191,
-2.07143695563862));
#46978=CARTESIAN_POINT('Ctrl Pts',(-18.9122500198708,-0.420152939479476,
-3.78796576074431));
#46979=CARTESIAN_POINT('Ctrl Pts',(-18.7134729933808,2.95844202985016,-2.40267223202429));
#46980=CARTESIAN_POINT('Ctrl Pts',(-18.5146959668909,3.62122866324853,1.18824074591766));
#46981=CARTESIAN_POINT('Ctrl Pts',(-18.3159189404009,0.959778114968857,
3.68836536418065));
#46982=CARTESIAN_POINT('Ctrl Pts',(-18.1286114345283,-2.37833073469481,
2.85373001603029));
#46983=CARTESIAN_POINT('Ctrl Pts',(-18.0075629374857,-3.21675715912152,
0.883214948664705));
#46984=CARTESIAN_POINT('Ctrl Pts',(-17.9527734492731,-3.22471002427666,
-0.00270240832099557));
#46985=CARTESIAN_POINT('Ctrl Pts',(-18.9562265507269,-3.2251695231843,-0.00257345280792092));
#46986=CARTESIAN_POINT('Ctrl Pts',(-18.9457373656789,-3.22664687306115,
-0.172115406970832));
#46987=CARTESIAN_POINT('Ctrl Pts',(-18.8689891718008,-3.13729927908916,
-1.41107459021403));
#46988=CARTESIAN_POINT('Ctrl Pts',(-18.7259819690928,-1.53126558554944,
-3.49004799470226));
#46989=CARTESIAN_POINT('Ctrl Pts',(-18.5272049426028,2.10676807472235,-3.17596246694));
#46990=CARTESIAN_POINT('Ctrl Pts',(-18.3284279161128,3.81081816296161,0.0536121173318595));
#46991=CARTESIAN_POINT('Ctrl Pts',(-18.1296508896229,2.01659055559616,3.23397151708182));
#46992=CARTESIAN_POINT('Ctrl Pts',(-17.9308738631329,-1.62883890977077,
3.44559039419421));
#46993=CARTESIAN_POINT('Ctrl Pts',(-17.7897324168342,-3.1555709823932,1.34996225449272));
#46994=CARTESIAN_POINT('Ctrl Pts',(-17.7148499793656,-3.22710547450993,
0.14155459287759));
#46995=CARTESIAN_POINT('Ctrl Pts',(-17.7062265507269,-3.22599478969022,
0.00226260895499947));
#46996=CARTESIAN_POINT('Origin',(-28.5777734492731,0.,0.));
#46997=CARTESIAN_POINT('',(-20.4527734492731,-3.22221210701407,0.00296761955232107));
#46998=CARTESIAN_POINT('',(-20.2062265507269,-3.21769251484553,-0.000932565804893093));
#46999=CARTESIAN_POINT('',(-28.5777734492731,-3.22275,-1.83004677902795E-13));
#47000=CARTESIAN_POINT('Ctrl Pts',(-20.4527734492731,-3.22221210701407,
0.00296761955232077));
#47001=CARTESIAN_POINT('Ctrl Pts',(-20.4030787012823,-3.21489552804955,
-0.802170257958906));
#47002=CARTESIAN_POINT('Ctrl Pts',(-20.2871249444615,-2.50155693228504,
-2.69237598717909));
#47003=CARTESIAN_POINT('Ctrl Pts',(-20.1049121788107,0.673860123029691,
-3.75114990807958));
#47004=CARTESIAN_POINT('Ctrl Pts',(-19.9061351523207,3.51934796221725,-1.4626698257142));
#47005=CARTESIAN_POINT('Ctrl Pts',(-19.7073581258307,3.13412367710237,2.16852066508976));
#47006=CARTESIAN_POINT('Ctrl Pts',(-19.5085810993407,-0.128182235481189,
3.80903956563999));
#47007=CARTESIAN_POINT('Ctrl Pts',(-19.3403862071549,-2.78901177056585,
2.2384811989213));
#47008=CARTESIAN_POINT('Ctrl Pts',(-19.238450323799,-3.21648534728463,0.579448009920417));
#47009=CARTESIAN_POINT('Ctrl Pts',(-19.2027734492731,-3.21757428963995,
-0.000678758514853252));
#47010=CARTESIAN_POINT('Ctrl Pts',(-20.2062265507269,-3.21769251484553,
-0.00093256580489396));
#47011=CARTESIAN_POINT('Ctrl Pts',(-20.1766247519921,-3.21893644686449,
-0.482230723198207));
#47012=CARTESIAN_POINT('Ctrl Pts',(-20.0807639444274,-2.89158218271902,
-2.03923190959996));
#47013=CARTESIAN_POINT('Ctrl Pts',(-19.9186441280327,-0.476102850960359,
-3.7813404214166));
#47014=CARTESIAN_POINT('Ctrl Pts',(-19.7198671015427,2.92260070569343,-2.44614276413548));
#47015=CARTESIAN_POINT('Ctrl Pts',(-19.5210900750527,3.63839775937779,1.13457968101029));
#47016=CARTESIAN_POINT('Ctrl Pts',(-19.3223130485627,1.01419664261627,3.67377387388617));
#47017=CARTESIAN_POINT('Ctrl Pts',(-19.1340252071208,-2.35341883760494,
2.8844660712419));
#47018=CARTESIAN_POINT('Ctrl Pts',(-19.0119963745089,-3.21731461911702,
0.898862155774589));
#47019=CARTESIAN_POINT('Ctrl Pts',(-18.9562265507269,-3.2251695231843,-0.00257345280792092));
#47020=CARTESIAN_POINT('Origin',(-28.5777734492731,0.,0.));
#47021=CARTESIAN_POINT('',(-21.7027734492731,-3.2278730893709,-0.000762706468288871));
#47022=CARTESIAN_POINT('',(-21.4562265507269,-3.22173931860895,0.00294029562399406));
#47023=CARTESIAN_POINT('',(-28.5777734492731,-3.22275,-1.83004677902795E-13));
#47024=CARTESIAN_POINT('Ctrl Pts',(-21.7027734492731,-3.2278730893709,-0.000762706468289505));
#47025=CARTESIAN_POINT('Ctrl Pts',(-21.7002250964256,-3.22800402191512,
-0.0418624340926581));
#47026=CARTESIAN_POINT('Ctrl Pts',(-21.631417734748,-3.20864937647278,-1.15145847964987));
#47027=CARTESIAN_POINT('Ctrl Pts',(-21.4963513642405,-1.93721818400033,
-3.28213326926849));
#47028=CARTESIAN_POINT('Ctrl Pts',(-21.2975743377506,1.71228483279679,-3.40489261991708));
#47029=CARTESIAN_POINT('Ctrl Pts',(-21.0987973112606,3.78993436216897,-0.402008244909776));
#47030=CARTESIAN_POINT('Ctrl Pts',(-20.9000202847706,2.38847724265994,2.96991406583087));
#47031=CARTESIAN_POINT('Ctrl Pts',(-20.7012432582806,-1.20556852363392,
3.6154968722977));
#47032=CARTESIAN_POINT('Ctrl Pts',(-20.5521609797814,-3.07107543849641,
1.61045897788706));
#47033=CARTESIAN_POINT('Ctrl Pts',(-20.4693377101123,-3.22465087020975,
0.271336297406685));
#47034=CARTESIAN_POINT('Ctrl Pts',(-20.4527734492731,-3.22221210701407,
0.00296761955232077));
#47035=CARTESIAN_POINT('Ctrl Pts',(-21.4562265507269,-3.22173931860895,
0.00294029562399399));
#47036=CARTESIAN_POINT('Ctrl Pts',(-21.4075121383054,-3.21471913280839,
-0.786608964437968));
#47037=CARTESIAN_POINT('Ctrl Pts',(-21.292538717054,-2.52408530047148,-2.66105030950266));
#47038=CARTESIAN_POINT('Ctrl Pts',(-21.1113062869725,0.618334760982468,
-3.76070092288226));
#47039=CARTESIAN_POINT('Ctrl Pts',(-20.9125292604826,3.49734092856599,-1.51453482522831));
#47040=CARTESIAN_POINT('Ctrl Pts',(-20.7137522339926,3.16583712036473,2.12195302366768));
#47041=CARTESIAN_POINT('Ctrl Pts',(-20.5149752075026,-0.0718608118791213,
3.81051772482967));
#47042=CARTESIAN_POINT('Ctrl Pts',(-20.3457999797474,-2.77125860116402,
2.2705412322501));
#47043=CARTESIAN_POINT('Ctrl Pts',(-20.2428837608221,-3.21615209908324,
0.59508012356279));
#47044=CARTESIAN_POINT('Ctrl Pts',(-20.2062265507269,-3.21769251484553,
-0.00093256580489396));
#47045=CARTESIAN_POINT('Origin',(-28.5777734492731,0.,0.));
#47046=CARTESIAN_POINT('',(-22.9527734492731,-3.21991554799802,-0.0025677011159218));
#47047=CARTESIAN_POINT('',(-22.7062265507269,-3.22800631070464,-0.000473251210255654));
#47048=CARTESIAN_POINT('',(-28.5777734492731,-3.22275,-1.83004677902795E-13));
#47049=CARTESIAN_POINT('Ctrl Pts',(-22.9527734492731,-3.21991554799802,
-0.00256770111592211));
#47050=CARTESIAN_POINT('Ctrl Pts',(-22.9311124827388,-3.22253028735674,
-0.35414605530089));
#47051=CARTESIAN_POINT('Ctrl Pts',(-22.8431925073746,-3.00720843641272,
-1.77805734035436));
#47052=CARTESIAN_POINT('Ctrl Pts',(-22.6890135231804,-0.924408668548408,
-3.69738843419269));
#47053=CARTESIAN_POINT('Ctrl Pts',(-22.4902364966904,2.60945901488757,-2.7777575280647));
#47054=CARTESIAN_POINT('Ctrl Pts',(-22.2914594702004,3.74787990632693,0.691815984784808));
#47055=CARTESIAN_POINT('Ctrl Pts',(-22.0926824437105,1.44579953705816,3.52631205824809));
#47056=CARTESIAN_POINT('Ctrl Pts',(-21.896453770068,-2.13697629406559,3.12886460489886));
#47057=CARTESIAN_POINT('Ctrl Pts',(-21.7664841052555,-3.22459968149505,
1.02676007562483));
#47058=CARTESIAN_POINT('Ctrl Pts',(-21.7027734492731,-3.2278730893709,-0.000762706468289505));
#47059=CARTESIAN_POINT('Ctrl Pts',(-22.7062265507269,-3.22800631070464,
-0.000473251210255806));
#47060=CARTESIAN_POINT('Ctrl Pts',(-22.7046585334487,-3.22805805244852,
-0.025759358427327));
#47061=CARTESIAN_POINT('Ctrl Pts',(-22.6368315073406,-3.21632122210707,
-1.11949996844933));
#47062=CARTESIAN_POINT('Ctrl Pts',(-22.5027454724024,-1.9855246223874,-3.2531371345379));
#47063=CARTESIAN_POINT('Ctrl Pts',(-22.3039684459124,1.66176444014233,-3.4298321060602));
#47064=CARTESIAN_POINT('Ctrl Pts',(-22.1051914194224,3.78357703340158,-0.45798924048176));
#47065=CARTESIAN_POINT('Ctrl Pts',(-21.9064143929325,2.43211891370082,2.93428132400969));
#47066=CARTESIAN_POINT('Ctrl Pts',(-21.7076373664425,-1.15199029393737,
3.63292274535707));
#47067=CARTESIAN_POINT('Ctrl Pts',(-21.557574752374,-3.05939350818334,1.64267923939091));
#47068=CARTESIAN_POINT('Ctrl Pts',(-21.4737711471354,-3.2242676530476,0.287298094966756));
#47069=CARTESIAN_POINT('Ctrl Pts',(-21.4562265507269,-3.22173931860895,
0.00294029562399399));
#47070=CARTESIAN_POINT('Origin',(-28.5777734492731,0.,0.));
#47071=CARTESIAN_POINT('',(-24.2027734492731,-3.21858419309814,0.00190193480539803));
#47072=CARTESIAN_POINT('',(-23.9562265507269,-3.22031942372998,-0.00269217174386716));
#47073=CARTESIAN_POINT('',(-28.5777734492731,-3.22275,-1.83004677902795E-13));
#47074=CARTESIAN_POINT('Ctrl Pts',(-24.2027734492731,-3.21858419309814,
0.00190193480539787));
#47075=CARTESIAN_POINT('Ctrl Pts',(-24.1619998690521,-3.21503940788334,
-0.660581282227665));
#47076=CARTESIAN_POINT('Ctrl Pts',(-24.0549672800012,-2.69295281648875,
-2.40476065474808));
#47077=CARTESIAN_POINT('Ctrl Pts',(-23.8816756821203,0.16465828588852,-3.80763393731814));
#47078=CARTESIAN_POINT('Ctrl Pts',(-23.6828986556303,3.29137222988386,-1.92148011273296));
#47079=CARTESIAN_POINT('Ctrl Pts',(-23.4841216291403,3.39665395902081,1.72857147389278));
#47080=CARTESIAN_POINT('Ctrl Pts',(-23.2853446026503,0.383854227871474,
3.79181560291581));
#47081=CARTESIAN_POINT('Ctrl Pts',(-23.1082285426946,-2.61461116784304,
2.52870393023895));
#47082=CARTESIAN_POINT('Ctrl Pts',(-22.9973714915688,-3.21453202753838,
0.721301489366681));
#47083=CARTESIAN_POINT('Ctrl Pts',(-22.9527734492731,-3.21991554799802,
-0.00256770111592211));
#47084=CARTESIAN_POINT('Ctrl Pts',(-23.9562265507269,-3.22031942372998,
-0.00269217174386771));
#47085=CARTESIAN_POINT('Ctrl Pts',(-23.935545919762,-3.22295957829101,-0.338252521270422));
#47086=CARTESIAN_POINT('Ctrl Pts',(-23.8486062799671,-3.02010243966437,
-1.74580737059892));
#47087=CARTESIAN_POINT('Ctrl Pts',(-23.6954076313422,-0.978964290720696,
-3.68331844135819));
#47088=CARTESIAN_POINT('Ctrl Pts',(-23.4966306048523,2.56811106183178,-2.81602834885952));
#47089=CARTESIAN_POINT('Ctrl Pts',(-23.2978535783623,3.75769675477037,0.636337094806224));
#47090=CARTESIAN_POINT('Ctrl Pts',(-23.0990765518723,1.49776930770217,3.50455359875708));
#47091=CARTESIAN_POINT('Ctrl Pts',(-22.9018675426605,-2.10841635961811,
3.15839155315196));
#47092=CARTESIAN_POINT('Ctrl Pts',(-22.7709175422787,-3.22587162458688,
1.04274442956557));
#47093=CARTESIAN_POINT('Ctrl Pts',(-22.7062265507269,-3.22800631070464,
-0.000473251210255806));
#47094=CARTESIAN_POINT('Origin',(-28.5777734492731,0.,0.));
#47095=CARTESIAN_POINT('',(-25.4527734492731,-3.22681880944319,0.00198271668292594));
#47096=CARTESIAN_POINT('',(-25.2062265507269,-3.2183080224723,0.00170933992184319));
#47097=CARTESIAN_POINT('',(-28.5777734492731,-3.22275,-1.83004677902795E-13));
#47098=CARTESIAN_POINT('Ctrl Pts',(-25.4527734492731,-3.22681880944319,
0.00198271668292602));
#47099=CARTESIAN_POINT('Ctrl Pts',(-25.3928872553654,-3.22038563950992,
-0.964597122860873));
#47100=CARTESIAN_POINT('Ctrl Pts',(-25.2667420526278,-2.244579208324,-3.01256650610898));
#47101=CARTESIAN_POINT('Ctrl Pts',(-25.0743378410601,1.24018106922513,-3.60361128581411));
#47102=CARTESIAN_POINT('Ctrl Pts',(-24.8755608145702,3.70175213266751,-0.906781358690897));
#47103=CARTESIAN_POINT('Ctrl Pts',(-24.6767837880802,2.76524014159366,2.62277736241376));
#47104=CARTESIAN_POINT('Ctrl Pts',(-24.4780067615902,-0.709761474991402,
3.74450018637222));
#47105=CARTESIAN_POINT('Ctrl Pts',(-24.3200033153212,-2.95404409032814,
1.90388762973689));
#47106=CARTESIAN_POINT('Ctrl Pts',(-24.2282588778821,-3.22079985260207,
0.415985482065448));
#47107=CARTESIAN_POINT('Ctrl Pts',(-24.2027734492731,-3.21858419309814,
0.00190193480539787));
#47108=CARTESIAN_POINT('Ctrl Pts',(-25.2062265507269,-3.2183080224723,0.00170933992184336));
#47109=CARTESIAN_POINT('Ctrl Pts',(-25.1664333060753,-3.21525215568242,
-0.644987807253467));
#47110=CARTESIAN_POINT('Ctrl Pts',(-25.0603810525937,-2.71217295639817,
-2.37289324999516));
#47111=CARTESIAN_POINT('Ctrl Pts',(-24.8880697902821,0.108362070287417,
-3.80963202337103));
#47112=CARTESIAN_POINT('Ctrl Pts',(-24.6892927637921,3.26260339792463,-1.96993487649339));
#47113=CARTESIAN_POINT('Ctrl Pts',(-24.4905157373022,3.42183734109356,1.67817626036435));
#47114=CARTESIAN_POINT('Ctrl Pts',(-24.2917387108122,0.439863865693541,
3.78572376365049));
#47115=CARTESIAN_POINT('Ctrl Pts',(-24.1136423152871,-2.59364198095809,
2.56033371879188));
#47116=CARTESIAN_POINT('Ctrl Pts',(-24.001804928592,-3.21450074428982,0.73685472279883));
#47117=CARTESIAN_POINT('Ctrl Pts',(-23.9562265507269,-3.22031942372998,
-0.00269217174386771));
#47118=CARTESIAN_POINT('Origin',(-13.9553333333333,5.160062080289E-16,2.1385152528819E-16));
#47119=CARTESIAN_POINT('',(-13.9553333333333,3.88062570733445,0.639713310456302));
#47120=CARTESIAN_POINT('Ctrl Pts',(-13.9553333333333,-1.03598926702577,
-3.05747757600545));
#47121=CARTESIAN_POINT('Ctrl Pts',(-13.9553333333333,-0.97444439476585,
-3.08634227761202));
#47122=CARTESIAN_POINT('Ctrl Pts',(-13.9553333333333,-0.912020754771081,
-3.11307510025756));
#47123=CARTESIAN_POINT('Ctrl Pts',(-13.9553333333333,-0.848797833127659,
-3.13759945495693));
#47124=CARTESIAN_POINT('Ctrl Pts',(-13.9553333333333,-0.753122772179508,
-3.17471208862814));
#47125=CARTESIAN_POINT('Ctrl Pts',(-13.9553333333333,-0.655618687658207,
-3.20676979988523));
#47126=CARTESIAN_POINT('Ctrl Pts',(-13.9553333333333,-0.55665830230821,
-3.23392646990319));
#47127=CARTESIAN_POINT('Ctrl Pts',(-13.9553333333333,-0.494205049156755,
-3.25106486706469));
#47128=CARTESIAN_POINT('Ctrl Pts',(-13.9553333333333,-0.431171105772932,
-3.26625041147114));
#47129=CARTESIAN_POINT('Ctrl Pts',(-13.9553333333333,-0.367644747143531,
-3.27951281571112));
#47130=CARTESIAN_POINT('Ctrl Pts',(-13.9553333333333,-0.327047912649835,
-3.28798822090568));
#47131=CARTESIAN_POINT('Ctrl Pts',(-13.9553333333333,-0.286249902435637,
-3.29567809271961));
#47132=CARTESIAN_POINT('Ctrl Pts',(-13.9553333333333,-0.245273098295,-3.3025886978361));
#47133=CARTESIAN_POINT('Ctrl Pts',(-13.9553333333333,-0.226865840120677,
-3.30569302222615));
#47134=CARTESIAN_POINT('Ctrl Pts',(-13.9553333333333,-0.20842389272401,
-3.30863977526898));
#47135=CARTESIAN_POINT('Ctrl Pts',(-13.9553333333333,-0.189961491201516,
-3.31142788908956));
#47136=CARTESIAN_POINT('Ctrl Pts',(-13.9553333333333,-0.0850514468879583,
-3.3272709604317));
#47137=CARTESIAN_POINT('Ctrl Pts',(-13.9553333333333,0.0206223431908923,
-3.33801358018381));
#47138=CARTESIAN_POINT('Ctrl Pts',(-13.9553333333333,0.126670272884673,
-3.34381218349164));
#47139=CARTESIAN_POINT('Ctrl Pts',(-13.9553333333333,0.227783133662497,
-3.34934094176786));
#47140=CARTESIAN_POINT('Ctrl Pts',(-13.9553333333333,0.329236905662223,
-3.35037480537384));
#47141=CARTESIAN_POINT('Ctrl Pts',(-13.9553333333333,0.430711103724674,
-3.34701090757602));
#47142=CARTESIAN_POINT('Ctrl Pts',(-13.9553333333333,0.475106065376996,
-3.34553920228947));
#47143=CARTESIAN_POINT('Ctrl Pts',(-13.9553333333333,0.519505098103338,
-3.34322525460124));
#47144=CARTESIAN_POINT('Ctrl Pts',(-13.9553333333333,0.563881915333782,
-3.34007494530072));
#47145=CARTESIAN_POINT('Ctrl Pts',(-13.9553333333333,0.58584474718944,-3.33851580433977));
#47146=CARTESIAN_POINT('Ctrl Pts',(-13.9553333333333,0.607802140900022,
-3.33675178165321));
#47147=CARTESIAN_POINT('Ctrl Pts',(-13.9553333333333,0.629750923720838,
-3.33478346606831));
#47148=CARTESIAN_POINT('Ctrl Pts',(-13.9553333333333,0.645395419510362,
-3.33338050422156));
#47149=CARTESIAN_POINT('Ctrl Pts',(-13.9553333333333,0.6610330550259,-3.33187393535576));
#47150=CARTESIAN_POINT('Ctrl Pts',(-13.9553333333333,0.676654075413203,
-3.33026504772646));
#47151=CARTESIAN_POINT('Ctrl Pts',(-13.9553333333333,0.787358794894414,
-3.31886301064675));
#47152=CARTESIAN_POINT('Ctrl Pts',(-13.9553333333333,0.897351501643973,
-3.30231524241035));
#47153=CARTESIAN_POINT('Ctrl Pts',(-13.9553333333333,1.00622074539013,-3.28078416772688));
#47154=CARTESIAN_POINT('Ctrl Pts',(-13.9553333333333,1.11680331542352,-3.25891424843516));
#47155=CARTESIAN_POINT('Ctrl Pts',(-13.9553333333333,1.22622766989774,-3.23190302698969));
#47156=CARTESIAN_POINT('Ctrl Pts',(-13.9553333333333,1.33407670763527,-3.19986895694082));
#47157=CARTESIAN_POINT('Ctrl Pts',(-13.9553333333333,1.44167031624772,-3.16791075622427));
#47158=CARTESIAN_POINT('Ctrl Pts',(-13.9553333333333,1.54769701641018,-3.13095340796043));
#47159=CARTESIAN_POINT('Ctrl Pts',(-13.9553333333333,1.65174263467817,-3.08906346075735));
#47160=CARTESIAN_POINT('Ctrl Pts',(-13.9553333333333,1.71930029668252,-3.06186397901429));
#47161=CARTESIAN_POINT('Ctrl Pts',(-13.9553333333333,1.78602270026487,-3.03258387425711));
#47162=CARTESIAN_POINT('Ctrl Pts',(-13.9553333333333,1.85179353602905,-3.00122997196956));
#47163=CARTESIAN_POINT('Ctrl Pts',(-13.9553333333333,1.87027794232932,-2.99241818993504));
#47164=CARTESIAN_POINT('Ctrl Pts',(-13.9553333333333,1.88868716769718,-2.98344255502655));
#47165=CARTESIAN_POINT('Ctrl Pts',(-13.9553333333333,1.90701857443447,-2.97430309205569));
#47166=CARTESIAN_POINT('Ctrl Pts',(-13.9553333333333,1.92415095587783,-2.96576142539321));
#47167=CARTESIAN_POINT('Ctrl Pts',(-13.9553333333333,1.94121695803161,-2.95707572927031));
#47168=CARTESIAN_POINT('Ctrl Pts',(-13.9553333333333,1.95819482658923,-2.94825646251065));
#47169=CARTESIAN_POINT('Ctrl Pts',(-13.9553333333333,2.06098978668038,-2.89485893669543));
#47170=CARTESIAN_POINT('Ctrl Pts',(-13.9553333333333,2.16071563092277,-2.83649011388479));
#47171=CARTESIAN_POINT('Ctrl Pts',(-13.9553333333333,2.25694248996472,-2.7732788016416));
#47172=CARTESIAN_POINT('Ctrl Pts',(-13.9553333333333,2.30934153235369,-2.73885793139112));
#47173=CARTESIAN_POINT('Ctrl Pts',(-13.9553333333333,2.36070308712004,-2.70300025428149));
#47174=CARTESIAN_POINT('Ctrl Pts',(-13.9553333333333,2.41095698484776,-2.66572010901368));
#47175=CARTESIAN_POINT('Ctrl Pts',(-13.9553333333333,2.50006598058015,-2.59961585728836));
#47176=CARTESIAN_POINT('Ctrl Pts',(-13.9553333333333,2.58569399841725,-2.529041984421));
#47177=CARTESIAN_POINT('Ctrl Pts',(-13.9553333333333,2.66776425450739,-2.45437987478522));
#47178=CARTESIAN_POINT('Ctrl Pts',(-13.9553333333333,2.75139660323382,-2.37829667622846));
#47179=CARTESIAN_POINT('Ctrl Pts',(-13.9553333333333,2.83133495883862,-2.29796765658672));
#47180=CARTESIAN_POINT('Ctrl Pts',(-13.9553333333333,2.90746923279272,-2.21375050651505));
#47181=CARTESIAN_POINT('Ctrl Pts',(-13.9553333333333,2.93145580090933,-2.187217378899));
#47182=CARTESIAN_POINT('Ctrl Pts',(-13.9553333333333,2.95506453274937,-2.1602980072191));
#47183=CARTESIAN_POINT('Ctrl Pts',(-13.9553333333333,2.97829128499789,-2.13300278094868));
#47184=CARTESIAN_POINT('Ctrl Pts',(-13.9553333333333,2.98871016252315,-2.12075889870061));
#47185=CARTESIAN_POINT('Ctrl Pts',(-13.9553333333333,2.99905384204844,-2.10843736379202));
#47186=CARTESIAN_POINT('Ctrl Pts',(-13.9553333333333,3.00931636832518,-2.09604582041943));
#47187=CARTESIAN_POINT('Ctrl Pts',(-13.9553333333333,3.08191587225961,-2.00838515309711));
#47188=CARTESIAN_POINT('Ctrl Pts',(-13.9553333333333,3.15031706995574,-1.91739553524079));
#47189=CARTESIAN_POINT('Ctrl Pts',(-13.9553333333333,3.21445896366597,-1.82349417167357));
#47190=CARTESIAN_POINT('Ctrl Pts',(-13.9553333333333,3.28071257870846,-1.72650132606391));
#47191=CARTESIAN_POINT('Ctrl Pts',(-13.9553333333333,3.34242236519139,-1.62640143226605));
#47192=CARTESIAN_POINT('Ctrl Pts',(-13.9553333333333,3.39949212600865,-1.52360685487494));
#47193=CARTESIAN_POINT('Ctrl Pts',(-13.9553333333333,3.45713807462249,-1.41977444273214));
#47194=CARTESIAN_POINT('Ctrl Pts',(-13.9553333333333,3.51005033110595,-1.31319198625781));
#47195=CARTESIAN_POINT('Ctrl Pts',(-13.9553333333333,3.55809281339713,-1.2042455082145));
#47196=CARTESIAN_POINT('Ctrl Pts',(-13.9553333333333,3.5898550154717,-1.13221800493205));
#47197=CARTESIAN_POINT('Ctrl Pts',(-13.9553333333333,3.61948792025525,-1.05915642697356));
#47198=CARTESIAN_POINT('Ctrl Pts',(-13.9553333333333,3.64694183534205,-0.985165363120071));
#47199=CARTESIAN_POINT('Ctrl Pts',(-13.9553333333333,3.66035272037872,-0.949021678405428));
#47200=CARTESIAN_POINT('Ctrl Pts',(-13.9553333333333,3.67324352307887,-0.912656128563678));
#47201=CARTESIAN_POINT('Ctrl Pts',(-13.9553333333333,3.685607658247,-0.876080550583037));
#47202=CARTESIAN_POINT('Ctrl Pts',(-13.9553333333333,3.69331037373375,-0.853294381787787));
#47203=CARTESIAN_POINT('Ctrl Pts',(-13.9553333333333,3.70081038899666,-0.830420968477908));
#47204=CARTESIAN_POINT('Ctrl Pts',(-13.9553333333333,3.70809603678459,-0.807495459346133));
#47205=CARTESIAN_POINT('Ctrl Pts',(-13.9553333333333,3.74524699475371,-0.69059375740188));
#47206=CARTESIAN_POINT('Ctrl Pts',(-13.9553333333333,3.77687334741109,-0.572212458485722));
#47207=CARTESIAN_POINT('Ctrl Pts',(-13.9553333333333,3.80287284700866,-0.452783927385374));
#47208=CARTESIAN_POINT('Ctrl Pts',(-13.9553333333333,3.82890220860145,-0.33321822540557));
#47209=CARTESIAN_POINT('Ctrl Pts',(-13.9553333333333,3.84929223191143,-0.212602085015147));
#47210=CARTESIAN_POINT('Ctrl Pts',(-13.9553333333333,3.86389824005303,-0.0913379545200216));
#47211=CARTESIAN_POINT('Ctrl Pts',(-13.9553333333333,3.87847911324018,0.0297174968913304));
#47212=CARTESIAN_POINT('Ctrl Pts',(-13.9553333333333,3.88729629975811,0.15141952707811));
#47213=CARTESIAN_POINT('Ctrl Pts',(-13.9553333333333,3.89015735625761,0.273386919606757));
#47214=CARTESIAN_POINT('Ctrl Pts',(-13.9553333333333,3.8930184127571,0.395354312135403));
#47215=CARTESIAN_POINT('Ctrl Pts',(-13.9553333333333,3.88992381340402,0.517587896581017));
#47216=CARTESIAN_POINT('Ctrl Pts',(-13.9553333333333,3.88062570733445,0.639713310456302));
#47217=CARTESIAN_POINT('',(-13.9553333333333,-3.933,-4.81653586104654E-16));
#47218=CARTESIAN_POINT('Origin',(-13.9553333333333,0.,0.));
#47219=CARTESIAN_POINT('',(-13.9553333333333,1.83776796987408,3.48100466478169));
#47220=CARTESIAN_POINT('Origin',(-13.9553333333333,0.,0.));
#47221=CARTESIAN_POINT('Ctrl Pts',(-13.9553333333333,1.83875391880586,3.48426281672735));
#47222=CARTESIAN_POINT('Ctrl Pts',(-13.9553333333333,1.76308895516893,3.51647153040244));
#47223=CARTESIAN_POINT('Ctrl Pts',(-13.9553333333333,1.68643718119151,3.54609006161243));
#47224=CARTESIAN_POINT('Ctrl Pts',(-13.9553333333333,1.60886810215454,3.57300966796364));
#47225=CARTESIAN_POINT('Ctrl Pts',(-13.9553333333333,1.49409022882316,3.61284223019423));
#47226=CARTESIAN_POINT('Ctrl Pts',(-13.9553333333333,1.37730380720653,3.64676788490432));
#47227=CARTESIAN_POINT('Ctrl Pts',(-13.9553333333333,1.25894917601004,3.67487673179449));
#47228=CARTESIAN_POINT('Ctrl Pts',(-13.9553333333333,1.19042394189699,3.69115125603004));
#47229=CARTESIAN_POINT('Ctrl Pts',(-13.9553333333333,1.12137289144904,3.7054748768118));
#47230=CARTESIAN_POINT('Ctrl Pts',(-13.9553333333333,1.05188174504114,3.7178572191697));
#47231=CARTESIAN_POINT('Ctrl Pts',(-13.9553333333333,0.99900121609365,3.7272797837314));
#47232=CARTESIAN_POINT('Ctrl Pts',(-13.9553333333333,0.945865841074519,
3.73557809047345));
#47233=CARTESIAN_POINT('Ctrl Pts',(-13.9553333333333,0.892513862605538,
3.74275424069541));
#47234=CARTESIAN_POINT('Ctrl Pts',(-13.9553333333333,0.870373911505189,
3.74573219239584));
#47235=CARTESIAN_POINT('Ctrl Pts',(-13.9553333333333,0.848195262249248,
3.74851695984359));
#47236=CARTESIAN_POINT('Ctrl Pts',(-13.9553333333333,0.825998844565343,
3.75110673049074));
#47237=CARTESIAN_POINT('Ctrl Pts',(-13.9553333333333,0.70366659282493,3.76537986587987));
#47238=CARTESIAN_POINT('Ctrl Pts',(-13.9553333333333,0.580670158678774,
3.77375230856627));
#47239=CARTESIAN_POINT('Ctrl Pts',(-13.9553333333333,0.457468363331996,
3.77631420882323));
#47240=CARTESIAN_POINT('Ctrl Pts',(-13.9553333333333,0.349666792403565,
3.77855587154807));
#47241=CARTESIAN_POINT('Ctrl Pts',(-13.9553333333333,0.241707527928521,
3.77634785611784));
#47242=CARTESIAN_POINT('Ctrl Pts',(-13.9553333333333,0.133905126459,3.76971649396968));
#47243=CARTESIAN_POINT('Ctrl Pts',(-13.9553333333333,0.0867415758160847,
3.76681527302986));
#47244=CARTESIAN_POINT('Ctrl Pts',(-13.9553333333333,0.039608186703455,
3.76306699939609));
#47245=CARTESIAN_POINT('Ctrl Pts',(-13.9553333333333,-0.0074678918743757,
3.75847207198772));
#47246=CARTESIAN_POINT('Ctrl Pts',(-13.9553333333333,-0.0364097747536519,
3.75564715846669));
#47247=CARTESIAN_POINT('Ctrl Pts',(-13.9553333333333,-0.0653299851271169,
3.75250221724033));
#47248=CARTESIAN_POINT('Ctrl Pts',(-13.9553333333333,-0.0942220930405801,
3.74903714231532));
#47249=CARTESIAN_POINT('Ctrl Pts',(-13.9553333333333,-0.116528637892405,
3.74636188409391));
#47250=CARTESIAN_POINT('Ctrl Pts',(-13.9553333333333,-0.138821572577901,
3.74349527660291));
#47251=CARTESIAN_POINT('Ctrl Pts',(-13.9553333333333,-0.161073145138907,
3.74044087441143));
#47252=CARTESIAN_POINT('Ctrl Pts',(-13.9553333333333,-0.278854314400997,
3.72427343004213));
#47253=CARTESIAN_POINT('Ctrl Pts',(-13.9553333333333,-0.395616864311933,
3.70283345101575));
#47254=CARTESIAN_POINT('Ctrl Pts',(-13.9553333333333,-0.510952667895199,
3.67619809061088));
#47255=CARTESIAN_POINT('Ctrl Pts',(-13.9553333333333,-0.625434416051205,
3.64975996361839));
#47256=CARTESIAN_POINT('Ctrl Pts',(-13.9553333333333,-0.738511305521624,
3.61820279633032));
#47257=CARTESIAN_POINT('Ctrl Pts',(-13.9553333333333,-0.849764871990641,
3.58155482781478));
#47258=CARTESIAN_POINT('Ctrl Pts',(-13.9553333333333,-0.957731897995734,
3.54598947656061));
#47259=CARTESIAN_POINT('Ctrl Pts',(-13.9553333333333,-1.06398233874069,
3.5056292399093));
#47260=CARTESIAN_POINT('Ctrl Pts',(-13.9553333333333,-1.16810511106794,
3.46046090716126));
#47261=CARTESIAN_POINT('Ctrl Pts',(-13.9553333333333,-1.23784694811165,
3.43020698257164));
#47262=CARTESIAN_POINT('Ctrl Pts',(-13.9553333333333,-1.30663363739179,
3.39779517970804));
#47263=CARTESIAN_POINT('Ctrl Pts',(-13.9553333333333,-1.37433213984351,
3.36321258891611));
#47264=CARTESIAN_POINT('Ctrl Pts',(-13.9553333333333,-1.40712864407733,
3.34645907082858));
#47265=CARTESIAN_POINT('Ctrl Pts',(-13.9553333333333,-1.43966963403488,
3.32919598381487));
#47266=CARTESIAN_POINT('Ctrl Pts',(-13.9553333333333,-1.47193922015119,
3.31142128892406));
#47267=CARTESIAN_POINT('Ctrl Pts',(-13.9553333333333,-1.48558859579644,
3.30390295613014));
#47268=CARTESIAN_POINT('Ctrl Pts',(-13.9553333333333,-1.49918555024823,
3.29629517051011));
#47269=CARTESIAN_POINT('Ctrl Pts',(-13.9553333333333,-1.51272211910769,
3.28860190887891));
#47270=CARTESIAN_POINT('Ctrl Pts',(-13.9553333333333,-1.60994673400505,
3.23334607505838));
#47271=CARTESIAN_POINT('Ctrl Pts',(-13.9553333333333,-1.70416783551671,
3.17362426881821));
#47272=CARTESIAN_POINT('Ctrl Pts',(-13.9553333333333,-1.79501394372711,
3.10946096733353));
#47273=CARTESIAN_POINT('Ctrl Pts',(-13.9553333333333,-1.84679517267689,
3.07288862901545));
#47274=CARTESIAN_POINT('Ctrl Pts',(-13.9553333333333,-1.8974793779626,3.03487255871099));
#47275=CARTESIAN_POINT('Ctrl Pts',(-13.9553333333333,-1.94699263852852,
2.99541163692221));
#47276=CARTESIAN_POINT('Ctrl Pts',(-13.9553333333333,-2.03553331123934,
2.9248467716511));
#47277=CARTESIAN_POINT('Ctrl Pts',(-13.9553333333333,-2.12033217628919,
2.84966300167236));
#47278=CARTESIAN_POINT('Ctrl Pts',(-13.9553333333333,-2.2012244629001,2.77024331980942));
#47279=CARTESIAN_POINT('Ctrl Pts',(-13.9553333333333,-2.28247472756623,
2.6904721767077));
#47280=CARTESIAN_POINT('Ctrl Pts',(-13.9553333333333,-2.35978409856056,
2.606426642024));
#47281=CARTESIAN_POINT('Ctrl Pts',(-13.9553333333333,-2.43293781738034,
2.51847398269812));
#47282=CARTESIAN_POINT('Ctrl Pts',(-13.9553333333333,-2.45500011328369,
2.49194850146709));
#47283=CARTESIAN_POINT('Ctrl Pts',(-13.9553333333333,-2.47668408288072,
2.46506755442072));
#47284=CARTESIAN_POINT('Ctrl Pts',(-13.9553333333333,-2.49798291570529,
2.43784103819821));
#47285=CARTESIAN_POINT('Ctrl Pts',(-13.9553333333333,-2.50883358180945,
2.42397052054389));
#47286=CARTESIAN_POINT('Ctrl Pts',(-13.9553333333333,-2.51958518129152,
2.41000901037187));
#47287=CARTESIAN_POINT('Ctrl Pts',(-13.9553333333333,-2.53022550926122,
2.39597302308478));
#47288=CARTESIAN_POINT('Ctrl Pts',(-13.9553333333333,-2.59749517874235,
2.30723551157832));
#47289=CARTESIAN_POINT('Ctrl Pts',(-13.9553333333333,-2.66042616738569,
2.21539127565337));
#47290=CARTESIAN_POINT('Ctrl Pts',(-13.9553333333333,-2.71889127549631,
2.12082239717396));
#47291=CARTESIAN_POINT('Ctrl Pts',(-13.9553333333333,-2.77741263197492,
2.02616253545261));
#47292=CARTESIAN_POINT('Ctrl Pts',(-13.9553333333333,-2.83145977799374,
1.92877187196212));
#47293=CARTESIAN_POINT('Ctrl Pts',(-13.9553333333333,-2.88085709477908,
1.82901312880459));
#47294=CARTESIAN_POINT('Ctrl Pts',(-13.9553333333333,-2.92964767956841,
1.73047969149956));
#47295=CARTESIAN_POINT('Ctrl Pts',(-13.9553333333333,-2.97390210276449,
1.62963512353767));
#47296=CARTESIAN_POINT('Ctrl Pts',(-13.9553333333333,-3.01340139041157,
1.52682226668093));
#47297=CARTESIAN_POINT('Ctrl Pts',(-13.9553333333333,-3.03691137670684,
1.46562802750184));
#47298=CARTESIAN_POINT('Ctrl Pts',(-13.9553333333333,-3.05873583260475,
1.4037364305582));
#47299=CARTESIAN_POINT('Ctrl Pts',(-13.9553333333333,-3.07881973126231,
1.34122049792282));
#47300=CARTESIAN_POINT('Ctrl Pts',(-13.9553333333333,-3.08803506168237,
1.31253558043859));
#47301=CARTESIAN_POINT('Ctrl Pts',(-13.9553333333333,-3.0968838486815,1.28371923382974));
#47302=CARTESIAN_POINT('Ctrl Pts',(-13.9553333333333,-3.10536029103769,
1.25477861820457));
#47303=CARTESIAN_POINT('Ctrl Pts',(-13.9553333333333,-3.10926402172898,
1.24145034147085));
#47304=CARTESIAN_POINT('Ctrl Pts',(-13.9553333333333,-3.11308820868124,
1.22809751314922));
#47305=CARTESIAN_POINT('Ctrl Pts',(-13.9553333333333,-3.11682997167633,
1.21472968520499));
#47306=CARTESIAN_POINT('Ctrl Pts',(-13.9553333333333,-3.14582478574141,
1.11114277010499));
#47307=CARTESIAN_POINT('Ctrl Pts',(-13.9553333333333,-3.16991857070316,
1.00650635296175));
#47308=CARTESIAN_POINT('Ctrl Pts',(-13.9553333333333,-3.18895492093138,
0.901150303424905));
#47309=CARTESIAN_POINT('Ctrl Pts',(-13.9553333333333,-3.20772681944474,
0.797257853140867));
#47310=CARTESIAN_POINT('Ctrl Pts',(-13.9553333333333,-3.22158089463548,
0.692664846008168));
#47311=CARTESIAN_POINT('Ctrl Pts',(-13.9553333333333,-3.23031744579328,
0.587688020009249));
#47312=CARTESIAN_POINT('Ctrl Pts',(-13.9553333333333,-3.2387841631479,0.485953468414905));
#47313=CARTESIAN_POINT('Ctrl Pts',(-13.9553333333333,-3.24244450620772,
0.383857830419708));
#47314=CARTESIAN_POINT('Ctrl Pts',(-13.9553333333333,-3.24107000631815,
0.281699843730534));
#47315=CARTESIAN_POINT('Ctrl Pts',(-13.9553333333333,-3.23974122264024,
0.182939657345128));
#47316=CARTESIAN_POINT('Ctrl Pts',(-13.9553333333333,-3.23370683694308,
0.0841207460689442));
#47317=CARTESIAN_POINT('Ctrl Pts',(-13.9553333333333,-3.22271751746272,
-0.0144694553766564));
#47318=CARTESIAN_POINT('Ctrl Pts',(-26.6770630286919,-1.43290239521325,
2.88667772504866));
#47319=CARTESIAN_POINT('Ctrl Pts',(-26.6108040198619,-2.39432226019554,
2.40944370083299));
#47320=CARTESIAN_POINT('Ctrl Pts',(-26.478286002202,-3.78590739708692,0.426683950034108));
#47321=CARTESIAN_POINT('Ctrl Pts',(-26.2795089757119,-2.40485858874901,
-2.95981954148459));
#47322=CARTESIAN_POINT('Ctrl Pts',(-26.080731949222,1.18722242799118,-3.6205134943868));
#47323=CARTESIAN_POINT('Ctrl Pts',(-25.881954922732,3.68771187601412,-0.961936478150598));
#47324=CARTESIAN_POINT('Ctrl Pts',(-25.683177896242,2.80382800818523,2.58188775682714));
#47325=CARTESIAN_POINT('Ctrl Pts',(-25.4844008697521,-0.654391852565681,
3.75444098441731));
#47326=CARTESIAN_POINT('Ctrl Pts',(-25.2856238432621,-3.51165133563114,
1.48105475903402));
#47327=CARTESIAN_POINT('Ctrl Pts',(-25.0868468167721,-3.14538674562905,
-2.15222056121083));
#47328=CARTESIAN_POINT('Ctrl Pts',(-24.8880697902821,0.108362070287417,
-3.80963202337103));
#47329=CARTESIAN_POINT('Ctrl Pts',(-24.6892927637921,3.26260339792463,-1.96993487649339));
#47330=CARTESIAN_POINT('Ctrl Pts',(-24.4905157373022,3.42183734109356,1.67817626036435));
#47331=CARTESIAN_POINT('Ctrl Pts',(-24.2917387108122,0.439863865693541,
3.78572376365049));
#47332=CARTESIAN_POINT('Ctrl Pts',(-24.0929616843222,-2.94589400020572,
2.41804089343147));
#47333=CARTESIAN_POINT('Ctrl Pts',(-23.8941846578322,-3.62736475341514,
-1.16937531657263));
#47334=CARTESIAN_POINT('Ctrl Pts',(-23.6954076313422,-0.978964290720696,
-3.68331844135819));
#47335=CARTESIAN_POINT('Ctrl Pts',(-23.4966306048523,2.56811106183178,-2.81602834885952));
#47336=CARTESIAN_POINT('Ctrl Pts',(-23.2978535783623,3.75769675477037,0.636337094806224));
#47337=CARTESIAN_POINT('Ctrl Pts',(-23.0990765518723,1.49776930770217,3.50455359875708));
#47338=CARTESIAN_POINT('Ctrl Pts',(-22.9002995253823,-2.13708929630228,
3.15563920390215));
#47339=CARTESIAN_POINT('Ctrl Pts',(-22.7015224988924,-3.81012990972458,
-0.0901078773958003));
#47340=CARTESIAN_POINT('Ctrl Pts',(-22.5027454724024,-1.9855246223874,-3.2531371345379));
#47341=CARTESIAN_POINT('Ctrl Pts',(-22.3039684459124,1.66176444014233,-3.4298321060602));
#47342=CARTESIAN_POINT('Ctrl Pts',(-22.1051914194224,3.78357703340158,-0.45798924048176));
#47343=CARTESIAN_POINT('Ctrl Pts',(-21.9064143929325,2.43211891370082,2.93428132400969));
#47344=CARTESIAN_POINT('Ctrl Pts',(-21.7076373664425,-1.15199029393737,
3.63292274535707));
#47345=CARTESIAN_POINT('Ctrl Pts',(-21.5088603399525,-3.67858855159617,
0.996591980611707));
#47346=CARTESIAN_POINT('Ctrl Pts',(-21.3100833134625,-2.8282940543877,-2.5545962593447));
#47347=CARTESIAN_POINT('Ctrl Pts',(-21.1113062869725,0.618334760982468,
-3.76070092288226));
#47348=CARTESIAN_POINT('Ctrl Pts',(-20.9125292604826,3.49734092856599,-1.51453482522831));
#47349=CARTESIAN_POINT('Ctrl Pts',(-20.7137522339926,3.16583712036473,2.12195302366768));
#47350=CARTESIAN_POINT('Ctrl Pts',(-20.5149752075026,-0.0718608118791213,
3.81051772482967));
#47351=CARTESIAN_POINT('Ctrl Pts',(-20.3161981810126,-3.24359152557454,
2.00108053877585));
#47352=CARTESIAN_POINT('Ctrl Pts',(-20.1174211545227,-3.43775066054039,
-1.64532054733392));
#47353=CARTESIAN_POINT('Ctrl Pts',(-19.9186441280327,-0.476102850960359,
-3.7813404214166));
#47354=CARTESIAN_POINT('Ctrl Pts',(-19.7198671015427,2.92260070569343,-2.44614276413548));
#47355=CARTESIAN_POINT('Ctrl Pts',(-19.5210900750527,3.63839775937779,1.13457968101029));
#47356=CARTESIAN_POINT('Ctrl Pts',(-19.3223130485627,1.01419664261627,3.67377387388617));
#47357=CARTESIAN_POINT('Ctrl Pts',(-19.1235360220728,-2.54102278309695,
2.84049511943538));
#47358=CARTESIAN_POINT('Ctrl Pts',(-18.9247589955828,-3.76361889362955,
-0.600318361016281));
#47359=CARTESIAN_POINT('Ctrl Pts',(-18.7259819690928,-1.53126558554944,
-3.49004799470226));
#47360=CARTESIAN_POINT('Ctrl Pts',(-18.5272049426028,2.10676807472235,-3.17596246694));
#47361=CARTESIAN_POINT('Ctrl Pts',(-18.3284279161128,3.81081816296161,0.0536121173318595));
#47362=CARTESIAN_POINT('Ctrl Pts',(-18.1296508896229,2.01659055559616,3.23397151708182));
#47363=CARTESIAN_POINT('Ctrl Pts',(-17.9308738631329,-1.62883890977077,
3.44559039419421));
#47364=CARTESIAN_POINT('Ctrl Pts',(-17.7320968366429,-3.77901711469435,
0.4942055163807));
#47365=CARTESIAN_POINT('Ctrl Pts',(-17.5333198101529,-2.46011047524903,
-2.91085301505003));
#47366=CARTESIAN_POINT('Ctrl Pts',(-17.334542783663,1.11714296776071,-3.64378942704172));
#47367=CARTESIAN_POINT('Ctrl Pts',(-17.135765757173,3.66887510281969,-1.03177786727233));
#47368=CARTESIAN_POINT('Ctrl Pts',(-16.936988730683,2.85263073953649,2.52739068741007));
#47369=CARTESIAN_POINT('Ctrl Pts',(-16.738211704193,-0.582287604380603,
3.76645122510734));
#47370=CARTESIAN_POINT('Ctrl Pts',(-16.539434677703,-3.48267616710018,1.54795992773304));
#47371=CARTESIAN_POINT('Ctrl Pts',(-16.3406576512131,-3.18601276291149,
-2.09153228748111));
#47372=CARTESIAN_POINT('Ctrl Pts',(-16.1418806247231,0.0353578955585694,
-3.81103610176739));
#47373=CARTESIAN_POINT('Ctrl Pts',(-15.9431035982331,3.22428567725235,-2.0320448374088));
#47374=CARTESIAN_POINT('Ctrl Pts',(-15.7443265717431,3.45333495329863,1.6123015202179));
#47375=CARTESIAN_POINT('Ctrl Pts',(-15.5455495452532,0.512328175864222,
3.77664281656251));
#47376=CARTESIAN_POINT('Ctrl Pts',(-15.3467725187632,-2.89909931249566,
2.47395260233185));
#47377=CARTESIAN_POINT('Ctrl Pts',(-15.1479954922732,-3.64897975376042,
-1.09954652417408));
#47378=CARTESIAN_POINT('Ctrl Pts',(-14.9492184657832,-1.04956382363505,
-3.66415224416977));
#47379=CARTESIAN_POINT('Ctrl Pts',(-14.7504414392933,2.51414376359986,-2.86419653732846));
#47380=CARTESIAN_POINT('Ctrl Pts',(-14.5516644128032,3.76833505696647,0.563263663837553));
#47381=CARTESIAN_POINT('Ctrl Pts',(-14.3528873863133,1.56631945652084,3.47714249206992));
#47382=CARTESIAN_POINT('Ctrl Pts',(-14.1541103598233,-2.07983560379109,
3.19208989123696));
#47383=CARTESIAN_POINT('Ctrl Pts',(-14.0215923421633,-3.22753662896723,
1.05886984177777));
#47384=CARTESIAN_POINT('Ctrl Pts',(-13.9553333333333,-3.22271751746272,
-0.0144694553766564));
#47385=CARTESIAN_POINT('Ctrl Pts',(-26.5403753524613,-1.53816642191923,
3.09873914818272));
#47386=CARTESIAN_POINT('Ctrl Pts',(-26.4741163436313,-2.57021421430345,
2.58644650780599));
#47387=CARTESIAN_POINT('Ctrl Pts',(-26.3415983259713,-4.06402812511743,
0.45802905132047));
#47388=CARTESIAN_POINT('Ctrl Pts',(-26.1428212994813,-2.58152456373508,
-3.17725411644275));
#47389=CARTESIAN_POINT('Ctrl Pts',(-25.9440442729914,1.27443828706397,-3.88648403811378));
#47390=CARTESIAN_POINT('Ctrl Pts',(-25.7452672465014,3.95861895433119,-1.03260235704353));
#47391=CARTESIAN_POINT('Ctrl Pts',(-25.5464902200114,3.00980311669128,2.77155866720764));
#47392=CARTESIAN_POINT('Ctrl Pts',(-25.3477131935214,-0.702464855775631,
4.03025012352547));
#47393=CARTESIAN_POINT('Ctrl Pts',(-25.1489361670314,-3.76962463598353,
1.58985615976362));
#47394=CARTESIAN_POINT('Ctrl Pts',(-24.9501591405415,-3.37645347808664,
-2.31032721480376));
#47395=CARTESIAN_POINT('Ctrl Pts',(-24.7513821140515,0.116322576110241,
-4.08949561239689));
#47396=CARTESIAN_POINT('Ctrl Pts',(-24.5526050875615,3.50228111244131,-2.11465043991279));
#47397=CARTESIAN_POINT('Ctrl Pts',(-24.3538280610715,3.6732127163178,1.80145862159038));
#47398=CARTESIAN_POINT('Ctrl Pts',(-24.1550510345815,0.472177191332509,
4.06383100158214));
#47399=CARTESIAN_POINT('Ctrl Pts',(-23.9562740080916,-3.16230557558347,
2.59567526827282));
#47400=CARTESIAN_POINT('Ctrl Pts',(-23.7574969816016,-3.8938386050546,-1.2552800892663));
#47401=CARTESIAN_POINT('Ctrl Pts',(-23.5587199551116,-1.05088106857445,
-3.95390276871574));
#47402=CARTESIAN_POINT('Ctrl Pts',(-23.3599429286216,2.75676990719324,-3.02289972007743));
#47403=CARTESIAN_POINT('Ctrl Pts',(-23.1611659021316,4.03374506962317,0.683083757499677));
#47404=CARTESIAN_POINT('Ctrl Pts',(-22.9623888756417,1.60779859436684,3.76200548441552));
#47405=CARTESIAN_POINT('Ctrl Pts',(-22.7636118491517,-2.2940843753185,3.38745910352944));
#47406=CARTESIAN_POINT('Ctrl Pts',(-22.5648348226617,-4.09003007453019,
-0.0967273917774301));
#47407=CARTESIAN_POINT('Ctrl Pts',(-22.3660577961717,-2.13138544136196,
-3.49211943741645));
#47408=CARTESIAN_POINT('Ctrl Pts',(-22.1672807696818,1.78384115450232,-3.68179479355063));
#47409=CARTESIAN_POINT('Ctrl Pts',(-21.9685037431918,4.06152656800954,-0.49163409431284));
#47410=CARTESIAN_POINT('Ctrl Pts',(-21.7697267167018,2.61078748955023,3.1498398077454));
#47411=CARTESIAN_POINT('Ctrl Pts',(-21.5709496902119,-1.23661792626678,
3.89980489878606));
#47412=CARTESIAN_POINT('Ctrl Pts',(-21.3721726637218,-3.94882541129375,
1.06980372567722));
#47413=CARTESIAN_POINT('Ctrl Pts',(-21.1733956372319,-3.03606649015725,
-2.74226227886213));
#47414=CARTESIAN_POINT('Ctrl Pts',(-20.9746186107419,0.66375893433211,-4.03696993024938));
#47415=CARTESIAN_POINT('Ctrl Pts',(-20.7758415842519,3.75426295628702,-1.62579574210764));
#47416=CARTESIAN_POINT('Ctrl Pts',(-20.5770645577619,3.39840618040549,2.27783616022909));
#47417=CARTESIAN_POINT('Ctrl Pts',(-20.378287531272,-0.0771398584115342,
4.09044637934939));
#47418=CARTESIAN_POINT('Ctrl Pts',(-20.179510504782,-3.48187258792183,2.14808412811888));
#47419=CARTESIAN_POINT('Ctrl Pts',(-19.980733478292,-3.69029506171422,-1.76618925870813));
#47420=CARTESIAN_POINT('Ctrl Pts',(-19.781956451802,-0.51107836875259,-4.05912564979931));
#47421=CARTESIAN_POINT('Ctrl Pts',(-19.583179425312,3.1373011066159,-2.62584156156287));
#47422=CARTESIAN_POINT('Ctrl Pts',(-19.3844023988221,3.90568211886354,1.21792829305873));
#47423=CARTESIAN_POINT('Ctrl Pts',(-19.1856253723321,1.08870166321652,3.94365703722262));
#47424=CARTESIAN_POINT('Ctrl Pts',(-18.9868483458421,-2.72769166647238,
3.04916387113078));
#47425=CARTESIAN_POINT('Ctrl Pts',(-18.7880713193521,-4.0401022612711,-0.644419011693669));
#47426=CARTESIAN_POINT('Ctrl Pts',(-18.5892942928622,-1.64375557930598,
-3.74643426814753));
#47427=CARTESIAN_POINT('Ctrl Pts',(-18.3905172663722,2.26153569296468,-3.40927535625753));
#47428=CARTESIAN_POINT('Ctrl Pts',(-18.1917402398822,4.09076888829903,0.057550576343037));
#47429=CARTESIAN_POINT('Ctrl Pts',(-17.9929632133922,2.16473354342874,3.47154587335181));
#47430=CARTESIAN_POINT('Ctrl Pts',(-17.7941861869023,-1.74849684535007,
3.69871071870759));
#47431=CARTESIAN_POINT('Ctrl Pts',(-17.5954091604123,-4.05663166807388,
0.530510894087064));
#47432=CARTESIAN_POINT('Ctrl Pts',(-17.3966321339223,-2.64083537014167,
-3.12469040588489));
#47433=CARTESIAN_POINT('Ctrl Pts',(-17.1978551074323,1.19921064214355,-3.91146986978538));
#47434=CARTESIAN_POINT('Ctrl Pts',(-16.9990780809423,3.93839839211999,-1.10757444165036));
#47435=CARTESIAN_POINT('Ctrl Pts',(-16.8003010544524,3.06219099943418,2.71305812833607));
#47436=CARTESIAN_POINT('Ctrl Pts',(-16.6015240279624,-0.625063677714576,
4.04314266178228));
#47437=CARTESIAN_POINT('Ctrl Pts',(-16.4027470014724,-3.73852089056956,
1.66167632301373));
#47438=CARTESIAN_POINT('Ctrl Pts',(-16.2039699749824,-3.42006396813043,
-2.24518065271611));
#47439=CARTESIAN_POINT('Ctrl Pts',(-16.0051929484924,0.0379553610068489,
-4.09100283734831));
#47440=CARTESIAN_POINT('Ctrl Pts',(-15.8064159220025,3.46114849133643,-2.18132312931992));
#47441=CARTESIAN_POINT('Ctrl Pts',(-15.6076388955125,3.70702420942879,1.73074458434373));
#47442=CARTESIAN_POINT('Ctrl Pts',(-15.4088618690225,0.549964882290692,
4.05408294900256));
#47443=CARTESIAN_POINT('Ctrl Pts',(-15.2100848425325,-3.11207325159528,
2.65569436902244));
#47444=CARTESIAN_POINT('Ctrl Pts',(-15.0113078160426,-3.91704148883227,
-1.18032152676447));
#47445=CARTESIAN_POINT('Ctrl Pts',(-14.8125307895526,-1.12666699181305,
-3.93332858233041));
#47446=CARTESIAN_POINT('Ctrl Pts',(-14.6137537630626,2.69883805761343,-3.07460644508194));
#47447=CARTESIAN_POINT('Ctrl Pts',(-14.4149767365726,4.0451648838959,0.604642198447279));
#47448=CARTESIAN_POINT('Ctrl Pts',(-14.2161997100826,1.68138458143942,3.73258070012128));
#47449=CARTESIAN_POINT('Ctrl Pts',(-14.0174226835927,-2.23262470601667,
3.42658753509713));
#47450=CARTESIAN_POINT('Ctrl Pts',(-13.8849046659327,-3.46463826480867,
1.13665664964091));
#47451=CARTESIAN_POINT('Ctrl Pts',(-13.8186456571027,-3.45946513122715,
-0.015532412031805));
#47452=CARTESIAN_POINT('Ctrl Pts',(-26.4036876762306,-1.64343044862521,
3.31080057131678));
#47453=CARTESIAN_POINT('Ctrl Pts',(-26.3374286674006,-2.74610616841136,
2.76344931477899));
#47454=CARTESIAN_POINT('Ctrl Pts',(-26.2049106497407,-4.34214885314794,
0.489374152606833));
#47455=CARTESIAN_POINT('Ctrl Pts',(-26.0061336232507,-2.75819053872115,
-3.39468869140092));
#47456=CARTESIAN_POINT('Ctrl Pts',(-25.8073565967607,1.36165414613677,-4.15245458184075));
#47457=CARTESIAN_POINT('Ctrl Pts',(-25.6085795702707,4.22952603264826,-1.10326823593646));
#47458=CARTESIAN_POINT('Ctrl Pts',(-25.4098025437808,3.21577822519734,2.96122957758815));
#47459=CARTESIAN_POINT('Ctrl Pts',(-25.2110255172908,-0.750537858985583,
4.30605926263362));
#47460=CARTESIAN_POINT('Ctrl Pts',(-25.0122484908008,-4.02759793633592,
1.69865756049324));
#47461=CARTESIAN_POINT('Ctrl Pts',(-24.8134714643108,-3.60752021054423,
-2.4684338683967));
#47462=CARTESIAN_POINT('Ctrl Pts',(-24.6146944378208,0.124283081933059,
-4.36935920142275));
#47463=CARTESIAN_POINT('Ctrl Pts',(-24.4159174113308,3.74195882695799,-2.25936600333218));
#47464=CARTESIAN_POINT('Ctrl Pts',(-24.2171403848409,3.92458809154204,1.92474098281642));
#47465=CARTESIAN_POINT('Ctrl Pts',(-24.0183633583509,0.504490516971484,
4.3419382395138));
#47466=CARTESIAN_POINT('Ctrl Pts',(-23.8195863318609,-3.37871715096123,
2.77330964311416));
#47467=CARTESIAN_POINT('Ctrl Pts',(-23.620809305371,-4.16031245669405,-1.34118486195997));
#47468=CARTESIAN_POINT('Ctrl Pts',(-23.4220322788809,-1.1227978464282,-4.22448709607329));
#47469=CARTESIAN_POINT('Ctrl Pts',(-23.223255252391,2.9454287525547,-3.22977109129534));
#47470=CARTESIAN_POINT('Ctrl Pts',(-23.024478225901,4.30979338447599,0.729830420193126));
#47471=CARTESIAN_POINT('Ctrl Pts',(-22.825701199411,1.71782788103149,4.01945737007395));
#47472=CARTESIAN_POINT('Ctrl Pts',(-22.6269241729211,-2.45107945433472,
3.61927900315673));
#47473=CARTESIAN_POINT('Ctrl Pts',(-22.4281471464311,-4.36993023933581,
-0.103346906159059));
#47474=CARTESIAN_POINT('Ctrl Pts',(-22.2293701199411,-2.27724626033652,
-3.73110174029499));
#47475=CARTESIAN_POINT('Ctrl Pts',(-22.0305930934511,1.90591786886231,-3.93375748104105));
#47476=CARTESIAN_POINT('Ctrl Pts',(-21.8318160669612,4.33947610261751,-0.525278948143918));
#47477=CARTESIAN_POINT('Ctrl Pts',(-21.6330390404711,2.78945606539964,3.36539829148111));
#47478=CARTESIAN_POINT('Ctrl Pts',(-21.4342620139812,-1.32124555859619,
4.16668705221506));
#47479=CARTESIAN_POINT('Ctrl Pts',(-21.2354849874912,-4.21906227099134,
1.14301547074272));
#47480=CARTESIAN_POINT('Ctrl Pts',(-21.0367079610012,-3.2438389259268,-2.92992829837957));
#47481=CARTESIAN_POINT('Ctrl Pts',(-20.8379309345113,0.709183107681748,
-4.3132389376165));
#47482=CARTESIAN_POINT('Ctrl Pts',(-20.6391539080213,4.01118498400806,-1.73705665898696));
#47483=CARTESIAN_POINT('Ctrl Pts',(-20.4403768815313,3.63097524044626,2.4337192967905));
#47484=CARTESIAN_POINT('Ctrl Pts',(-20.2415998550413,-0.0824189049439472,
4.37037503386911));
#47485=CARTESIAN_POINT('Ctrl Pts',(-20.0428228285513,-3.72015365026912,
2.2950877174619));
#47486=CARTESIAN_POINT('Ctrl Pts',(-19.8440458020614,-3.94283946288805,
-1.88705797008235));
#47487=CARTESIAN_POINT('Ctrl Pts',(-19.6452687755714,-0.546053886544821,
-4.33691087818202));
#47488=CARTESIAN_POINT('Ctrl Pts',(-19.4464917490814,3.35200150753837,-2.80554035899026));
#47489=CARTESIAN_POINT('Ctrl Pts',(-19.2477147225914,4.17296647834929,1.30127690510718));
#47490=CARTESIAN_POINT('Ctrl Pts',(-19.0489376961014,1.16320668381677,4.21354020055907));
#47491=CARTESIAN_POINT('Ctrl Pts',(-18.8501606696115,-2.91436054984781,
3.25783262282619));
#47492=CARTESIAN_POINT('Ctrl Pts',(-18.6513836431215,-4.31658562891265,
-0.688519662371059));
#47493=CARTESIAN_POINT('Ctrl Pts',(-18.4526066166315,-1.75624557306252,
-4.00282054159279));
#47494=CARTESIAN_POINT('Ctrl Pts',(-18.2538295901415,2.41630331120702,-3.64258824557506));
#47495=CARTESIAN_POINT('Ctrl Pts',(-18.0550525636516,4.37071961363644,0.0614890353542112));
#47496=CARTESIAN_POINT('Ctrl Pts',(-17.8562755371616,2.31287653126131,3.70912022962179));
#47497=CARTESIAN_POINT('Ctrl Pts',(-17.6574985106716,-1.86815478092937,
3.95183104322097));
#47498=CARTESIAN_POINT('Ctrl Pts',(-17.4587214841817,-4.33424622145341,
0.566816271793429));
#47499=CARTESIAN_POINT('Ctrl Pts',(-17.2599444576916,-2.82156026503431,
-3.33852779671976));
#47500=CARTESIAN_POINT('Ctrl Pts',(-17.0611674312017,1.28127831652639,-4.17915031252904));
#47501=CARTESIAN_POINT('Ctrl Pts',(-16.8623904047117,4.20792168142029,-1.18337101602838));
#47502=CARTESIAN_POINT('Ctrl Pts',(-16.6636133782217,3.27175125933188,2.89872556926209));
#47503=CARTESIAN_POINT('Ctrl Pts',(-16.4648363517317,-0.667839751048547,
4.31983409845722));
#47504=CARTESIAN_POINT('Ctrl Pts',(-16.2660593252418,-3.99436561403894,
1.77539271829442));
#47505=CARTESIAN_POINT('Ctrl Pts',(-16.0672822987518,-3.65411517334937,
-2.39882901795111));
#47506=CARTESIAN_POINT('Ctrl Pts',(-15.8685052722618,0.040552826455128,
-4.37096957292924));
#47507=CARTESIAN_POINT('Ctrl Pts',(-15.6697282457718,3.69801130542051,-2.33060142123105));
#47508=CARTESIAN_POINT('Ctrl Pts',(-15.4709512192819,3.96071346555895,1.84918764846957));
#47509=CARTESIAN_POINT('Ctrl Pts',(-15.2721741927919,0.587601588717162,
4.33152308144261));
#47510=CARTESIAN_POINT('Ctrl Pts',(-15.0733971663019,-3.32504719069491,
2.83743613571303));
#47511=CARTESIAN_POINT('Ctrl Pts',(-14.8746201398119,-4.18510322390412,
-1.26109652935485));
#47512=CARTESIAN_POINT('Ctrl Pts',(-14.6758431133219,-1.20377015999105,
-4.20250492049104));
#47513=CARTESIAN_POINT('Ctrl Pts',(-14.477066086832,2.883532351627,-3.28501635283543));
#47514=CARTESIAN_POINT('Ctrl Pts',(-14.278289060342,4.32199471082533,0.646020733057002));
#47515=CARTESIAN_POINT('Ctrl Pts',(-14.079512033852,1.796449706358,3.98801890817264));
#47516=CARTESIAN_POINT('Ctrl Pts',(-13.880735007362,-2.38541380824225,3.6610851789573));
#47517=CARTESIAN_POINT('Ctrl Pts',(-13.748216989702,-3.7017399006501,1.21444345750405));
#47518=CARTESIAN_POINT('Ctrl Pts',(-13.681957980872,-3.69621274499157,-0.0165953686869537));
#47519=CARTESIAN_POINT('Ctrl Pts',(-26.267,-1.7486944753312,3.52286199445084));
#47520=CARTESIAN_POINT('Ctrl Pts',(-26.20074099117,-2.92199812251927,2.94045212175199));
#47521=CARTESIAN_POINT('Ctrl Pts',(-26.06822297351,-4.62026958117845,0.520719253893197));
#47522=CARTESIAN_POINT('Ctrl Pts',(-25.86944594702,-2.93485651370723,-3.6121232663591));
#47523=CARTESIAN_POINT('Ctrl Pts',(-25.6706689205301,1.44887000520957,-4.41842512556771));
#47524=CARTESIAN_POINT('Ctrl Pts',(-25.4718918940401,4.50043311096533,-1.1739341148294));
#47525=CARTESIAN_POINT('Ctrl Pts',(-25.2731148675501,3.42175333370339,3.15090048796866));
#47526=CARTESIAN_POINT('Ctrl Pts',(-25.0743378410601,-0.798610862195538,
4.58186840174178));
#47527=CARTESIAN_POINT('Ctrl Pts',(-24.8755608145702,-4.2855712366883,1.80745896122284));
#47528=CARTESIAN_POINT('Ctrl Pts',(-24.6767837880802,-3.83858694300183,
-2.62654052198963));
#47529=CARTESIAN_POINT('Ctrl Pts',(-24.4780067615902,0.132243587755882,
-4.64922279044861));
#47530=CARTESIAN_POINT('Ctrl Pts',(-24.2792297351002,3.98163654147467,-2.40408156675157));
#47531=CARTESIAN_POINT('Ctrl Pts',(-24.0804527086102,4.17596346676628,2.04802334404246));
#47532=CARTESIAN_POINT('Ctrl Pts',(-23.8816756821203,0.536803842610455,
4.62004547744546));
#47533=CARTESIAN_POINT('Ctrl Pts',(-23.6828986556303,-3.59512872633899,
2.9509440179555));
#47534=CARTESIAN_POINT('Ctrl Pts',(-23.4841216291403,-4.42678630833351,
-1.42708963465364));
#47535=CARTESIAN_POINT('Ctrl Pts',(-23.2853446026503,-1.19471462428195,
-4.49507142343084));
#47536=CARTESIAN_POINT('Ctrl Pts',(-23.0865675761604,3.13408759791616,-3.43664246251325));
#47537=CARTESIAN_POINT('Ctrl Pts',(-22.8877905496704,4.58584169932879,0.776577082886578));
#47538=CARTESIAN_POINT('Ctrl Pts',(-22.6890135231804,1.82785716769616,4.27690925573239));
#47539=CARTESIAN_POINT('Ctrl Pts',(-22.4902364966904,-2.60807453335094,
3.85109890278403));
#47540=CARTESIAN_POINT('Ctrl Pts',(-22.2914594702004,-4.64983040414143,
-0.109966420540693));
#47541=CARTESIAN_POINT('Ctrl Pts',(-22.0926824437105,-2.42310707931108,
-3.97008404317354));
#47542=CARTESIAN_POINT('Ctrl Pts',(-21.8939054172205,2.02799458322229,-4.18572016853148));
#47543=CARTESIAN_POINT('Ctrl Pts',(-21.6951283907305,4.61742563722547,-0.558923801975));
#47544=CARTESIAN_POINT('Ctrl Pts',(-21.4963513642405,2.96812464124906,3.58095677521683));
#47545=CARTESIAN_POINT('Ctrl Pts',(-21.2975743377506,-1.40587319092561,
4.43356920564406));
#47546=CARTESIAN_POINT('Ctrl Pts',(-21.0987973112605,-4.48929913068892,
1.21622721580824));
#47547=CARTESIAN_POINT('Ctrl Pts',(-20.9000202847706,-3.45161136169635,
-3.11759431789701));
#47548=CARTESIAN_POINT('Ctrl Pts',(-20.7012432582806,0.754607281031384,
-4.58950794498361));
#47549=CARTESIAN_POINT('Ctrl Pts',(-20.5024662317907,4.2681070117291,-1.84831757586629));
#47550=CARTESIAN_POINT('Ctrl Pts',(-20.3036892053006,3.86354430048703,2.58960243335191));
#47551=CARTESIAN_POINT('Ctrl Pts',(-20.1049121788107,-0.0876979514763586,
4.65030368838883));
#47552=CARTESIAN_POINT('Ctrl Pts',(-19.9061351523207,-3.95843471261642,
2.44209130680492));
#47553=CARTESIAN_POINT('Ctrl Pts',(-19.7073581258307,-4.19538386406187,
-2.00792668145656));
#47554=CARTESIAN_POINT('Ctrl Pts',(-19.5085810993407,-0.581029404337056,
-4.61469610656473));
#47555=CARTESIAN_POINT('Ctrl Pts',(-19.3098040728508,3.56670190846084,-2.98523915641764));
#47556=CARTESIAN_POINT('Ctrl Pts',(-19.1110270463608,4.44025083783504,1.38462551715563));
#47557=CARTESIAN_POINT('Ctrl Pts',(-18.9122500198708,1.23771170441702,4.48342336389552));
#47558=CARTESIAN_POINT('Ctrl Pts',(-18.7134729933808,-3.10102943322324,
3.46650137452159));
#47559=CARTESIAN_POINT('Ctrl Pts',(-18.5146959668909,-4.59306899655421,
-0.732620313048447));
#47560=CARTESIAN_POINT('Ctrl Pts',(-18.3159189404009,-1.86873556681905,
-4.25920681503806));
#47561=CARTESIAN_POINT('Ctrl Pts',(-18.1171419139109,2.57107092944934,-3.87590113489259));
#47562=CARTESIAN_POINT('Ctrl Pts',(-17.9183648874209,4.65067033897386,0.0654274943653892));
#47563=CARTESIAN_POINT('Ctrl Pts',(-17.7195878609309,2.46101951909389,3.94669458589177));
#47564=CARTESIAN_POINT('Ctrl Pts',(-17.520810834441,-1.98781271650867,4.20495136773435));
#47565=CARTESIAN_POINT('Ctrl Pts',(-17.322033807951,-4.61186077483295,0.60312164949979));
#47566=CARTESIAN_POINT('Ctrl Pts',(-17.123256781461,-3.00228515992694,-3.55236518755462));
#47567=CARTESIAN_POINT('Ctrl Pts',(-16.924479754971,1.36334599090922,-4.4468307552727));
#47568=CARTESIAN_POINT('Ctrl Pts',(-16.725702728481,4.4774449707206,-1.25916759040641));
#47569=CARTESIAN_POINT('Ctrl Pts',(-16.5269257019911,3.48131151922957,3.0843930101881));
#47570=CARTESIAN_POINT('Ctrl Pts',(-16.3281486755011,-0.710615824382518,
4.59652553513216));
#47571=CARTESIAN_POINT('Ctrl Pts',(-16.1293716490111,-4.25021033750832,
1.88910911357511));
#47572=CARTESIAN_POINT('Ctrl Pts',(-15.9305946225211,-3.8881663785683,-2.55247738318612));
#47573=CARTESIAN_POINT('Ctrl Pts',(-15.7318175960312,0.0431502919034069,
-4.65093630851017));
#47574=CARTESIAN_POINT('Ctrl Pts',(-15.5330405695412,3.93487411950459,-2.47987971314217));
#47575=CARTESIAN_POINT('Ctrl Pts',(-15.3342635430512,4.21440272168911,1.9676307125954));
#47576=CARTESIAN_POINT('Ctrl Pts',(-15.1354865165612,0.625238295143632,
4.60896321388266));
#47577=CARTESIAN_POINT('Ctrl Pts',(-14.9367094900712,-3.53802112979453,
3.01917790240362));
#47578=CARTESIAN_POINT('Ctrl Pts',(-14.7379324635813,-4.45316495897597,
-1.34187153194524));
#47579=CARTESIAN_POINT('Ctrl Pts',(-14.5391554370913,-1.28087332816905,
-4.47168125865167));
#47580=CARTESIAN_POINT('Ctrl Pts',(-14.3403784106013,3.06822664564056,-3.49542626058891));
#47581=CARTESIAN_POINT('Ctrl Pts',(-14.1416013841113,4.59882453775476,0.687399267666724));
#47582=CARTESIAN_POINT('Ctrl Pts',(-13.9428243576214,1.91151483127657,4.24345711622401));
#47583=CARTESIAN_POINT('Ctrl Pts',(-13.7440473311314,-2.53820291046783,
3.89558282281748));
#47584=CARTESIAN_POINT('Ctrl Pts',(-13.6115293134714,-3.93884153649153,
1.29223026536719));
#47585=CARTESIAN_POINT('Ctrl Pts',(-13.5452703046414,-3.932960358756,-0.0176583253421023));
#47586=CARTESIAN_POINT('Ctrl Pts',(-14.796163522035,-3.93066717675506,-0.00339337507098336));
#47587=CARTESIAN_POINT('Ctrl Pts',(-14.7767531692171,-3.93387125603329,
-0.387580586707519));
#47588=CARTESIAN_POINT('Ctrl Pts',(-14.7573428163992,-3.88212968630794,
-0.770927932742981));
#47589=CARTESIAN_POINT('Ctrl Pts',(-14.7379324635813,-3.77192571564458,
-1.13666491400483));
#47590=CARTESIAN_POINT('Ctrl Pts',(-14.6716734547513,-3.39573441537366,
-2.38514144084738));
#47591=CARTESIAN_POINT('Ctrl Pts',(-14.6054144459213,-2.33830387177135,
-3.42841134974953));
#47592=CARTESIAN_POINT('Ctrl Pts',(-14.5391554370913,-1.08473860433526,
-3.78733713785681));
#47593=CARTESIAN_POINT('Ctrl Pts',(-14.4728964282613,0.168826663100827,
-4.14626292596409));
#47594=CARTESIAN_POINT('Ctrl Pts',(-14.4066374194313,1.61852665437069,-3.8208445932765));
#47595=CARTESIAN_POINT('Ctrl Pts',(-14.3403784106013,2.59847629869133,-2.9609978388901));
#47596=CARTESIAN_POINT('Ctrl Pts',(-14.2741194017713,3.57842594301196,-2.1011510845037));
#47597=CARTESIAN_POINT('Ctrl Pts',(-14.2078603929413,4.08862524038336,-0.706875908418483));
#47598=CARTESIAN_POINT('Ctrl Pts',(-14.1416013841113,3.89583993798937,0.582937987716999));
#47599=CARTESIAN_POINT('Ctrl Pts',(-14.079512033852,3.71518655399588,1.79158430133742));
#47600=CARTESIAN_POINT('Ctrl Pts',(-14.0174226835927,2.9172418482862,2.90850308409889));
#47601=CARTESIAN_POINT('Ctrl Pts',(-13.9553333333333,1.83875391880586,3.48426281672735));
#47602=CARTESIAN_POINT('',(-26.267,-1.87158653173891,-2.62360084935066));
#47603=CARTESIAN_POINT('Ctrl Pts',(-26.267,-1.87563364385541,-2.62744043199008));
#47604=CARTESIAN_POINT('Ctrl Pts',(-26.267,-1.93502283818884,-2.59436675243734));
#47605=CARTESIAN_POINT('Ctrl Pts',(-26.267,-1.99319562091243,-2.55933411580012));
#47606=CARTESIAN_POINT('Ctrl Pts',(-26.267,-2.05004339163671,-2.52236226376319));
#47607=CARTESIAN_POINT('Ctrl Pts',(-26.267,-2.13607085868267,-2.46641293202665));
#47608=CARTESIAN_POINT('Ctrl Pts',(-26.267,-2.21906528067624,-2.40602533039299));
#47609=CARTESIAN_POINT('Ctrl Pts',(-26.267,-2.29893371013539,-2.3415918437389));
#47610=CARTESIAN_POINT('Ctrl Pts',(-26.267,-2.34933821690132,-2.30092824066067));
#47611=CARTESIAN_POINT('Ctrl Pts',(-26.267,-2.39849739182093,-2.25865218486351));
#47612=CARTESIAN_POINT('Ctrl Pts',(-26.267,-2.44638375817581,-2.21485267411829));
#47613=CARTESIAN_POINT('Ctrl Pts',(-26.267,-2.4769857683737,-2.1868623884375));
#47614=CARTESIAN_POINT('Ctrl Pts',(-26.267,-2.50706790697913,-2.15824979279682));
#47615=CARTESIAN_POINT('Ctrl Pts',(-26.267,-2.53662217937948,-2.12903671190489));
#47616=CARTESIAN_POINT('Ctrl Pts',(-26.267,-2.54989830294754,-2.11591385553843));
#47617=CARTESIAN_POINT('Ctrl Pts',(-26.267,-2.5630668342312,-2.10267076594302));
#47618=CARTESIAN_POINT('Ctrl Pts',(-26.267,-2.57611858766727,-2.0893183706114));
#47619=CARTESIAN_POINT('Ctrl Pts',(-26.267,-2.65028331647228,-2.01344528708147));
#47620=CARTESIAN_POINT('Ctrl Pts',(-26.267,-2.72075551146666,-1.93397177742404));
#47621=CARTESIAN_POINT('Ctrl Pts',(-26.267,-2.78743443104751,-1.85130541984555));
#47622=CARTESIAN_POINT('Ctrl Pts',(-26.267,-2.8510104455509,-1.77248594314454));
#47623=CARTESIAN_POINT('Ctrl Pts',(-26.267,-2.91113820636111,-1.69076303840862));
#47624=CARTESIAN_POINT('Ctrl Pts',(-26.267,-2.96770924376778,-1.60645353911803));
#47625=CARTESIAN_POINT('Ctrl Pts',(-26.267,-2.9924590726332,-1.56956813317839));
#47626=CARTESIAN_POINT('Ctrl Pts',(-26.267,-3.01652782447795,-1.53218722341775));
#47627=CARTESIAN_POINT('Ctrl Pts',(-26.267,-3.03990490959769,-1.49433557773647));
#47628=CARTESIAN_POINT('Ctrl Pts',(-26.267,-3.05147433099463,-1.47560263317938));
#47629=CARTESIAN_POINT('Ctrl Pts',(-26.267,-3.06287432707377,-1.45675437603992));
#47630=CARTESIAN_POINT('Ctrl Pts',(-26.267,-3.07410352161292,-1.43779372484651));
#47631=CARTESIAN_POINT('Ctrl Pts',(-26.267,-3.08210732291092,-1.42427919501059));
#47632=CARTESIAN_POINT('Ctrl Pts',(-26.267,-3.09002304737044,-1.41070968749839));
#47633=CARTESIAN_POINT('Ctrl Pts',(-26.267,-3.09784603919882,-1.39709387173809));
#47634=CARTESIAN_POINT('Ctrl Pts',(-26.267,-3.15328862986162,-1.30059676215397));
#47635=CARTESIAN_POINT('Ctrl Pts',(-26.267,-3.2041395175185,-1.20167030949908));
#47636=CARTESIAN_POINT('Ctrl Pts',(-26.267,-3.25029005553095,-1.10074331911095));
#47637=CARTESIAN_POINT('Ctrl Pts',(-26.267,-3.29716691060663,-0.998227939975572));
#47638=CARTESIAN_POINT('Ctrl Pts',(-26.267,-3.33919489299649,-0.893647890501421));
#47639=CARTESIAN_POINT('Ctrl Pts',(-26.267,-3.37622637228166,-0.78741086593843));
#47640=CARTESIAN_POINT('Ctrl Pts',(-26.267,-3.41317015926056,-0.681425415708303));
#47641=CARTESIAN_POINT('Ctrl Pts',(-26.267,-3.44514158615419,-0.573790016793496));
#47642=CARTESIAN_POINT('Ctrl Pts',(-26.267,-3.47195261401537,-0.464879656108174));
#47643=CARTESIAN_POINT('Ctrl Pts',(-26.267,-3.48936130848388,-0.394162964325869));
#47644=CARTESIAN_POINT('Ctrl Pts',(-26.267,-3.50459349604628,-0.322908164365236));
#47645=CARTESIAN_POINT('Ctrl Pts',(-26.267,-3.51758674381885,-0.251213629832156));
#47646=CARTESIAN_POINT('Ctrl Pts',(-26.267,-3.52123597647577,-0.231077783789654));
#47647=CARTESIAN_POINT('Ctrl Pts',(-26.267,-3.52470854490799,-0.210907237194771));
#47648=CARTESIAN_POINT('Ctrl Pts',(-26.267,-3.52800293081593,-0.190704140748007));
#47649=CARTESIAN_POINT('Ctrl Pts',(-26.267,-3.5310853921128,-0.171800689660538));
#47650=CARTESIAN_POINT('Ctrl Pts',(-26.267,-3.53401203475742,-0.152866889646329));
#47651=CARTESIAN_POINT('Ctrl Pts',(-26.267,-3.53677862597875,-0.13392654036373));
#47652=CARTESIAN_POINT('Ctrl Pts',(-26.267,-3.5535210675383,-0.0193061770309027));
#47653=CARTESIAN_POINT('Ctrl Pts',(-26.267,-3.56443587029357,0.0957288600444009));
#47654=CARTESIAN_POINT('Ctrl Pts',(-26.267,-3.56937634543034,0.210754462446548));
#47655=CARTESIAN_POINT('Ctrl Pts',(-26.267,-3.57206682834186,0.273395080824828));
#47656=CARTESIAN_POINT('Ctrl Pts',(-26.267,-3.57298480067844,0.336033459704283));
#47657=CARTESIAN_POINT('Ctrl Pts',(-26.267,-3.57210088426465,0.398604262522089));
#47658=CARTESIAN_POINT('Ctrl Pts',(-26.267,-3.57053367028861,0.509544431908386));
#47659=CARTESIAN_POINT('Ctrl Pts',(-26.267,-3.56330522231868,0.620271859661915));
#47660=CARTESIAN_POINT('Ctrl Pts',(-26.267,-3.55068015331886,0.730501366588306));
#47661=CARTESIAN_POINT('Ctrl Pts',(-26.267,-3.53781478472759,0.842828929808865));
#47662=CARTESIAN_POINT('Ctrl Pts',(-26.267,-3.51934530799955,0.954640114197353));
#47663=CARTESIAN_POINT('Ctrl Pts',(-26.267,-3.49549764638492,1.06563656127855));
#47664=CARTESIAN_POINT('Ctrl Pts',(-26.267,-3.4879842997281,1.10060664757351));
#47665=CARTESIAN_POINT('Ctrl Pts',(-26.267,-3.47993672291489,1.13549584598195));
#47666=CARTESIAN_POINT('Ctrl Pts',(-26.267,-3.47136092544872,1.17029472302242));
#47667=CARTESIAN_POINT('Ctrl Pts',(-26.267,-3.46751408660795,1.18590442839879));
#47668=CARTESIAN_POINT('Ctrl Pts',(-26.267,-3.4635602913321,1.20149849192874));
#47669=CARTESIAN_POINT('Ctrl Pts',(-26.267,-3.45950226226653,1.21706761472067));
#47670=CARTESIAN_POINT('Ctrl Pts',(-26.267,-3.43079460214631,1.32720804946344));
#47671=CARTESIAN_POINT('Ctrl Pts',(-26.267,-3.39693213439927,1.43588706906917));
#47672=CARTESIAN_POINT('Ctrl Pts',(-26.267,-3.3582177646934,1.54281137140461));
#47673=CARTESIAN_POINT('Ctrl Pts',(-26.267,-3.31822881808711,1.65325589754548));
#47674=CARTESIAN_POINT('Ctrl Pts',(-26.267,-3.27306321397473,1.76182895533595));
#47675=CARTESIAN_POINT('Ctrl Pts',(-26.267,-3.22299936023802,1.86821150838332));
#47676=CARTESIAN_POINT('Ctrl Pts',(-26.267,-3.17243003712686,1.97566815218736));
#47677=CARTESIAN_POINT('Ctrl Pts',(-26.267,-3.1168627999695,2.0808906344938));
#47678=CARTESIAN_POINT('Ctrl Pts',(-26.267,-3.05653137285161,2.18354294711263));
#47679=CARTESIAN_POINT('Ctrl Pts',(-26.267,-3.01664457625045,2.251409266702));
#47680=CARTESIAN_POINT('Ctrl Pts',(-26.267,-2.97467431085533,2.31815202427033));
#47681=CARTESIAN_POINT('Ctrl Pts',(-26.267,-2.93067640862396,2.38366977677781));
#47682=CARTESIAN_POINT('Ctrl Pts',(-26.267,-2.90918410881585,2.41567419308474));
#47683=CARTESIAN_POINT('Ctrl Pts',(-26.267,-2.88720784447261,2.44738623633731));
#47684=CARTESIAN_POINT('Ctrl Pts',(-26.267,-2.86475337266313,2.47879364579308));
#47685=CARTESIAN_POINT('Ctrl Pts',(-26.267,-2.8507640646594,2.49836070255592));
#47686=CARTESIAN_POINT('Ctrl Pts',(-26.267,-2.83658549398819,2.5178142532328));
#47687=CARTESIAN_POINT('Ctrl Pts',(-26.267,-2.82223936577275,2.53712428807426));
#47688=CARTESIAN_POINT('Ctrl Pts',(-26.267,-2.74908754426023,2.63558738563692));
#47689=CARTESIAN_POINT('Ctrl Pts',(-26.267,-2.6715065446943,2.73043209404712));
#47690=CARTESIAN_POINT('Ctrl Pts',(-26.267,-2.58978746881353,2.82132277898767));
#47691=CARTESIAN_POINT('Ctrl Pts',(-26.267,-2.50797450479922,2.91231788944545));
#47692=CARTESIAN_POINT('Ctrl Pts',(-26.267,-2.42201356354227,2.99935071595012));
#47693=CARTESIAN_POINT('Ctrl Pts',(-26.267,-2.33214667543519,3.08206867663245));
#47694=CARTESIAN_POINT('Ctrl Pts',(-26.267,-2.24243448349077,3.16464424726023));
#47695=CARTESIAN_POINT('Ctrl Pts',(-26.267,-2.14882937383503,3.2429206277689));
#47696=CARTESIAN_POINT('Ctrl Pts',(-26.267,-2.05152823317363,3.31651888350284));
#47697=CARTESIAN_POINT('Ctrl Pts',(-26.267,-1.95422709251222,3.39011713923678));
#47698=CARTESIAN_POINT('Ctrl Pts',(-26.267,-1.85322952476273,3.45903813975137));
#47699=CARTESIAN_POINT('Ctrl Pts',(-26.267,-1.74869447533123,3.52286199445082));
#47700=CARTESIAN_POINT('Ctrl Pts',(-26.267,-1.87563364385542,-2.62744043199007));
#47701=CARTESIAN_POINT('Ctrl Pts',(-26.2049106497406,-1.05751970818542,
-3.20557823490714));
#47702=CARTESIAN_POINT('Ctrl Pts',(-26.0765622906514,1.23967409930297,-3.56474568943846));
#47703=CARTESIAN_POINT('Ctrl Pts',(-25.881954922732,3.68771187601412,-0.961936478150598));
#47704=CARTESIAN_POINT('Ctrl Pts',(-25.683177896242,2.80382800818523,2.58188775682714));
#47705=CARTESIAN_POINT('Ctrl Pts',(-25.4844008697521,-0.654391852565681,
3.75444098441731));
#47706=CARTESIAN_POINT('Ctrl Pts',(-25.3254170879137,-2.93965552881964,
1.93616476772919));
#47707=CARTESIAN_POINT('Ctrl Pts',(-25.2326923149053,-3.2203404239648,0.431815865334146));
#47708=CARTESIAN_POINT('Ctrl Pts',(-25.2062265507269,-3.2183080224723,0.00170933992184336));
#47709=CARTESIAN_POINT('Origin',(-26.267,-5.160062080289E-16,2.1385152528819E-16));
#47710=CARTESIAN_POINT('',(-26.267,-3.933,-4.81653586104654E-16));
#47711=CARTESIAN_POINT('Origin',(-26.267,0.,0.));
#47712=CARTESIAN_POINT('Origin',(-26.267,0.,0.));
#47713=CARTESIAN_POINT('',(-26.267,1.87158653173906,-2.62360084935056));
#47714=CARTESIAN_POINT('Ctrl Pts',(-26.267,1.75283089415088,3.52826931739087));
#47715=CARTESIAN_POINT('Ctrl Pts',(-26.267,1.82318529142576,3.48569183564302));
#47716=CARTESIAN_POINT('Ctrl Pts',(-26.267,1.89201450465608,3.44079991594677));
#47717=CARTESIAN_POINT('Ctrl Pts',(-26.267,1.95918967345583,3.39358641303125));
#47718=CARTESIAN_POINT('Ctrl Pts',(-26.267,2.05858783056501,3.32372525355339));
#47719=CARTESIAN_POINT('Ctrl Pts',(-26.267,2.15436645871861,3.2487822944279));
#47720=CARTESIAN_POINT('Ctrl Pts',(-26.267,2.2463413446018,3.16916750603609));
#47721=CARTESIAN_POINT('Ctrl Pts',(-26.267,2.29959316990593,3.12307195764421));
#47722=CARTESIAN_POINT('Ctrl Pts',(-26.267,2.35156916978231,3.07540964020356));
#47723=CARTESIAN_POINT('Ctrl Pts',(-26.267,2.40222706109326,3.02625573708493));
#47724=CARTESIAN_POINT('Ctrl Pts',(-26.267,2.44077608680837,2.98885119800362));
#47725=CARTESIAN_POINT('Ctrl Pts',(-26.267,2.47856173650469,2.95058285557362));
#47726=CARTESIAN_POINT('Ctrl Pts',(-26.267,2.51556336696653,2.91148297010551));
#47727=CARTESIAN_POINT('Ctrl Pts',(-26.267,2.5309182697087,2.89525733542134));
#47728=CARTESIAN_POINT('Ctrl Pts',(-26.267,2.54613902333768,2.87888740355848));
#47729=CARTESIAN_POINT('Ctrl Pts',(-26.267,2.56121192590708,2.86238909910956));
#47730=CARTESIAN_POINT('Ctrl Pts',(-26.267,2.6442839721244,2.7714611638046));
#47731=CARTESIAN_POINT('Ctrl Pts',(-26.267,2.72295590508143,2.67654596393466));
#47732=CARTESIAN_POINT('Ctrl Pts',(-26.267,2.79703275170125,2.57806849708916));
#47733=CARTESIAN_POINT('Ctrl Pts',(-26.267,2.8618499924936,2.49190071359935));
#47734=CARTESIAN_POINT('Ctrl Pts',(-26.267,2.92314859484406,2.40300461939636));
#47735=CARTESIAN_POINT('Ctrl Pts',(-26.267,2.98076610429264,2.31165085214935));
#47736=CARTESIAN_POINT('Ctrl Pts',(-26.267,3.0059737646764,2.27168357897878));
#47737=CARTESIAN_POINT('Ctrl Pts',(-26.267,3.03047643909033,2.23124577127131));
#47738=CARTESIAN_POINT('Ctrl Pts',(-26.267,3.05425858581036,2.19035969246717));
#47739=CARTESIAN_POINT('Ctrl Pts',(-26.267,3.06887962712138,2.16522331372566));
#47740=CARTESIAN_POINT('Ctrl Pts',(-26.267,3.08322830871726,2.13991749966683));
#47741=CARTESIAN_POINT('Ctrl Pts',(-26.267,3.09730078700632,2.11444740602352));
#47742=CARTESIAN_POINT('Ctrl Pts',(-26.267,3.10816559861413,2.09478294015024));
#47743=CARTESIAN_POINT('Ctrl Pts',(-26.267,3.11886718250786,2.07501769605134));
#47744=CARTESIAN_POINT('Ctrl Pts',(-26.267,3.12939220522335,2.05517627074448));
#47745=CARTESIAN_POINT('Ctrl Pts',(-26.267,3.18510294740167,1.95015221905346));
#47746=CARTESIAN_POINT('Ctrl Pts',(-26.267,3.23593990370189,1.84287352231398));
#47747=CARTESIAN_POINT('Ctrl Pts',(-26.267,3.28172717922646,1.73371644648934));
#47748=CARTESIAN_POINT('Ctrl Pts',(-26.267,3.32717541816672,1.62536763544387));
#47749=CARTESIAN_POINT('Ctrl Pts',(-26.267,3.36764871242685,1.51516729601585));
#47750=CARTESIAN_POINT('Ctrl Pts',(-26.267,3.40292543327883,1.40347149798005));
#47751=CARTESIAN_POINT('Ctrl Pts',(-26.267,3.43716006905266,1.29507522783728));
#47752=CARTESIAN_POINT('Ctrl Pts',(-26.267,3.46650062833312,1.18526981387765));
#47753=CARTESIAN_POINT('Ctrl Pts',(-26.267,3.49069615978602,1.07438111431325));
#47754=CARTESIAN_POINT('Ctrl Pts',(-26.267,3.50690239180499,1.000107565211));
#47755=CARTESIAN_POINT('Ctrl Pts',(-26.267,3.52079939350193,0.92534803949904));
#47756=CARTESIAN_POINT('Ctrl Pts',(-26.267,3.53229894330973,0.850202948550371));
#47757=CARTESIAN_POINT('Ctrl Pts',(-26.267,3.53786991304331,0.813798825406446));
#47758=CARTESIAN_POINT('Ctrl Pts',(-26.267,3.54287805976906,0.777304254618612));
#47759=CARTESIAN_POINT('Ctrl Pts',(-26.267,3.5473124432343,0.740730938484744));
#47760=CARTESIAN_POINT('Ctrl Pts',(-26.267,3.54918812804797,0.725260915606478));
#47761=CARTESIAN_POINT('Ctrl Pts',(-26.267,3.55096058609398,0.709781155383269));
#47762=CARTESIAN_POINT('Ctrl Pts',(-26.267,3.55262839016636,0.694300444279272));
#47763=CARTESIAN_POINT('Ctrl Pts',(-26.267,3.56460695007169,0.58311434729857));
#47764=CARTESIAN_POINT('Ctrl Pts',(-26.267,3.57120627580917,0.471755619772827));
#47765=CARTESIAN_POINT('Ctrl Pts',(-26.267,3.57222914249298,0.360540007381168));
#47766=CARTESIAN_POINT('Ctrl Pts',(-26.267,3.57281215830709,0.297149086719328));
#47767=CARTESIAN_POINT('Ctrl Pts',(-26.267,3.57158257655703,0.233804656091378));
#47768=CARTESIAN_POINT('Ctrl Pts',(-26.267,3.56849629185414,0.1705660434067));
#47769=CARTESIAN_POINT('Ctrl Pts',(-26.267,3.56297727258772,0.0574801957330568));
#47770=CARTESIAN_POINT('Ctrl Pts',(-26.267,3.55152347402166,-0.0552685595518794));
#47771=CARTESIAN_POINT('Ctrl Pts',(-26.267,3.53434939023894,-0.167322691080499));
#47772=CARTESIAN_POINT('Ctrl Pts',(-26.267,3.51709931727261,-0.279872622098812));
#47773=CARTESIAN_POINT('Ctrl Pts',(-26.267,3.49407768877409,-0.391722571953211));
#47774=CARTESIAN_POINT('Ctrl Pts',(-26.267,3.46545702485941,-0.502483636464418));
#47775=CARTESIAN_POINT('Ctrl Pts',(-26.267,3.45682536428132,-0.53588789001278));
#47776=CARTESIAN_POINT('Ctrl Pts',(-26.267,3.44768416297063,-0.569192875179334));
#47777=CARTESIAN_POINT('Ctrl Pts',(-26.267,3.4380374717033,-0.602387281756488));
#47778=CARTESIAN_POINT('Ctrl Pts',(-26.267,3.43312300749121,-0.619298025414007));
#47779=CARTESIAN_POINT('Ctrl Pts',(-26.267,3.42807681352333,-0.636181555219225));
#47780=CARTESIAN_POINT('Ctrl Pts',(-26.267,3.42290515904448,-0.653018316007086));
#47781=CARTESIAN_POINT('Ctrl Pts',(-26.267,3.39020902314041,-0.759463365875591));
#47782=CARTESIAN_POINT('Ctrl Pts',(-26.267,3.35245638616911,-0.864203255159293));
#47783=CARTESIAN_POINT('Ctrl Pts',(-26.267,3.30988295914673,-0.966911473140547));
#47784=CARTESIAN_POINT('Ctrl Pts',(-26.267,3.26726860350859,-1.06971843123938));
#47785=CARTESIAN_POINT('Ctrl Pts',(-26.267,3.21982359879886,-1.17049056087227));
#47786=CARTESIAN_POINT('Ctrl Pts',(-26.267,3.16773965001191,-1.26887337505142));
#47787=CARTESIAN_POINT('Ctrl Pts',(-26.267,3.11629546913592,-1.36604771389475));
#47788=CARTESIAN_POINT('Ctrl Pts',(-26.267,3.06032498942971,-1.46089169808994));
#47789=CARTESIAN_POINT('Ctrl Pts',(-26.267,2.99997844698005,-1.55302727802699));
#47790=CARTESIAN_POINT('Ctrl Pts',(-26.267,2.96406011993936,-1.60786647440717));
#47791=CARTESIAN_POINT('Ctrl Pts',(-26.267,2.92659089603249,-1.66174543872833));
#47792=CARTESIAN_POINT('Ctrl Pts',(-26.267,2.88759787269679,-1.71457684344143));
#47793=CARTESIAN_POINT('Ctrl Pts',(-26.267,2.86970645321483,-1.73881781638177));
#47794=CARTESIAN_POINT('Ctrl Pts',(-26.267,2.85149418486337,-1.76283816019293));
#47795=CARTESIAN_POINT('Ctrl Pts',(-26.267,2.83296348753158,-1.7866289832168));
#47796=CARTESIAN_POINT('Ctrl Pts',(-26.267,2.82442940049083,-1.79758555710183));
#47797=CARTESIAN_POINT('Ctrl Pts',(-26.267,2.81582890705879,-1.80849193308911));
#47798=CARTESIAN_POINT('Ctrl Pts',(-26.267,2.80716807563418,-1.81934019128409));
#47799=CARTESIAN_POINT('Ctrl Pts',(-26.267,2.74005470260851,-1.90340408344692));
#47800=CARTESIAN_POINT('Ctrl Pts',(-26.267,2.66922556996508,-1.98410424668023));
#47801=CARTESIAN_POINT('Ctrl Pts',(-26.267,2.5948569520778,-2.0611209847473));
#47802=CARTESIAN_POINT('Ctrl Pts',(-26.267,2.52152149137489,-2.13706777693517));
#47803=CARTESIAN_POINT('Ctrl Pts',(-26.267,2.44474361560077,-2.20943329052733));
#47804=CARTESIAN_POINT('Ctrl Pts',(-26.267,2.36466364179145,-2.27787037127922));
#47805=CARTESIAN_POINT('Ctrl Pts',(-26.267,2.28705702719922,-2.34419369653874));
#47806=CARTESIAN_POINT('Ctrl Pts',(-26.267,2.20634859789478,-2.40682779771474));
#47807=CARTESIAN_POINT('Ctrl Pts',(-26.267,2.12264725251138,-2.465412696323));
#47808=CARTESIAN_POINT('Ctrl Pts',(-26.267,2.04172880706709,-2.5220497658967));
#47809=CARTESIAN_POINT('Ctrl Pts',(-26.267,1.95801272086933,-2.57490258924474));
#47810=CARTESIAN_POINT('Ctrl Pts',(-26.267,1.87158653173909,-2.62360084935053));
#47811=CARTESIAN_POINT('Origin',(-26.267,0.,0.));
#47812=CARTESIAN_POINT('Origin',(-28.5777734492731,0.,0.));
#47813=CARTESIAN_POINT('Ctrl Pts',(-26.267,1.87158653173906,-2.62360084935056));
#47814=CARTESIAN_POINT('Ctrl Pts',(-26.20074099117,2.74538756344498,-2.00026127284245));
#47815=CARTESIAN_POINT('Ctrl Pts',(-26.06822297351,3.80572572838508,0.177707626592857));
#47816=CARTESIAN_POINT('Ctrl Pts',(-25.86944594702,1.90626263650645,3.30303297573159));
#47817=CARTESIAN_POINT('Ctrl Pts',(-25.6706689205301,-1.74511074991996,
3.38706745932803));
#47818=CARTESIAN_POINT('Ctrl Pts',(-25.5317780879477,-3.17634659584044,
1.27640733554319));
#47819=CARTESIAN_POINT('Ctrl Pts',(-25.4591462641954,-3.22750339797143,
0.104841723461124));
#47820=CARTESIAN_POINT('Ctrl Pts',(-25.4527734492731,-3.22681880944319,
0.00198271668292602));
#47821=CARTESIAN_POINT('Ctrl Pts',(-26.6770630286919,2.28405859260867,-3.20180657528379));
#47822=CARTESIAN_POINT('Ctrl Pts',(-26.6108040198619,3.35043341463937,-2.44109148587059));
#47823=CARTESIAN_POINT('Ctrl Pts',(-26.478286002202,4.64445560150136,0.21687195574883));
#47824=CARTESIAN_POINT('Ctrl Pts',(-26.279508975712,2.32637683636025,4.03097624499334));
#47825=CARTESIAN_POINT('Ctrl Pts',(-26.080731949222,-2.12970927916688,4.13353077884949));
#47826=CARTESIAN_POINT('Ctrl Pts',(-25.881954922732,-4.62948555759545,0.447081669639946));
#47827=CARTESIAN_POINT('Ctrl Pts',(-25.683177896242,-2.88011351910651,-3.65260393366682));
#47828=CARTESIAN_POINT('Ctrl Pts',(-25.4844008697521,1.51350000628727,-4.39779790151484));
#47829=CARTESIAN_POINT('Ctrl Pts',(-25.2856238432621,4.51756764805872,-1.10662356178153));
#47830=CARTESIAN_POINT('Ctrl Pts',(-25.0868468167721,3.37466122935008,3.20080160309462));
#47831=CARTESIAN_POINT('Ctrl Pts',(-24.8880697902821,-0.866183191727884,
4.56973678783709));
#47832=CARTESIAN_POINT('Ctrl Pts',(-24.6892927637922,-4.31185972195668,
1.74382019235027));
#47833=CARTESIAN_POINT('Ctrl Pts',(-24.4905157373022,-3.79932173433631,
-2.6829517902416));
#47834=CARTESIAN_POINT('Ctrl Pts',(-24.2917387108122,0.200946718919985,
-4.64678435357141));
#47835=CARTESIAN_POINT('Ctrl Pts',(-24.0929616843222,4.01674563032601,-2.34494803611166));
#47836=CARTESIAN_POINT('Ctrl Pts',(-23.8941846578323,4.14523001189322,2.10952497302619));
#47837=CARTESIAN_POINT('Ctrl Pts',(-23.6954076313422,0.468450447046365,
4.62747987472434));
#47838=CARTESIAN_POINT('Ctrl Pts',(-23.4966306048523,-3.63835961735965,
2.89747500715715));
#47839=CARTESIAN_POINT('Ctrl Pts',(-23.2978535783623,-4.40520675631299,
-1.49237231725802));
#47840=CARTESIAN_POINT('Ctrl Pts',(-23.0990765518723,-1.12813568952015,
-4.51224225015275));
#47841=CARTESIAN_POINT('Ctrl Pts',(-22.9002995253823,3.18454807402148,-3.38993727651186));
#47842=CARTESIAN_POINT('Ctrl Pts',(-22.7015224988924,4.57386135182184,0.844282761045225));
#47843=CARTESIAN_POINT('Ctrl Pts',(-22.5027454724023,1.76443397075476,4.30346298195321));
#47844=CARTESIAN_POINT('Ctrl Pts',(-22.3039684459125,-2.6647190678634,3.81212451182053));
#47845=CARTESIAN_POINT('Ctrl Pts',(-22.1051914194224,-4.64769733843289,
-0.178690872093036));
#47846=CARTESIAN_POINT('Ctrl Pts',(-21.9064143929325,-2.36415456292714,
-4.00547052921664));
#47847=CARTESIAN_POINT('Ctrl Pts',(-21.7076373664425,2.08964897909848,-4.15528436091349));
#47848=CARTESIAN_POINT('Ctrl Pts',(-21.5088603399525,4.62518403425973,-0.490605361020961));
#47849=CARTESIAN_POINT('Ctrl Pts',(-21.3100833134625,2.9148649431019,3.62444248573818));
#47850=CARTESIAN_POINT('Ctrl Pts',(-21.1113062869726,-1.47125932928464,
4.41230290861746));
#47851=CARTESIAN_POINT('Ctrl Pts',(-20.9125292604826,-4.50678814936917,
1.14973107607421));
#47852=CARTESIAN_POINT('Ctrl Pts',(-20.7137522339926,-3.40514858703943,
-3.16827777674092));
#47853=CARTESIAN_POINT('Ctrl Pts',(-20.5149752075026,0.822369673066674,
-4.57785201721419));
#47854=CARTESIAN_POINT('Ctrl Pts',(-20.3161981810127,4.29496409445361,-1.78502224017813));
#47855=CARTESIAN_POINT('Ctrl Pts',(-20.1174211545226,3.82484164829531,2.64643294571342));
#47856=CARTESIAN_POINT('Ctrl Pts',(-19.9186441280327,-0.1564318461399,4.64849976314082));
#47857=CARTESIAN_POINT('Ctrl Pts',(-19.7198671015427,-3.99410309733264,
2.38330892216325));
#47858=CARTESIAN_POINT('Ctrl Pts',(-19.5210900750527,-4.16524366145492,
-2.06972612007259));
#47859=CARTESIAN_POINT('Ctrl Pts',(-19.3223130485628,-0.512748897982449,
-4.62278158001935));
#47860=CARTESIAN_POINT('Ctrl Pts',(-19.1235360220728,3.61044217001027,-2.93218831387842));
#47861=CARTESIAN_POINT('Ctrl Pts',(-18.9247589955828,4.41929790786022,1.45011274647242));
#47862=CARTESIAN_POINT('Ctrl Pts',(-18.7259819690928,1.17130007793737,4.50123061898145));
#47863=CARTESIAN_POINT('Ctrl Pts',(-18.5272049426028,-3.1519348112702,3.42028184846639));
#47864=CARTESIAN_POINT('Ctrl Pts',(-18.3284279161129,-4.58173770662756,
-0.800437750187337));
#47865=CARTESIAN_POINT('Ctrl Pts',(-18.1296508896229,-1.80556956591054,
-4.28636669183268));
#47866=CARTESIAN_POINT('Ctrl Pts',(-17.9308738631329,2.62808612112309,-3.83747109256185));
#47867=CARTESIAN_POINT('Ctrl Pts',(-17.7320968366429,4.64919560587807,0.134169268920524));
#47868=CARTESIAN_POINT('Ctrl Pts',(-17.5333198101529,2.40240858414375,3.98264400277819));
#47869=CARTESIAN_POINT('Ctrl Pts',(-17.334542783663,-2.04975571703512,4.1751075674365));
#47870=CARTESIAN_POINT('Ctrl Pts',(-17.135765757173,-4.62027326531467,0.534880431640867));
#47871=CARTESIAN_POINT('Ctrl Pts',(-16.936988730683,-2.94944414375022,-3.59635858267975));
#47872=CARTESIAN_POINT('Ctrl Pts',(-16.738211704193,1.42893233174933,-4.42619247825972));
#47873=CARTESIAN_POINT('Ctrl Pts',(-16.539434677703,4.49557098069678,-1.19284043707613));
#47874=CARTESIAN_POINT('Ctrl Pts',(-16.3406576512131,3.43533450362267,3.1355161075428));
#47875=CARTESIAN_POINT('Ctrl Pts',(-16.1418806247231,-0.778483263328775,
4.58552502538999));
#47876=CARTESIAN_POINT('Ctrl Pts',(-15.9431035982331,-4.27767915166076,
1.82606248538427));
#47877=CARTESIAN_POINT('Ctrl Pts',(-15.7443265717431,-3.84999670245527,
-2.60965381283173));
#47878=CARTESIAN_POINT('Ctrl Pts',(-15.5455495452531,0.111872910139692,
-4.64983373543921));
#47879=CARTESIAN_POINT('Ctrl Pts',(-15.3467725187632,3.97115313116304,-2.42135829053259));
#47880=CARTESIAN_POINT('Ctrl Pts',(-15.1479954922732,4.18476020427858,2.02955430680881));
#47881=CARTESIAN_POINT('Ctrl Pts',(-14.9492184657832,0.557223801909945,
4.61801591744371));
#47882=CARTESIAN_POINT('Ctrl Pts',(-14.7504414392932,-3.58262751545605,
2.96593975542493));
#47883=CARTESIAN_POINT('Ctrl Pts',(-14.5516644128033,-4.43213866584023,
-1.40637305158682));
#47884=CARTESIAN_POINT('Ctrl Pts',(-14.3528873863133,-1.21602745322486,
-4.49244653896489));
#47885=CARTESIAN_POINT('Ctrl Pts',(-14.1541103598233,3.1225857469175,-3.44491792829022));
#47886=CARTESIAN_POINT('Ctrl Pts',(-14.0215923421633,4.09368485114861,-0.652745009784278));
#47887=CARTESIAN_POINT('Ctrl Pts',(-13.9553333333333,3.88062570733445,0.639713310456302));
#47888=CARTESIAN_POINT('Ctrl Pts',(-26.5403753524613,2.14656790565213,-3.00907133330604));
#47889=CARTESIAN_POINT('Ctrl Pts',(-26.4741163436313,3.14875146424124,-2.29414808152788));
#47890=CARTESIAN_POINT('Ctrl Pts',(-26.3415983259713,4.36487897712927,0.203817179363504));
#47891=CARTESIAN_POINT('Ctrl Pts',(-26.1428212994813,2.18633876974231,3.78832848857276));
#47892=CARTESIAN_POINT('Ctrl Pts',(-25.9440442729914,-2.00150976941791,
3.88470967234234));
#47893=CARTESIAN_POINT('Ctrl Pts',(-25.7452672465014,-4.35081006668247,
0.420169240123723));
#47894=CARTESIAN_POINT('Ctrl Pts',(-25.5464902200114,-2.70674284134183,
-3.43273259339334));
#47895=CARTESIAN_POINT('Ctrl Pts',(-25.3477131935214,1.42239369393322,-4.1330690296146));
#47896=CARTESIAN_POINT('Ctrl Pts',(-25.1489361670314,4.24562914292832,-1.04000949408466));
#47897=CARTESIAN_POINT('Ctrl Pts',(-24.9501591405415,3.17152086676461,3.008126856201));
#47898=CARTESIAN_POINT('Ctrl Pts',(-24.7513821140515,-0.814042619482387,
4.29465792068213));
#47899=CARTESIAN_POINT('Ctrl Pts',(-24.5526050875615,-4.05230396574686,
1.63884957690685));
#47900=CARTESIAN_POINT('Ctrl Pts',(-24.3538280610715,-3.57061860171385,
-2.52144941639475));
#47901=CARTESIAN_POINT('Ctrl Pts',(-24.1550510345816,0.188850574576165,
-4.36706754815366));
#47902=CARTESIAN_POINT('Ctrl Pts',(-23.9562740080916,3.77495449684529,-2.20379206165209));
#47903=CARTESIAN_POINT('Ctrl Pts',(-23.7574969816016,3.89570466093576,1.98254047331505));
#47904=CARTESIAN_POINT('Ctrl Pts',(-23.5587199551116,0.440251707321398,
4.34892511745484));
#47905=CARTESIAN_POINT('Ctrl Pts',(-23.3599429286216,-3.41934572480692,
2.72305924108939));
#47906=CARTESIAN_POINT('Ctrl Pts',(-23.1611659021317,-4.14003190262443,
-1.40253780260996));
#47907=CARTESIAN_POINT('Ctrl Pts',(-22.9623888756417,-1.06022668252956,
-4.2406243114994));
#47908=CARTESIAN_POINT('Ctrl Pts',(-22.7636118491517,2.99285172097684,-3.18587736036281));
#47909=CARTESIAN_POINT('Ctrl Pts',(-22.5648348226617,4.29853420332353,0.793460502291752));
#47910=CARTESIAN_POINT('Ctrl Pts',(-22.3660577961718,1.65822249285589,4.0444126740515));
#47911=CARTESIAN_POINT('Ctrl Pts',(-22.1672807696817,-2.50431422694893,
3.58265070603016));
#47912=CARTESIAN_POINT('Ctrl Pts',(-21.9685037431918,-4.3679255751799,-0.167934435793016));
#47913=CARTESIAN_POINT('Ctrl Pts',(-21.7697267167018,-2.2218424366182,-3.76435810923392));
#47914=CARTESIAN_POINT('Ctrl Pts',(-21.5709496902118,1.96386093033125,-3.90515378058136));
#47915=CARTESIAN_POINT('Ctrl Pts',(-21.3721726637218,4.34676747689614,-0.461072988983897));
#47916=CARTESIAN_POINT('Ctrl Pts',(-21.1733956372319,2.73940237628791,3.40626634576907));
#47917=CARTESIAN_POINT('Ctrl Pts',(-20.9746186107419,-1.38269572740107,
4.14670089651087));
#47918=CARTESIAN_POINT('Ctrl Pts',(-20.7758415842519,-4.23549852456288,
1.08052211796066));
#47919=CARTESIAN_POINT('Ctrl Pts',(-20.577064557762,-3.20017301419894,-2.97756082692059));
#47920=CARTESIAN_POINT('Ctrl Pts',(-20.3782875312719,0.772866489721012,
-4.30228464750265));
#47921=CARTESIAN_POINT('Ctrl Pts',(-20.179510504782,4.03642538370816,-1.67757143535682));
#47922=CARTESIAN_POINT('Ctrl Pts',(-19.980733478292,3.59460232456433,2.4871288521722));
#47923=CARTESIAN_POINT('Ctrl Pts',(-19.781956451802,-0.147015309253664,
4.36867969730722));
#47924=CARTESIAN_POINT('Ctrl Pts',(-19.583179425312,-3.75367494877086,2.23984378427304));
#47925=CARTESIAN_POINT('Ctrl Pts',(-19.3844023988221,-3.91451357326538,
-1.94513734333037));
#47926=CARTESIAN_POINT('Ctrl Pts',(-19.1856253723321,-0.481883578481456,
-4.344509640261));
#47927=CARTESIAN_POINT('Ctrl Pts',(-18.9868483458421,3.3931087899569,-2.75568295326037));
#47928=CARTESIAN_POINT('Ctrl Pts',(-18.7880713193521,4.153274826323,1.36282207962083));
#47929=CARTESIAN_POINT('Ctrl Pts',(-18.5892942928622,1.10079275694786,4.23027553404785));
#47930=CARTESIAN_POINT('Ctrl Pts',(-18.3905172663722,-2.9622016389925,3.21439531716091));
#47931=CARTESIAN_POINT('Ctrl Pts',(-18.1917402398822,-4.30593643481365,
-0.752254776031014));
#47932=CARTESIAN_POINT('Ctrl Pts',(-17.9929632133922,-1.69688189880417,
-4.02834550843798));
#47933=CARTESIAN_POINT('Ctrl Pts',(-17.7941861869023,2.46988642898584,-3.60647152959107));
#47934=CARTESIAN_POINT('Ctrl Pts',(-17.5954091604123,4.36933365324861,0.126092845219305));
#47935=CARTESIAN_POINT('Ctrl Pts',(-17.3966321339223,2.25779372721619,3.74290564334323));
#47936=CARTESIAN_POINT('Ctrl Pts',(-17.1978551074323,-1.92636907426674,
3.92378371373942));
#47937=CARTESIAN_POINT('Ctrl Pts',(-16.9990780809424,-4.34215231551471,
0.502682887224133));
#47938=CARTESIAN_POINT('Ctrl Pts',(-16.8003010544524,-2.77190005500552,
-3.37987297514113));
#47939=CARTESIAN_POINT('Ctrl Pts',(-16.6015240279624,1.34291663646797,-4.15975437268433));
#47940=CARTESIAN_POINT('Ctrl Pts',(-16.4027470014724,4.2249565821003,-1.12103647738179));
#47941=CARTESIAN_POINT('Ctrl Pts',(-16.2039699749824,3.22854186600948,2.94677127193112));
#47942=CARTESIAN_POINT('Ctrl Pts',(-16.0051929484924,-0.731621856618111,
4.30949577297171));
#47943=CARTESIAN_POINT('Ctrl Pts',(-15.8064159220025,-4.02018092151693,
1.71614123101997));
#47944=CARTESIAN_POINT('Ctrl Pts',(-15.6076388955125,-3.61824315063571,
-2.45256366785642));
#47945=CARTESIAN_POINT('Ctrl Pts',(-15.4088618690225,0.105138633130912,
-4.36993337010353));
#47946=CARTESIAN_POINT('Ctrl Pts',(-15.2100848425326,3.73210647369982,-2.27560274126138));
#47947=CARTESIAN_POINT('Ctrl Pts',(-15.0113078160425,3.93285530258446,1.90738370367203));
#47948=CARTESIAN_POINT('Ctrl Pts',(-14.8125307895526,0.523681280907598,
4.340030850458));
#47949=CARTESIAN_POINT('Ctrl Pts',(-14.6137537630626,-3.36696846020962,
2.78740270048038));
#47950=CARTESIAN_POINT('Ctrl Pts',(-14.4149767365726,-4.16534262486954,
-1.32171532975536));
#47951=CARTESIAN_POINT('Ctrl Pts',(-14.2161997100827,-1.14282773302373,
-4.22202021857335));
#47952=CARTESIAN_POINT('Ctrl Pts',(-14.0174226835927,2.93461926444034,-3.23754840896076));
#47953=CARTESIAN_POINT('Ctrl Pts',(-13.8849046659327,3.84726230131148,-0.613452515233941));
#47954=CARTESIAN_POINT('Ctrl Pts',(-13.8186456571027,3.64702841869692,0.601205269202682));
#47955=CARTESIAN_POINT('Ctrl Pts',(-26.4036876762306,2.00907721869559,-2.8163360913283));
#47956=CARTESIAN_POINT('Ctrl Pts',(-26.3374286674006,2.94706951384311,-2.14720467718516));
#47957=CARTESIAN_POINT('Ctrl Pts',(-26.2049106497406,4.08530235275718,0.190762402978181));
#47958=CARTESIAN_POINT('Ctrl Pts',(-26.0061336232507,2.04630070312438,3.54568073215218));
#47959=CARTESIAN_POINT('Ctrl Pts',(-25.8073565967607,-1.87331025966893,
3.63588856583518));
#47960=CARTESIAN_POINT('Ctrl Pts',(-25.6085795702707,-4.0721345757695,0.3932568106075));
#47961=CARTESIAN_POINT('Ctrl Pts',(-25.4098025437808,-2.53337216357714,
-3.21286125311987));
#47962=CARTESIAN_POINT('Ctrl Pts',(-25.2110255172908,1.33128738157918,-3.86834015771436));
#47963=CARTESIAN_POINT('Ctrl Pts',(-25.0122484908008,3.97369063779791,-0.973395426387776));
#47964=CARTESIAN_POINT('Ctrl Pts',(-24.8134714643108,2.96838050417913,2.81545210930738));
#47965=CARTESIAN_POINT('Ctrl Pts',(-24.6146944378208,-0.761902047236896,
4.01957905352718));
#47966=CARTESIAN_POINT('Ctrl Pts',(-24.4159174113309,-3.79274820953704,
1.53387896146343));
#47967=CARTESIAN_POINT('Ctrl Pts',(-24.2171403848409,-3.34191546909139,
-2.3599470425479));
#47968=CARTESIAN_POINT('Ctrl Pts',(-24.0183633583509,0.176754430232343,
-4.0873507427359));
#47969=CARTESIAN_POINT('Ctrl Pts',(-23.8195863318609,3.53316336336457,-2.06263608719252));
#47970=CARTESIAN_POINT('Ctrl Pts',(-23.6208093053709,3.64617930997828,1.85555597360391));
#47971=CARTESIAN_POINT('Ctrl Pts',(-23.422032278881,0.412052967596436,4.07037036018533));
#47972=CARTESIAN_POINT('Ctrl Pts',(-23.223255252391,-3.2003318322542,2.54864347502163));
#47973=CARTESIAN_POINT('Ctrl Pts',(-23.024478225901,-3.87485704893586,-1.31270328796191));
#47974=CARTESIAN_POINT('Ctrl Pts',(-22.825701199411,-0.992317675538989,
-3.96900637284604));
#47975=CARTESIAN_POINT('Ctrl Pts',(-22.6269241729211,2.80115536793221,-2.98181744421376));
#47976=CARTESIAN_POINT('Ctrl Pts',(-22.4281471464311,4.02320705482523,0.742638243538281));
#47977=CARTESIAN_POINT('Ctrl Pts',(-22.2293701199411,1.55201101495703,3.7853623661498));
#47978=CARTESIAN_POINT('Ctrl Pts',(-22.0305930934511,-2.34390938603446,
3.35317690023979));
#47979=CARTESIAN_POINT('Ctrl Pts',(-21.8318160669611,-4.08815381192692,
-0.157177999492998));
#47980=CARTESIAN_POINT('Ctrl Pts',(-21.6330390404712,-2.07953031030926,
-3.52324568925121));
#47981=CARTESIAN_POINT('Ctrl Pts',(-21.4342620139812,1.83807288156401,-3.65502320024922));
#47982=CARTESIAN_POINT('Ctrl Pts',(-21.2354849874912,4.06835091953256,-0.431540616946836));
#47983=CARTESIAN_POINT('Ctrl Pts',(-21.0367079610012,2.56393980947392,3.18809020579997));
#47984=CARTESIAN_POINT('Ctrl Pts',(-20.8379309345113,-1.29413212551749,
3.88109888440429));
#47985=CARTESIAN_POINT('Ctrl Pts',(-20.6391539080213,-3.96420889975659,
1.0113131598471));
#47986=CARTESIAN_POINT('Ctrl Pts',(-20.4403768815313,-2.99519744135846,
-2.78684387710026));
#47987=CARTESIAN_POINT('Ctrl Pts',(-20.2415998550413,0.723363306375352,
-4.02671727779112));
#47988=CARTESIAN_POINT('Ctrl Pts',(-20.0428228285513,3.7778866729627,-1.57012063053551));
#47989=CARTESIAN_POINT('Ctrl Pts',(-19.8440458020614,3.36436300083335,2.32782475863098));
#47990=CARTESIAN_POINT('Ctrl Pts',(-19.6452687755714,-0.137598772367427,
4.0888596314736));
#47991=CARTESIAN_POINT('Ctrl Pts',(-19.4464917490814,-3.51324680020908,
2.09637864638283));
#47992=CARTESIAN_POINT('Ctrl Pts',(-19.2477147225914,-3.66378348507584,
-1.82054856658815));
#47993=CARTESIAN_POINT('Ctrl Pts',(-19.0489376961015,-0.451018258980463,
-4.06623770050266));
#47994=CARTESIAN_POINT('Ctrl Pts',(-18.8501606696115,3.17577540990353,-2.57917759264233));
#47995=CARTESIAN_POINT('Ctrl Pts',(-18.6513836431215,3.88725174478577,1.27553141276924));
#47996=CARTESIAN_POINT('Ctrl Pts',(-18.4526066166315,1.03028543595836,3.95932044911425));
#47997=CARTESIAN_POINT('Ctrl Pts',(-18.2538295901415,-2.7724684667148,3.00850878585543));
#47998=CARTESIAN_POINT('Ctrl Pts',(-18.0550525636516,-4.03013516299975,
-0.704071801874699));
#47999=CARTESIAN_POINT('Ctrl Pts',(-17.8562755371616,-1.5881942316978,-3.77032432504327));
#48000=CARTESIAN_POINT('Ctrl Pts',(-17.6574985106716,2.31168673684857,-3.3754719666203));
#48001=CARTESIAN_POINT('Ctrl Pts',(-17.4587214841816,4.08947170061916,0.118016421518091));
#48002=CARTESIAN_POINT('Ctrl Pts',(-17.2599444576917,2.11317887028864,3.50316728390827));
#48003=CARTESIAN_POINT('Ctrl Pts',(-17.0611674312017,-1.80298243149837,
3.67245986004234));
#48004=CARTESIAN_POINT('Ctrl Pts',(-16.8623904047117,-4.06403136571475,
0.470485342807395));
#48005=CARTESIAN_POINT('Ctrl Pts',(-16.6636133782217,-2.59435596626082,
-3.16338736760251));
#48006=CARTESIAN_POINT('Ctrl Pts',(-16.4648363517318,1.2569009411866,-3.89331626710894));
#48007=CARTESIAN_POINT('Ctrl Pts',(-16.2660593252418,3.95434218350383,-1.04923251768746));
#48008=CARTESIAN_POINT('Ctrl Pts',(-16.0672822987518,3.02174922839628,2.75802643631945));
#48009=CARTESIAN_POINT('Ctrl Pts',(-15.8685052722618,-0.684760449907449,
4.03346652055343));
#48010=CARTESIAN_POINT('Ctrl Pts',(-15.6697282457718,-3.76268269137311,
1.60621997665568));
#48011=CARTESIAN_POINT('Ctrl Pts',(-15.4709512192819,-3.38648959881615,
-2.29547352288112));
#48012=CARTESIAN_POINT('Ctrl Pts',(-15.2721741927919,0.0984043561221374,
-4.09003300476785));
#48013=CARTESIAN_POINT('Ctrl Pts',(-15.0733971663019,3.49305981623661,-2.12984719199018));
#48014=CARTESIAN_POINT('Ctrl Pts',(-14.8746201398119,3.68095040089034,1.78521310053525));
#48015=CARTESIAN_POINT('Ctrl Pts',(-14.6758431133219,0.490138759905249,
4.06204578347229));
#48016=CARTESIAN_POINT('Ctrl Pts',(-14.477066086832,-3.15130940496319,2.60886564553584));
#48017=CARTESIAN_POINT('Ctrl Pts',(-14.278289060342,-3.89854658389887,-1.2370576079239));
#48018=CARTESIAN_POINT('Ctrl Pts',(-14.079512033852,-1.0696280128226,-3.95159389818181));
#48019=CARTESIAN_POINT('Ctrl Pts',(-13.880735007362,2.74665278196318,-3.03017888963131));
#48020=CARTESIAN_POINT('Ctrl Pts',(-13.748216989702,3.60083975147436,-0.574160020683605));
#48021=CARTESIAN_POINT('Ctrl Pts',(-13.681957980872,3.41343113005938,0.562697227949063));
#48022=CARTESIAN_POINT('Ctrl Pts',(-26.267,1.87158653173906,-2.62360084935056));
#48023=CARTESIAN_POINT('Ctrl Pts',(-26.20074099117,2.74538756344498,-2.00026127284245));
#48024=CARTESIAN_POINT('Ctrl Pts',(-26.06822297351,3.80572572838508,0.177707626592857));
#48025=CARTESIAN_POINT('Ctrl Pts',(-25.86944594702,1.90626263650645,3.30303297573159));
#48026=CARTESIAN_POINT('Ctrl Pts',(-25.6706689205301,-1.74511074991996,
3.38706745932803));
#48027=CARTESIAN_POINT('Ctrl Pts',(-25.47189189404,-3.79345908485653,0.366344381091274));
#48028=CARTESIAN_POINT('Ctrl Pts',(-25.2731148675501,-2.36000148581246,
-2.99298991284639));
#48029=CARTESIAN_POINT('Ctrl Pts',(-25.0743378410601,1.24018106922513,-3.60361128581411));
#48030=CARTESIAN_POINT('Ctrl Pts',(-24.8755608145702,3.70175213266751,-0.906781358690897));
#48031=CARTESIAN_POINT('Ctrl Pts',(-24.6767837880802,2.76524014159366,2.62277736241376));
#48032=CARTESIAN_POINT('Ctrl Pts',(-24.4780067615902,-0.709761474991402,
3.74450018637222));
#48033=CARTESIAN_POINT('Ctrl Pts',(-24.2792297351002,-3.53319245332722,
1.42890834602001));
#48034=CARTESIAN_POINT('Ctrl Pts',(-24.0804527086102,-3.11321233646892,
-2.19844466870105));
#48035=CARTESIAN_POINT('Ctrl Pts',(-23.8816756821203,0.16465828588852,-3.80763393731814));
#48036=CARTESIAN_POINT('Ctrl Pts',(-23.6828986556303,3.29137222988386,-1.92148011273296));
#48037=CARTESIAN_POINT('Ctrl Pts',(-23.4841216291403,3.39665395902081,1.72857147389278));
#48038=CARTESIAN_POINT('Ctrl Pts',(-23.2853446026503,0.383854227871474,
3.79181560291581));
#48039=CARTESIAN_POINT('Ctrl Pts',(-23.0865675761604,-2.98131793970147,
2.37422770895388));
#48040=CARTESIAN_POINT('Ctrl Pts',(-22.8877905496704,-3.60968219524731,
-1.22286877331386));
#48041=CARTESIAN_POINT('Ctrl Pts',(-22.6890135231804,-0.924408668548408,
-3.69738843419269));
#48042=CARTESIAN_POINT('Ctrl Pts',(-22.4902364966904,2.60945901488757,-2.7777575280647));
#48043=CARTESIAN_POINT('Ctrl Pts',(-22.2914594702004,3.74787990632693,0.691815984784808));
#48044=CARTESIAN_POINT('Ctrl Pts',(-22.0926824437105,1.44579953705816,3.52631205824809));
#48045=CARTESIAN_POINT('Ctrl Pts',(-21.8939054172205,-2.18350454511998,
3.12370309444941));
#48046=CARTESIAN_POINT('Ctrl Pts',(-21.6951283907305,-3.80838204867393,
-0.146421563192979));
#48047=CARTESIAN_POINT('Ctrl Pts',(-21.4963513642405,-1.93721818400033,
-3.28213326926849));
#48048=CARTESIAN_POINT('Ctrl Pts',(-21.2975743377506,1.71228483279679,-3.40489261991708));
#48049=CARTESIAN_POINT('Ctrl Pts',(-21.0987973112606,3.78993436216897,-0.402008244909776));
#48050=CARTESIAN_POINT('Ctrl Pts',(-20.9000202847706,2.38847724265994,2.96991406583087));
#48051=CARTESIAN_POINT('Ctrl Pts',(-20.7012432582806,-1.20556852363392,
3.6154968722977));
#48052=CARTESIAN_POINT('Ctrl Pts',(-20.5024662317906,-3.6929192749503,0.942104201733542));
#48053=CARTESIAN_POINT('Ctrl Pts',(-20.3036892053007,-2.79022186851798,
-2.59612692727992));
#48054=CARTESIAN_POINT('Ctrl Pts',(-20.1049121788107,0.673860123029691,
-3.75114990807958));
#48055=CARTESIAN_POINT('Ctrl Pts',(-19.9061351523207,3.51934796221725,-1.4626698257142));
#48056=CARTESIAN_POINT('Ctrl Pts',(-19.7073581258307,3.13412367710237,2.16852066508976));
#48057=CARTESIAN_POINT('Ctrl Pts',(-19.5085810993407,-0.128182235481189,
3.80903956563999));
#48058=CARTESIAN_POINT('Ctrl Pts',(-19.3098040728508,-3.27281865164731,
1.95291350849262));
#48059=CARTESIAN_POINT('Ctrl Pts',(-19.1110270463608,-3.41305339688629,
-1.69595978984593));
#48060=CARTESIAN_POINT('Ctrl Pts',(-18.9122500198708,-0.420152939479476,
-3.78796576074431));
#48061=CARTESIAN_POINT('Ctrl Pts',(-18.7134729933808,2.95844202985016,-2.40267223202429));
#48062=CARTESIAN_POINT('Ctrl Pts',(-18.5146959668909,3.62122866324853,1.18824074591766));
#48063=CARTESIAN_POINT('Ctrl Pts',(-18.3159189404009,0.959778114968857,
3.68836536418065));
#48064=CARTESIAN_POINT('Ctrl Pts',(-18.1171419139109,-2.58273529443711,
2.80262225454995));
#48065=CARTESIAN_POINT('Ctrl Pts',(-17.9183648874209,-3.75433389118585,
-0.655888827718381));
#48066=CARTESIAN_POINT('Ctrl Pts',(-17.719587860931,-1.47950656459142,-3.51230314164857));
#48067=CARTESIAN_POINT('Ctrl Pts',(-17.520810834441,2.15348704471131,-3.14447240364953));
#48068=CARTESIAN_POINT('Ctrl Pts',(-17.322033807951,3.80960974798971,0.109939997816874));
#48069=CARTESIAN_POINT('Ctrl Pts',(-17.123256781461,1.96856401336108,3.2634289244733));
#48070=CARTESIAN_POINT('Ctrl Pts',(-16.924479754971,-1.67959578872999,3.42113600634526));
#48071=CARTESIAN_POINT('Ctrl Pts',(-16.725702728481,-3.78591041591479,0.438287798390658));
#48072=CARTESIAN_POINT('Ctrl Pts',(-16.5269257019911,-2.41681187751612,
-2.94690176006388));
#48073=CARTESIAN_POINT('Ctrl Pts',(-16.3281486755011,1.17088524590524,-3.62687816153355));
#48074=CARTESIAN_POINT('Ctrl Pts',(-16.1293716490111,3.68372778490734,-0.977428557993123));
#48075=CARTESIAN_POINT('Ctrl Pts',(-15.9305946225211,2.81495659078308,2.56928160070777));
#48076=CARTESIAN_POINT('Ctrl Pts',(-15.7318175960312,-0.637899043196787,
3.75743726813516));
#48077=CARTESIAN_POINT('Ctrl Pts',(-15.5330405695412,-3.50518446122928,
1.49629872229138));
#48078=CARTESIAN_POINT('Ctrl Pts',(-15.3342635430512,-3.1547360469966,-2.13838337790581));
#48079=CARTESIAN_POINT('Ctrl Pts',(-15.1354865165612,0.0916700791133597,
-3.81013263943217));
#48080=CARTESIAN_POINT('Ctrl Pts',(-14.9367094900712,3.25401315877339,-1.98409164271898));
#48081=CARTESIAN_POINT('Ctrl Pts',(-14.7379324635813,3.42904549919622,1.66304249739848));
#48082=CARTESIAN_POINT('Ctrl Pts',(-14.5391554370913,0.456596238902905,
3.78406071648658));
#48083=CARTESIAN_POINT('Ctrl Pts',(-14.3403784106013,-2.93565034971678,
2.4303285905913));
#48084=CARTESIAN_POINT('Ctrl Pts',(-14.1416013841113,-3.63175054292818,
-1.15239988609244));
#48085=CARTESIAN_POINT('Ctrl Pts',(-13.9428243576214,-0.996428292621477,
-3.68116757779027));
#48086=CARTESIAN_POINT('Ctrl Pts',(-13.7440473311314,2.55868629948601,-2.82280937030186));
#48087=CARTESIAN_POINT('Ctrl Pts',(-13.6115293134714,3.35441720163723,-0.534867526133269));
#48088=CARTESIAN_POINT('Ctrl Pts',(-13.5452703046414,3.17983384142184,0.524189186695443));
#48089=CARTESIAN_POINT('Ctrl Pts',(-13.9553333333333,3.88062570733446,0.639713310456247));
#48090=CARTESIAN_POINT('Ctrl Pts',(-14.0215923421633,4.0936848511486,-0.652745009784315));
#48091=CARTESIAN_POINT('Ctrl Pts',(-14.0878513509933,3.60813529903304,-2.04883146903726));
#48092=CARTESIAN_POINT('Ctrl Pts',(-14.1541103598233,2.64225832295155,-2.92146280044285));
#48093=CARTESIAN_POINT('Ctrl Pts',(-14.2203693686533,1.67638134687004,-3.79409413184845));
#48094=CARTESIAN_POINT('Ctrl Pts',(-14.2866283774833,0.2301769468226,-4.14327033540667));
#48095=CARTESIAN_POINT('Ctrl Pts',(-14.3528873863133,-1.02894378863703,
-3.8035128559561));
#48096=CARTESIAN_POINT('Ctrl Pts',(-14.4191463951433,-2.28806452409662,
-3.46375537650554));
#48097=CARTESIAN_POINT('Ctrl Pts',(-14.4854054039733,-3.36010159496844,
-2.43506421404616));
#48098=CARTESIAN_POINT('Ctrl Pts',(-14.5516644128033,-3.75453493867364,
-1.19199983164787));
#48099=CARTESIAN_POINT('Ctrl Pts',(-14.5720551011905,-3.87591869528357,
-0.809456553166102));
#48100=CARTESIAN_POINT('Ctrl Pts',(-14.5924457895778,-3.93312984357014,
-0.406611012275522));
#48101=CARTESIAN_POINT('Ctrl Pts',(-14.612836477965,-3.92993428904087,-0.00292452251886177));
#48102=CARTESIAN_POINT('Origin',(0.4,7.96243204728166,-1.20090627961635));
#48103=CARTESIAN_POINT('',(6.4,7.90447580357277,-1.2325835755569));
#48104=CARTESIAN_POINT('',(0.4,7.90447580357277,-1.2325835755569));
#48105=CARTESIAN_POINT('',(3.25,7.90447580357277,-1.2325835755569));
#48106=CARTESIAN_POINT('',(6.4,7.68150047349522,-1.35445578580206));
#48107=CARTESIAN_POINT('',(6.4,7.96243204728166,-1.20090627961635));
#48108=CARTESIAN_POINT('',(0.4,7.68150047349522,-1.35445578580206));
#48109=CARTESIAN_POINT('',(0.4,7.68150047349522,-1.35445578580206));
#48110=CARTESIAN_POINT('',(0.4,7.96243204728166,-1.20090627961635));
#48111=CARTESIAN_POINT('Origin',(0.4,7.80460144262175,-1.37616180801042));
#48112=CARTESIAN_POINT('',(0.4,7.84934599497093,-1.54524025679951));
#48113=CARTESIAN_POINT('Origin',(0.4,0.,0.));
#48114=CARTESIAN_POINT('',(0.4,7.68150047349522,-1.35445578580206));
#48115=CARTESIAN_POINT('Origin',(0.4,7.68150047349522,-1.35445578580206));
#48116=CARTESIAN_POINT('',(6.4,7.84934599497093,-1.54524025679951));
#48117=CARTESIAN_POINT('',(3.25,7.84934599497093,-1.54524025679951));
#48118=CARTESIAN_POINT('',(6.4,7.68150047349522,-1.35445578580206));
#48119=CARTESIAN_POINT('Origin',(6.4,7.80460144262175,-1.37616180801042));
#48120=CARTESIAN_POINT('Origin',(6.4,0.,0.));
#48121=CARTESIAN_POINT('Origin',(0.4,7.63292962599169,-2.56532362961446));
#48122=CARTESIAN_POINT('',(6.4,7.57035316313822,-2.58645568014671));
#48123=CARTESIAN_POINT('',(0.4,7.57035316313822,-2.58645568014671));
#48124=CARTESIAN_POINT('',(3.25,7.57035316313822,-2.58645568014671));
#48125=CARTESIAN_POINT('',(6.4,7.32960244213008,-2.66775711794022));
#48126=CARTESIAN_POINT('',(6.4,7.63292962599169,-2.56532362961446));
#48127=CARTESIAN_POINT('',(0.4,7.32960244213008,-2.66775711794022));
#48128=CARTESIAN_POINT('',(0.4,7.32960244213008,-2.66775711794022));
#48129=CARTESIAN_POINT('',(0.4,7.63292962599169,-2.56532362961446));
#48130=CARTESIAN_POINT('Origin',(0.4,7.44706401972832,-2.71050963585593));
#48131=CARTESIAN_POINT('',(0.4,7.46176863727188,-2.88478921306666));
#48132=CARTESIAN_POINT('Origin',(0.4,0.,0.));
#48133=CARTESIAN_POINT('',(0.4,7.32960244213008,-2.66775711794022));
#48134=CARTESIAN_POINT('Origin',(0.4,7.32960244213008,-2.66775711794022));
#48135=CARTESIAN_POINT('',(6.4,7.46176863727188,-2.88478921306666));
#48136=CARTESIAN_POINT('',(3.25,7.46176863727188,-2.88478921306666));
#48137=CARTESIAN_POINT('',(6.4,7.32960244213008,-2.66775711794022));
#48138=CARTESIAN_POINT('Origin',(6.4,7.44706401972832,-2.71050963585593));
#48139=CARTESIAN_POINT('Origin',(6.4,0.,0.));
#48140=CARTESIAN_POINT('Origin',(0.4,7.07150450046473,-3.85179491924312));
#48141=CARTESIAN_POINT('',(6.4,7.00620917262526,-3.86173963770497));
#48142=CARTESIAN_POINT('',(0.4,7.00620917262526,-3.86173963770497));
#48143=CARTESIAN_POINT('',(3.25,7.00620917262526,-3.86173963770497));
#48144=CARTESIAN_POINT('',(6.4,6.75499814951862,-3.9));
#48145=CARTESIAN_POINT('',(6.4,7.07150450046473,-3.85179491924312));
#48146=CARTESIAN_POINT('',(0.4,6.75499814951862,-3.9));
#48147=CARTESIAN_POINT('',(0.4,6.75499814951862,-3.9));
#48148=CARTESIAN_POINT('',(0.4,7.07150450046473,-3.85179491924312));
#48149=CARTESIAN_POINT('Origin',(0.4,6.86325132499167,-3.9625));
#48150=CARTESIAN_POINT('',(0.4,6.84746921536645,-4.13668530886854));
#48151=CARTESIAN_POINT('Origin',(0.4,0.,0.));
#48152=CARTESIAN_POINT('',(0.4,6.75499814951862,-3.9));
#48153=CARTESIAN_POINT('Origin',(0.4,6.75499814951862,-3.9));
#48154=CARTESIAN_POINT('',(6.4,6.84746921536645,-4.13668530886854));
#48155=CARTESIAN_POINT('',(3.25,6.84746921536645,-4.13668530886854));
#48156=CARTESIAN_POINT('',(6.4,6.75499814951862,-3.9));
#48157=CARTESIAN_POINT('Origin',(6.4,6.86325132499167,-3.9625));
#48158=CARTESIAN_POINT('Origin',(6.4,0.,0.));
#48159=CARTESIAN_POINT('Origin',(0.4,6.29521528904508,-5.02123136935285));
#48160=CARTESIAN_POINT('',(6.4,6.22918506171498,-5.01968659050612));
#48161=CARTESIAN_POINT('',(0.4,6.22918506171498,-5.01968659050612));
#48162=CARTESIAN_POINT('',(3.25,6.22918506171498,-5.01968659050612));
#48163=CARTESIAN_POINT('',(6.4,5.97514665632803,-5.01374335555501));
#48164=CARTESIAN_POINT('',(6.4,6.29521528904508,-5.02123136935285));
#48165=CARTESIAN_POINT('',(0.4,5.97514665632803,-5.01374335555501));
#48166=CARTESIAN_POINT('',(0.4,5.97514665632803,-5.01374335555501));
#48167=CARTESIAN_POINT('',(0.4,6.29521528904508,-5.02123136935285));
#48168=CARTESIAN_POINT('Origin',(0.4,6.0709022117179,-5.09409180676583));
#48169=CARTESIAN_POINT('',(0.4,6.02511290633871,-5.26289031482423));
#48170=CARTESIAN_POINT('Origin',(0.4,0.,0.));
#48171=CARTESIAN_POINT('',(0.4,5.97514665632803,-5.01374335555501));
#48172=CARTESIAN_POINT('Origin',(0.4,5.97514665632803,-5.01374335555501));
#48173=CARTESIAN_POINT('',(6.4,6.02511290633871,-5.26289031482423));
#48174=CARTESIAN_POINT('',(3.25,6.02511290633871,-5.26289031482423));
#48175=CARTESIAN_POINT('',(6.4,5.97514665632803,-5.01374335555501));
#48176=CARTESIAN_POINT('Origin',(6.4,6.0709022117179,-5.09409180676583));
#48177=CARTESIAN_POINT('Origin',(6.4,0.,0.));
#48178=CARTESIAN_POINT('Origin',(0.4,5.32764914660044,-6.03810024517047));
#48179=CARTESIAN_POINT('',(6.4,5.26289031482423,-6.02511290633871));
#48180=CARTESIAN_POINT('',(0.4,5.26289031482423,-6.02511290633871));
#48181=CARTESIAN_POINT('',(3.25,5.26289031482423,-6.02511290633871));
#48182=CARTESIAN_POINT('',(6.4,5.01374335555501,-5.97514665632803));
#48183=CARTESIAN_POINT('',(6.4,5.32764914660044,-6.03810024517047));
#48184=CARTESIAN_POINT('',(0.4,5.01374335555501,-5.97514665632803));
#48185=CARTESIAN_POINT('',(0.4,5.01374335555501,-5.97514665632803));
#48186=CARTESIAN_POINT('',(0.4,5.32764914660044,-6.03810024517047));
#48187=CARTESIAN_POINT('Origin',(0.4,5.09409180676582,-6.0709022117179));
#48188=CARTESIAN_POINT('',(0.4,5.01968659050612,-6.22918506171498));
#48189=CARTESIAN_POINT('Origin',(0.4,0.,0.));
#48190=CARTESIAN_POINT('',(0.4,5.01374335555501,-5.97514665632803));
#48191=CARTESIAN_POINT('Origin',(0.4,5.01374335555501,-5.97514665632803));
#48192=CARTESIAN_POINT('',(6.4,5.01968659050612,-6.22918506171498));
#48193=CARTESIAN_POINT('',(3.25,5.01968659050612,-6.22918506171498));
#48194=CARTESIAN_POINT('',(6.4,5.01374335555501,-5.97514665632803));
#48195=CARTESIAN_POINT('Origin',(6.4,5.09409180676582,-6.0709022117179));
#48196=CARTESIAN_POINT('Origin',(6.4,0.,0.));
#48197=CARTESIAN_POINT('Origin',(0.4,4.19820508075689,-6.87150450046473));
#48198=CARTESIAN_POINT('',(6.4,4.13668530886854,-6.84746921536645));
#48199=CARTESIAN_POINT('',(0.4,4.13668530886854,-6.84746921536645));
#48200=CARTESIAN_POINT('',(3.25,4.13668530886854,-6.84746921536645));
#48201=CARTESIAN_POINT('',(6.4,3.9,-6.75499814951862));
#48202=CARTESIAN_POINT('',(6.4,4.19820508075689,-6.87150450046473));
#48203=CARTESIAN_POINT('',(0.4,3.9,-6.75499814951862));
#48204=CARTESIAN_POINT('',(0.4,3.9,-6.75499814951862));
#48205=CARTESIAN_POINT('',(0.4,4.19820508075689,-6.87150450046473));
#48206=CARTESIAN_POINT('Origin',(0.4,3.9625,-6.86325132499168));
#48207=CARTESIAN_POINT('',(0.4,3.86173963770497,-7.00620917262526));
#48208=CARTESIAN_POINT('Origin',(0.4,0.,0.));
#48209=CARTESIAN_POINT('',(0.4,3.9,-6.75499814951862));
#48210=CARTESIAN_POINT('Origin',(0.4,3.9,-6.75499814951862));
#48211=CARTESIAN_POINT('',(6.4,3.86173963770497,-7.00620917262526));
#48212=CARTESIAN_POINT('',(3.25,3.86173963770497,-7.00620917262526));
#48213=CARTESIAN_POINT('',(6.4,3.9,-6.75499814951862));
#48214=CARTESIAN_POINT('Origin',(6.4,3.9625,-6.86325132499168));
#48215=CARTESIAN_POINT('Origin',(6.4,0.,0.));
#48216=CARTESIAN_POINT('Origin',(0.4,2.94120067792881,-7.49612156866143));
#48217=CARTESIAN_POINT('',(6.4,2.88478921306664,-7.46176863727189));
#48218=CARTESIAN_POINT('',(0.4,2.88478921306664,-7.46176863727189));
#48219=CARTESIAN_POINT('',(3.25,2.88478921306664,-7.46176863727189));
#48220=CARTESIAN_POINT('',(6.4,2.66775711794021,-7.32960244213009));
#48221=CARTESIAN_POINT('',(6.4,2.94120067792881,-7.49612156866143));
#48222=CARTESIAN_POINT('',(0.4,2.66775711794021,-7.32960244213009));
#48223=CARTESIAN_POINT('',(0.4,2.66775711794021,-7.32960244213009));
#48224=CARTESIAN_POINT('',(0.4,2.94120067792881,-7.49612156866143));
#48225=CARTESIAN_POINT('Origin',(0.4,2.71050963585592,-7.44706401972833));
#48226=CARTESIAN_POINT('',(0.4,2.5864556801467,-7.57035316313822));
#48227=CARTESIAN_POINT('Origin',(0.4,0.,0.));
#48228=CARTESIAN_POINT('',(0.4,2.66775711794021,-7.32960244213009));
#48229=CARTESIAN_POINT('Origin',(0.4,2.66775711794021,-7.32960244213009));
#48230=CARTESIAN_POINT('',(6.4,2.5864556801467,-7.57035316313822));
#48231=CARTESIAN_POINT('',(3.25,2.5864556801467,-7.57035316313822));
#48232=CARTESIAN_POINT('',(6.4,2.66775711794021,-7.32960244213009));
#48233=CARTESIAN_POINT('Origin',(6.4,2.71050963585592,-7.44706401972833));
#48234=CARTESIAN_POINT('Origin',(6.4,0.,0.));
#48235=CARTESIAN_POINT('Origin',(0.4,1.59482938082123,-7.89297277621489));
#48236=CARTESIAN_POINT('',(6.4,1.5452402567995,-7.84934599497093));
#48237=CARTESIAN_POINT('',(0.4,1.5452402567995,-7.84934599497093));
#48238=CARTESIAN_POINT('',(3.25,1.5452402567995,-7.84934599497093));
#48239=CARTESIAN_POINT('',(6.4,1.35445578580205,-7.68150047349522));
#48240=CARTESIAN_POINT('',(6.4,1.59482938082123,-7.89297277621489));
#48241=CARTESIAN_POINT('',(0.4,1.35445578580205,-7.68150047349522));
#48242=CARTESIAN_POINT('',(0.4,1.35445578580205,-7.68150047349522));
#48243=CARTESIAN_POINT('',(0.4,1.59482938082123,-7.89297277621489));
#48244=CARTESIAN_POINT('Origin',(0.4,1.37616180801042,-7.80460144262175));
#48245=CARTESIAN_POINT('',(0.4,1.2325835755569,-7.90447580357277));
#48246=CARTESIAN_POINT('Origin',(0.4,0.,0.));
#48247=CARTESIAN_POINT('',(0.4,1.35445578580205,-7.68150047349522));
#48248=CARTESIAN_POINT('Origin',(0.4,1.35445578580205,-7.68150047349522));
#48249=CARTESIAN_POINT('',(6.4,1.2325835755569,-7.90447580357277));
#48250=CARTESIAN_POINT('',(3.25,1.2325835755569,-7.90447580357277));
#48251=CARTESIAN_POINT('',(6.4,1.35445578580205,-7.68150047349522));
#48252=CARTESIAN_POINT('Origin',(6.4,1.37616180801042,-7.80460144262175));
#48253=CARTESIAN_POINT('Origin',(6.4,0.,0.));
#48254=CARTESIAN_POINT('Origin',(0.4,0.199999999999999,-8.05));
#48255=CARTESIAN_POINT('',(6.4,0.158739957258808,-7.99842494657351));
#48256=CARTESIAN_POINT('',(0.4,0.158739957258808,-7.99842494657351));
#48257=CARTESIAN_POINT('',(3.25,0.158739957258808,-7.99842494657351));
#48258=CARTESIAN_POINT('',(6.4,-1.4328367550024E-15,-7.8));
#48259=CARTESIAN_POINT('',(6.4,0.199999999999999,-8.05));
#48260=CARTESIAN_POINT('',(0.4,-1.4328367550024E-15,-7.8));
#48261=CARTESIAN_POINT('',(0.4,-1.4328367550024E-15,-7.8));
#48262=CARTESIAN_POINT('',(0.4,0.199999999999999,-8.05));
#48263=CARTESIAN_POINT('Origin',(0.4,-1.45579888248642E-15,-7.925));
#48264=CARTESIAN_POINT('',(0.4,-0.158739957258811,-7.99842494657351));
#48265=CARTESIAN_POINT('Origin',(0.4,0.,0.));
#48266=CARTESIAN_POINT('',(0.4,-1.4328367550024E-15,-7.8));
#48267=CARTESIAN_POINT('Origin',(0.4,-1.4328367550024E-15,-7.8));
#48268=CARTESIAN_POINT('',(6.4,-0.158739957258811,-7.99842494657351));
#48269=CARTESIAN_POINT('',(3.25,-0.158739957258811,-7.99842494657351));
#48270=CARTESIAN_POINT('',(6.4,-1.4328367550024E-15,-7.8));
#48271=CARTESIAN_POINT('Origin',(6.4,-1.45579888248642E-15,-7.925));
#48272=CARTESIAN_POINT('Origin',(6.4,0.,0.));
#48273=CARTESIAN_POINT('Origin',(0.4,-1.20090627961635,-7.96243204728166));
#48274=CARTESIAN_POINT('',(6.4,-1.2325835755569,-7.90447580357277));
#48275=CARTESIAN_POINT('',(0.4,-1.2325835755569,-7.90447580357277));
#48276=CARTESIAN_POINT('',(3.25,-1.2325835755569,-7.90447580357277));
#48277=CARTESIAN_POINT('',(6.4,-1.35445578580206,-7.68150047349522));
#48278=CARTESIAN_POINT('',(6.4,-1.20090627961635,-7.96243204728166));
#48279=CARTESIAN_POINT('',(0.4,-1.35445578580206,-7.68150047349522));
#48280=CARTESIAN_POINT('',(0.4,-1.35445578580206,-7.68150047349522));
#48281=CARTESIAN_POINT('',(0.4,-1.20090627961635,-7.96243204728166));
#48282=CARTESIAN_POINT('Origin',(0.4,-1.37616180801042,-7.80460144262175));
#48283=CARTESIAN_POINT('',(0.4,-1.54524025679951,-7.84934599497093));
#48284=CARTESIAN_POINT('Origin',(0.4,0.,0.));
#48285=CARTESIAN_POINT('',(0.4,-1.35445578580206,-7.68150047349522));
#48286=CARTESIAN_POINT('Origin',(0.4,-1.35445578580206,-7.68150047349522));
#48287=CARTESIAN_POINT('',(6.4,-1.54524025679951,-7.84934599497093));
#48288=CARTESIAN_POINT('',(3.25,-1.54524025679951,-7.84934599497093));
#48289=CARTESIAN_POINT('',(6.4,-1.35445578580206,-7.68150047349522));
#48290=CARTESIAN_POINT('Origin',(6.4,-1.37616180801042,-7.80460144262175));
#48291=CARTESIAN_POINT('Origin',(6.4,0.,0.));
#48292=CARTESIAN_POINT('Origin',(0.4,-2.56532362961446,-7.6329296259917));
#48293=CARTESIAN_POINT('',(6.4,-2.58645568014671,-7.57035316313822));
#48294=CARTESIAN_POINT('',(0.4,-2.58645568014671,-7.57035316313822));
#48295=CARTESIAN_POINT('',(3.25,-2.58645568014671,-7.57035316313822));
#48296=CARTESIAN_POINT('',(6.4,-2.66775711794022,-7.32960244213008));
#48297=CARTESIAN_POINT('',(6.4,-2.56532362961446,-7.6329296259917));
#48298=CARTESIAN_POINT('',(0.4,-2.66775711794022,-7.32960244213008));
#48299=CARTESIAN_POINT('',(0.4,-2.66775711794022,-7.32960244213008));
#48300=CARTESIAN_POINT('',(0.4,-2.56532362961446,-7.6329296259917));
#48301=CARTESIAN_POINT('Origin',(0.4,-2.71050963585593,-7.44706401972832));
#48302=CARTESIAN_POINT('',(0.4,-2.88478921306665,-7.46176863727188));
#48303=CARTESIAN_POINT('Origin',(0.4,0.,0.));
#48304=CARTESIAN_POINT('',(0.4,-2.66775711794022,-7.32960244213008));
#48305=CARTESIAN_POINT('Origin',(0.4,-2.66775711794022,-7.32960244213008));
#48306=CARTESIAN_POINT('',(6.4,-2.88478921306665,-7.46176863727188));
#48307=CARTESIAN_POINT('',(3.25,-2.88478921306665,-7.46176863727188));
#48308=CARTESIAN_POINT('',(6.4,-2.66775711794022,-7.32960244213008));
#48309=CARTESIAN_POINT('Origin',(6.4,-2.71050963585593,-7.44706401972832));
#48310=CARTESIAN_POINT('Origin',(6.4,0.,0.));
#48311=CARTESIAN_POINT('Origin',(0.4,-3.85179491924312,-7.07150450046473));
#48312=CARTESIAN_POINT('',(6.4,-3.86173963770497,-7.00620917262526));
#48313=CARTESIAN_POINT('',(0.4,-3.86173963770497,-7.00620917262526));
#48314=CARTESIAN_POINT('',(3.25,-3.86173963770497,-7.00620917262526));
#48315=CARTESIAN_POINT('',(6.4,-3.9,-6.75499814951862));
#48316=CARTESIAN_POINT('',(6.4,-3.85179491924312,-7.07150450046473));
#48317=CARTESIAN_POINT('',(0.4,-3.9,-6.75499814951862));
#48318=CARTESIAN_POINT('',(0.4,-3.9,-6.75499814951862));
#48319=CARTESIAN_POINT('',(0.4,-3.85179491924312,-7.07150450046473));
#48320=CARTESIAN_POINT('Origin',(0.4,-3.9625,-6.86325132499167));
#48321=CARTESIAN_POINT('',(0.4,-4.13668530886854,-6.84746921536645));
#48322=CARTESIAN_POINT('Origin',(0.4,0.,0.));
#48323=CARTESIAN_POINT('',(0.4,-3.9,-6.75499814951862));
#48324=CARTESIAN_POINT('Origin',(0.4,-3.9,-6.75499814951862));
#48325=CARTESIAN_POINT('',(6.4,-4.13668530886854,-6.84746921536645));
#48326=CARTESIAN_POINT('',(3.25,-4.13668530886854,-6.84746921536645));
#48327=CARTESIAN_POINT('',(6.4,-3.9,-6.75499814951862));
#48328=CARTESIAN_POINT('Origin',(6.4,-3.9625,-6.86325132499167));
#48329=CARTESIAN_POINT('Origin',(6.4,0.,0.));
#48330=CARTESIAN_POINT('Origin',(0.4,-5.02123136935285,-6.29521528904508));
#48331=CARTESIAN_POINT('',(6.4,-5.01968659050612,-6.22918506171498));
#48332=CARTESIAN_POINT('',(0.4,-5.01968659050612,-6.22918506171498));
#48333=CARTESIAN_POINT('',(3.25,-5.01968659050612,-6.22918506171498));
#48334=CARTESIAN_POINT('',(6.4,-5.01374335555501,-5.97514665632803));
#48335=CARTESIAN_POINT('',(6.4,-5.02123136935285,-6.29521528904508));
#48336=CARTESIAN_POINT('',(0.4,-5.01374335555501,-5.97514665632803));
#48337=CARTESIAN_POINT('',(0.4,-5.01374335555501,-5.97514665632803));
#48338=CARTESIAN_POINT('',(0.4,-5.02123136935285,-6.29521528904508));
#48339=CARTESIAN_POINT('Origin',(0.4,-5.09409180676582,-6.0709022117179));
#48340=CARTESIAN_POINT('',(0.4,-5.26289031482423,-6.02511290633871));
#48341=CARTESIAN_POINT('Origin',(0.4,0.,0.));
#48342=CARTESIAN_POINT('',(0.4,-5.01374335555501,-5.97514665632803));
#48343=CARTESIAN_POINT('Origin',(0.4,-5.01374335555501,-5.97514665632803));
#48344=CARTESIAN_POINT('',(6.4,-5.26289031482423,-6.02511290633871));
#48345=CARTESIAN_POINT('',(3.25,-5.26289031482423,-6.02511290633871));
#48346=CARTESIAN_POINT('',(6.4,-5.01374335555501,-5.97514665632803));
#48347=CARTESIAN_POINT('Origin',(6.4,-5.09409180676582,-6.0709022117179));
#48348=CARTESIAN_POINT('Origin',(6.4,0.,0.));
#48349=CARTESIAN_POINT('Origin',(0.4,-6.03810024517047,-5.32764914660044));
#48350=CARTESIAN_POINT('',(6.4,-6.02511290633871,-5.26289031482423));
#48351=CARTESIAN_POINT('',(0.4,-6.02511290633871,-5.26289031482423));
#48352=CARTESIAN_POINT('',(3.25,-6.02511290633871,-5.26289031482423));
#48353=CARTESIAN_POINT('',(6.4,-5.97514665632803,-5.01374335555501));
#48354=CARTESIAN_POINT('',(6.4,-6.03810024517047,-5.32764914660044));
#48355=CARTESIAN_POINT('',(0.4,-5.97514665632803,-5.01374335555501));
#48356=CARTESIAN_POINT('',(0.4,-5.97514665632803,-5.01374335555501));
#48357=CARTESIAN_POINT('',(0.4,-6.03810024517047,-5.32764914660044));
#48358=CARTESIAN_POINT('Origin',(0.4,-6.0709022117179,-5.09409180676582));
#48359=CARTESIAN_POINT('',(0.4,-6.22918506171498,-5.01968659050612));
#48360=CARTESIAN_POINT('Origin',(0.4,0.,0.));
#48361=CARTESIAN_POINT('',(0.4,-5.97514665632803,-5.01374335555501));
#48362=CARTESIAN_POINT('Origin',(0.4,-5.97514665632803,-5.01374335555501));
#48363=CARTESIAN_POINT('',(6.4,-6.22918506171498,-5.01968659050612));
#48364=CARTESIAN_POINT('',(3.25,-6.22918506171498,-5.01968659050612));
#48365=CARTESIAN_POINT('',(6.4,-5.97514665632803,-5.01374335555501));
#48366=CARTESIAN_POINT('Origin',(6.4,-6.0709022117179,-5.09409180676582));
#48367=CARTESIAN_POINT('Origin',(6.4,0.,0.));
#48368=CARTESIAN_POINT('Origin',(0.4,-6.87150450046473,-4.19820508075689));
#48369=CARTESIAN_POINT('',(6.4,-6.84746921536645,-4.13668530886854));
#48370=CARTESIAN_POINT('',(0.4,-6.84746921536645,-4.13668530886854));
#48371=CARTESIAN_POINT('',(3.25,-6.84746921536645,-4.13668530886854));
#48372=CARTESIAN_POINT('',(6.4,-6.75499814951862,-3.9));
#48373=CARTESIAN_POINT('',(6.4,-6.87150450046473,-4.19820508075689));
#48374=CARTESIAN_POINT('',(0.4,-6.75499814951862,-3.9));
#48375=CARTESIAN_POINT('',(0.4,-6.75499814951862,-3.9));
#48376=CARTESIAN_POINT('',(0.4,-6.87150450046473,-4.19820508075689));
#48377=CARTESIAN_POINT('Origin',(0.4,-6.86325132499168,-3.9625));
#48378=CARTESIAN_POINT('',(0.4,-7.00620917262526,-3.86173963770497));
#48379=CARTESIAN_POINT('Origin',(0.4,0.,0.));
#48380=CARTESIAN_POINT('',(0.4,-6.75499814951862,-3.9));
#48381=CARTESIAN_POINT('Origin',(0.4,-6.75499814951862,-3.9));
#48382=CARTESIAN_POINT('',(6.4,-7.00620917262526,-3.86173963770497));
#48383=CARTESIAN_POINT('',(3.25,-7.00620917262526,-3.86173963770497));
#48384=CARTESIAN_POINT('',(6.4,-6.75499814951862,-3.9));
#48385=CARTESIAN_POINT('Origin',(6.4,-6.86325132499168,-3.9625));
#48386=CARTESIAN_POINT('Origin',(6.4,0.,0.));
#48387=CARTESIAN_POINT('Origin',(0.4,-7.49612156866143,-2.94120067792881));
#48388=CARTESIAN_POINT('',(6.4,-7.46176863727189,-2.88478921306665));
#48389=CARTESIAN_POINT('',(0.4,-7.46176863727189,-2.88478921306665));
#48390=CARTESIAN_POINT('',(3.25,-7.46176863727188,-2.88478921306665));
#48391=CARTESIAN_POINT('',(6.4,-7.32960244213009,-2.66775711794022));
#48392=CARTESIAN_POINT('',(6.4,-7.49612156866143,-2.94120067792881));
#48393=CARTESIAN_POINT('',(0.4,-7.32960244213009,-2.66775711794022));
#48394=CARTESIAN_POINT('',(0.4,-7.32960244213009,-2.66775711794022));
#48395=CARTESIAN_POINT('',(0.4,-7.49612156866143,-2.94120067792881));
#48396=CARTESIAN_POINT('Origin',(0.4,-7.44706401972832,-2.71050963585592));
#48397=CARTESIAN_POINT('',(0.4,-7.57035316313822,-2.5864556801467));
#48398=CARTESIAN_POINT('Origin',(0.4,0.,0.));
#48399=CARTESIAN_POINT('',(0.4,-7.32960244213009,-2.66775711794022));
#48400=CARTESIAN_POINT('Origin',(0.4,-7.32960244213009,-2.66775711794022));
#48401=CARTESIAN_POINT('',(6.4,-7.57035316313822,-2.5864556801467));
#48402=CARTESIAN_POINT('',(3.25,-7.57035316313822,-2.5864556801467));
#48403=CARTESIAN_POINT('',(6.4,-7.32960244213009,-2.66775711794022));
#48404=CARTESIAN_POINT('Origin',(6.4,-7.44706401972832,-2.71050963585592));
#48405=CARTESIAN_POINT('Origin',(6.4,0.,0.));
#48406=CARTESIAN_POINT('Origin',(0.4,-7.89297277621489,-1.59482938082123));
#48407=CARTESIAN_POINT('',(6.4,-7.84934599497093,-1.5452402567995));
#48408=CARTESIAN_POINT('',(0.4,-7.84934599497093,-1.5452402567995));
#48409=CARTESIAN_POINT('',(3.25,-7.84934599497093,-1.5452402567995));
#48410=CARTESIAN_POINT('',(6.4,-7.68150047349522,-1.35445578580205));
#48411=CARTESIAN_POINT('',(6.4,-7.89297277621489,-1.59482938082123));
#48412=CARTESIAN_POINT('',(0.4,-7.68150047349522,-1.35445578580205));
#48413=CARTESIAN_POINT('',(0.4,-7.68150047349522,-1.35445578580205));
#48414=CARTESIAN_POINT('',(0.4,-7.89297277621489,-1.59482938082123));
#48415=CARTESIAN_POINT('Origin',(0.4,-7.80460144262175,-1.37616180801042));
#48416=CARTESIAN_POINT('',(0.4,-7.90447580357277,-1.2325835755569));
#48417=CARTESIAN_POINT('Origin',(0.4,0.,0.));
#48418=CARTESIAN_POINT('',(0.4,-7.68150047349522,-1.35445578580205));
#48419=CARTESIAN_POINT('Origin',(0.4,-7.68150047349522,-1.35445578580205));
#48420=CARTESIAN_POINT('',(6.4,-7.90447580357277,-1.2325835755569));
#48421=CARTESIAN_POINT('',(3.25,-7.90447580357277,-1.2325835755569));
#48422=CARTESIAN_POINT('',(6.4,-7.68150047349522,-1.35445578580205));
#48423=CARTESIAN_POINT('Origin',(6.4,-7.80460144262175,-1.37616180801042));
#48424=CARTESIAN_POINT('Origin',(6.4,0.,0.));
#48425=CARTESIAN_POINT('Origin',(0.4,-8.05,-0.199999999999999));
#48426=CARTESIAN_POINT('',(6.4,-7.99842494657351,-0.158739957258808));
#48427=CARTESIAN_POINT('',(0.4,-7.99842494657351,-0.158739957258808));
#48428=CARTESIAN_POINT('',(3.25,-7.99842494657351,-0.158739957258808));
#48429=CARTESIAN_POINT('',(6.4,-7.8,9.55224503334935E-16));
#48430=CARTESIAN_POINT('',(6.4,-8.05,-0.199999999999999));
#48431=CARTESIAN_POINT('',(0.4,-7.8,9.55224503334935E-16));
#48432=CARTESIAN_POINT('',(0.4,-7.8,9.55224503334935E-16));
#48433=CARTESIAN_POINT('',(0.4,-8.05,-0.199999999999999));
#48434=CARTESIAN_POINT('Origin',(0.4,-7.925,9.70532588324277E-16));
#48435=CARTESIAN_POINT('',(0.4,-8.,-9.79717439317883E-16));
#48436=CARTESIAN_POINT('Origin',(0.4,0.,0.));
#48437=CARTESIAN_POINT('',(0.4,-7.99842494657351,0.15873995725881));
#48438=CARTESIAN_POINT('',(0.4,-7.8,9.55224503334935E-16));
#48439=CARTESIAN_POINT('Origin',(0.4,0.,0.));
#48440=CARTESIAN_POINT('Origin',(0.4,-7.8,9.55224503334935E-16));
#48441=CARTESIAN_POINT('',(6.4,-7.99842494657351,0.15873995725881));
#48442=CARTESIAN_POINT('',(3.25,-7.99842494657351,0.15873995725881));
#48443=CARTESIAN_POINT('',(6.4,-7.8,9.55224503334935E-16));
#48444=CARTESIAN_POINT('Origin',(6.4,-7.925,9.70532588324277E-16));
#48445=CARTESIAN_POINT('',(6.4,-8.,-9.79717439317883E-16));
#48446=CARTESIAN_POINT('Origin',(6.4,0.,0.));
#48447=CARTESIAN_POINT('Origin',(6.4,0.,0.));
#48448=CARTESIAN_POINT('Origin',(0.4,-7.96243204728166,1.20090627961635));
#48449=CARTESIAN_POINT('',(6.4,-7.90447580357277,1.23258357555691));
#48450=CARTESIAN_POINT('',(0.4,-7.90447580357277,1.23258357555691));
#48451=CARTESIAN_POINT('',(3.25,-7.90447580357277,1.23258357555691));
#48452=CARTESIAN_POINT('',(6.4,-7.68150047349522,1.35445578580206));
#48453=CARTESIAN_POINT('',(6.4,-7.96243204728166,1.20090627961635));
#48454=CARTESIAN_POINT('',(0.4,-7.68150047349522,1.35445578580206));
#48455=CARTESIAN_POINT('',(0.4,-7.68150047349522,1.35445578580206));
#48456=CARTESIAN_POINT('',(0.4,-7.96243204728166,1.20090627961635));
#48457=CARTESIAN_POINT('Origin',(0.4,-7.80460144262175,1.37616180801043));
#48458=CARTESIAN_POINT('',(0.4,-7.84934599497093,1.54524025679951));
#48459=CARTESIAN_POINT('Origin',(0.4,0.,0.));
#48460=CARTESIAN_POINT('',(0.4,-7.68150047349522,1.35445578580206));
#48461=CARTESIAN_POINT('Origin',(0.4,-7.68150047349522,1.35445578580206));
#48462=CARTESIAN_POINT('',(6.4,-7.84934599497093,1.54524025679951));
#48463=CARTESIAN_POINT('',(3.25,-7.84934599497093,1.54524025679951));
#48464=CARTESIAN_POINT('',(6.4,-7.68150047349522,1.35445578580206));
#48465=CARTESIAN_POINT('Origin',(6.4,-7.80460144262175,1.37616180801043));
#48466=CARTESIAN_POINT('Origin',(6.4,0.,0.));
#48467=CARTESIAN_POINT('Origin',(0.4,-7.6329296259917,2.56532362961445));
#48468=CARTESIAN_POINT('',(6.4,-7.57035316313822,2.58645568014671));
#48469=CARTESIAN_POINT('',(0.4,-7.57035316313822,2.58645568014671));
#48470=CARTESIAN_POINT('',(3.25,-7.57035316313822,2.58645568014671));
#48471=CARTESIAN_POINT('',(6.4,-7.32960244213009,2.66775711794022));
#48472=CARTESIAN_POINT('',(6.4,-7.6329296259917,2.56532362961445));
#48473=CARTESIAN_POINT('',(0.4,-7.32960244213009,2.66775711794022));
#48474=CARTESIAN_POINT('',(0.4,-7.32960244213009,2.66775711794022));
#48475=CARTESIAN_POINT('',(0.4,-7.6329296259917,2.56532362961445));
#48476=CARTESIAN_POINT('Origin',(0.4,-7.44706401972832,2.71050963585593));
#48477=CARTESIAN_POINT('',(0.4,-7.46176863727188,2.88478921306665));
#48478=CARTESIAN_POINT('Origin',(0.4,0.,0.));
#48479=CARTESIAN_POINT('',(0.4,-7.32960244213009,2.66775711794022));
#48480=CARTESIAN_POINT('Origin',(0.4,-7.32960244213009,2.66775711794022));
#48481=CARTESIAN_POINT('',(6.4,-7.46176863727188,2.88478921306665));
#48482=CARTESIAN_POINT('',(3.25,-7.46176863727188,2.88478921306665));
#48483=CARTESIAN_POINT('',(6.4,-7.32960244213009,2.66775711794022));
#48484=CARTESIAN_POINT('Origin',(6.4,-7.44706401972832,2.71050963585593));
#48485=CARTESIAN_POINT('Origin',(6.4,0.,0.));
#48486=CARTESIAN_POINT('Origin',(0.4,-7.07150450046473,3.85179491924311));
#48487=CARTESIAN_POINT('',(6.4,-7.00620917262526,3.86173963770497));
#48488=CARTESIAN_POINT('',(0.4,-7.00620917262526,3.86173963770497));
#48489=CARTESIAN_POINT('',(3.25,-7.00620917262526,3.86173963770497));
#48490=CARTESIAN_POINT('',(6.4,-6.75499814951862,3.9));
#48491=CARTESIAN_POINT('',(6.4,-7.07150450046473,3.85179491924311));
#48492=CARTESIAN_POINT('',(0.4,-6.75499814951862,3.9));
#48493=CARTESIAN_POINT('',(0.4,-6.75499814951862,3.9));
#48494=CARTESIAN_POINT('',(0.4,-7.07150450046473,3.85179491924311));
#48495=CARTESIAN_POINT('Origin',(0.4,-6.86325132499168,3.9625));
#48496=CARTESIAN_POINT('',(0.4,-6.84746921536645,4.13668530886854));
#48497=CARTESIAN_POINT('Origin',(0.4,0.,0.));
#48498=CARTESIAN_POINT('',(0.4,-6.75499814951862,3.9));
#48499=CARTESIAN_POINT('Origin',(0.4,-6.75499814951862,3.9));
#48500=CARTESIAN_POINT('',(6.4,-6.84746921536645,4.13668530886854));
#48501=CARTESIAN_POINT('',(3.25,-6.84746921536645,4.13668530886854));
#48502=CARTESIAN_POINT('',(6.4,-6.75499814951862,3.9));
#48503=CARTESIAN_POINT('Origin',(6.4,-6.86325132499168,3.9625));
#48504=CARTESIAN_POINT('Origin',(6.4,0.,0.));
#48505=CARTESIAN_POINT('Origin',(0.4,-6.29521528904508,5.02123136935285));
#48506=CARTESIAN_POINT('',(6.4,-6.22918506171498,5.01968659050612));
#48507=CARTESIAN_POINT('',(0.4,-6.22918506171498,5.01968659050612));
#48508=CARTESIAN_POINT('',(3.25,-6.22918506171498,5.01968659050612));
#48509=CARTESIAN_POINT('',(6.4,-5.97514665632803,5.01374335555501));
#48510=CARTESIAN_POINT('',(6.4,-6.29521528904508,5.02123136935285));
#48511=CARTESIAN_POINT('',(0.4,-5.97514665632803,5.01374335555501));
#48512=CARTESIAN_POINT('',(0.4,-5.97514665632803,5.01374335555501));
#48513=CARTESIAN_POINT('',(0.4,-6.29521528904508,5.02123136935285));
#48514=CARTESIAN_POINT('Origin',(0.4,-6.0709022117179,5.09409180676582));
#48515=CARTESIAN_POINT('',(0.4,-6.02511290633871,5.26289031482423));
#48516=CARTESIAN_POINT('Origin',(0.4,0.,0.));
#48517=CARTESIAN_POINT('',(0.4,-5.97514665632803,5.01374335555501));
#48518=CARTESIAN_POINT('Origin',(0.4,-5.97514665632803,5.01374335555501));
#48519=CARTESIAN_POINT('',(6.4,-6.02511290633871,5.26289031482423));
#48520=CARTESIAN_POINT('',(3.25,-6.02511290633871,5.26289031482423));
#48521=CARTESIAN_POINT('',(6.4,-5.97514665632803,5.01374335555501));
#48522=CARTESIAN_POINT('Origin',(6.4,-6.0709022117179,5.09409180676582));
#48523=CARTESIAN_POINT('Origin',(6.4,0.,0.));
#48524=CARTESIAN_POINT('Origin',(0.4,-5.32764914660044,6.03810024517047));
#48525=CARTESIAN_POINT('',(6.4,-5.26289031482423,6.02511290633871));
#48526=CARTESIAN_POINT('',(0.4,-5.26289031482423,6.02511290633871));
#48527=CARTESIAN_POINT('',(3.25,-5.26289031482423,6.02511290633871));
#48528=CARTESIAN_POINT('',(6.4,-5.01374335555501,5.97514665632803));
#48529=CARTESIAN_POINT('',(6.4,-5.32764914660044,6.03810024517047));
#48530=CARTESIAN_POINT('',(0.4,-5.01374335555501,5.97514665632803));
#48531=CARTESIAN_POINT('',(0.4,-5.01374335555501,5.97514665632803));
#48532=CARTESIAN_POINT('',(0.4,-5.32764914660044,6.03810024517047));
#48533=CARTESIAN_POINT('Origin',(0.4,-5.09409180676582,6.0709022117179));
#48534=CARTESIAN_POINT('',(0.4,-5.01968659050612,6.22918506171498));
#48535=CARTESIAN_POINT('Origin',(0.4,0.,0.));
#48536=CARTESIAN_POINT('',(0.4,-5.01374335555501,5.97514665632803));
#48537=CARTESIAN_POINT('Origin',(0.4,-5.01374335555501,5.97514665632803));
#48538=CARTESIAN_POINT('',(6.4,-5.01968659050612,6.22918506171498));
#48539=CARTESIAN_POINT('',(3.25,-5.01968659050612,6.22918506171498));
#48540=CARTESIAN_POINT('',(6.4,-5.01374335555501,5.97514665632803));
#48541=CARTESIAN_POINT('Origin',(6.4,-5.09409180676582,6.0709022117179));
#48542=CARTESIAN_POINT('Origin',(6.4,0.,0.));
#48543=CARTESIAN_POINT('Origin',(0.4,-4.19820508075689,6.87150450046473));
#48544=CARTESIAN_POINT('',(6.4,-4.13668530886854,6.84746921536645));
#48545=CARTESIAN_POINT('',(0.4,-4.13668530886854,6.84746921536645));
#48546=CARTESIAN_POINT('',(3.25,-4.13668530886854,6.84746921536645));
#48547=CARTESIAN_POINT('',(6.4,-3.9,6.75499814951862));
#48548=CARTESIAN_POINT('',(6.4,-4.19820508075689,6.87150450046473));
#48549=CARTESIAN_POINT('',(0.4,-3.9,6.75499814951862));
#48550=CARTESIAN_POINT('',(0.4,-3.9,6.75499814951862));
#48551=CARTESIAN_POINT('',(0.4,-4.19820508075689,6.87150450046473));
#48552=CARTESIAN_POINT('Origin',(0.4,-3.9625,6.86325132499168));
#48553=CARTESIAN_POINT('',(0.4,-3.86173963770497,7.00620917262526));
#48554=CARTESIAN_POINT('Origin',(0.4,0.,0.));
#48555=CARTESIAN_POINT('',(0.4,-3.9,6.75499814951862));
#48556=CARTESIAN_POINT('Origin',(0.4,-3.9,6.75499814951862));
#48557=CARTESIAN_POINT('',(6.4,-3.86173963770497,7.00620917262526));
#48558=CARTESIAN_POINT('',(3.25,-3.86173963770497,7.00620917262526));
#48559=CARTESIAN_POINT('',(6.4,-3.9,6.75499814951862));
#48560=CARTESIAN_POINT('Origin',(6.4,-3.9625,6.86325132499168));
#48561=CARTESIAN_POINT('Origin',(6.4,0.,0.));
#48562=CARTESIAN_POINT('Origin',(0.4,-2.94120067792882,7.49612156866143));
#48563=CARTESIAN_POINT('',(6.4,-2.88478921306665,7.46176863727188));
#48564=CARTESIAN_POINT('',(0.4,-2.88478921306665,7.46176863727188));
#48565=CARTESIAN_POINT('',(3.25,-2.88478921306665,7.46176863727188));
#48566=CARTESIAN_POINT('',(6.4,-2.66775711794022,7.32960244213009));
#48567=CARTESIAN_POINT('',(6.4,-2.94120067792882,7.49612156866143));
#48568=CARTESIAN_POINT('',(0.4,-2.66775711794022,7.32960244213009));
#48569=CARTESIAN_POINT('',(0.4,-2.66775711794022,7.32960244213009));
#48570=CARTESIAN_POINT('',(0.4,-2.94120067792882,7.49612156866143));
#48571=CARTESIAN_POINT('Origin',(0.4,-2.71050963585592,7.44706401972832));
#48572=CARTESIAN_POINT('',(0.4,-2.5864556801467,7.57035316313822));
#48573=CARTESIAN_POINT('Origin',(0.4,0.,0.));
#48574=CARTESIAN_POINT('',(0.4,-2.66775711794022,7.32960244213009));
#48575=CARTESIAN_POINT('Origin',(0.4,-2.66775711794022,7.32960244213009));
#48576=CARTESIAN_POINT('',(6.4,-2.5864556801467,7.57035316313822));
#48577=CARTESIAN_POINT('',(3.25,-2.5864556801467,7.57035316313822));
#48578=CARTESIAN_POINT('',(6.4,-2.66775711794022,7.32960244213009));
#48579=CARTESIAN_POINT('Origin',(6.4,-2.71050963585592,7.44706401972832));
#48580=CARTESIAN_POINT('Origin',(6.4,0.,0.));
#48581=CARTESIAN_POINT('Origin',(0.4,-1.59482938082123,7.89297277621489));
#48582=CARTESIAN_POINT('',(6.4,-1.5452402567995,7.84934599497093));
#48583=CARTESIAN_POINT('',(0.4,-1.5452402567995,7.84934599497093));
#48584=CARTESIAN_POINT('',(3.25,-1.5452402567995,7.84934599497093));
#48585=CARTESIAN_POINT('',(6.4,-1.35445578580206,7.68150047349522));
#48586=CARTESIAN_POINT('',(6.4,-1.59482938082123,7.89297277621489));
#48587=CARTESIAN_POINT('',(0.4,-1.35445578580206,7.68150047349522));
#48588=CARTESIAN_POINT('',(0.4,-1.35445578580206,7.68150047349522));
#48589=CARTESIAN_POINT('',(0.4,-1.59482938082123,7.89297277621489));
#48590=CARTESIAN_POINT('Origin',(0.4,-1.37616180801042,7.80460144262175));
#48591=CARTESIAN_POINT('',(0.4,-1.2325835755569,7.90447580357277));
#48592=CARTESIAN_POINT('Origin',(0.4,0.,0.));
#48593=CARTESIAN_POINT('',(0.4,-1.35445578580206,7.68150047349522));
#48594=CARTESIAN_POINT('Origin',(0.4,-1.35445578580206,7.68150047349522));
#48595=CARTESIAN_POINT('',(6.4,-1.2325835755569,7.90447580357277));
#48596=CARTESIAN_POINT('',(3.25,-1.2325835755569,7.90447580357277));
#48597=CARTESIAN_POINT('',(6.4,-1.35445578580206,7.68150047349522));
#48598=CARTESIAN_POINT('Origin',(6.4,-1.37616180801042,7.80460144262175));
#48599=CARTESIAN_POINT('Origin',(6.4,0.,0.));
#48600=CARTESIAN_POINT('Origin',(0.4,-0.2,8.05));
#48601=CARTESIAN_POINT('',(6.4,-0.158739957258808,7.99842494657351));
#48602=CARTESIAN_POINT('',(0.4,-0.158739957258808,7.99842494657351));
#48603=CARTESIAN_POINT('',(3.25,-0.158739957258808,7.99842494657351));
#48604=CARTESIAN_POINT('',(6.4,4.77612251667468E-16,7.8));
#48605=CARTESIAN_POINT('',(6.4,-0.2,8.05));
#48606=CARTESIAN_POINT('',(0.4,4.77612251667468E-16,7.8));
#48607=CARTESIAN_POINT('',(0.4,4.77612251667468E-16,7.8));
#48608=CARTESIAN_POINT('',(0.4,-0.2,8.05));
#48609=CARTESIAN_POINT('Origin',(0.4,4.85266294162139E-16,7.925));
#48610=CARTESIAN_POINT('',(0.4,0.158739957258811,7.99842494657351));
#48611=CARTESIAN_POINT('Origin',(0.4,0.,0.));
#48612=CARTESIAN_POINT('',(0.4,4.77612251667468E-16,7.8));
#48613=CARTESIAN_POINT('Origin',(0.4,4.77612251667468E-16,7.8));
#48614=CARTESIAN_POINT('',(6.4,0.158739957258811,7.99842494657351));
#48615=CARTESIAN_POINT('',(3.25,0.158739957258811,7.99842494657351));
#48616=CARTESIAN_POINT('',(6.4,4.77612251667468E-16,7.8));
#48617=CARTESIAN_POINT('Origin',(6.4,4.85266294162139E-16,7.925));
#48618=CARTESIAN_POINT('Origin',(6.4,0.,0.));
#48619=CARTESIAN_POINT('Origin',(0.4,1.20090627961635,7.96243204728166));
#48620=CARTESIAN_POINT('',(6.4,1.2325835755569,7.90447580357277));
#48621=CARTESIAN_POINT('',(0.4,1.2325835755569,7.90447580357277));
#48622=CARTESIAN_POINT('',(3.25,1.2325835755569,7.90447580357277));
#48623=CARTESIAN_POINT('',(6.4,1.35445578580206,7.68150047349522));
#48624=CARTESIAN_POINT('',(6.4,1.20090627961635,7.96243204728166));
#48625=CARTESIAN_POINT('',(0.4,1.35445578580206,7.68150047349522));
#48626=CARTESIAN_POINT('',(0.4,1.35445578580206,7.68150047349522));
#48627=CARTESIAN_POINT('',(0.4,1.20090627961635,7.96243204728166));
#48628=CARTESIAN_POINT('Origin',(0.4,1.37616180801042,7.80460144262175));
#48629=CARTESIAN_POINT('',(0.4,1.54524025679951,7.84934599497093));
#48630=CARTESIAN_POINT('Origin',(0.4,0.,0.));
#48631=CARTESIAN_POINT('',(0.4,1.35445578580206,7.68150047349522));
#48632=CARTESIAN_POINT('Origin',(0.4,1.35445578580206,7.68150047349522));
#48633=CARTESIAN_POINT('',(6.4,1.54524025679951,7.84934599497093));
#48634=CARTESIAN_POINT('',(3.25,1.54524025679951,7.84934599497093));
#48635=CARTESIAN_POINT('',(6.4,1.35445578580206,7.68150047349522));
#48636=CARTESIAN_POINT('Origin',(6.4,1.37616180801042,7.80460144262175));
#48637=CARTESIAN_POINT('Origin',(6.4,0.,0.));
#48638=CARTESIAN_POINT('Origin',(0.4,2.56532362961445,7.6329296259917));
#48639=CARTESIAN_POINT('',(6.4,2.5864556801467,7.57035316313822));
#48640=CARTESIAN_POINT('',(0.4,2.5864556801467,7.57035316313822));
#48641=CARTESIAN_POINT('',(3.25,2.5864556801467,7.57035316313822));
#48642=CARTESIAN_POINT('',(6.4,2.66775711794022,7.32960244213009));
#48643=CARTESIAN_POINT('',(6.4,2.56532362961445,7.6329296259917));
#48644=CARTESIAN_POINT('',(0.4,2.66775711794022,7.32960244213009));
#48645=CARTESIAN_POINT('',(0.4,2.66775711794022,7.32960244213009));
#48646=CARTESIAN_POINT('',(0.4,2.56532362961445,7.6329296259917));
#48647=CARTESIAN_POINT('Origin',(0.4,2.71050963585593,7.44706401972832));
#48648=CARTESIAN_POINT('',(0.4,2.88478921306665,7.46176863727188));
#48649=CARTESIAN_POINT('Origin',(0.4,0.,0.));
#48650=CARTESIAN_POINT('',(0.4,2.66775711794022,7.32960244213009));
#48651=CARTESIAN_POINT('Origin',(0.4,2.66775711794022,7.32960244213009));
#48652=CARTESIAN_POINT('',(6.4,2.88478921306665,7.46176863727188));
#48653=CARTESIAN_POINT('',(3.25,2.88478921306665,7.46176863727188));
#48654=CARTESIAN_POINT('',(6.4,2.66775711794022,7.32960244213009));
#48655=CARTESIAN_POINT('Origin',(6.4,2.71050963585593,7.44706401972832));
#48656=CARTESIAN_POINT('Origin',(6.4,0.,0.));
#48657=CARTESIAN_POINT('Origin',(0.4,3.85179491924311,7.07150450046473));
#48658=CARTESIAN_POINT('',(6.4,3.86173963770497,7.00620917262526));
#48659=CARTESIAN_POINT('',(0.4,3.86173963770497,7.00620917262526));
#48660=CARTESIAN_POINT('',(3.25,3.86173963770497,7.00620917262526));
#48661=CARTESIAN_POINT('',(6.4,3.9,6.75499814951862));
#48662=CARTESIAN_POINT('',(6.4,3.85179491924311,7.07150450046473));
#48663=CARTESIAN_POINT('',(0.4,3.9,6.75499814951862));
#48664=CARTESIAN_POINT('',(0.4,3.9,6.75499814951862));
#48665=CARTESIAN_POINT('',(0.4,3.85179491924311,7.07150450046473));
#48666=CARTESIAN_POINT('Origin',(0.4,3.9625,6.86325132499168));
#48667=CARTESIAN_POINT('',(0.4,4.13668530886854,6.84746921536645));
#48668=CARTESIAN_POINT('Origin',(0.4,0.,0.));
#48669=CARTESIAN_POINT('',(0.4,3.9,6.75499814951862));
#48670=CARTESIAN_POINT('Origin',(0.4,3.9,6.75499814951862));
#48671=CARTESIAN_POINT('',(6.4,4.13668530886854,6.84746921536645));
#48672=CARTESIAN_POINT('',(3.25,4.13668530886854,6.84746921536645));
#48673=CARTESIAN_POINT('',(6.4,3.9,6.75499814951862));
#48674=CARTESIAN_POINT('Origin',(6.4,3.9625,6.86325132499168));
#48675=CARTESIAN_POINT('Origin',(6.4,0.,0.));
#48676=CARTESIAN_POINT('Origin',(0.4,5.02123136935285,6.29521528904508));
#48677=CARTESIAN_POINT('',(6.4,5.01968659050612,6.22918506171498));
#48678=CARTESIAN_POINT('',(0.4,5.01968659050612,6.22918506171498));
#48679=CARTESIAN_POINT('',(3.25,5.01968659050612,6.22918506171498));
#48680=CARTESIAN_POINT('',(6.4,5.01374335555501,5.97514665632803));
#48681=CARTESIAN_POINT('',(6.4,5.02123136935285,6.29521528904508));
#48682=CARTESIAN_POINT('',(0.4,5.01374335555501,5.97514665632803));
#48683=CARTESIAN_POINT('',(0.4,5.01374335555501,5.97514665632803));
#48684=CARTESIAN_POINT('',(0.4,5.02123136935285,6.29521528904508));
#48685=CARTESIAN_POINT('Origin',(0.4,5.09409180676582,6.0709022117179));
#48686=CARTESIAN_POINT('',(0.4,5.26289031482423,6.02511290633871));
#48687=CARTESIAN_POINT('Origin',(0.4,0.,0.));
#48688=CARTESIAN_POINT('',(0.4,5.01374335555501,5.97514665632803));
#48689=CARTESIAN_POINT('Origin',(0.4,5.01374335555501,5.97514665632803));
#48690=CARTESIAN_POINT('',(6.4,5.26289031482423,6.02511290633871));
#48691=CARTESIAN_POINT('',(3.25,5.26289031482423,6.02511290633871));
#48692=CARTESIAN_POINT('',(6.4,5.01374335555501,5.97514665632803));
#48693=CARTESIAN_POINT('Origin',(6.4,5.09409180676582,6.0709022117179));
#48694=CARTESIAN_POINT('Origin',(6.4,0.,0.));
#48695=CARTESIAN_POINT('Origin',(0.4,6.03810024517047,5.32764914660044));
#48696=CARTESIAN_POINT('',(6.4,6.02511290633871,5.26289031482423));
#48697=CARTESIAN_POINT('',(0.4,6.02511290633871,5.26289031482423));
#48698=CARTESIAN_POINT('',(3.25,6.02511290633871,5.26289031482423));
#48699=CARTESIAN_POINT('',(6.4,5.97514665632803,5.01374335555501));
#48700=CARTESIAN_POINT('',(6.4,6.03810024517047,5.32764914660044));
#48701=CARTESIAN_POINT('',(0.4,5.97514665632803,5.01374335555501));
#48702=CARTESIAN_POINT('',(0.4,5.97514665632803,5.01374335555501));
#48703=CARTESIAN_POINT('',(0.4,6.03810024517047,5.32764914660044));
#48704=CARTESIAN_POINT('Origin',(0.4,6.0709022117179,5.09409180676582));
#48705=CARTESIAN_POINT('',(0.4,6.22918506171498,5.01968659050612));
#48706=CARTESIAN_POINT('Origin',(0.4,0.,0.));
#48707=CARTESIAN_POINT('',(0.4,5.97514665632803,5.01374335555501));
#48708=CARTESIAN_POINT('Origin',(0.4,5.97514665632803,5.01374335555501));
#48709=CARTESIAN_POINT('',(6.4,6.22918506171498,5.01968659050612));
#48710=CARTESIAN_POINT('',(3.25,6.22918506171498,5.01968659050612));
#48711=CARTESIAN_POINT('',(6.4,5.97514665632803,5.01374335555501));
#48712=CARTESIAN_POINT('Origin',(6.4,6.0709022117179,5.09409180676582));
#48713=CARTESIAN_POINT('Origin',(6.4,0.,0.));
#48714=CARTESIAN_POINT('Origin',(0.4,6.87150450046473,4.19820508075689));
#48715=CARTESIAN_POINT('',(6.4,6.84746921536645,4.13668530886854));
#48716=CARTESIAN_POINT('',(0.4,6.84746921536645,4.13668530886854));
#48717=CARTESIAN_POINT('',(3.25,6.84746921536645,4.13668530886854));
#48718=CARTESIAN_POINT('',(6.4,6.75499814951862,3.9));
#48719=CARTESIAN_POINT('',(6.4,6.87150450046473,4.19820508075689));
#48720=CARTESIAN_POINT('',(0.4,6.75499814951862,3.9));
#48721=CARTESIAN_POINT('',(0.4,6.75499814951862,3.9));
#48722=CARTESIAN_POINT('',(0.4,6.87150450046473,4.19820508075689));
#48723=CARTESIAN_POINT('Origin',(0.4,6.86325132499168,3.9625));
#48724=CARTESIAN_POINT('',(0.4,7.00620917262526,3.86173963770497));
#48725=CARTESIAN_POINT('Origin',(0.4,0.,0.));
#48726=CARTESIAN_POINT('',(0.4,6.75499814951862,3.9));
#48727=CARTESIAN_POINT('Origin',(0.4,6.75499814951862,3.9));
#48728=CARTESIAN_POINT('',(6.4,7.00620917262526,3.86173963770497));
#48729=CARTESIAN_POINT('',(3.25,7.00620917262526,3.86173963770497));
#48730=CARTESIAN_POINT('',(6.4,6.75499814951862,3.9));
#48731=CARTESIAN_POINT('Origin',(6.4,6.86325132499168,3.9625));
#48732=CARTESIAN_POINT('Origin',(6.4,0.,0.));
#48733=CARTESIAN_POINT('Origin',(0.4,7.49612156866143,2.94120067792882));
#48734=CARTESIAN_POINT('',(6.4,7.46176863727188,2.88478921306665));
#48735=CARTESIAN_POINT('',(0.4,7.46176863727188,2.88478921306665));
#48736=CARTESIAN_POINT('',(3.25,7.46176863727188,2.88478921306665));
#48737=CARTESIAN_POINT('',(6.4,7.32960244213009,2.66775711794022));
#48738=CARTESIAN_POINT('',(6.4,7.49612156866143,2.94120067792882));
#48739=CARTESIAN_POINT('',(0.4,7.32960244213009,2.66775711794022));
#48740=CARTESIAN_POINT('',(0.4,7.32960244213009,2.66775711794022));
#48741=CARTESIAN_POINT('',(0.4,7.49612156866143,2.94120067792882));
#48742=CARTESIAN_POINT('Origin',(0.4,7.44706401972832,2.71050963585592));
#48743=CARTESIAN_POINT('',(0.4,7.57035316313822,2.5864556801467));
#48744=CARTESIAN_POINT('Origin',(0.4,0.,0.));
#48745=CARTESIAN_POINT('',(0.4,7.32960244213009,2.66775711794022));
#48746=CARTESIAN_POINT('Origin',(0.4,7.32960244213009,2.66775711794022));
#48747=CARTESIAN_POINT('',(6.4,7.57035316313822,2.5864556801467));
#48748=CARTESIAN_POINT('',(3.25,7.57035316313822,2.5864556801467));
#48749=CARTESIAN_POINT('',(6.4,7.32960244213009,2.66775711794022));
#48750=CARTESIAN_POINT('Origin',(6.4,7.44706401972832,2.71050963585592));
#48751=CARTESIAN_POINT('Origin',(6.4,0.,0.));
#48752=CARTESIAN_POINT('Origin',(0.4,7.89297277621489,1.59482938082123));
#48753=CARTESIAN_POINT('',(6.4,7.84934599497093,1.5452402567995));
#48754=CARTESIAN_POINT('',(0.4,7.84934599497093,1.5452402567995));
#48755=CARTESIAN_POINT('',(3.25,7.84934599497093,1.5452402567995));
#48756=CARTESIAN_POINT('',(6.4,7.68150047349522,1.35445578580206));
#48757=CARTESIAN_POINT('',(6.4,7.89297277621489,1.59482938082123));
#48758=CARTESIAN_POINT('',(0.4,7.68150047349522,1.35445578580206));
#48759=CARTESIAN_POINT('',(0.4,7.68150047349522,1.35445578580206));
#48760=CARTESIAN_POINT('',(0.4,7.89297277621489,1.59482938082123));
#48761=CARTESIAN_POINT('Origin',(0.4,7.80460144262175,1.37616180801042));
#48762=CARTESIAN_POINT('',(0.4,7.90447580357277,1.2325835755569));
#48763=CARTESIAN_POINT('Origin',(0.4,0.,0.));
#48764=CARTESIAN_POINT('',(0.4,7.68150047349522,1.35445578580206));
#48765=CARTESIAN_POINT('Origin',(0.4,7.68150047349522,1.35445578580206));
#48766=CARTESIAN_POINT('',(6.4,7.90447580357277,1.2325835755569));
#48767=CARTESIAN_POINT('',(3.25,7.90447580357277,1.2325835755569));
#48768=CARTESIAN_POINT('',(6.4,7.68150047349522,1.35445578580206));
#48769=CARTESIAN_POINT('Origin',(6.4,7.80460144262175,1.37616180801042));
#48770=CARTESIAN_POINT('Origin',(6.4,0.,0.));
#48771=CARTESIAN_POINT('Origin',(0.4,8.05,0.2));
#48772=CARTESIAN_POINT('',(6.4,7.99842494657351,0.158739957258809));
#48773=CARTESIAN_POINT('',(0.4,7.99842494657351,0.158739957258809));
#48774=CARTESIAN_POINT('',(3.25,7.99842494657351,0.158739957258809));
#48775=CARTESIAN_POINT('',(6.4,7.8,0.));
#48776=CARTESIAN_POINT('',(6.4,8.05,0.2));
#48777=CARTESIAN_POINT('',(0.4,7.8,0.));
#48778=CARTESIAN_POINT('',(0.4,7.8,0.));
#48779=CARTESIAN_POINT('',(0.4,8.05,0.2));
#48780=CARTESIAN_POINT('Origin',(0.4,7.925,0.));
#48781=CARTESIAN_POINT('',(0.4,7.99842494657351,-0.158739957258809));
#48782=CARTESIAN_POINT('Origin',(0.4,0.,0.));
#48783=CARTESIAN_POINT('',(0.4,7.8,0.));
#48784=CARTESIAN_POINT('Origin',(0.4,7.8,0.));
#48785=CARTESIAN_POINT('',(6.4,7.99842494657351,-0.158739957258809));
#48786=CARTESIAN_POINT('',(3.25,7.99842494657351,-0.158739957258809));
#48787=CARTESIAN_POINT('',(6.4,7.8,0.));
#48788=CARTESIAN_POINT('Origin',(6.4,7.925,0.));
#48789=CARTESIAN_POINT('Origin',(6.4,0.,0.));
#48790=CARTESIAN_POINT('Origin',(1.75392422621555,0.,0.));
#48791=CARTESIAN_POINT('',(0.997848452431099,0.,0.));
#48792=CARTESIAN_POINT('',(2.5,-2.48346726553949,3.04137023753017E-16));
#48793=CARTESIAN_POINT('',(1.75392422621555,-1.25,-1.53080849893419E-16));
#48794=CARTESIAN_POINT('Origin',(2.5,0.,0.));
#48795=CARTESIAN_POINT('Origin',(7.,0.,2.88675134594813));
#48796=CARTESIAN_POINT('',(7.,1.76762539787484E-16,2.88675134594813));
#48797=CARTESIAN_POINT('',(7.,2.5,1.44337567297406));
#48798=CARTESIAN_POINT('',(7.,0.625,2.52590742770461));
#48799=CARTESIAN_POINT('',(2.5,2.77555756156289E-16,2.88675134594813));
#48800=CARTESIAN_POINT('',(7.,1.76762539787484E-16,2.88675134594813));
#48801=CARTESIAN_POINT('',(2.5,2.5,1.44337567297406));
#48802=CARTESIAN_POINT('',(2.5,2.5,1.44337567297406));
#48803=CARTESIAN_POINT('',(7.,2.5,1.44337567297406));
#48804=CARTESIAN_POINT('Origin',(7.,-2.5,1.44337567297406));
#48805=CARTESIAN_POINT('',(7.,-2.5,1.44337567297406));
#48806=CARTESIAN_POINT('',(7.,-1.875,1.80421959121758));
#48807=CARTESIAN_POINT('',(2.5,-2.5,1.44337567297406));
#48808=CARTESIAN_POINT('',(7.,-2.5,1.44337567297406));
#48809=CARTESIAN_POINT('',(2.5,1.76762539787484E-16,2.88675134594813));
#48810=CARTESIAN_POINT('Origin',(7.,-2.5,-1.44337567297406));
#48811=CARTESIAN_POINT('',(7.,-2.5,-1.44337567297406));
#48812=CARTESIAN_POINT('',(7.,-2.5,-0.721687836487033));
#48813=CARTESIAN_POINT('',(2.5,-2.5,-1.44337567297406));
#48814=CARTESIAN_POINT('',(7.,-2.5,-1.44337567297406));
#48815=CARTESIAN_POINT('',(2.5,-2.5,1.44337567297406));
#48816=CARTESIAN_POINT('Origin',(7.,-5.55111512312578E-16,-2.88675134594813));
#48817=CARTESIAN_POINT('',(7.,-5.30287619362453E-16,-2.88675134594813));
#48818=CARTESIAN_POINT('',(7.,-0.625000000000001,-2.52590742770461));
#48819=CARTESIAN_POINT('',(2.5,-5.55111512312578E-16,-2.88675134594813));
#48820=CARTESIAN_POINT('',(7.,-5.30287619362453E-16,-2.88675134594813));
#48821=CARTESIAN_POINT('',(2.5,-2.5,-1.44337567297406));
#48822=CARTESIAN_POINT('Origin',(7.,2.5,-1.44337567297407));
#48823=CARTESIAN_POINT('',(7.,2.5,-1.44337567297407));
#48824=CARTESIAN_POINT('',(7.,1.875,-1.80421959121758));
#48825=CARTESIAN_POINT('',(2.5,2.5,-1.44337567297407));
#48826=CARTESIAN_POINT('',(7.,2.5,-1.44337567297407));
#48827=CARTESIAN_POINT('',(2.5,-5.30287619362453E-16,-2.88675134594813));
#48828=CARTESIAN_POINT('Origin',(7.,2.5,1.44337567297406));
#48829=CARTESIAN_POINT('',(7.,2.5,0.721687836487032));
#48830=CARTESIAN_POINT('',(2.5,2.5,-1.44337567297407));
#48831=CARTESIAN_POINT('Origin',(2.5,0.,0.));
#48832=CARTESIAN_POINT('Origin',(-0.4,0.,0.));
#48833=CARTESIAN_POINT('',(-0.4,-5.,-6.12323399573677E-16));
#48834=CARTESIAN_POINT('',(-0.4,-6.12323399573677E-16,5.));
#48835=CARTESIAN_POINT('Origin',(-0.4,0.,0.));
#48836=CARTESIAN_POINT('',(0.,-6.61309271539571E-16,5.4));
#48837=CARTESIAN_POINT('Origin',(-0.4,-6.61309271539571E-16,5.4));
#48838=CARTESIAN_POINT('Origin',(0.,0.,0.));
#48839=CARTESIAN_POINT('Origin',(-0.4,0.,0.));
#48840=CARTESIAN_POINT('Origin',(-6.,0.,0.));
#48841=CARTESIAN_POINT('',(-12.,-5.,-6.12323399573677E-16));
#48842=CARTESIAN_POINT('',(-6.,-5.,-6.12323399573677E-16));
#48843=CARTESIAN_POINT('Origin',(-12.,0.,0.));
#48844=CARTESIAN_POINT('Origin',(0.,8.,0.));
#48845=CARTESIAN_POINT('',(0.,-8.,-9.79717439317883E-16));
#48846=CARTESIAN_POINT('Origin',(0.,0.,0.));
#48847=CARTESIAN_POINT('Origin',(-27.,3.2,0.));
#48848=CARTESIAN_POINT('',(-27.,-3.2,-3.91886975727153E-16));
#48849=CARTESIAN_POINT('Origin',(-27.,0.,0.));
#48850=CARTESIAN_POINT('Origin',(-26.6,0.,0.));
#48851=CARTESIAN_POINT('',(-26.6,-3.6,-4.40872847693047E-16));
#48852=CARTESIAN_POINT('Origin',(-20.1,0.,0.));
#48853=CARTESIAN_POINT('Origin',(-13.9553333333333,0.,0.));
#48854=CARTESIAN_POINT('Origin',(-13.75,0.,0.));
#48855=CARTESIAN_POINT('',(-13.5,-3.25,-3.9801020972289E-16));
#48856=CARTESIAN_POINT('Origin',(-13.5,0.,0.));
#48857=CARTESIAN_POINT('',(-13.75,-3.625,-4.43934464690916E-16));
#48858=CARTESIAN_POINT('Origin',(-12.75,0.,0.));
#48859=CARTESIAN_POINT('',(-12.,-3.25,-3.9801020972289E-16));
#48860=CARTESIAN_POINT('Origin',(-12.,0.,0.));
#48861=CARTESIAN_POINT('',(-12.75,-3.25,-3.9801020972289E-16));
#48862=CARTESIAN_POINT('Origin',(-12.,5.,0.));
#48863=CARTESIAN_POINT('Origin',(3.25,0.,0.));
#48864=CARTESIAN_POINT('',(6.5,-8.,-9.79717439317883E-16));
#48865=CARTESIAN_POINT('Origin',(6.5,0.,0.));
#48866=CARTESIAN_POINT('',(3.25,-8.,-9.79717439317883E-16));
#48867=CARTESIAN_POINT('',(3.25,-8.,-9.79717439317883E-16));
#48868=CARTESIAN_POINT('Origin',(6.75,0.,0.));
#48869=CARTESIAN_POINT('',(7.,-7.5,-9.18485099360515E-16));
#48870=CARTESIAN_POINT('Origin',(7.,0.,0.));
#48871=CARTESIAN_POINT('',(6.75,-7.75,-9.49101269339199E-16));
#48872=CARTESIAN_POINT('Origin',(7.,0.,0.));
#48873=CARTESIAN_POINT('',(0.,0.,0.));
#48874=CARTESIAN_POINT('Origin',(0.375,0.,0.));
#48875=CARTESIAN_POINT('',(0.75,-5.25,-6.42939569552361E-16));
#48876=CARTESIAN_POINT('Origin',(0.75,0.,0.));
#48877=CARTESIAN_POINT('',(0.,-5.25,-6.42939569552361E-16));
#48878=CARTESIAN_POINT('',(0.375,-5.25,-6.42939569552361E-16));
#48879=CARTESIAN_POINT('Origin',(0.,0.,0.));
#48880=CARTESIAN_POINT('Origin',(0.,15.,0.));
#48881=CARTESIAN_POINT('',(0.,-15.,-1.83697019872103E-15));
#48882=CARTESIAN_POINT('Origin',(0.,0.,0.));
#48883=CARTESIAN_POINT('Origin',(0.375,0.,0.));
#48884=CARTESIAN_POINT('',(0.75,-15.,-1.83697019872103E-15));
#48885=CARTESIAN_POINT('Origin',(0.75,0.,0.));
#48886=CARTESIAN_POINT('',(0.375,-15.,-1.83697019872103E-15));
#48887=CARTESIAN_POINT('Origin',(0.75,5.25,0.));
#48888=CARTESIAN_POINT('',(0.,0.,0.));
#48889=CARTESIAN_POINT('Origin',(0.,0.,0.));
#48890=CARTESIAN_POINT('',(-4.86031698411606E-16,-5.95217163743925E-32,
7.9375));
#48891=CARTESIAN_POINT('',(-4.86031698411606E-16,-5.95217163743925E-32,
-7.9375));
#48892=CARTESIAN_POINT('Origin',(0.,0.,0.));
#48893=CARTESIAN_POINT('',(0.,0.,0.));
#48894=CARTESIAN_POINT('Origin',(-4.5,4.7,0.));
#48895=CARTESIAN_POINT('',(-4.5,-4.7,-5.75583995599256E-16));
#48896=CARTESIAN_POINT('Origin',(-4.5,0.,0.));
#48897=CARTESIAN_POINT('Origin',(-4.35,0.,0.));
#48898=CARTESIAN_POINT('',(-4.2,-5.,-6.12323399573677E-16));
#48899=CARTESIAN_POINT('Origin',(-4.2,0.,0.));
#48900=CARTESIAN_POINT('',(-4.35,-4.85,-5.93953697586466E-16));
#48901=CARTESIAN_POINT('Origin',(-2.,0.,0.));
#48902=CARTESIAN_POINT('',(0.2,-5.,-6.12323399573677E-16));
#48903=CARTESIAN_POINT('Origin',(0.2,0.,0.));
#48904=CARTESIAN_POINT('',(-2.,-5.,-6.12323399573677E-16));
#48905=CARTESIAN_POINT('Origin',(0.35,0.,0.));
#48906=CARTESIAN_POINT('',(0.5,-4.7,-5.75583995599256E-16));
#48907=CARTESIAN_POINT('Origin',(0.5,0.,0.));
#48908=CARTESIAN_POINT('',(0.35,-4.85,-5.93953697586466E-16));
#48909=CARTESIAN_POINT('Origin',(0.5,0.,0.));
#48910=CARTESIAN_POINT('',(0.,0.,0.));
#48911=CARTESIAN_POINT('Ctrl Pts',(0.819255282401605,4.08201774695168,-0.0164881184408875));
#48912=CARTESIAN_POINT('Ctrl Pts',(0.833647839427758,4.08136951356852,0.332730692506625));
#48913=CARTESIAN_POINT('Ctrl Pts',(0.862424164350343,3.99464878834545,1.01269819378028));
#48914=CARTESIAN_POINT('Ctrl Pts',(0.919954808790661,3.48448113484463,2.29729435781398));
#48915=CARTESIAN_POINT('Ctrl Pts',(0.991725652203481,2.27056227452172,3.58372650506595));
#48916=CARTESIAN_POINT('Ctrl Pts',(1.07769113094686,0.253097459046851,4.2251855373779));
#48917=CARTESIAN_POINT('Ctrl Pts',(1.16347077574154,-1.81861982244698,3.81296900421478));
#48918=CARTESIAN_POINT('Ctrl Pts',(1.24907694843032,-3.42892053444273,2.45241968585354));
#48919=CARTESIAN_POINT('Ctrl Pts',(1.33450471449867,-4.17898154492915,0.486373019945627));
#48920=CARTESIAN_POINT('Ctrl Pts',(1.41975716940604,-3.88424365287751,-1.59151010962673));
#48921=CARTESIAN_POINT('Ctrl Pts',(1.51428676246171,-2.48577698688278,-3.45375961761171));
#48922=CARTESIAN_POINT('Ctrl Pts',(1.61802046319107,-0.0153163492785946,
-4.32134394881041));
#48923=CARTESIAN_POINT('Ctrl Pts',(1.73087587072984,2.67390119243303,-3.37517265531219));
#48924=CARTESIAN_POINT('Ctrl Pts',(1.8340460245136,4.05814750090039,-1.17181735141679));
#48925=CARTESIAN_POINT('Ctrl Pts',(1.92761553091683,3.9881968345771,1.13405393434499));
#48926=CARTESIAN_POINT('Ctrl Pts',(2.01165845365384,2.93784040804679,2.91554288974069));
#48927=CARTESIAN_POINT('Ctrl Pts',(2.09553292909152,1.15761277245939,3.96500388007765));
#48928=CARTESIAN_POINT('Ctrl Pts',(2.17924015408095,-0.902685284708361,
4.02211313220007));
#48929=CARTESIAN_POINT('Ctrl Pts',(2.2627817399313,-2.73048831066467,3.07746477058807));
#48930=CARTESIAN_POINT('Ctrl Pts',(2.34615886380898,-3.87072716449363,1.36987146987605));
#48931=CARTESIAN_POINT('Ctrl Pts',(2.42937324452721,-4.04253779113375,-0.672153450197734));
#48932=CARTESIAN_POINT('Ctrl Pts',(2.5124264631253,-3.20653945792688,-2.53891271248575));
#48933=CARTESIAN_POINT('Ctrl Pts',(2.59532000309479,-1.57527313865766,-3.76573008547188));
#48934=CARTESIAN_POINT('Ctrl Pts',(2.6780559376851,0.442467025625347,-4.05110137529429));
#48935=CARTESIAN_POINT('Ctrl Pts',(2.76063571470389,2.34131333359061,-3.32438634197174));
#48936=CARTESIAN_POINT('Ctrl Pts',(2.85221995159825,3.79872064908654,-1.60222299878064));
#48937=CARTESIAN_POINT('Ctrl Pts',(2.95274547399346,4.08479192723997,0.918805655449201));
#48938=CARTESIAN_POINT('Ctrl Pts',(3.06214407322622,2.6135493550915,3.25767084238896));
#48939=CARTESIAN_POINT('Ctrl Pts',(3.17128200065986,0.0126874208154328,
4.16628120635192));
#48940=CARTESIAN_POINT('Ctrl Pts',(3.2801643881585,-2.58236222387558,3.2566985796479));
#48941=CARTESIAN_POINT('Ctrl Pts',(3.38879683430733,-4.0403675070705,0.934430207343202));
#48942=CARTESIAN_POINT('Ctrl Pts',(3.49718492954501,-3.73339917040816,-1.78510203262339));
#48943=CARTESIAN_POINT('Ctrl Pts',(3.60533447778441,-1.80111124427296,-3.71502447158834));
#48944=CARTESIAN_POINT('Ctrl Pts',(3.71325145393808,0.904775445874618,-4.01918696084893));
#48945=CARTESIAN_POINT('Ctrl Pts',(3.82094203728054,3.20936283752695,-2.571197999788));
#48946=CARTESIAN_POINT('Ctrl Pts',(3.91647151249559,4.00145049915075,-0.29571072285262));
#48947=CARTESIAN_POINT('Ctrl Pts',(3.99992145777189,3.5431991882695,1.69504463314381));
#48948=CARTESIAN_POINT('Ctrl Pts',(4.07135713096102,2.45497139944041,3.06100203276521));
#48949=CARTESIAN_POINT('Ctrl Pts',(4.14270197092423,0.881853561078643,3.81799014426518));
#48950=CARTESIAN_POINT('Ctrl Pts',(4.21395799243881,-0.861429164779569,
3.81797589404032));
#48951=CARTESIAN_POINT('Ctrl Pts',(4.28512732882279,-2.42881599426564,3.0619250272124));
#48952=CARTESIAN_POINT('Ctrl Pts',(4.36805951249859,-3.69594778554289,1.47649887946172));
#48953=CARTESIAN_POINT('Ctrl Pts',(4.46270170274693,-3.96692590546529,-0.895015026539982));
#48954=CARTESIAN_POINT('Ctrl Pts',(4.56899588927351,-2.53814506387232,-3.16929534884689));
#48955=CARTESIAN_POINT('Ctrl Pts',(4.67511951925845,-0.00731392962691536,
-4.05241086380995));
#48956=CARTESIAN_POINT('Ctrl Pts',(4.75900454470091,1.98949699762205,-3.3517417086098));
#48957=CARTESIAN_POINT('Ctrl Pts',(4.82075273581193,3.02233350769069,-2.28440057824284));
#48958=CARTESIAN_POINT('Ctrl Pts',(4.87365081036613,3.65461916001154,-1.18105747976893));
#48959=CARTESIAN_POINT('Ctrl Pts',(4.93972199990629,3.88226253998919,0.430130146824839));
#48960=CARTESIAN_POINT('Ctrl Pts',(5.01892385351248,3.1862949056612,2.25227108844347));
#48961=CARTESIAN_POINT('Ctrl Pts',(5.09805405016988,1.69731476496512,3.50939368439439));
#48962=CARTESIAN_POINT('Ctrl Pts',(5.1770982730845,-0.211935388920614,3.88861454173858));
#48963=CARTESIAN_POINT('Ctrl Pts',(5.25609901422973,-2.06556469044695,3.29826074050364));
#48964=CARTESIAN_POINT('Ctrl Pts',(5.32183036241063,-3.17710297136331,2.11977728888582));
#48965=CARTESIAN_POINT('Ctrl Pts',(5.37445658284115,-3.64354521148007,0.94464387910966));
#48966=CARTESIAN_POINT('Ctrl Pts',(5.40066782824364,-3.7225043072094,0.325277046050365));
#48967=CARTESIAN_POINT('Ctrl Pts',(5.41387509844318,-3.72309915587958,0.00481785410125595));
#48968=CARTESIAN_POINT('Ctrl Pts',(0.824640136614524,4.2015762629893,-0.0164881184408875));
#48969=CARTESIAN_POINT('Ctrl Pts',(0.839431985789634,4.20091004569264,0.342419056375953));
#48970=CARTESIAN_POINT('Ctrl Pts',(0.869072200786422,4.11157275927187,1.04279181579199));
#48971=CARTESIAN_POINT('Ctrl Pts',(0.928267722148388,3.58659663339935,2.36455001110231));
#48972=CARTESIAN_POINT('Ctrl Pts',(1.00215309687483,2.33702889879683,3.68890382723956));
#48973=CARTESIAN_POINT('Ctrl Pts',(1.09062883690456,0.260587439725404,4.34897986608869));
#48974=CARTESIAN_POINT('Ctrl Pts',(1.17892287593827,-1.87177845740307,3.9247667085923));
#48975=CARTESIAN_POINT('Ctrl Pts',(1.26703196787133,-3.52913452482669,2.52439435278604));
#48976=CARTESIAN_POINT('Ctrl Pts',(1.35495625243847,-4.30109139555032,0.50094317918772));
#48977=CARTESIAN_POINT('Ctrl Pts',(1.44269582525899,-3.9977297615693,-1.63751557321081));
#48978=CARTESIAN_POINT('Ctrl Pts',(1.5399756322524,-2.5585815640104,-3.5539190962212));
#48979=CARTESIAN_POINT('Ctrl Pts',(1.64672492869982,-0.0163754272290712,
-4.44659940088065));
#48980=CARTESIAN_POINT('Ctrl Pts',(1.76283902689796,2.75044669042401,-3.47307159811878));
#48981=CARTESIAN_POINT('Ctrl Pts',(1.86897507368532,4.17436579205807,-1.20636694422441));
#48982=CARTESIAN_POINT('Ctrl Pts',(1.96522263354048,4.10238322499514,1.16541871037112));
#48983=CARTESIAN_POINT('Ctrl Pts',(2.05165710362801,3.02211393705529,2.99753313019623));
#48984=CARTESIAN_POINT('Ctrl Pts',(2.13790608656523,1.19152379694103,4.07662937239164));
#48985=CARTESIAN_POINT('Ctrl Pts',(2.22396853721079,-0.92668455854852,4.13528794998342));
#48986=CARTESIAN_POINT('Ctrl Pts',(2.30984545260645,-2.80549314624558,3.1642129683559));
#48987=CARTESIAN_POINT('Ctrl Pts',(2.39553686100961,-3.97729136934551,1.40924616985589));
#48988=CARTESIAN_POINT('Ctrl Pts',(2.48104362502894,-4.15376134490771,-0.688964949607138));
#48989=CARTESIAN_POINT('Ctrl Pts',(2.56636603958861,-3.29488852269384,-2.60662935524543));
#48990=CARTESIAN_POINT('Ctrl Pts',(2.65150601176586,-1.6194446573953,-3.86659630407993));
#48991=CARTESIAN_POINT('Ctrl Pts',(2.7364562269555,0.452274685033002,-4.15950968776552));
#48992=CARTESIAN_POINT('Ctrl Pts',(2.82123369824732,2.401520934455,-3.41344276030548));
#48993=CARTESIAN_POINT('Ctrl Pts',(2.91522208597613,3.89706826318983,-1.6460527156315));
#48994=CARTESIAN_POINT('Ctrl Pts',(3.01836404165339,4.19040693527911,0.94044790777557));
#48995=CARTESIAN_POINT('Ctrl Pts',(3.13054921535111,2.6814963714641,3.33868994257943));
#48996=CARTESIAN_POINT('Ctrl Pts',(3.24242029767871,0.0155424594777439,
4.26987430103556));
#48997=CARTESIAN_POINT('Ctrl Pts',(3.3539895659281,-2.64333786816468,3.3376826393174));
#48998=CARTESIAN_POINT('Ctrl Pts',(3.46524571947031,-4.13627311376035,0.959334384270673));
#48999=CARTESIAN_POINT('Ctrl Pts',(3.57619705361628,-3.82183356058938,-1.82432962022422));
#49000=CARTESIAN_POINT('Ctrl Pts',(3.68684681702081,-1.84478602084904,-3.79856245398834));
#49001=CARTESIAN_POINT('Ctrl Pts',(3.79720037313777,0.922021015180541,-4.10928217548828));
#49002=CARTESIAN_POINT('Ctrl Pts',(3.90726517222986,3.2771119107697,-2.62920334376493));
#49003=CARTESIAN_POINT('Ctrl Pts',(4.00483845873107,4.0857544532321,-0.305065708256623));
#49004=CARTESIAN_POINT('Ctrl Pts',(4.09002503800373,3.61790933094986,1.72702890336477));
#49005=CARTESIAN_POINT('Ctrl Pts',(4.16291899396928,2.50739659818956,3.12074066151443));
#49006=CARTESIAN_POINT('Ctrl Pts',(4.23569505179648,0.902784231955232,3.89280951201864));
#49007=CARTESIAN_POINT('Ctrl Pts',(4.30834828786622,-0.874602142649366,
3.89269192604326));
#49008=CARTESIAN_POINT('Ctrl Pts',(4.38087880591526,-2.47186195995458,3.12216898704288));
#49009=CARTESIAN_POINT('Ctrl Pts',(4.46535124680923,-3.76242506193018,1.50725518353649));
#49010=CARTESIAN_POINT('Ctrl Pts',(4.56172024478122,-4.03814548915269,-0.907329733904541));
#49011=CARTESIAN_POINT('Ctrl Pts',(4.66986044234963,-2.58427433554338,-3.22078427640133));
#49012=CARTESIAN_POINT('Ctrl Pts',(4.77776244000021,-0.0112384327514414,
-4.11841255765522));
#49013=CARTESIAN_POINT('Ctrl Pts',(4.86299326470177,2.01734328485411,-3.40624440202035));
#49014=CARTESIAN_POINT('Ctrl Pts',(4.92568672840066,3.06591863946052,-2.3226066451472));
#49015=CARTESIAN_POINT('Ctrl Pts',(4.97937885874153,3.7076520043964,-1.20271576540012));
#49016=CARTESIAN_POINT('Ctrl Pts',(5.0464263087054,3.93851483645866,0.432169333302392));
#49017=CARTESIAN_POINT('Ctrl Pts',(5.12674548922357,3.23260571308643,2.27981274817417));
#49018=CARTESIAN_POINT('Ctrl Pts',(5.2069452542926,1.72351417449459,3.55377340543451));
#49019=CARTESIAN_POINT('Ctrl Pts',(5.2870145686814,-0.210354086810664,3.93762595286232));
#49020=CARTESIAN_POINT('Ctrl Pts',(5.36698174629884,-2.08657397566065,3.34001993257469));
#49021=CARTESIAN_POINT('Ctrl Pts',(5.43350061820321,-3.21118799583293,2.14740741089702));
#49022=CARTESIAN_POINT('Ctrl Pts',(5.48669802545167,-3.68270059153974,0.959547171811996));
#49023=CARTESIAN_POINT('Ctrl Pts',(5.51320378504322,-3.76257892303397,0.333246203341611));
#49024=CARTESIAN_POINT('Ctrl Pts',(5.52654504990663,-3.76317980675502,0.00953578528314671));
#49025=CARTESIAN_POINT('Ctrl Pts',(0.721349619056559,4.4446284705926,-0.0117799836912939));
#49026=CARTESIAN_POINT('Ctrl Pts',(0.736957855041727,4.44392548365293,0.366935876306607));
#49027=CARTESIAN_POINT('Ctrl Pts',(0.768360964143123,4.34926747377125,1.10896390283271));
#49028=CARTESIAN_POINT('Ctrl Pts',(0.830966254263804,3.79399948150504,2.50685739811196));
#49029=CARTESIAN_POINT('Ctrl Pts',(0.909210267000149,2.47103126673906,3.90955883472892));
#49030=CARTESIAN_POINT('Ctrl Pts',(1.00291621006086,0.271693767768096,4.60862704115563));
#49031=CARTESIAN_POINT('Ctrl Pts',(1.0964998335884,-1.98838678064238,4.159329753954));
#49032=CARTESIAN_POINT('Ctrl Pts',(1.18992635866776,-3.74592111887884,2.67442969917082));
#49033=CARTESIAN_POINT('Ctrl Pts',(1.28320714472658,-4.56505572410638,0.527791428817508));
#49034=CARTESIAN_POINT('Ctrl Pts',(1.37633252272725,-4.24320511158861,-1.74204226726109));
#49035=CARTESIAN_POINT('Ctrl Pts',(1.47963324006593,-2.71509531029906,-3.77713627432662));
#49036=CARTESIAN_POINT('Ctrl Pts',(1.59303642701725,-0.0144100838093061,
-4.72580783762743));
#49037=CARTESIAN_POINT('Ctrl Pts',(1.71646151777425,2.92674151457479,-3.69119740428124));
#49038=CARTESIAN_POINT('Ctrl Pts',(1.82933043318807,4.44124697239644,-1.28077969442911));
#49039=CARTESIAN_POINT('Ctrl Pts',(1.93171929991264,4.36476264210786,1.24245072999059));
#49040=CARTESIAN_POINT('Ctrl Pts',(2.02369784986608,3.21525962979788,3.19218270635683));
#49041=CARTESIAN_POINT('Ctrl Pts',(2.11550244926919,1.2667206481616,4.34090326895668));
#49042=CARTESIAN_POINT('Ctrl Pts',(2.20713114238615,-0.988562626728529,
4.40343714551048));
#49043=CARTESIAN_POINT('Ctrl Pts',(2.29858133892869,-2.98941688938529,3.36936251834729));
#49044=CARTESIAN_POINT('Ctrl Pts',(2.38985139584946,-4.23760513244482,1.50010391473584));
#49045=CARTESIAN_POINT('Ctrl Pts',(2.48093895485383,-4.42565896182909,-0.73514385559243));
#49046=CARTESIAN_POINT('Ctrl Pts',(2.57184221732155,-3.51061303053924,-2.77835529581547));
#49047=CARTESIAN_POINT('Ctrl Pts',(2.66255917237085,-1.72534777250972,-4.12094012326353));
#49048=CARTESIAN_POINT('Ctrl Pts',(2.75308995897641,0.482512841602628,-4.43315431624234));
#49049=CARTESIAN_POINT('Ctrl Pts',(2.84342871960781,2.55977655442506,-3.63808847502519));
#49050=CARTESIAN_POINT('Ctrl Pts',(2.94359478029657,4.15371119436262,-1.75447635724346));
#49051=CARTESIAN_POINT('Ctrl Pts',(3.0534993425427,4.46628458035253,1.00183963908389));
#49052=CARTESIAN_POINT('Ctrl Pts',(3.17305409175693,2.85824449239317,3.55773500128709));
#49053=CARTESIAN_POINT('Ctrl Pts',(3.29225985050516,0.0173235716522711,
4.54988594670075));
#49054=CARTESIAN_POINT('Ctrl Pts',(3.4111105227762,-2.81524508966015,3.55670262369316));
#49055=CARTESIAN_POINT('Ctrl Pts',(3.52960855645907,-4.405387229637,1.02329494694289));
#49056=CARTESIAN_POINT('Ctrl Pts',(3.6477501002266,-4.07038494409819,-1.94097575854084));
#49057=CARTESIAN_POINT('Ctrl Pts',(3.76553344210117,-1.96563188563558,-4.04254830277241));
#49058=CARTESIAN_POINT('Ctrl Pts',(3.88295640499411,0.978743431351436,-4.37306760064782));
#49059=CARTESIAN_POINT('Ctrl Pts',(4.00001647488213,3.48362425976114,-2.79862452415612));
#49060=CARTESIAN_POINT('Ctrl Pts',(4.10374982384875,4.34335375479657,-0.327542203921762));
#49061=CARTESIAN_POINT('Ctrl Pts',(4.19428357469367,3.84599312218839,1.83216290559211));
#49062=CARTESIAN_POINT('Ctrl Pts',(4.27172174146588,2.66619885637548,3.31283119466691));
#49063=CARTESIAN_POINT('Ctrl Pts',(4.3489962055938,0.962215676959993,4.13258461147938));
#49064=CARTESIAN_POINT('Ctrl Pts',(4.42610940427065,-0.924394322650957,
4.13239028422168));
#49065=CARTESIAN_POINT('Ctrl Pts',(4.50306202721066,-2.61909336374746,3.31471375033465));
#49066=CARTESIAN_POINT('Ctrl Pts',(4.59265492084215,-3.98783075870693,1.60177932334117));
#49067=CARTESIAN_POINT('Ctrl Pts',(4.69476794148969,-4.27957493282873,-0.957131878749704));
#49068=CARTESIAN_POINT('Ctrl Pts',(4.80928970451843,-2.73953987979411,-3.40712746382027));
#49069=CARTESIAN_POINT('Ctrl Pts',(4.92344454247167,-0.0168010565349765,
-4.35630898735798));
#49070=CARTESIAN_POINT('Ctrl Pts',(5.01353042498076,2.12747449769232,-3.6032744047598));
#49071=CARTESIAN_POINT('Ctrl Pts',(5.07977128366408,3.23540859117732,-2.45821654233957));
#49072=CARTESIAN_POINT('Ctrl Pts',(5.13648217147255,3.9132385700417,-1.27530118138368));
#49073=CARTESIAN_POINT('Ctrl Pts',(5.20723938783248,4.15676099397256,0.450296379183357));
#49074=CARTESIAN_POINT('Ctrl Pts',(5.29195031220706,3.41204160437477,2.39903766275371));
#49075=CARTESIAN_POINT('Ctrl Pts',(5.37646206815912,1.82147811323575,3.74154376031287));
#49076=CARTESIAN_POINT('Ctrl Pts',(5.46077274553291,-0.215006596808714,
4.14549362307883));
#49077=CARTESIAN_POINT('Ctrl Pts',(5.54489246234653,-2.18888112277199,3.51672742480131));
#49078=CARTESIAN_POINT('Ctrl Pts',(5.61481604425459,-3.3708591485671,2.26269917616057));
#49079=CARTESIAN_POINT('Ctrl Pts',(5.67067535851732,-3.86597185995675,1.01536008122));
#49080=CARTESIAN_POINT('Ctrl Pts',(5.69854838705874,-3.94993232400006,0.356719058343651));
#49081=CARTESIAN_POINT('Ctrl Pts',(5.71252681611691,-3.95056190526938,0.0175485853374247));
#49082=CARTESIAN_POINT('Ctrl Pts',(0.338294245062112,4.55057569759653,0.0042037625125323));
#49083=CARTESIAN_POINT('Ctrl Pts',(0.354268648491283,4.54985621866307,0.391804253585384));
#49084=CARTESIAN_POINT('Ctrl Pts',(0.386459378345815,4.45283082043768,1.15244596626663));
#49085=CARTESIAN_POINT('Ctrl Pts',(0.450616543875562,3.88385341068114,2.58501032157865));
#49086=CARTESIAN_POINT('Ctrl Pts',(0.530955849690747,2.52591527649954,4.02565141037595));
#49087=CARTESIAN_POINT('Ctrl Pts',(0.627316019963871,0.264310635675801,
4.74491088714956));
#49088=CARTESIAN_POINT('Ctrl Pts',(0.723735630399143,-2.06432369137029,
4.28261993537111));
#49089=CARTESIAN_POINT('Ctrl Pts',(0.820158716135239,-3.87859456041539,
2.75041308513713));
#49090=CARTESIAN_POINT('Ctrl Pts',(0.916604340177546,-4.72602159109779,
0.531153832572511));
#49091=CARTESIAN_POINT('Ctrl Pts',(1.01305708152335,-4.3931659313265,-1.81989142402865));
#49092=CARTESIAN_POINT('Ctrl Pts',(1.12023653269649,-2.80816949118131,-3.9317242365496));
#49093=CARTESIAN_POINT('Ctrl Pts',(1.23813434882944,-0.000845642312135034,
-4.91906623538766));
#49094=CARTESIAN_POINT('Ctrl Pts',(1.36674602112875,3.06436157356124,-3.84215147235125));
#49095=CARTESIAN_POINT('Ctrl Pts',(1.48462403231379,4.64699863806454,-1.32534654137082));
#49096=CARTESIAN_POINT('Ctrl Pts',(1.5917660543832,4.56754799498206,1.31508654618603));
#49097=CARTESIAN_POINT('Ctrl Pts',(1.68817454439384,3.36309034412128,3.35895443333445));
#49098=CARTESIAN_POINT('Ctrl Pts',(1.78455906475243,1.31760244443516,4.56540662740121));
#49099=CARTESIAN_POINT('Ctrl Pts',(1.88091586352283,-1.05403946201403,4.63164486754336));
#49100=CARTESIAN_POINT('Ctrl Pts',(1.97723984292947,-3.16173649335291,3.54288691717697));
#49101=CARTESIAN_POINT('Ctrl Pts',(2.07352760672484,-4.47893140935848,1.57113238893729));
#49102=CARTESIAN_POINT('Ctrl Pts',(2.16977428334187,-4.67809571146175,-0.790665594289713));
#49103=CARTESIAN_POINT('Ctrl Pts',(2.26597577186357,-3.71014035199594,-2.95313903444104));
#49104=CARTESIAN_POINT('Ctrl Pts',(2.36212818012517,-1.81819297436985,-4.37651655635092));
#49105=CARTESIAN_POINT('Ctrl Pts',(2.45822704593622,0.525382903834377,-4.70837370126972));
#49106=CARTESIAN_POINT('Ctrl Pts',(2.55426812798931,2.73390242131373,-3.86353524962737));
#49107=CARTESIAN_POINT('Ctrl Pts',(2.66091177974622,4.43125636327941,-1.85846415538236));
#49108=CARTESIAN_POINT('Ctrl Pts',(2.778125747073,4.76554836922057,1.08098165568452));
#49109=CARTESIAN_POINT('Ctrl Pts',(2.90586892717749,3.04823830608109,3.81245443079));
#49110=CARTESIAN_POINT('Ctrl Pts',(3.0334755035129,0.00746606555007182,
4.87546967927499));
#49111=CARTESIAN_POINT('Ctrl Pts',(3.16093638887513,-3.03058736838478,3.81127322987509));
#49112=CARTESIAN_POINT('Ctrl Pts',(3.28824189006681,-4.73967683233644,1.09011017587669));
#49113=CARTESIAN_POINT('Ctrl Pts',(3.41538293420855,-4.38008226091659,-2.10000329693593));
#49114=CARTESIAN_POINT('Ctrl Pts',(3.54235044805458,-2.11186742976046,-4.36603149706744));
#49115=CARTESIAN_POINT('Ctrl Pts',(3.66913560141088,1.06707005130317,-4.72372043413534));
#49116=CARTESIAN_POINT('Ctrl Pts',(3.79572968394069,3.77635347593267,-3.02180133458617));
#49117=CARTESIAN_POINT('Ctrl Pts',(3.90807986203822,4.70807681195506,-0.345707133205359));
#49118=CARTESIAN_POINT('Ctrl Pts',(4.00625086823649,4.16903836543804,1.99624669567541));
#49119=CARTESIAN_POINT('Ctrl Pts',(4.09030243497979,2.88864931482185,3.60345074345437));
#49120=CARTESIAN_POINT('Ctrl Pts',(4.17425667899429,1.03751182625136,4.49424551995377));
#49121=CARTESIAN_POINT('Ctrl Pts',(4.25811096117765,-1.01398351055992,4.49423193370373));
#49122=CARTESIAN_POINT('Ctrl Pts',(4.34186270486352,-2.85847066249326,3.60451089771684));
#49123=CARTESIAN_POINT('Ctrl Pts',(4.43945045829832,-4.34951025112053,1.73889518038142));
#49124=CARTESIAN_POINT('Ctrl Pts',(4.55080259036115,-4.66822863041078,-1.0513329150146));
#49125=CARTESIAN_POINT('Ctrl Pts',(4.67582439075613,-2.98754166448033,-3.72620227444088));
#49126=CARTESIAN_POINT('Ctrl Pts',(4.80059124105991,-0.0120263346449302,
-4.76420085141347));
#49127=CARTESIAN_POINT('Ctrl Pts',(4.89915759678945,2.33414178609631,-3.94066076243851));
#49128=CARTESIAN_POINT('Ctrl Pts',(4.97167566555085,3.54709124235374,-2.68713431954456));
#49129=CARTESIAN_POINT('Ctrl Pts',(5.03378324431733,4.28942840336649,-1.39170068273366));
#49130=CARTESIAN_POINT('Ctrl Pts',(5.11132117925335,4.55644642555039,0.499203058196916));
#49131=CARTESIAN_POINT('Ctrl Pts',(5.204211387733,3.74000364932671,2.63600318529615));
#49132=CARTESIAN_POINT('Ctrl Pts',(5.29693616161317,1.99500656671931,4.10924355241873));
#49133=CARTESIAN_POINT('Ctrl Pts',(5.38950997969758,-0.240812582675891,
4.55262068051626));
#49134=CARTESIAN_POINT('Ctrl Pts',(5.48189232557165,-2.40883366006337,3.86258435496537));
#49135=CARTESIAN_POINT('Ctrl Pts',(5.55878512673359,-3.70832690498296,2.48354978245651));
#49136=CARTESIAN_POINT('Ctrl Pts',(5.62013978700551,-4.25231974581853,1.11355089098657));
#49137=CARTESIAN_POINT('Ctrl Pts',(5.65086529948741,-4.34491805581802,0.387529562643469));
#49138=CARTESIAN_POINT('Ctrl Pts',(5.66616207112364,-4.34560701456032,0.0163710261772646));
#49139=CARTESIAN_POINT('Ctrl Pts',(0.0170593592885323,4.31704107416506,
0.0170095058833432));
#49140=CARTESIAN_POINT('Ctrl Pts',(0.0322611335795961,4.31635639405152,
0.385863041260761));
#49141=CARTESIAN_POINT('Ctrl Pts',(0.0627811164807782,4.22437961039894,
1.10702759249781));
#49142=CARTESIAN_POINT('Ctrl Pts',(0.123740644702303,3.68390364811152,2.46821503884992));
#49143=CARTESIAN_POINT('Ctrl Pts',(0.200137694585886,2.39277960921485,3.83834435684185));
#49144=CARTESIAN_POINT('Ctrl Pts',(0.291937383647275,0.238467124150499,
4.52412171480303));
#49145=CARTESIAN_POINT('Ctrl Pts',(0.383934796302062,-1.98348327945548,
4.08341629079867));
#49146=CARTESIAN_POINT('Ctrl Pts',(0.476092625455518,-3.71777484054837,
2.61943491788025));
#49147=CARTESIAN_POINT('Ctrl Pts',(0.56842428847296,-4.52951306801332,0.495006553824729));
#49148=CARTESIAN_POINT('Ctrl Pts',(0.660920234839758,-4.2107917226016,-1.75962219957637));
#49149=CARTESIAN_POINT('Ctrl Pts',(0.763876444042794,-2.68873282536383,
-3.78855127791505));
#49150=CARTESIAN_POINT('Ctrl Pts',(0.87735917552732,0.0130019404539594,
-4.73992215653712));
#49151=CARTESIAN_POINT('Ctrl Pts',(1.00143747209998,2.97060794801125,-3.70215346005079));
#49152=CARTESIAN_POINT('Ctrl Pts',(1.1154269878762,4.50194744597732,-1.26897989212455));
#49153=CARTESIAN_POINT('Ctrl Pts',(1.21924908958377,4.42558239314702,1.28967440102454));
#49154=CARTESIAN_POINT('Ctrl Pts',(1.31283559471094,3.25681703771963,3.27395184877909));
#49155=CARTESIAN_POINT('Ctrl Pts',(1.40656633944771,1.26794513627352,4.44763751155047));
#49156=CARTESIAN_POINT('Ctrl Pts',(1.50043819264168,-1.04250891768418,4.51269321358057));
#49157=CARTESIAN_POINT('Ctrl Pts',(1.59444757833183,-3.09978507668561,3.45058005865305));
#49158=CARTESIAN_POINT('Ctrl Pts',(1.68859182136922,-4.38809455742526,1.52302965753274));
#49159=CARTESIAN_POINT('Ctrl Pts',(1.78286724301521,-4.58371350320302,-0.790333782115738));
#49160=CARTESIAN_POINT('Ctrl Pts',(1.87727051009661,-3.63435021507503,-2.91259494370384));
#49161=CARTESIAN_POINT('Ctrl Pts',(1.97179874248413,-1.77469819511752,-4.31235357101871));
#49162=CARTESIAN_POINT('Ctrl Pts',(2.06644688130757,0.53340573178967,-4.63973867522705));
#49163=CARTESIAN_POINT('Ctrl Pts',(2.16121394362965,2.71281770433348,-3.8066169222486));
#49164=CARTESIAN_POINT('Ctrl Pts',(2.26663623481388,4.39117481455026,-1.82494485863798));
#49165=CARTESIAN_POINT('Ctrl Pts',(2.3827596064462,4.72356161527894,1.08695595365977));
#49166=CARTESIAN_POINT('Ctrl Pts',(2.50962550191681,3.01919334092261,3.80038703978924));
#49167=CARTESIAN_POINT('Ctrl Pts',(2.63667020255104,-0.00773784804516612,
4.85999193198101));
#49168=CARTESIAN_POINT('Ctrl Pts',(2.76388543993548,-3.04038192998101,3.79913758985865));
#49169=CARTESIAN_POINT('Ctrl Pts',(2.8912606984098,-4.75154001018512,1.07720632230085));
#49170=CARTESIAN_POINT('Ctrl Pts',(3.01878711224752,-4.39221276685536,-2.12271333904207));
#49171=CARTESIAN_POINT('Ctrl Pts',(3.1464553025505,-2.112434572143,-4.40221261301575));
#49172=CARTESIAN_POINT('Ctrl Pts',(3.27425588526695,1.09179351798158,-4.7640888732722));
#49173=CARTESIAN_POINT('Ctrl Pts',(3.40217948205457,3.83027103061875,-3.04548218475403));
#49174=CARTESIAN_POINT('Ctrl Pts',(3.51598938618772,4.7752036557919,-0.334962986231444));
#49175=CARTESIAN_POINT('Ctrl Pts',(3.61563973232771,4.22849780113868,2.04242980680349));
#49176=CARTESIAN_POINT('Ctrl Pts',(3.70109729466062,2.92698374082993,3.67674162607492));
#49177=CARTESIAN_POINT('Ctrl Pts',(3.78659509245201,1.04198382964828,4.58426838084057));
#49178=CARTESIAN_POINT('Ctrl Pts',(3.87212990675981,-1.05062940346987,4.58464289114657));
#49179=CARTESIAN_POINT('Ctrl Pts',(3.95769867440709,-2.93530142451636,3.67594696906703));
#49180=CARTESIAN_POINT('Ctrl Pts',(4.05756489439709,-4.46149605353647,1.7670832262665));
#49181=CARTESIAN_POINT('Ctrl Pts',(4.1717454215982,-4.78942536463651,-1.09384432241825));
#49182=CARTESIAN_POINT('Ctrl Pts',(4.30025111609553,-3.06306433763481,-3.84395647764373));
#49183=CARTESIAN_POINT('Ctrl Pts',(4.42879998759059,0.00225573918968807,
-4.91468643030986));
#49184=CARTESIAN_POINT('Ctrl Pts',(4.5305942867175,2.4256086471289,-4.06511079601246));
#49185=CARTESIAN_POINT('Ctrl Pts',(4.60560876665858,3.68042867344509,-2.76847280341322));
#49186=CARTESIAN_POINT('Ctrl Pts',(4.66991088188852,4.44905704578208,-1.42732745616853));
#49187=CARTESIAN_POINT('Ctrl Pts',(4.75029250165825,4.72630844924892,0.532881291021042));
#49188=CARTESIAN_POINT('Ctrl Pts',(4.84675818745935,3.87892864485845,2.75210127777632));
#49189=CARTESIAN_POINT('Ctrl Pts',(4.94321603172176,2.0639903822995,4.28511445138593));
#49190=CARTESIAN_POINT('Ctrl Pts',(5.03968552854927,-0.265786119546311,
4.74757649013579));
#49191=CARTESIAN_POINT('Ctrl Pts',(5.13610992605831,-2.52891273917334,4.02793579977318));
#49192=CARTESIAN_POINT('Ctrl Pts',(5.21651607630675,-3.88799657674959,2.58610912462865));
#49193=CARTESIAN_POINT('Ctrl Pts',(5.28073297925971,-4.45751297641237,1.15222839320222));
#49194=CARTESIAN_POINT('Ctrl Pts',(5.31295628255007,-4.55464067477421,0.390818592699824));
#49195=CARTESIAN_POINT('Ctrl Pts',(5.32894534279131,-4.5553608138399,0.00286247099432417));
#49196=CARTESIAN_POINT('Ctrl Pts',(-0.000509373030547474,3.92021534661009,
0.016996973047247));
#49197=CARTESIAN_POINT('Ctrl Pts',(0.0133655849277437,3.91959042562335,
0.353656839069412));
#49198=CARTESIAN_POINT('Ctrl Pts',(0.0410178057586762,3.83628172595668,
1.00706848486642));
#49199=CARTESIAN_POINT('Ctrl Pts',(0.0964473712623517,3.3449812065841,2.24480055647181));
#49200=CARTESIAN_POINT('Ctrl Pts',(0.165833000914959,2.17209893003467,3.48910168092513));
#49201=CARTESIAN_POINT('Ctrl Pts',(0.249299786414105,0.213616043118768,
4.11301832351545));
#49202=CARTESIAN_POINT('Ctrl Pts',(0.332952618295147,-1.80695501753449,
3.71214532456504));
#49203=CARTESIAN_POINT('Ctrl Pts',(0.416802497335945,-3.38495223229509,
2.38039261819367));
#49204=CARTESIAN_POINT('Ctrl Pts',(0.500846500139207,-4.12396088271141,
0.446611903120177));
#49205=CARTESIAN_POINT('Ctrl Pts',(0.585087885198009,-3.83383487106712,
-1.60680296233244));
#49206=CARTESIAN_POINT('Ctrl Pts',(0.678908855398844,-2.4469602145113,-3.45582042752092));
#49207=CARTESIAN_POINT('Ctrl Pts',(0.78239581946303,0.0166703941746675,
-4.32374610526772));
#49208=CARTESIAN_POINT('Ctrl Pts',(0.895646446224181,2.71635016747082,-3.37695733163609));
#49209=CARTESIAN_POINT('Ctrl Pts',(0.999787586550202,4.11575032209256,-1.15422710837935));
#49210=CARTESIAN_POINT('Ctrl Pts',(1.09472345355387,4.04616602639483,1.18546806705486));
#49211=CARTESIAN_POINT('Ctrl Pts',(1.18036859245895,2.97675618213071,3.00148026190969));
#49212=CARTESIAN_POINT('Ctrl Pts',(1.26621705771563,1.155248892265,4.07666825088898));
#49213=CARTESIAN_POINT('Ctrl Pts',(1.35226925935515,-0.962745675997109,
4.13654259389504));
#49214=CARTESIAN_POINT('Ctrl Pts',(1.43852556730039,-2.85047653482757,3.16223962035245));
#49215=CARTESIAN_POINT('Ctrl Pts',(1.52498617068693,-4.03385922256971,1.39214156439959));
#49216=CARTESIAN_POINT('Ctrl Pts',(1.61165124607536,-4.21395408979635,-0.734463165223846));
#49217=CARTESIAN_POINT('Ctrl Pts',(1.69852082762757,-3.34060056023991,-2.68748353854695));
#49218=CARTESIAN_POINT('Ctrl Pts',(1.78559486750465,-1.62775490667668,-3.97709376117724));
#49219=CARTESIAN_POINT('Ctrl Pts',(1.87287344377062,0.500587977333086,-4.27928334792637));
#49220=CARTESIAN_POINT('Ctrl Pts',(1.96035587732167,2.51259896961598,-3.51047090069615));
#49221=CARTESIAN_POINT('Ctrl Pts',(2.05778526152882,4.06396467869906,-1.6792876022321));
#49222=CARTESIAN_POINT('Ctrl Pts',(2.16524726584212,4.37226319720578,1.0153436549924));
#49223=CARTESIAN_POINT('Ctrl Pts',(2.2828395210483,2.79318044202061,3.53087293178842));
#49224=CARTESIAN_POINT('Ctrl Pts',(2.40079070809031,-0.0168285977474749,
4.51542105142518));
#49225=CARTESIAN_POINT('Ctrl Pts',(2.51909864959676,-2.83743776879735,3.52966478818611));
#49226=CARTESIAN_POINT('Ctrl Pts',(2.63776186062134,-4.43231756105859,0.994362843096609));
#49227=CARTESIAN_POINT('Ctrl Pts',(2.75677778921884,-4.09788532816048,-1.99212131743342));
#49228=CARTESIAN_POINT('Ctrl Pts',(2.87614384522742,-1.96701233519621,-4.12407406978207));
#49229=CARTESIAN_POINT('Ctrl Pts',(2.99585707630498,1.03434971847348,-4.46399782820216));
#49230=CARTESIAN_POINT('Ctrl Pts',(3.11591416505015,3.60498437698043,-2.85193723841394));
#49231=CARTESIAN_POINT('Ctrl Pts',(3.22293457137712,4.49439067358845,-0.303368192450996));
#49232=CARTESIAN_POINT('Ctrl Pts',(3.31679611001667,3.97978943060175,1.9360373994789));
#49233=CARTESIAN_POINT('Ctrl Pts',(3.39739730622727,2.7524658458149,3.47765530299832));
#49234=CARTESIAN_POINT('Ctrl Pts',(3.47814554446175,0.972308519013181,4.33504755156959));
#49235=CARTESIAN_POINT('Ctrl Pts',(3.55903990182147,-1.00678432949211,4.33571435385092));
#49236=CARTESIAN_POINT('Ctrl Pts',(3.64007911331806,-2.79183322033623,3.47538186734198));
#49237=CARTESIAN_POINT('Ctrl Pts',(3.73479255980622,-4.23956446318879,1.66526560265338));
#49238=CARTESIAN_POINT('Ctrl Pts',(3.84327171133281,-4.55205389252981,-1.05267677488261));
#49239=CARTESIAN_POINT('Ctrl Pts',(3.96562611564225,-2.90933219122212,-3.67175612600794));
#49240=CARTESIAN_POINT('Ctrl Pts',(4.08828871140458,0.0152883107737241,
-4.69457325075005));
#49241=CARTESIAN_POINT('Ctrl Pts',(4.18563699424379,2.33312265754483,-3.8829464124187));
#49242=CARTESIAN_POINT('Ctrl Pts',(4.25748715092105,3.53511437004692,-2.64104529091489));
#49243=CARTESIAN_POINT('Ctrl Pts',(4.31912870973056,4.27199921354012,-1.35544035073423));
#49244=CARTESIAN_POINT('Ctrl Pts',(4.39628211340819,4.53851738355101,0.525971082460842));
#49245=CARTESIAN_POINT('Ctrl Pts',(4.48903104290479,3.72425076863922,2.65992095145394));
#49246=CARTESIAN_POINT('Ctrl Pts',(4.58193549181756,1.97650556376007,4.13676409759574));
#49247=CARTESIAN_POINT('Ctrl Pts',(4.67500541351684,-0.271152556122982,
4.5835619815803));
#49248=CARTESIAN_POINT('Ctrl Pts',(4.76821030596407,-2.45874208118696,3.88828759969444));
#49249=CARTESIAN_POINT('Ctrl Pts',(4.84603932740361,-3.77474566277566,2.49302437023683));
#49250=CARTESIAN_POINT('Ctrl Pts',(4.90832676369923,-4.32719027071689,1.10223497733668));
#49251=CARTESIAN_POINT('Ctrl Pts',(4.93956556049856,-4.42134796182669,0.364085063305676));
#49252=CARTESIAN_POINT('Ctrl Pts',(4.95509803681809,-4.42204753658693,-0.0127925756858374));
#49253=CARTESIAN_POINT('Ctrl Pts',(0.298096584279089,3.65836109017721,0.00420428892078251));
#49254=CARTESIAN_POINT('Ctrl Pts',(0.311087334711855,3.6577759934437,0.319409878254403));
#49255=CARTESIAN_POINT('Ctrl Pts',(0.336830084091236,3.5802354464982,0.927709628550148));
#49256=CARTESIAN_POINT('Ctrl Pts',(0.38855260702266,3.12183104328619,2.08266824732869));
#49257=CARTESIAN_POINT('Ctrl Pts',(0.453129934636734,2.02971933680628,3.24042531085447));
#49258=CARTESIAN_POINT('Ctrl Pts',(0.530755063824667,0.208415697693674,
3.8205922887506));
#49259=CARTESIAN_POINT('Ctrl Pts',(0.608414396037071,-1.66745393285822,
3.44786535315643));
#49260=CARTESIAN_POINT('Ctrl Pts',(0.686159436538254,-3.13032413522546,
2.21294951308035));
#49261=CARTESIAN_POINT('Ctrl Pts',(0.763972879863645,-3.81423765920946,
0.422321925736774));
#49262=CARTESIAN_POINT('Ctrl Pts',(0.84186845439323,-3.54566782855519,-1.47634282001782));
#49263=CARTESIAN_POINT('Ctrl Pts',(0.928510023393671,-2.26460758686192,
-3.18369230311773));
#49264=CARTESIAN_POINT('Ctrl Pts',(1.02393926290267,0.00745279667992231,
-3.98343126373423));
#49265=CARTESIAN_POINT('Ctrl Pts',(1.1282088165072,2.49279512049407,-3.11107079600691));
#49266=CARTESIAN_POINT('Ctrl Pts',(1.22394778855269,3.77880815931524,-1.06735588227691));
#49267=CARTESIAN_POINT('Ctrl Pts',(1.31111514094575,3.71461026876317,1.08086001346169));
#49268=CARTESIAN_POINT('Ctrl Pts',(1.3896723008585,2.73349922536098,2.7464657129172));
#49269=CARTESIAN_POINT('Ctrl Pts',(1.46833905161798,1.06424073934361,3.73150146410114));
#49270=CARTESIAN_POINT('Ctrl Pts',(1.54711899544478,-0.874769694920365,
3.78609161644686));
#49271=CARTESIAN_POINT('Ctrl Pts',(1.62601619609109,-2.60134983389898,2.89471971378898));
#49272=CARTESIAN_POINT('Ctrl Pts',(1.70503355230775,-3.68268674678379,1.27689142569084));
#49273=CARTESIAN_POINT('Ctrl Pts',(1.78417499391135,-3.8469551181542,-0.6651138286791));
#49274=CARTESIAN_POINT('Ctrl Pts',(1.86344387042269,-3.04984922963428,-2.44717700797688));
#49275=CARTESIAN_POINT('Ctrl Pts',(1.94284316920819,-1.48787263639168,-3.62298369274466));
#49276=CARTESIAN_POINT('Ctrl Pts',(2.02237693622473,0.451629060530175,-3.89819852788527));
#49277=CARTESIAN_POINT('Ctrl Pts',(2.10204759676506,2.28391860618936,-3.1979016042206));
#49278=CARTESIAN_POINT('Ctrl Pts',(2.19072686284899,3.69583592175625,-1.53107534941479));
#49279=CARTESIAN_POINT('Ctrl Pts',(2.28847866353304,3.97600385511532,0.920104709516196));
#49280=CARTESIAN_POINT('Ctrl Pts',(2.39537928379895,2.54026942442417,3.20676446315769));
#49281=CARTESIAN_POINT('Ctrl Pts',(2.50254921833245,-0.0129562004679963,
4.10110737239459));
#49282=CARTESIAN_POINT('Ctrl Pts',(2.60999586145542,-2.57453765912131,3.20567216837469));
#49283=CARTESIAN_POINT('Ctrl Pts',(2.71772516765194,-4.02232258005484,0.903913813484832));
#49284=CARTESIAN_POINT('Ctrl Pts',(2.82574372839834,-3.71867938979836,-1.80657721613234));
#49285=CARTESIAN_POINT('Ctrl Pts',(2.93405757815297,-1.78506235042054,-3.74105574559891));
#49286=CARTESIAN_POINT('Ctrl Pts',(3.04267271783813,0.938031464050205,-4.04941214503227));
#49287=CARTESIAN_POINT('Ctrl Pts',(3.15159502061989,3.27021991188957,-2.58686956509611));
#49288=CARTESIAN_POINT('Ctrl Pts',(3.24869195571493,4.07715622206919,-0.274641703989928));
#49289=CARTESIAN_POINT('Ctrl Pts',(3.33385675064398,3.6102629295096,1.75726838594271));
#49290=CARTESIAN_POINT('Ctrl Pts',(3.40699786221515,2.49655157382426,3.15620212552146));
#49291=CARTESIAN_POINT('Ctrl Pts',(3.48028345483719,0.880944659700569,3.93437721261743));
#49292=CARTESIAN_POINT('Ctrl Pts',(3.55371422038057,-0.915536983185619,
3.93501794003845));
#49293=CARTESIAN_POINT('Ctrl Pts',(3.62729125737481,-2.53622425264173,3.15395432305343));
#49294=CARTESIAN_POINT('Ctrl Pts',(3.71330261507569,-3.8509806770859,1.51019720414124));
#49295=CARTESIAN_POINT('Ctrl Pts',(3.8118527186074,-4.13505336346601,-0.958902703289102));
#49296=CARTESIAN_POINT('Ctrl Pts',(3.92305859063978,-2.64222932727816,-3.33943426601281));
#49297=CARTESIAN_POINT('Ctrl Pts',(4.03460899727506,0.0172906347131659,
-4.26987015966603));
#49298=CARTESIAN_POINT('Ctrl Pts',(4.12319413503313,2.12653084069738,-3.53152596583768));
#49299=CARTESIAN_POINT('Ctrl Pts',(4.18860565230255,3.22082638065193,-2.40094424117363));
#49300=CARTESIAN_POINT('Ctrl Pts',(4.24473809079781,3.89186716862466,-1.23025202544185));
#49301=CARTESIAN_POINT('Ctrl Pts',(4.31502966074825,4.13478863470262,0.483742163642918));
#49302=CARTESIAN_POINT('Ctrl Pts',(4.39957589386275,3.39268989860514,2.429083429048));
#49303=CARTESIAN_POINT('Ctrl Pts',(4.48432451794297,1.79854838577187,3.77622697986339));
#49304=CARTESIAN_POINT('Ctrl Pts',(4.5692686183663,-0.252936245272161,4.18443079336503));
#49305=CARTESIAN_POINT('Ctrl Pts',(4.65442518287259,-2.25140394373808,3.5490997128701));
#49306=CARTESIAN_POINT('Ctrl Pts',(4.72553786073744,-3.45425595710783,2.27452643733581));
#49307=CARTESIAN_POINT('Ctrl Pts',(4.78256122142649,-3.95993018611354,1.0012669710165));
#49308=CARTESIAN_POINT('Ctrl Pts',(4.81107750552547,-4.04587113521165,0.327446493022771));
#49309=CARTESIAN_POINT('Ctrl Pts',(4.82534909064748,-4.0465139200796,-0.0188370740532776));
#49310=CARTESIAN_POINT('Ctrl Pts',(0.688956982238612,3.72989859436059,-0.011771676272502));
#49311=CARTESIAN_POINT('Ctrl Pts',(0.702174766109974,3.7293032721575,0.308942617826199));
#49312=CARTESIAN_POINT('Ctrl Pts',(0.728412419797738,3.65025149910867,0.928927699894124));
#49313=CARTESIAN_POINT('Ctrl Pts',(0.781055770698673,3.18356680884235,2.1044162778148));
#49314=CARTESIAN_POINT('Ctrl Pts',(0.846674620528363,2.07353195281602,3.28052198629612));
#49315=CARTESIAN_POINT('Ctrl Pts',(0.925372417292195,0.226915654958949,
3.86816221327804));
#49316=CARTESIAN_POINT('Ctrl Pts',(1.0039282373004,-1.67046670484249,3.49061937856621));
#49317=CARTESIAN_POINT('Ctrl Pts',(1.08239262224571,-3.14650150602498,2.24387354628045));
#49318=CARTESIAN_POINT('Ctrl Pts',(1.16074810104558,-3.83465270230634,0.440602979531981));
#49319=CARTESIAN_POINT('Ctrl Pts',(1.23900844652084,-3.56429950374443,-1.46684219978431));
#49320=CARTESIAN_POINT('Ctrl Pts',(1.32585707942573,-2.27966928390904,-3.17791782495388));
#49321=CARTESIAN_POINT('Ctrl Pts',(1.42126320702305,-0.00774635499684935,
-3.9763100078759));
#49322=CARTESIAN_POINT('Ctrl Pts',(1.5251889897962,2.46889842538329,-3.1055672655037));
#49323=CARTESIAN_POINT('Ctrl Pts',(1.62032386985681,3.74579076667661,-1.07411530102224));
#49324=CARTESIAN_POINT('Ctrl Pts',(1.70671299419631,3.68153000413254,1.05483485686011));
#49325=CARTESIAN_POINT('Ctrl Pts',(1.78439233771942,2.71093422500403,2.70156674187247));
#49326=CARTESIAN_POINT('Ctrl Pts',(1.86200496845593,1.06376581310854,3.67292919184799));
#49327=CARTESIAN_POINT('Ctrl Pts',(1.93955458075406,-0.844971763668853,
3.72613393319396));
#49328=CARTESIAN_POINT('Ctrl Pts',(2.01704603660621,-2.54054699924709,2.85016942977958));
#49329=CARTESIAN_POINT('Ctrl Pts',(2.09448268075612,-3.59981265404682,1.2644088722943));
#49330=CARTESIAN_POINT('Ctrl Pts',(2.17186924701519,-3.75991607911409,-0.634585005549751));
#49331=CARTESIAN_POINT('Ctrl Pts',(2.24920986959975,-2.98172066966817,-2.37309080416439));
#49332=CARTESIAN_POINT('Ctrl Pts',(2.32650817304572,-1.46075735861725,-3.5173780157574));
#49333=CARTESIAN_POINT('Ctrl Pts',(2.4037704539101,0.423440863053585,-3.78422132593972));
#49334=CARTESIAN_POINT('Ctrl Pts',(2.48099742993376,2.19935922972781,-3.10493127396526));
#49335=CARTESIAN_POINT('Ctrl Pts',(2.56677463084692,3.56466710193294,-1.49224467784406));
#49336=CARTESIAN_POINT('Ctrl Pts',(2.66109148663689,3.83389443421792,0.872997558466858));
#49337=CARTESIAN_POINT('Ctrl Pts',(2.76395230037421,2.45138388800358,3.07261614748915));
#49338=CARTESIAN_POINT('Ctrl Pts',(2.86678959686819,0.000962930291893762,
3.92967379273786));
#49339=CARTESIAN_POINT('Ctrl Pts',(2.96961058667187,-2.44999053829016,3.0716577741312));
#49340=CARTESIAN_POINT('Ctrl Pts',(3.07242986170307,-3.83085160241301,0.874160218469037));
#49341=CARTESIAN_POINT('Ctrl Pts',(3.17525621245274,-3.5406642117419,-1.70597889374842));
#49342=CARTESIAN_POINT('Ctrl Pts',(3.27810003269075,-1.70389003181941,-3.54201749378549));
#49343=CARTESIAN_POINT('Ctrl Pts',(3.38097100851841,0.875408995607918,-3.83303032919846));
#49344=CARTESIAN_POINT('Ctrl Pts',(3.48387834482028,3.07828851197773,-2.45029862200831));
#49345=CARTESIAN_POINT('Ctrl Pts',(3.57539602828975,3.83808495585644,-0.270620622306617));
#49346=CARTESIAN_POINT('Ctrl Pts',(3.65551391848674,3.39850167651178,1.64079042729728));
#49347=CARTESIAN_POINT('Ctrl Pts',(3.72421465191342,2.35218871393199,2.95467125124523));
#49348=CARTESIAN_POINT('Ctrl Pts',(3.79294539429065,0.836823541180858,3.68423759790819));
#49349=CARTESIAN_POINT('Ctrl Pts',(3.86171128648602,-0.845569294720187,
3.6845686834364));
#49350=CARTESIAN_POINT('Ctrl Pts',(3.9305160372789,-2.36105179514293,2.95390454763975));
#49351=CARTESIAN_POINT('Ctrl Pts',(4.01083890816804,-3.58862834578777,1.41862728882207));
#49352=CARTESIAN_POINT('Ctrl Pts',(4.10270010008198,-3.85262944454734,-0.88313055241628));
#49353=CARTESIAN_POINT('Ctrl Pts',(4.20615878865277,-2.4630265539622,-3.09744279594199));
#49354=CARTESIAN_POINT('Ctrl Pts',(4.30973054597676,0.00668693977155496,
-3.96049481183038));
#49355=CARTESIAN_POINT('Ctrl Pts',(4.39182398199372,1.96125111015289,-3.27568322468014));
#49356=CARTESIAN_POINT('Ctrl Pts',(4.45237494972608,2.9741864942725,-2.2290598638584));
#49357=CARTESIAN_POINT('Ctrl Pts',(4.50430190138047,3.59493532071667,-1.14601631965969));
#49358=CARTESIAN_POINT('Ctrl Pts',(4.56925693234196,3.81916629261384,0.4379350138335));
#49359=CARTESIAN_POINT('Ctrl Pts',(4.64728728639836,3.13397091050645,2.23339295261525));
#49360=CARTESIAN_POINT('Ctrl Pts',(4.72541311711678,1.66418205411997,3.47494711303392));
#49361=CARTESIAN_POINT('Ctrl Pts',(4.80361529922962,-0.224728631862202,
3.85074359773365));
#49362=CARTESIAN_POINT('Ctrl Pts',(4.88195040442182,-2.06287164850845,3.26576977045013));
#49363=CARTESIAN_POINT('Ctrl Pts',(4.94724603874465,-3.16747854887194,2.09537568929752));
#49364=CARTESIAN_POINT('Ctrl Pts',(4.99963868315035,-3.63192116122577,0.925462967583616));
#49365=CARTESIAN_POINT('Ctrl Pts',(5.02574333679671,-3.71055096761041,0.308604734669394));
#49366=CARTESIAN_POINT('Ctrl Pts',(5.03890131113639,-3.71114359602036,-0.0106583500463774));
#49367=CARTESIAN_POINT('Ctrl Pts',(0.813870428188686,3.96245923091406,-0.0164881184408875));
#49368=CARTESIAN_POINT('Ctrl Pts',(0.827863881435175,3.96182897296034,0.323046899201097));
#49369=CARTESIAN_POINT('Ctrl Pts',(0.855776576686915,3.8777235191813,0.98261372822563));
#49370=CARTESIAN_POINT('Ctrl Pts',(0.91164293979103,3.38235777450735,2.23005863274043));
#49371=CARTESIAN_POINT('Ctrl Pts',(0.981299333783199,2.20407781698023,3.47855069743377));
#49372=CARTESIAN_POINT('Ctrl Pts',(1.06475475796298,0.245591313523208,4.10137579394894));
#49373=CARTESIAN_POINT('Ctrl Pts',(1.14801995745261,-1.76546201737438,3.70113724609284));
#49374=CARTESIAN_POINT('Ctrl Pts',(1.23112334588228,-3.3286789257896,2.38040969948328));
#49375=CARTESIAN_POINT('Ctrl Pts',(1.31405425162276,-4.0568214497295,0.471783311416064));
#49376=CARTESIAN_POINT('Ctrl Pts',(1.39682007324284,-3.77068607508619,-1.54548516328751));
#49377=CARTESIAN_POINT('Ctrl Pts',(1.48859751335545,-2.41293504528005,-3.3535345600583));
#49378=CARTESIAN_POINT('Ctrl Pts',(1.58932060338395,-0.0141931238132137,
-4.1959578414747));
#49379=CARTESIAN_POINT('Ctrl Pts',(1.69891363944235,2.59730954355204,-3.2771941918542));
#49380=CARTESIAN_POINT('Ctrl Pts',(1.79911717211155,3.94178755900518,-1.13723469292121));
#49381=CARTESIAN_POINT('Ctrl Pts',(1.89001020184871,3.87387138983037,1.10266716450794));
#49382=CARTESIAN_POINT('Ctrl Pts',(1.97166092482987,2.85344269161481,2.83344742015103));
#49383=CARTESIAN_POINT('Ctrl Pts',(2.05316121208527,1.12364269113143,3.85321962107559));
#49384=CARTESIAN_POINT('Ctrl Pts',(2.13451307741901,-0.878658896837783,
3.90875659364244));
#49385=CARTESIAN_POINT('Ctrl Pts',(2.21571945417949,-2.65536261814589,2.99056101462381));
#49386=CARTESIAN_POINT('Ctrl Pts',(2.2967823085229,-3.76397021259743,1.33041373899585));
#49387=CARTESIAN_POINT('Ctrl Pts',(2.37770464847043,-3.93109025436271,-0.655327951595781));
#49388=CARTESIAN_POINT('Ctrl Pts',(2.45848894616092,-3.11798970322431,-2.47107411872514));
#49389=CARTESIAN_POINT('Ctrl Pts',(2.539138236748,-1.53095692651357,-3.6646976699462));
#49390=CARTESIAN_POINT('Ctrl Pts',(2.61965150239195,0.43254661592197,-3.94244977897841));
#49391=CARTESIAN_POINT('Ctrl Pts',(2.70003978500417,2.28096457989066,-3.2351055267086));
#49392=CARTESIAN_POINT('Ctrl Pts',(2.78921497281684,3.70005464083461,-1.55832357099016));
#49393=CARTESIAN_POINT('Ctrl Pts',(2.88713754483823,3.978871723082,0.897304502209273));
#49394=CARTESIAN_POINT('Ctrl Pts',(2.99373926382005,2.54539755561737,3.1764149602916));
#49395=CARTESIAN_POINT('Ctrl Pts',(3.10013487511961,0.0100260539871462,
4.06239810401769));
#49396=CARTESIAN_POINT('Ctrl Pts',(3.20633868411026,-2.52115841647006,3.17542686994721));
#49397=CARTESIAN_POINT('Ctrl Pts',(3.31234811237552,-3.94408155000773,0.90944188237858));
#49398=CARTESIAN_POINT('Ctrl Pts',(3.41817428538941,-3.6446229361879,-1.74571659991173));
#49399=CARTESIAN_POINT('Ctrl Pts',(3.52382459568201,-1.75722515420472,-3.63111700668246));
#49400=CARTESIAN_POINT('Ctrl Pts',(3.62930813345658,0.887450966770746,-3.92861999578969));
#49401=CARTESIAN_POINT('Ctrl Pts',(3.73463542446446,3.14148071884394,-2.51269203574673));
#49402=CARTESIAN_POINT('Ctrl Pts',(3.82812092232632,3.91670767970764,-0.286048650138266));
#49403=CARTESIAN_POINT('Ctrl Pts',(3.90982285467911,3.46818164980758,1.66298970973192));
#49404=CARTESIAN_POINT('Ctrl Pts',(3.97979345533908,2.40232887286283,3.0009094587564));
#49405=CARTESIAN_POINT('Ctrl Pts',(4.0497099280914,0.860827997743688,3.74279364024213));
#49406=CARTESIAN_POINT('Ctrl Pts',(4.11956952823211,-0.848223352254005,
3.74285099046553));
#49407=CARTESIAN_POINT('Ctrl Pts',(4.18937342077798,-2.38551844241705,3.00143347916426));
#49408=CARTESIAN_POINT('Ctrl Pts',(4.27074480521005,-3.62886084584353,1.44594609859824));
#49409=CARTESIAN_POINT('Ctrl Pts',(4.36368118378899,-3.89527620214059,-0.882569356349999));
#49410=CARTESIAN_POINT('Ctrl Pts',(4.46811929683045,-2.49174100886108,-3.11716551782941));
#49411=CARTESIAN_POINT('Ctrl Pts',(4.57247822032509,-0.00337846350186114,
-3.98594899624739));
#49412=CARTESIAN_POINT('Ctrl Pts',(4.65503336657386,1.96170059971088,-3.29661664499807));
#49413=CARTESIAN_POINT('Ctrl Pts',(4.71582271106075,2.9784869170383,-2.24591417407558));
#49414=CARTESIAN_POINT('Ctrl Pts',(4.76791393631401,3.60111877586318,-1.15944268096052));
#49415=CARTESIAN_POINT('Ctrl Pts',(4.83301893094167,3.82552050348602,0.428030004985985));
#49416=CARTESIAN_POINT('Ctrl Pts',(4.91110192413723,3.1395319735366,2.2243674028123));
#49417=CARTESIAN_POINT('Ctrl Pts',(4.98916391106651,1.67086400618948,3.46453264131029));
#49418=CARTESIAN_POINT('Ctrl Pts',(5.06718831755995,-0.213604995253956,
3.83895695068989));
#49419=CARTESIAN_POINT('Ctrl Pts',(5.14521889040735,-2.04438566721443,3.25600753491638));
#49420=CARTESIAN_POINT('Ctrl Pts',(5.21018829958173,-3.14309383374398,2.09139171932537));
#49421=CARTESIAN_POINT('Ctrl Pts',(5.26222496048943,-3.60433678749298,0.929455512264779));
#49422=CARTESIAN_POINT('Ctrl Pts',(5.28813860325278,-3.68242999458204,0.317144549177678));
#49423=CARTESIAN_POINT('Ctrl Pts',(5.30120514697973,-3.68301850500413,9.99229193651664E-5));
#49424=CARTESIAN_POINT('Ctrl Pts',(0.819255282401605,4.08201774695168,-0.0164881184408875));
#49425=CARTESIAN_POINT('Ctrl Pts',(0.833647839427758,4.08136951356852,0.332730692506625));
#49426=CARTESIAN_POINT('Ctrl Pts',(0.862424164350343,3.99464878834545,1.01269819378028));
#49427=CARTESIAN_POINT('Ctrl Pts',(0.919954808790661,3.48448113484463,2.29729435781398));
#49428=CARTESIAN_POINT('Ctrl Pts',(0.991725652203481,2.27056227452172,3.58372650506595));
#49429=CARTESIAN_POINT('Ctrl Pts',(1.07769113094686,0.253097459046851,4.2251855373779));
#49430=CARTESIAN_POINT('Ctrl Pts',(1.16347077574154,-1.81861982244698,3.81296900421478));
#49431=CARTESIAN_POINT('Ctrl Pts',(1.24907694843032,-3.42892053444273,2.45241968585354));
#49432=CARTESIAN_POINT('Ctrl Pts',(1.33450471449867,-4.17898154492915,0.486373019945627));
#49433=CARTESIAN_POINT('Ctrl Pts',(1.41975716940604,-3.8842436528775,-1.59151010962673));
#49434=CARTESIAN_POINT('Ctrl Pts',(1.51428676246171,-2.48577698688278,-3.45375961761171));
#49435=CARTESIAN_POINT('Ctrl Pts',(1.61802046319107,-0.0153163492785947,
-4.32134394881041));
#49436=CARTESIAN_POINT('Ctrl Pts',(1.73087587072984,2.67390119243303,-3.37517265531219));
#49437=CARTESIAN_POINT('Ctrl Pts',(1.8340460245136,4.05814750090038,-1.17181735141679));
#49438=CARTESIAN_POINT('Ctrl Pts',(1.92761553091683,3.9881968345771,1.134053934345));
#49439=CARTESIAN_POINT('Ctrl Pts',(2.01165845365384,2.93784040804679,2.91554288974069));
#49440=CARTESIAN_POINT('Ctrl Pts',(2.09553292909152,1.15761277245939,3.96500388007765));
#49441=CARTESIAN_POINT('Ctrl Pts',(2.17924015408095,-0.902685284708361,
4.02211313220007));
#49442=CARTESIAN_POINT('Ctrl Pts',(2.2627817399313,-2.73048831066467,3.07746477058807));
#49443=CARTESIAN_POINT('Ctrl Pts',(2.34615886380898,-3.87072716449363,1.36987146987605));
#49444=CARTESIAN_POINT('Ctrl Pts',(2.42937324452721,-4.04253779113375,-0.672153450197734));
#49445=CARTESIAN_POINT('Ctrl Pts',(2.5124264631253,-3.20653945792688,-2.53891271248575));
#49446=CARTESIAN_POINT('Ctrl Pts',(2.59532000309479,-1.57527313865766,-3.76573008547188));
#49447=CARTESIAN_POINT('Ctrl Pts',(2.6780559376851,0.442467025625347,-4.05110137529429));
#49448=CARTESIAN_POINT('Ctrl Pts',(2.76063571470389,2.34131333359061,-3.32438634197174));
#49449=CARTESIAN_POINT('Ctrl Pts',(2.85221995159825,3.79872064908654,-1.60222299878064));
#49450=CARTESIAN_POINT('Ctrl Pts',(2.95274547399346,4.08479192723997,0.918805655449201));
#49451=CARTESIAN_POINT('Ctrl Pts',(3.06214407322622,2.6135493550915,3.25767084238896));
#49452=CARTESIAN_POINT('Ctrl Pts',(3.17128200065986,0.0126874208154326,
4.16628120635192));
#49453=CARTESIAN_POINT('Ctrl Pts',(3.2801643881585,-2.58236222387558,3.2566985796479));
#49454=CARTESIAN_POINT('Ctrl Pts',(3.38879683430733,-4.0403675070705,0.934430207343202));
#49455=CARTESIAN_POINT('Ctrl Pts',(3.49718492954501,-3.73339917040816,-1.78510203262339));
#49456=CARTESIAN_POINT('Ctrl Pts',(3.60533447778441,-1.80111124427296,-3.71502447158834));
#49457=CARTESIAN_POINT('Ctrl Pts',(3.71325145393808,0.904775445874618,-4.01918696084893));
#49458=CARTESIAN_POINT('Ctrl Pts',(3.82094203728053,3.20936283752695,-2.571197999788));
#49459=CARTESIAN_POINT('Ctrl Pts',(3.91647151249559,4.00145049915075,-0.29571072285262));
#49460=CARTESIAN_POINT('Ctrl Pts',(3.99992145777189,3.54319918826949,1.69504463314381));
#49461=CARTESIAN_POINT('Ctrl Pts',(4.07135713096102,2.45497139944041,3.06100203276521));
#49462=CARTESIAN_POINT('Ctrl Pts',(4.14270197092423,0.881853561078642,3.81799014426518));
#49463=CARTESIAN_POINT('Ctrl Pts',(4.21395799243881,-0.861429164779569,
3.81797589404032));
#49464=CARTESIAN_POINT('Ctrl Pts',(4.28512732882279,-2.42881599426564,3.0619250272124));
#49465=CARTESIAN_POINT('Ctrl Pts',(4.36805951249859,-3.69594778554289,1.47649887946172));
#49466=CARTESIAN_POINT('Ctrl Pts',(4.46270170274693,-3.96692590546529,-0.895015026539982));
#49467=CARTESIAN_POINT('Ctrl Pts',(4.56899588927351,-2.53814506387232,-3.16929534884689));
#49468=CARTESIAN_POINT('Ctrl Pts',(4.67511951925845,-0.00731392962691536,
-4.05241086380995));
#49469=CARTESIAN_POINT('Ctrl Pts',(4.75900454470091,1.98949699762205,-3.3517417086098));
#49470=CARTESIAN_POINT('Ctrl Pts',(4.82075273581193,3.02233350769069,-2.28440057824284));
#49471=CARTESIAN_POINT('Ctrl Pts',(4.87365081036613,3.65461916001154,-1.18105747976893));
#49472=CARTESIAN_POINT('Ctrl Pts',(4.93972199990629,3.88226253998919,0.430130146824839));
#49473=CARTESIAN_POINT('Ctrl Pts',(5.01892385351248,3.1862949056612,2.25227108844347));
#49474=CARTESIAN_POINT('Ctrl Pts',(5.09805405016988,1.69731476496512,3.50939368439439));
#49475=CARTESIAN_POINT('Ctrl Pts',(5.1770982730845,-0.211935388920614,3.88861454173858));
#49476=CARTESIAN_POINT('Ctrl Pts',(5.25609901422973,-2.06556469044695,3.29826074050364));
#49477=CARTESIAN_POINT('Ctrl Pts',(5.32183036241063,-3.17710297136331,2.11977728888582));
#49478=CARTESIAN_POINT('Ctrl Pts',(5.37445658284115,-3.64354521148007,0.94464387910966));
#49479=CARTESIAN_POINT('Ctrl Pts',(5.40066782824364,-3.7225043072094,0.325277046050365));
#49480=CARTESIAN_POINT('Ctrl Pts',(5.41387509844318,-3.72309915587958,0.00481785410125593));
#49481=CARTESIAN_POINT('',(0.819255282401605,4.08201774695168,-0.0164881184408875));
#49482=CARTESIAN_POINT('Origin',(0.42,4.1,-3.04061776853425E-19));
#49483=CARTESIAN_POINT('',(5.41387509844318,-3.72309915587958,0.00481785410125595));
#49484=CARTESIAN_POINT('Ctrl Pts',(0.819255282401605,4.08201774695168,-0.0164881184408875));
#49485=CARTESIAN_POINT('Ctrl Pts',(0.833647839427758,4.08136951356852,0.332730692506625));
#49486=CARTESIAN_POINT('Ctrl Pts',(0.862424164350343,3.99464878834545,1.01269819378028));
#49487=CARTESIAN_POINT('Ctrl Pts',(0.919954808790661,3.48448113484463,2.29729435781398));
#49488=CARTESIAN_POINT('Ctrl Pts',(0.991725652203481,2.27056227452172,3.58372650506595));
#49489=CARTESIAN_POINT('Ctrl Pts',(1.07769113094686,0.253097459046851,4.2251855373779));
#49490=CARTESIAN_POINT('Ctrl Pts',(1.16347077574154,-1.81861982244698,3.81296900421478));
#49491=CARTESIAN_POINT('Ctrl Pts',(1.24907694843032,-3.42892053444273,2.45241968585354));
#49492=CARTESIAN_POINT('Ctrl Pts',(1.33450471449867,-4.17898154492915,0.486373019945627));
#49493=CARTESIAN_POINT('Ctrl Pts',(1.41975716940604,-3.8842436528775,-1.59151010962673));
#49494=CARTESIAN_POINT('Ctrl Pts',(1.51428676246171,-2.48577698688278,-3.45375961761171));
#49495=CARTESIAN_POINT('Ctrl Pts',(1.61802046319107,-0.0153163492785947,
-4.32134394881041));
#49496=CARTESIAN_POINT('Ctrl Pts',(1.73087587072984,2.67390119243303,-3.37517265531219));
#49497=CARTESIAN_POINT('Ctrl Pts',(1.8340460245136,4.05814750090038,-1.17181735141679));
#49498=CARTESIAN_POINT('Ctrl Pts',(1.92761553091683,3.9881968345771,1.134053934345));
#49499=CARTESIAN_POINT('Ctrl Pts',(2.01165845365384,2.93784040804679,2.91554288974069));
#49500=CARTESIAN_POINT('Ctrl Pts',(2.09553292909152,1.15761277245939,3.96500388007765));
#49501=CARTESIAN_POINT('Ctrl Pts',(2.17924015408095,-0.902685284708361,
4.02211313220007));
#49502=CARTESIAN_POINT('Ctrl Pts',(2.2627817399313,-2.73048831066467,3.07746477058807));
#49503=CARTESIAN_POINT('Ctrl Pts',(2.34615886380898,-3.87072716449363,1.36987146987605));
#49504=CARTESIAN_POINT('Ctrl Pts',(2.42937324452721,-4.04253779113375,-0.672153450197734));
#49505=CARTESIAN_POINT('Ctrl Pts',(2.5124264631253,-3.20653945792688,-2.53891271248575));
#49506=CARTESIAN_POINT('Ctrl Pts',(2.59532000309479,-1.57527313865766,-3.76573008547188));
#49507=CARTESIAN_POINT('Ctrl Pts',(2.6780559376851,0.442467025625347,-4.05110137529429));
#49508=CARTESIAN_POINT('Ctrl Pts',(2.76063571470389,2.34131333359061,-3.32438634197174));
#49509=CARTESIAN_POINT('Ctrl Pts',(2.85221995159825,3.79872064908654,-1.60222299878064));
#49510=CARTESIAN_POINT('Ctrl Pts',(2.95274547399346,4.08479192723997,0.918805655449201));
#49511=CARTESIAN_POINT('Ctrl Pts',(3.06214407322622,2.6135493550915,3.25767084238896));
#49512=CARTESIAN_POINT('Ctrl Pts',(3.17128200065986,0.0126874208154326,
4.16628120635192));
#49513=CARTESIAN_POINT('Ctrl Pts',(3.2801643881585,-2.58236222387558,3.2566985796479));
#49514=CARTESIAN_POINT('Ctrl Pts',(3.38879683430733,-4.0403675070705,0.934430207343202));
#49515=CARTESIAN_POINT('Ctrl Pts',(3.49718492954501,-3.73339917040816,-1.78510203262339));
#49516=CARTESIAN_POINT('Ctrl Pts',(3.60533447778441,-1.80111124427296,-3.71502447158834));
#49517=CARTESIAN_POINT('Ctrl Pts',(3.71325145393808,0.904775445874618,-4.01918696084893));
#49518=CARTESIAN_POINT('Ctrl Pts',(3.82094203728053,3.20936283752695,-2.571197999788));
#49519=CARTESIAN_POINT('Ctrl Pts',(3.91647151249559,4.00145049915075,-0.29571072285262));
#49520=CARTESIAN_POINT('Ctrl Pts',(3.99992145777189,3.54319918826949,1.69504463314381));
#49521=CARTESIAN_POINT('Ctrl Pts',(4.07135713096102,2.45497139944041,3.06100203276521));
#49522=CARTESIAN_POINT('Ctrl Pts',(4.14270197092423,0.881853561078642,3.81799014426518));
#49523=CARTESIAN_POINT('Ctrl Pts',(4.21395799243881,-0.861429164779569,
3.81797589404032));
#49524=CARTESIAN_POINT('Ctrl Pts',(4.28512732882279,-2.42881599426564,3.0619250272124));
#49525=CARTESIAN_POINT('Ctrl Pts',(4.36805951249859,-3.69594778554289,1.47649887946172));
#49526=CARTESIAN_POINT('Ctrl Pts',(4.46270170274693,-3.96692590546529,-0.895015026539982));
#49527=CARTESIAN_POINT('Ctrl Pts',(4.56899588927351,-2.53814506387232,-3.16929534884689));
#49528=CARTESIAN_POINT('Ctrl Pts',(4.67511951925845,-0.00731392962691536,
-4.05241086380995));
#49529=CARTESIAN_POINT('Ctrl Pts',(4.75900454470091,1.98949699762205,-3.3517417086098));
#49530=CARTESIAN_POINT('Ctrl Pts',(4.82075273581193,3.02233350769069,-2.28440057824284));
#49531=CARTESIAN_POINT('Ctrl Pts',(4.87365081036613,3.65461916001154,-1.18105747976893));
#49532=CARTESIAN_POINT('Ctrl Pts',(4.93972199990629,3.88226253998919,0.430130146824839));
#49533=CARTESIAN_POINT('Ctrl Pts',(5.01892385351248,3.1862949056612,2.25227108844347));
#49534=CARTESIAN_POINT('Ctrl Pts',(5.09805405016988,1.69731476496512,3.50939368439439));
#49535=CARTESIAN_POINT('Ctrl Pts',(5.1770982730845,-0.211935388920614,3.88861454173858));
#49536=CARTESIAN_POINT('Ctrl Pts',(5.25609901422973,-2.06556469044695,3.29826074050364));
#49537=CARTESIAN_POINT('Ctrl Pts',(5.32183036241063,-3.17710297136331,2.11977728888582));
#49538=CARTESIAN_POINT('Ctrl Pts',(5.37445658284115,-3.64354521148007,0.94464387910966));
#49539=CARTESIAN_POINT('Ctrl Pts',(5.40066782824364,-3.7225043072094,0.325277046050365));
#49540=CARTESIAN_POINT('Ctrl Pts',(5.41387509844318,-3.72309915587958,0.00481785410125593));
#49541=CARTESIAN_POINT('Origin',(5.28,-4.1,4.54497550705923E-15));
#49542=CARTESIAN_POINT('Origin',(5.28,-4.1,4.54497550705923E-15));
#49543=CARTESIAN_POINT('Origin',(0.42,4.1,-3.04061776853425E-19));
#49544=CARTESIAN_POINT('',(0.,0.,0.));
#49545=CARTESIAN_POINT('Origin',(0.7,0.,0.));
#49546=CARTESIAN_POINT('',(0.8,4.3,-5.26598123633362E-16));
#49547=CARTESIAN_POINT('Origin',(0.8,0.,0.));
#49548=CARTESIAN_POINT('',(0.6,4.5,5.51091059616309E-16));
#49549=CARTESIAN_POINT('',(0.7,4.4,5.38844591624835E-16));
#49550=CARTESIAN_POINT('',(0.6,-4.5,-5.51091059616309E-16));
#49551=CARTESIAN_POINT('Origin',(0.6,0.,0.));
#49552=CARTESIAN_POINT('Origin',(0.6,0.,0.));
#49553=CARTESIAN_POINT('Origin',(0.475,0.,0.));
#49554=CARTESIAN_POINT('',(0.15,-4.5,-5.51091059616309E-16));
#49555=CARTESIAN_POINT('',(0.475,-4.5,-5.51091059616309E-16));
#49556=CARTESIAN_POINT('Origin',(0.15,0.,0.));
#49557=CARTESIAN_POINT('Origin',(0.8,2.225,0.));
#49558=CARTESIAN_POINT('',(0.8,-2.225,-2.72483912810286E-16));
#49559=CARTESIAN_POINT('Origin',(0.8,0.,0.));
#49560=CARTESIAN_POINT('Origin',(0.4,0.,0.));
#49561=CARTESIAN_POINT('',(0.,-2.225,-2.72483912810286E-16));
#49562=CARTESIAN_POINT('',(0.4,-2.225,-2.72483912810286E-16));
#49563=CARTESIAN_POINT('Origin',(0.,0.,0.));
#49564=CARTESIAN_POINT('Origin',(0.,4.35,0.));
#49565=CARTESIAN_POINT('',(-3.20923843055709E-16,-4.35,-5.32721357629099E-16));
#49566=CARTESIAN_POINT('Origin',(0.,0.,0.));
#49567=CARTESIAN_POINT('Origin',(0.0749999999999999,0.,0.));
#49568=CARTESIAN_POINT('',(0.0749999999999999,-4.425,-5.41906208622704E-16));
#49569=CARTESIAN_POINT('',(0.,0.,0.));
#49570=CARTESIAN_POINT('Origin',(-14.8,0.,0.));
#49571=CARTESIAN_POINT('',(-29.4201303078758,-1.95635727925632,0.00126400008466199));
#49572=CARTESIAN_POINT('',(-29.5218696921242,-1.95587002060241,0.00207606461394834));
#49573=CARTESIAN_POINT('',(-14.8,-1.954,-2.39295984553393E-16));
#49574=CARTESIAN_POINT('',(-29.646,0.862546263840124,1.75512488719095));
#49575=CARTESIAN_POINT('Ctrl Pts',(-29.4201303078758,-1.95635727925632,
0.00126400008466199));
#49576=CARTESIAN_POINT('Ctrl Pts',(-29.4239164395046,-1.95681317725995,
0.0674360876992789));
#49577=CARTESIAN_POINT('Ctrl Pts',(-29.4277025711335,-1.95374769504203,
0.133562632555316));
#49578=CARTESIAN_POINT('Ctrl Pts',(-29.4314887027624,-1.94702183852209,
0.199311248981777));
#49579=CARTESIAN_POINT('Ctrl Pts',(-29.4685374843882,-1.88120669687356,
0.84268722503347));
#49580=CARTESIAN_POINT('Ctrl Pts',(-29.505586266014,-1.46489646277197,1.44987508234769));
#49581=CARTESIAN_POINT('Ctrl Pts',(-29.5426350476398,-0.888515909042488,
1.74370487454672));
#49582=CARTESIAN_POINT('Ctrl Pts',(-29.5770900317598,-0.352487949298946,
2.0169635454113));
#49583=CARTESIAN_POINT('Ctrl Pts',(-29.6115450158799,0.321981753721779,
2.01920484775088));
#49584=CARTESIAN_POINT('Ctrl Pts',(-29.646,0.86356666800971,1.75642846275437));
#49585=CARTESIAN_POINT('',(-29.646,-0.86152585967032,1.75382131162765));
#49586=CARTESIAN_POINT('Origin',(-29.646,0.,0.));
#49587=CARTESIAN_POINT('Ctrl Pts',(-29.646,-0.861525859670322,1.75382131162764));
#49588=CARTESIAN_POINT('Ctrl Pts',(-29.6089512183742,-1.44475753426074,
1.46732167423177));
#49589=CARTESIAN_POINT('Ctrl Pts',(-29.5719024367484,-1.86881203157243,
0.869533272325591));
#49590=CARTESIAN_POINT('Ctrl Pts',(-29.5348536551226,-1.94371535502012,
0.228137491017513));
#49591=CARTESIAN_POINT('Ctrl Pts',(-29.5305256674564,-1.95246545814925,
0.153210518825829));
#49592=CARTESIAN_POINT('Ctrl Pts',(-29.5261976797903,-1.9564508380952,0.0776884545733211));
#49593=CARTESIAN_POINT('Ctrl Pts',(-29.5218696921242,-1.95587002060241,
0.00207606461394834));
#49594=CARTESIAN_POINT('Origin',(-14.8,0.,0.));
#49595=CARTESIAN_POINT('',(-28.7201303078758,-1.95131029814799,0.00101044981481321));
#49596=CARTESIAN_POINT('',(-28.8218696921242,-1.95116704690989,0.000889418674697316));
#49597=CARTESIAN_POINT('',(-14.8,-1.954,-2.39295984553393E-16));
#49598=CARTESIAN_POINT('Ctrl Pts',(-28.7201303078758,-1.95131029814799,
0.00101044981481321));
#49599=CARTESIAN_POINT('Ctrl Pts',(-28.7349570830831,-1.95252967038394,
0.261887710632697));
#49600=CARTESIAN_POINT('Ctrl Pts',(-28.7497838582905,-1.90389966119072,
0.522328508406575));
#49601=CARTESIAN_POINT('Ctrl Pts',(-28.7646106334978,-1.80327229746782,
0.760829685636639));
#49602=CARTESIAN_POINT('Ctrl Pts',(-28.8016594151236,-1.55182711319731,
1.35679056783254));
#49603=CARTESIAN_POINT('Ctrl Pts',(-28.8387081967495,-0.975716756591996,
1.81576312150198));
#49604=CARTESIAN_POINT('Ctrl Pts',(-28.8757569783753,-0.338635417708894,
1.92768240089395));
#49605=CARTESIAN_POINT('Ctrl Pts',(-28.9128057600011,0.298445921174204,
2.03960168028592));
#49606=CARTESIAN_POINT('Ctrl Pts',(-28.9498545416268,0.996498242335083,
1.80446768540043));
#49607=CARTESIAN_POINT('Ctrl Pts',(-28.9869033232527,1.43600427644337,1.32987593120208));
#49608=CARTESIAN_POINT('Ctrl Pts',(-29.0239521048785,1.87551031055165,0.855284177003728));
#49609=CARTESIAN_POINT('Ctrl Pts',(-29.0610008865043,2.05647005760734,0.14123466349252));
#49610=CARTESIAN_POINT('Ctrl Pts',(-29.0980496681301,1.89606454202561,-0.485381428782411));
#49611=CARTESIAN_POINT('Ctrl Pts',(-29.1350984497559,1.73565902644388,-1.11199752105734));
#49612=CARTESIAN_POINT('Ctrl Pts',(-29.1721472313817,1.23388824822474,-1.65118019209599));
#49613=CARTESIAN_POINT('Ctrl Pts',(-29.2091960130075,0.62040376768731,-1.85624320320092));
#49614=CARTESIAN_POINT('Ctrl Pts',(-29.2462447946333,0.0069192871498789,
-2.06130621430585));
#49615=CARTESIAN_POINT('Ctrl Pts',(-29.2832935762591,-0.718278895705847,
-1.93224956547705));
#49616=CARTESIAN_POINT('Ctrl Pts',(-29.320342357885,-1.22321796253597,-1.52793919366807));
#49617=CARTESIAN_POINT('Ctrl Pts',(-29.3536050078819,-1.67655571651092,
-1.16494657157745));
#49618=CARTESIAN_POINT('Ctrl Pts',(-29.3868676578788,-1.95235203664581,
-0.580083719870375));
#49619=CARTESIAN_POINT('Ctrl Pts',(-29.4201303078758,-1.95635727925632,
0.00126400008466199));
#49620=CARTESIAN_POINT('Ctrl Pts',(-29.5218696921242,-1.95587002060241,
0.00207606461394834));
#49621=CARTESIAN_POINT('Ctrl Pts',(-29.4891488981645,-1.95147887834975,
-0.569574694009445));
#49622=CARTESIAN_POINT('Ctrl Pts',(-29.4564281042048,-1.68609385625763,
-1.14638827290075));
#49623=CARTESIAN_POINT('Ctrl Pts',(-29.4237073102451,-1.24550369432567,
-1.51024047045956));
#49624=CARTESIAN_POINT('Ctrl Pts',(-29.3866585286193,-0.746636560599803,
-1.92221948991858));
#49625=CARTESIAN_POINT('Ctrl Pts',(-29.3496097469935,-0.0231501435643523,
-2.06117436812664));
#49626=CARTESIAN_POINT('Ctrl Pts',(-29.3125609653677,0.593320342234026,
-1.86492298541111));
#49627=CARTESIAN_POINT('Ctrl Pts',(-29.2755121837419,1.2097908280324,-1.66867160269558));
#49628=CARTESIAN_POINT('Ctrl Pts',(-29.2384634021161,1.71924538259371,-1.13721395905646));
#49629=CARTESIAN_POINT('Ctrl Pts',(-29.2014146204903,1.88874566918039,-0.513087459649483));
#49630=CARTESIAN_POINT('Ctrl Pts',(-29.1643658388645,2.05824595576708,0.111039039757497));
#49631=CARTESIAN_POINT('Ctrl Pts',(-29.1273170572387,1.88779197437914,0.827834394932333));
#49632=CARTESIAN_POINT('Ctrl Pts',(-29.0902682756129,1.45527344708612,1.30883134527791));
#49633=CARTESIAN_POINT('Ctrl Pts',(-29.0532194939871,1.02275491979311,1.78982829562348));
#49634=CARTESIAN_POINT('Ctrl Pts',(-29.0161707123613,0.328171846595005,
2.03502684113979));
#49635=CARTESIAN_POINT('Ctrl Pts',(-28.9791219307355,-0.310483119724783,
1.93239222026172));
#49636=CARTESIAN_POINT('Ctrl Pts',(-28.9420731491096,-0.949138086044573,
1.82975759938366));
#49637=CARTESIAN_POINT('Ctrl Pts',(-28.9050243674839,-1.53186494548605,
1.37928981211122));
#49638=CARTESIAN_POINT('Ctrl Pts',(-28.867975585858,-1.79197429141891,0.78707299175062));
#49639=CARTESIAN_POINT('Ctrl Pts',(-28.8526069546134,-1.89987324100642,
0.541408720765679));
#49640=CARTESIAN_POINT('Ctrl Pts',(-28.8372383233688,-1.9522571758889,0.271352718622898));
#49641=CARTESIAN_POINT('Ctrl Pts',(-28.8218696921242,-1.95116704690989,
0.000889418674697316));
#49642=CARTESIAN_POINT('Origin',(-14.8,0.,0.));
#49643=CARTESIAN_POINT('',(-28.0201303078758,-1.95270169711206,-0.00166393224656974));
#49644=CARTESIAN_POINT('',(-28.1218696921242,-1.95296243627918,-0.001715799027382));
#49645=CARTESIAN_POINT('',(-14.8,-1.954,-2.39295984553393E-16));
#49646=CARTESIAN_POINT('Ctrl Pts',(-28.0201303078758,-1.95270169711206,
-0.00166393224656974));
#49647=CARTESIAN_POINT('Ctrl Pts',(-28.0459977266616,-1.94902264159807,
0.452657212652301));
#49648=CARTESIAN_POINT('Ctrl Pts',(-28.0718651454474,-1.79103646858732,
0.909285351732831));
#49649=CARTESIAN_POINT('Ctrl Pts',(-28.0977325642333,-1.50128604242506,
1.25570336172352));
#49650=CARTESIAN_POINT('Ctrl Pts',(-28.1347813458591,-1.08628907833883,
1.75186284750948));
#49651=CARTESIAN_POINT('Ctrl Pts',(-28.1718301274849,-0.400996326824849,
2.0219417923873));
#49652=CARTESIAN_POINT('Ctrl Pts',(-28.2088789091107,0.240920463268404,
1.94232014777131));
#49653=CARTESIAN_POINT('Ctrl Pts',(-28.2459276907365,0.882837253361657,
1.86269850315532));
#49654=CARTESIAN_POINT('Ctrl Pts',(-28.2829764723623,1.48137808203418,1.43337626904552));
#49655=CARTESIAN_POINT('Ctrl Pts',(-28.3200252539881,1.76257907476627,0.850861942132011));
#49656=CARTESIAN_POINT('Ctrl Pts',(-28.3570740356139,2.04378006749835,0.268347615218507));
#49657=CARTESIAN_POINT('Ctrl Pts',(-28.3941228172398,2.00764122428999,-0.467358804498699));
#49658=CARTESIAN_POINT('Ctrl Pts',(-28.4311715988656,1.67070420294189,-1.01950899589596));
#49659=CARTESIAN_POINT('Ctrl Pts',(-28.4682203804914,1.3337671815938,-1.57165918729322));
#49660=CARTESIAN_POINT('Ctrl Pts',(-28.5052691621172,0.696031982105959,
-1.94025315037054));
#49661=CARTESIAN_POINT('Ctrl Pts',(-28.542317943743,0.0494020009907347,
-1.95658054933522));
#49662=CARTESIAN_POINT('Ctrl Pts',(-28.5793667253688,-0.597227980124488,
-1.9729079482999));
#49663=CARTESIAN_POINT('Ctrl Pts',(-28.6164155069946,-1.2527527428671,-1.63696878315194));
#49664=CARTESIAN_POINT('Ctrl Pts',(-28.6534642886204,-1.61712511827056,
-1.10252459521678));
#49665=CARTESIAN_POINT('Ctrl Pts',(-28.6756862950389,-1.83567711673311,
-0.781962847881812));
#49666=CARTESIAN_POINT('Ctrl Pts',(-28.6979083014573,-1.94948273299814,
-0.389985979499672));
#49667=CARTESIAN_POINT('Ctrl Pts',(-28.7201303078758,-1.95131029814799,
0.00101044981481321));
#49668=CARTESIAN_POINT('Ctrl Pts',(-28.8218696921242,-1.95116704690989,
0.000889418674697316));
#49669=CARTESIAN_POINT('Ctrl Pts',(-28.800189541743,-1.94962922875134,-0.380646511372493));
#49670=CARTESIAN_POINT('Ctrl Pts',(-28.7785093913618,-1.84167774817481,
-0.762992966149612));
#49671=CARTESIAN_POINT('Ctrl Pts',(-28.7568292409806,-1.63304206720153,
-1.07881961262616));
#49672=CARTESIAN_POINT('Ctrl Pts',(-28.7197804593548,-1.27650866462705,
-1.61852954319356));
#49673=CARTESIAN_POINT('Ctrl Pts',(-28.682731677729,-0.625950027053866,
-1.96398355087959));
#49674=CARTESIAN_POINT('Ctrl Pts',(-28.6456828961032,0.0208505694140376,
-1.95708928963784));
#49675=CARTESIAN_POINT('Ctrl Pts',(-28.6086341144774,0.667651165881941,
-1.9501950283961));
#49676=CARTESIAN_POINT('Ctrl Pts',(-28.5715853328516,1.31069372124456,-1.59095249822659));
#49677=CARTESIAN_POINT('Ctrl Pts',(-28.5345365512257,1.65565039527921,-1.04377891490295));
#49678=CARTESIAN_POINT('Ctrl Pts',(-28.4974877695999,2.00060706931387,-0.496605331579296));
#49679=CARTESIAN_POINT('Ctrl Pts',(-28.4604389879741,2.04747786202056,0.238499304898493));
#49680=CARTESIAN_POINT('Ctrl Pts',(-28.4233902063483,1.77480635131727,0.82505539855511));
#49681=CARTESIAN_POINT('Ctrl Pts',(-28.3863414247225,1.50213484061398,1.41161149221173));
#49682=CARTESIAN_POINT('Ctrl Pts',(-28.3492926430967,0.909921026500707,
1.84961904304717));
#49683=CARTESIAN_POINT('Ctrl Pts',(-28.3122438614709,0.269234122665934,
1.93859765049293));
#49684=CARTESIAN_POINT('Ctrl Pts',(-28.2751950798451,-0.371452781168839,
2.02757625793869));
#49685=CARTESIAN_POINT('Ctrl Pts',(-28.2381462982193,-1.06061277472511,
1.76752592199477));
#49686=CARTESIAN_POINT('Ctrl Pts',(-28.2010975165935,-1.48280470005023,
1.2774745440133));
#49687=CARTESIAN_POINT('Ctrl Pts',(-28.1746882417704,-1.78375339781367,
0.928153973926285));
#49688=CARTESIAN_POINT('Ctrl Pts',(-28.1482789669473,-1.94905065505998,
0.461965596840646));
#49689=CARTESIAN_POINT('Ctrl Pts',(-28.1218696921242,-1.95296243627918,
-0.001715799027382));
#49690=CARTESIAN_POINT('Origin',(-14.8,0.,0.));
#49691=CARTESIAN_POINT('',(-27.3201303078758,-1.95720343110015,-4.59226069798868E-5));
#49692=CARTESIAN_POINT('',(-27.4218696921242,-1.95719380567024,0.000130774435998158));
#49693=CARTESIAN_POINT('',(-14.8,-1.954,-2.39295984553393E-16));
#49694=CARTESIAN_POINT('Ctrl Pts',(-27.3201303078758,-1.95720343110015,
-4.59226069798868E-5));
#49695=CARTESIAN_POINT('Ctrl Pts',(-27.3570383702401,-1.95698081009987,
0.644334435783812));
#49696=CARTESIAN_POINT('Ctrl Pts',(-27.3939464326044,-1.6076554733493,1.28892163264944));
#49697=CARTESIAN_POINT('Ctrl Pts',(-27.4308544949687,-1.06757773856952,
1.64040494610073));
#49698=CARTESIAN_POINT('Ctrl Pts',(-27.4679032765946,-0.525440850989191,
1.9932283589537));
#49699=CARTESIAN_POINT('Ctrl Pts',(-27.5049520582203,0.208905769743558,
2.05070859500226));
#49700=CARTESIAN_POINT('Ctrl Pts',(-27.5420008398462,0.799337409788294,
1.78653584048903));
#49701=CARTESIAN_POINT('Ctrl Pts',(-27.579049621472,1.38976904983303,1.5223630859758));
#49702=CARTESIAN_POINT('Ctrl Pts',(-27.6160984030978,1.83628570918976,0.936537340900787));
#49703=CARTESIAN_POINT('Ctrl Pts',(-27.6531471847236,1.93450803573618,0.297202416780847));
#49704=CARTESIAN_POINT('Ctrl Pts',(-27.6901959663494,2.0327303622826,-0.342132507339095));
#49705=CARTESIAN_POINT('Ctrl Pts',(-27.7272447479752,1.78265835601873,-1.03497661050397));
#49706=CARTESIAN_POINT('Ctrl Pts',(-27.764293529601,1.29875483693254,-1.46420166094053));
#49707=CARTESIAN_POINT('Ctrl Pts',(-27.8013423112268,0.814851317846355,
-1.89342671137708));
#49708=CARTESIAN_POINT('Ctrl Pts',(-27.8383910928526,0.0971162859378687,
-2.05903270908532));
#49709=CARTESIAN_POINT('Ctrl Pts',(-27.8754398744784,-0.52592899899265,
-1.88521861971562));
#49710=CARTESIAN_POINT('Ctrl Pts',(-27.9124886561042,-1.14897428392317,
-1.71140453034592));
#49711=CARTESIAN_POINT('Ctrl Pts',(-27.9495374377301,-1.67732982187572,
-1.19817035389827));
#49712=CARTESIAN_POINT('Ctrl Pts',(-27.9865862193559,-1.86915700252275,
-0.580433252327395));
#49713=CARTESIAN_POINT('Ctrl Pts',(-27.9977675821958,-1.92705065557309,
-0.393999519036611));
#49714=CARTESIAN_POINT('Ctrl Pts',(-28.0089489450358,-1.95429199318879,
-0.198047251704987));
#49715=CARTESIAN_POINT('Ctrl Pts',(-28.0201303078758,-1.95270169711206,
-0.00166393224656974));
#49716=CARTESIAN_POINT('Ctrl Pts',(-28.1218696921242,-1.95296243627918,
-0.001715799027382));
#49717=CARTESIAN_POINT('Ctrl Pts',(-28.1112301853215,-1.95453837591293,
-0.188519162567876));
#49718=CARTESIAN_POINT('Ctrl Pts',(-28.1005906785188,-1.92992075791155,
-0.374915632262465));
#49719=CARTESIAN_POINT('Ctrl Pts',(-28.0899511717161,-1.87742689675453,
-0.553099583238752));
#49720=CARTESIAN_POINT('Ctrl Pts',(-28.0529023900903,-1.69463331103975,
-1.17356991249032));
#49721=CARTESIAN_POINT('Ctrl Pts',(-28.0158536084645,-1.17382228251622,
-1.69445815097443));
#49722=CARTESIAN_POINT('Ctrl Pts',(-27.9788048268387,-0.553379347191945,
-1.8773442373971));
#49723=CARTESIAN_POINT('Ctrl Pts',(-27.9417560452129,0.0670635881323265,
-2.06023032381977));
#49724=CARTESIAN_POINT('Ctrl Pts',(-27.904707263587,0.787138430257349,-1.905114258181));
#49725=CARTESIAN_POINT('Ctrl Pts',(-27.8676584819612,1.27725304489518,-1.48299535913524));
#49726=CARTESIAN_POINT('Ctrl Pts',(-27.8306097003354,1.76736765953301,-1.06087646008947));
#49727=CARTESIAN_POINT('Ctrl Pts',(-27.7935609187096,2.02752204668364,-0.371754727636712));
#49728=CARTESIAN_POINT('Ctrl Pts',(-27.7565121370838,1.93863843106925,0.268945265900702));
#49729=CARTESIAN_POINT('Ctrl Pts',(-27.719463355458,1.84975481545485,0.909645259438115));
#49730=CARTESIAN_POINT('Ctrl Pts',(-27.6824145738322,1.41183319707542,1.50192351406018));
#49731=CARTESIAN_POINT('Ctrl Pts',(-27.6453657922064,0.825318839035808,
1.77468285389483));
#49732=CARTESIAN_POINT('Ctrl Pts',(-27.6083170105806,0.238804480996198,
2.04744219372948));
#49733=CARTESIAN_POINT('Ctrl Pts',(-27.5712682289548,-0.496302616703593,
2.00068261877672));
#49734=CARTESIAN_POINT('Ctrl Pts',(-27.534219447329,-1.04352966997717,1.65580684870039));
#49735=CARTESIAN_POINT('Ctrl Pts',(-27.4971706657032,-1.59075672325075,
1.31093107862406));
#49736=CARTESIAN_POINT('Ctrl Pts',(-27.4601218840773,-1.95010373209812,
0.667939113424155));
#49737=CARTESIAN_POINT('Ctrl Pts',(-27.4230731024515,-1.9570905808131,0.021140891794882));
#49738=CARTESIAN_POINT('Ctrl Pts',(-27.4226719656757,-1.95716622923779,
0.0141378395533869));
#49739=CARTESIAN_POINT('Ctrl Pts',(-27.4222708288999,-1.95720057063946,
0.00713434110616324));
#49740=CARTESIAN_POINT('Ctrl Pts',(-27.4218696921242,-1.95719380567024,
0.000130774435998158));
#49741=CARTESIAN_POINT('Origin',(-14.8,0.,0.));
#49742=CARTESIAN_POINT('',(-26.6201303078758,-1.95283586288168,0.00169258002336921));
#49743=CARTESIAN_POINT('',(-26.7218696921242,-1.95258020183271,0.00163427418135859));
#49744=CARTESIAN_POINT('',(-14.8,-1.954,-2.39295984553393E-16));
#49745=CARTESIAN_POINT('Ctrl Pts',(-26.6201303078758,-1.95283586288168,
0.00169258002336925));
#49746=CARTESIAN_POINT('Ctrl Pts',(-26.6310302321928,-1.95442075370972,
0.193099573221502));
#49747=CARTESIAN_POINT('Ctrl Pts',(-26.6419301565098,-1.92855963518578,
0.384087563662016));
#49748=CARTESIAN_POINT('Ctrl Pts',(-26.6528300808268,-1.87350212627677,
0.566251176395773));
#49749=CARTESIAN_POINT('Ctrl Pts',(-26.6898788624526,-1.68636196226216,
1.18542427448898));
#49750=CARTESIAN_POINT('Ctrl Pts',(-26.7269276440784,-1.16191114472938,
1.70264789965425));
#49751=CARTESIAN_POINT('Ctrl Pts',(-26.7639764257042,-0.540201001802173,
1.88117875005868));
#49752=CARTESIAN_POINT('Ctrl Pts',(-26.80102520733,0.0815091411250285,2.0597096004631));
#49753=CARTESIAN_POINT('Ctrl Pts',(-26.8380739889558,0.800478609446652,
1.89954767610668));
#49754=CARTESIAN_POINT('Ctrl Pts',(-26.8751227705816,1.28762110954235,1.47400220150885));
#49755=CARTESIAN_POINT('Ctrl Pts',(-26.9121715522074,1.77476360963806,1.04845672691101));
#49756=CARTESIAN_POINT('Ctrl Pts',(-26.9492203338332,2.03007914150785,0.357527702071744));
#49757=CARTESIAN_POINT('Ctrl Pts',(-26.986269115459,1.93670482594731,-0.282533235389988));
#49758=CARTESIAN_POINT('Ctrl Pts',(-27.0233178970849,1.84333051038677,-0.922594172851714));
#49759=CARTESIAN_POINT('Ctrl Pts',(-27.0603666787107,1.40126634739592,-1.5117870229359));
#49760=CARTESIAN_POINT('Ctrl Pts',(-27.0974154603365,0.81285369280208,-1.78042677090386));
#49761=CARTESIAN_POINT('Ctrl Pts',(-27.1344642419623,0.224441038208241,
-2.04906651887181));
#49762=CARTESIAN_POINT('Ctrl Pts',(-27.1715130235881,-0.510320107988586,
-1.99715316472352));
#49763=CARTESIAN_POINT('Ctrl Pts',(-27.2085618052139,-1.05511529455704,
-1.64844846023135));
#49764=CARTESIAN_POINT('Ctrl Pts',(-27.2456105868397,-1.5999104811255,-1.29974375573918));
#49765=CARTESIAN_POINT('Ctrl Pts',(-27.2826593684655,-1.95473970806558,
-0.654247700903117));
#49766=CARTESIAN_POINT('Ctrl Pts',(-27.3197081500913,-1.95719074432167,
-0.00741637865638378));
#49767=CARTESIAN_POINT('Ctrl Pts',(-27.3198488693528,-1.95720005388589,
-0.00495957381760083));
#49768=CARTESIAN_POINT('Ctrl Pts',(-27.3199895886143,-1.95720427988659,
-0.0025027497156606));
#49769=CARTESIAN_POINT('Ctrl Pts',(-27.3201303078758,-1.95720343110015,
-4.59226069797758E-5));
#49770=CARTESIAN_POINT('Ctrl Pts',(-27.4218696921242,-1.95719380567024,
0.000130774435998158));
#49771=CARTESIAN_POINT('Ctrl Pts',(-27.3852220472741,-1.95657576164103,
-0.6397113928845));
#49772=CARTESIAN_POINT('Ctrl Pts',(-27.3485744024242,-1.61286119405438,
-1.28012298663609));
#49773=CARTESIAN_POINT('Ctrl Pts',(-27.3119267575741,-1.07905472547464,
-1.6328782457365));
#49774=CARTESIAN_POINT('Ctrl Pts',(-27.2748779759483,-0.539405332838623,
-1.98949468357996));
#49775=CARTESIAN_POINT('Ctrl Pts',(-27.2378291943225,0.194520141016002,
-2.05212308120823));
#49776=CARTESIAN_POINT('Ctrl Pts',(-27.2007804126967,0.786789750479916,
-1.79209719757795));
#49777=CARTESIAN_POINT('Ctrl Pts',(-27.1637316310709,1.37905935994383,-1.53207131394768));
#49778=CARTESIAN_POINT('Ctrl Pts',(-27.1266828494451,1.82967310501703,-0.949391149058858));
#49779=CARTESIAN_POINT('Ctrl Pts',(-27.0896340678193,1.93237631892021,-0.310760738106043));
#49780=CARTESIAN_POINT('Ctrl Pts',(-27.0525852861935,2.03507953282338,0.327869672846779));
#49781=CARTESIAN_POINT('Ctrl Pts',(-27.0155365045676,1.78987221555653,1.0224503298636));
#49782=CARTESIAN_POINT('Ctrl Pts',(-26.9784877229418,1.30899052071573,1.45505817391017));
#49783=CARTESIAN_POINT('Ctrl Pts',(-26.941438941316,0.828108825874929,1.88766601795674));
#49784=CARTESIAN_POINT('Ctrl Pts',(-26.9043901596902,0.11155275346018,2.05830104903307));
#49785=CARTESIAN_POINT('Ctrl Pts',(-26.8673413780644,-0.512696061414957,
1.88886029737629));
#49786=CARTESIAN_POINT('Ctrl Pts',(-26.8302925964386,-1.1369448762901,1.71941954571951));
#49787=CARTESIAN_POINT('Ctrl Pts',(-26.7932438148128,-1.66888643362564,
1.20990301132961));
#49788=CARTESIAN_POINT('Ctrl Pts',(-26.756195033187,-1.86504074799682,0.593526311295277));
#49789=CARTESIAN_POINT('Ctrl Pts',(-26.7447532528327,-1.92561911203712,
0.40317060976334));
#49790=CARTESIAN_POINT('Ctrl Pts',(-26.7333114724784,-1.9541714137465,0.202623007266345));
#49791=CARTESIAN_POINT('Ctrl Pts',(-26.7218696921242,-1.95258020183271,
0.00163427418135859));
#49792=CARTESIAN_POINT('Origin',(-14.8,0.,0.));
#49793=CARTESIAN_POINT('',(-25.9201303078758,-1.95123630633075,-0.000939509159223334));
#49794=CARTESIAN_POINT('',(-26.0218696921242,-1.95138426211563,-0.00106972641374984));
#49795=CARTESIAN_POINT('',(-14.8,-1.954,-2.39295984553393E-16));
#49796=CARTESIAN_POINT('Ctrl Pts',(-25.9201303078758,-1.95123630633075,
-0.000939509159223334));
#49797=CARTESIAN_POINT('Ctrl Pts',(-25.9420708757713,-1.94955826401817,
0.385140851071647));
#49798=CARTESIAN_POINT('Ctrl Pts',(-25.9640114436667,-1.83881330297959,
0.77210885471596));
#49799=CARTESIAN_POINT('Ctrl Pts',(-25.9859520115622,-1.6254339170275,1.09023630159484));
#49800=CARTESIAN_POINT('Ctrl Pts',(-26.023000793188,-1.26512208229091,1.62742541924811));
#49801=CARTESIAN_POINT('Ctrl Pts',(-26.0600495748139,-0.612162500266134,
1.96832529110062));
#49802=CARTESIAN_POINT('Ctrl Pts',(-26.0970983564397,0.0345725427856284,
1.9568994228693));
#49803=CARTESIAN_POINT('Ctrl Pts',(-26.1341471380655,0.681307585837391,
1.94547355463798));
#49804=CARTESIAN_POINT('Ctrl Pts',(-26.1711959196913,1.32181808991614,1.58172194632284));
#49805=CARTESIAN_POINT('Ctrl Pts',(-26.2082447013171,1.66292995359561,1.03214077594632));
#49806=CARTESIAN_POINT('Ctrl Pts',(-26.2452934829429,2.00404181727508,0.482559605569794));
#49807=CARTESIAN_POINT('Ctrl Pts',(-26.2823422645687,2.04575504055526,-0.252851126868104));
#49808=CARTESIAN_POINT('Ctrl Pts',(-26.3193910461945,1.76897667074363,-0.837479641723851));
#49809=CARTESIAN_POINT('Ctrl Pts',(-26.3564398278203,1.492198300932,-1.4221081565796));
#49810=CARTESIAN_POINT('Ctrl Pts',(-26.3934886094461,0.896928338028557,
-1.85595445385319));
#49811=CARTESIAN_POINT('Ctrl Pts',(-26.4305373910719,0.255633408841942,
-1.94043865459214));
#49812=CARTESIAN_POINT('Ctrl Pts',(-26.4675861726977,-0.385661520344672,
-2.02492285533109));
#49813=CARTESIAN_POINT('Ctrl Pts',(-26.5046349543235,-1.07298141581446,
-1.7600449595354));
#49814=CARTESIAN_POINT('Ctrl Pts',(-26.5416837359493,-1.49172660830113,
-1.26704472612698));
#49815=CARTESIAN_POINT('Ctrl Pts',(-26.5678325932581,-1.78727501250166,
-0.919087460303604));
#49816=CARTESIAN_POINT('Ctrl Pts',(-26.593981450567,-1.94903371867341,-0.457491723232458));
#49817=CARTESIAN_POINT('Ctrl Pts',(-26.6201303078758,-1.95283586288168,
0.00169258002336921));
#49818=CARTESIAN_POINT('Ctrl Pts',(-26.7218696921242,-1.95258020183271,
0.00163427418135859));
#49819=CARTESIAN_POINT('Ctrl Pts',(-26.6962626908526,-1.9490190282882,-0.448183724793736));
#49820=CARTESIAN_POINT('Ctrl Pts',(-26.6706556895811,-1.79447622573103,
-0.900211241067141));
#49821=CARTESIAN_POINT('Ctrl Pts',(-26.6450486883096,-1.51005466648862,
-1.24514472168841));
#49822=CARTESIAN_POINT('Ctrl Pts',(-26.6079999066838,-1.09854719920242,
-1.74420218895902));
#49823=CARTESIAN_POINT('Ctrl Pts',(-26.5709511250579,-0.415165193223192,
-2.01908025782145));
#49824=CARTESIAN_POINT('Ctrl Pts',(-26.5339023434321,0.227294130752652,
-1.94396189573941));
#49825=CARTESIAN_POINT('Ctrl Pts',(-26.4968535618063,0.86975345472849,-1.86884353365738));
#49826=CARTESIAN_POINT('Ctrl Pts',(-26.4598047801805,1.47129009670094,-1.44372874063089));
#49827=CARTESIAN_POINT('Ctrl Pts',(-26.4227559985547,1.75656904907977,-0.863200816547895));
#49828=CARTESIAN_POINT('Ctrl Pts',(-26.3857072169289,2.0418480014586,-0.282672892464901));
#49829=CARTESIAN_POINT('Ctrl Pts',(-26.3486584353031,2.01086926424381,0.453268162674601));
#49830=CARTESIAN_POINT('Ctrl Pts',(-26.3116096536773,1.67781240732092,1.00776783025682));
#49831=CARTESIAN_POINT('Ctrl Pts',(-26.2745608720515,1.34475555039803,1.56226749783905));
#49832=CARTESIAN_POINT('Ctrl Pts',(-26.2375120904257,0.709620573767041,
1.93532577786399));
#49833=CARTESIAN_POINT('Ctrl Pts',(-26.2004633087999,0.0631210955000985,
1.95618664784198));
#49834=CARTESIAN_POINT('Ctrl Pts',(-26.1634145271741,-0.583378382766842,
1.97704751781996));
#49835=CARTESIAN_POINT('Ctrl Pts',(-26.1263657455483,-1.24124236266973,
1.645710977751));
#49836=CARTESIAN_POINT('Ctrl Pts',(-26.0893169639225,-1.60935371975343,
1.11383619917551));
#49837=CARTESIAN_POINT('Ctrl Pts',(-26.0668345399897,-1.8327358451903,0.791077022589047));
#49838=CARTESIAN_POINT('Ctrl Pts',(-26.0443521160569,-1.94941763628547,
0.394470379537052));
#49839=CARTESIAN_POINT('Ctrl Pts',(-26.0218696921242,-1.95138426211563,
-0.00106972641374984));
#49840=CARTESIAN_POINT('Origin',(-14.8,0.,0.));
#49841=CARTESIAN_POINT('',(-25.2201303078758,-1.95626804686365,-0.00119577595913939));
#49842=CARTESIAN_POINT('',(-25.3218696921242,-1.95648018646661,-0.00106297053860165));
#49843=CARTESIAN_POINT('',(-14.8,-1.954,-2.39295984553393E-16));
#49844=CARTESIAN_POINT('Ctrl Pts',(-25.2201303078758,-1.95626804686365,
-0.00119577595913939));
#49845=CARTESIAN_POINT('Ctrl Pts',(-25.2531115193497,-1.95211771839792,
0.575356106654941));
#49846=CARTESIAN_POINT('Ctrl Pts',(-25.2860927308237,-1.68152135564075,
1.15529448608977));
#49847=CARTESIAN_POINT('Ctrl Pts',(-25.3190739422977,-1.23475142449969,
1.51856495798993));
#49848=CARTESIAN_POINT('Ctrl Pts',(-25.3561227239235,-0.732881393773812,
1.92663754789925));
#49849=CARTESIAN_POINT('Ctrl Pts',(-25.3931715055493,-0.00870320332811321,
2.06130338198116));
#49850=CARTESIAN_POINT('Ctrl Pts',(-25.4302202871751,0.606312719881358,
1.86092329171546));
#49851=CARTESIAN_POINT('Ctrl Pts',(-25.4672690688009,1.22132864309083,1.66054320144975));
#49852=CARTESIAN_POINT('Ctrl Pts',(-25.5043178504267,1.72718229906407,1.12511718683642));
#49853=CARTESIAN_POINT('Ctrl Pts',(-25.5413666320525,1.89233464183849,0.499720136913584));
#49854=CARTESIAN_POINT('Ctrl Pts',(-25.5784154136783,2.05748698461291,-0.125676913009264));
#49855=CARTESIAN_POINT('Ctrl Pts',(-25.6154641953042,1.8819380141885,-0.841044998241625));
#49856=CARTESIAN_POINT('Ctrl Pts',(-25.65251297693,1.44603990485877,-1.31894624814468));
#49857=CARTESIAN_POINT('Ctrl Pts',(-25.6895617585558,1.01014179552905,-1.79684749804773));
#49858=CARTESIAN_POINT('Ctrl Pts',(-25.7266105401816,0.313894547294022,
-2.03728191262149));
#49859=CARTESIAN_POINT('Ctrl Pts',(-25.7636593218074,-0.324015947776813,
-1.93019798920358));
#49860=CARTESIAN_POINT('Ctrl Pts',(-25.8007081034332,-0.961926442847647,
-1.82311406578568));
#49861=CARTESIAN_POINT('Ctrl Pts',(-25.837756885059,-1.54150018475429,-1.36851180437611));
#49862=CARTESIAN_POINT('Ctrl Pts',(-25.8748056666848,-1.7974550119834,-0.774471491944305));
#49863=CARTESIAN_POINT('Ctrl Pts',(-25.8899138804151,-1.90183146015221,
-0.532226332702917));
#49864=CARTESIAN_POINT('Ctrl Pts',(-25.9050220941455,-1.95239180157717,
-0.266793366143644));
#49865=CARTESIAN_POINT('Ctrl Pts',(-25.9201303078758,-1.95123630633075,
-0.000939509159223334));
#49866=CARTESIAN_POINT('Ctrl Pts',(-26.0218696921242,-1.95138426211563,
-0.00106972641374984));
#49867=CARTESIAN_POINT('Ctrl Pts',(-26.0073033344311,-1.95265843857347,
-0.257340077086639));
#49868=CARTESIAN_POINT('Ctrl Pts',(-25.9927369767381,-1.90577815577188,
-0.513162723070535));
#49869=CARTESIAN_POINT('Ctrl Pts',(-25.978170619045,-1.80856360753824,-0.748163184984166));
#49870=CARTESIAN_POINT('Ctrl Pts',(-25.9411218374192,-1.56130340397485,
-1.34587477348635));
#49871=CARTESIAN_POINT('Ctrl Pts',(-25.9040730557934,-0.988424262583569,
-1.80888493340869));
#49872=CARTESIAN_POINT('Ctrl Pts',(-25.8670242741676,-0.352144096159522,
-1.92526491928297));
#49873=CARTESIAN_POINT('Ctrl Pts',(-25.8299754925418,0.284136070264529,
-2.04164490515726));
#49874=CARTESIAN_POINT('Ctrl Pts',(-25.792926710916,0.98381726172135,-1.81139471698347));
#49875=CARTESIAN_POINT('Ctrl Pts',(-25.7558779292902,1.42664180361434,-1.33990433914493));
#49876=CARTESIAN_POINT('Ctrl Pts',(-25.7188291476644,1.86946634550733,-0.86841396130639));
#49877=CARTESIAN_POINT('Ctrl Pts',(-25.6817803660386,2.0554342378365,-0.155683393803116));
#49878=CARTESIAN_POINT('Ctrl Pts',(-25.6447315844128,1.89942436333606,0.472056735832567));
#49879=CARTESIAN_POINT('Ctrl Pts',(-25.6076828027869,1.74341448883562,1.09979686546825));
#49880=CARTESIAN_POINT('Ctrl Pts',(-25.5706340211611,1.24542684750557,1.64254655723634));
#49881=CARTESIAN_POINT('Ctrl Pts',(-25.5335852395353,0.63340005758682,1.85187873278168));
#49882=CARTESIAN_POINT('Ctrl Pts',(-25.4965364579095,0.021373267668069,
2.06121090832702));
#49883=CARTESIAN_POINT('Ctrl Pts',(-25.4594876762837,-0.704692670839375,
1.93712556764961));
#49884=CARTESIAN_POINT('Ctrl Pts',(-25.4224388946579,-1.21246327201675,
1.53641898188292));
#49885=CARTESIAN_POINT('Ctrl Pts',(-25.3889158271467,-1.67191233880164,
1.17384527939171));
#49886=CARTESIAN_POINT('Ctrl Pts',(-25.3553927596354,-1.95263690100395,
0.584794018605935));
#49887=CARTESIAN_POINT('Ctrl Pts',(-25.3218696921242,-1.95648018646661,
-0.00106297053860165));
#49888=CARTESIAN_POINT('Origin',(-14.8,0.,0.));
#49889=CARTESIAN_POINT('',(-24.5201303078758,-1.95487751651067,0.00168938103890723));
#49890=CARTESIAN_POINT('',(-24.6218696921242,-1.95459134654687,0.00173615845593911));
#49891=CARTESIAN_POINT('',(-14.8,-1.954,-2.39295984553393E-16));
#49892=CARTESIAN_POINT('Ctrl Pts',(-24.5201303078758,-1.95487751651067,
0.00168938103890723));
#49893=CARTESIAN_POINT('Ctrl Pts',(-24.5271033813024,-1.95599066552706,
0.123812897405317));
#49894=CARTESIAN_POINT('Ctrl Pts',(-24.5340764547291,-1.94552840215917,
0.245746288538353));
#49895=CARTESIAN_POINT('Ctrl Pts',(-24.5410495281557,-1.92280272977114,
0.365349523502659));
#49896=CARTESIAN_POINT('Ctrl Pts',(-24.5780983097815,-1.80205848658205,
1.00081596172956));
#49897=CARTESIAN_POINT('Ctrl Pts',(-24.6151470914073,-1.33512736895152,
1.57050383221171));
#49898=CARTESIAN_POINT('Ctrl Pts',(-24.6521958730332,-0.735732820863401,
1.81365592884741));
#49899=CARTESIAN_POINT('Ctrl Pts',(-24.6892446546589,-0.136338272775288,
2.05680802548311));
#49900=CARTESIAN_POINT('Ctrl Pts',(-24.7262934362848,0.595519705770406,
1.97342434827236));
#49901=CARTESIAN_POINT('Ctrl Pts',(-24.7633422179106,1.12485549960288,1.60167122623594));
#49902=CARTESIAN_POINT('Ctrl Pts',(-24.8003909995364,1.65419129343536,1.22991810419951));
#49903=CARTESIAN_POINT('Ctrl Pts',(-24.8374397811622,1.98100490255462,0.569795537337402));
#49904=CARTESIAN_POINT('Ctrl Pts',(-24.874488562788,1.95570738879735,-0.0765455507683978));
#49905=CARTESIAN_POINT('Ctrl Pts',(-24.9115373444138,1.93040987504007,-0.722886638874206));
#49906=CARTESIAN_POINT('Ctrl Pts',(-24.9485861260396,1.55300123840625,-1.35544624822371));
#49907=CARTESIAN_POINT('Ctrl Pts',(-24.9856349076654,0.996228744102698,
-1.68468955637605));
#49908=CARTESIAN_POINT('Ctrl Pts',(-25.0226836892912,0.439456249799152,
-2.01393286452839));
#49909=CARTESIAN_POINT('Ctrl Pts',(-25.059732470917,-0.296680102174122,
-2.03985987148359));
#49910=CARTESIAN_POINT('Ctrl Pts',(-25.0967812525429,-0.875236402009141,
-1.75060328245353));
#49911=CARTESIAN_POINT('Ctrl Pts',(-25.1338300341687,-1.45379270184416,
-1.46134669342348));
#49912=CARTESIAN_POINT('Ctrl Pts',(-25.1708788157945,-1.87476894954092,
-0.856906508408172));
#49913=CARTESIAN_POINT('Ctrl Pts',(-25.2079275974203,-1.94547613788628,
-0.213946743032157));
#49914=CARTESIAN_POINT('Ctrl Pts',(-25.2119951675721,-1.95323905035499,
-0.143356460823001));
#49915=CARTESIAN_POINT('Ctrl Pts',(-25.2160627377239,-1.95677990653869,
-0.0723018731548959));
#49916=CARTESIAN_POINT('Ctrl Pts',(-25.2201303078758,-1.95626804686365,
-0.00119577595913939));
#49917=CARTESIAN_POINT('Ctrl Pts',(-25.3218696921242,-1.95648018646661,
-0.00106297053860165));
#49918=CARTESIAN_POINT('Ctrl Pts',(-25.3183439780096,-1.95688439547276,
-0.0626791772013422));
#49919=CARTESIAN_POINT('Ctrl Pts',(-25.314818263895,-1.95422593398816,-0.124260051025364));
#49920=CARTESIAN_POINT('Ctrl Pts',(-25.3112925497805,-1.94839061142824,
-0.185538403512732));
#49921=CARTESIAN_POINT('Ctrl Pts',(-25.2742437681547,-1.88707208581506,
-0.829461372285711));
#49922=CARTESIAN_POINT('Ctrl Pts',(-25.2371949865289,-1.4749597707414,-1.43997947897568));
#49923=CARTESIAN_POINT('Ctrl Pts',(-25.2001462049031,-0.900685479252096,
-1.7376467251269));
#49924=CARTESIAN_POINT('Ctrl Pts',(-25.1630974232773,-0.326411187762791,
-2.03531397127813));
#49925=CARTESIAN_POINT('Ctrl Pts',(-25.1260486416514,0.41002508014217,-2.02013035689061));
#49926=CARTESIAN_POINT('Ctrl Pts',(-25.0889998600256,0.971542137306138,
-1.69904571725378));
#49927=CARTESIAN_POINT('Ctrl Pts',(-25.0519510783998,1.53305919447011,-1.37796107761694));
#49928=CARTESIAN_POINT('Ctrl Pts',(-25.014902296774,1.91965704089309,-0.750975412730779));
#49929=CARTESIAN_POINT('Ctrl Pts',(-24.9778535151482,1.95438233152165,-0.105072242365784));
#49930=CARTESIAN_POINT('Ctrl Pts',(-24.9408047335224,1.98910762215022,0.540830927999212));
#49931=CARTESIAN_POINT('Ctrl Pts',(-24.9037559518966,1.67196035698436,1.20565160384305));
#49932=CARTESIAN_POINT('Ctrl Pts',(-24.8667071702708,1.14810500076414,1.58508844582887));
#49933=CARTESIAN_POINT('Ctrl Pts',(-24.829658388645,0.624249644543904,1.9645252878147));
#49934=CARTESIAN_POINT('Ctrl Pts',(-24.7926096070192,-0.106313802730695,
2.0585782959425));
#49935=CARTESIAN_POINT('Ctrl Pts',(-24.7555608253934,-0.709192258001544,
1.82419758114917));
#49936=CARTESIAN_POINT('Ctrl Pts',(-24.7185120437676,-1.31207071327239,
1.58981686635583));
#49937=CARTESIAN_POINT('Ctrl Pts',(-24.6814632621418,-1.78726417653948,
1.02700242864135));
#49938=CARTESIAN_POINT('Ctrl Pts',(-24.6444144805159,-1.91726736770191,
0.393365370393976));
#49939=CARTESIAN_POINT('Ctrl Pts',(-24.636899551052,-1.9436370556862,0.264839205983174));
#49940=CARTESIAN_POINT('Ctrl Pts',(-24.6293846215881,-1.95580438407669,
0.133399146235603));
#49941=CARTESIAN_POINT('Ctrl Pts',(-24.6218696921242,-1.95459134654687,
0.00173615845593911));
#49942=CARTESIAN_POINT('Origin',(-14.8,0.,0.));
#49943=CARTESIAN_POINT('',(-23.8201303078758,-1.95080280993935,0.000147472618682448));
#49944=CARTESIAN_POINT('',(-23.9218696921242,-1.95079258945597,-9.01504953382289E-6));
#49945=CARTESIAN_POINT('',(-14.8,-1.954,-2.39295984553393E-16));
#49946=CARTESIAN_POINT('Ctrl Pts',(-23.8201303078758,-1.95080280993935,
0.000147472618682448));
#49947=CARTESIAN_POINT('Ctrl Pts',(-23.8381440248809,-1.95101633693393,
0.317304418787394));
#49948=CARTESIAN_POINT('Ctrl Pts',(-23.856157741886,-1.87806774605225,0.634368765803142));
#49949=CARTESIAN_POINT('Ctrl Pts',(-23.8741714588912,-1.73142413449119,
0.912590312484417));
#49950=CARTESIAN_POINT('Ctrl Pts',(-23.911220240517,-1.42982246394235,1.48480810205256));
#49951=CARTESIAN_POINT('Ctrl Pts',(-23.9482690221428,-0.816490265778046,
1.89272053515694));
#49952=CARTESIAN_POINT('Ctrl Pts',(-23.9853178037686,-0.172161602793372,
1.94961816632452));
#49953=CARTESIAN_POINT('Ctrl Pts',(-24.0223665853944,0.472167060191294,
2.00651579749211));
#49954=CARTESIAN_POINT('Ctrl Pts',(-24.0594153670202,1.14749218799633,1.7123986267229));
#49955=CARTESIAN_POINT('Ctrl Pts',(-24.096464148646,1.54470434954386,1.20188979712753));
#49956=CARTESIAN_POINT('Ctrl Pts',(-24.1335129302718,1.94191651109139,0.691380967532166));
#49957=CARTESIAN_POINT('Ctrl Pts',(-24.1705617118977,2.06101570638141,-0.0355195208893543));
#49958=CARTESIAN_POINT('Ctrl Pts',(-24.2076104935235,1.84748791989433,-0.646095192509194));
#49959=CARTESIAN_POINT('Ctrl Pts',(-24.2446592751493,1.63396013340725,-1.25667086412904));
#49960=CARTESIAN_POINT('Ctrl Pts',(-24.2817080567751,1.08780536514307,-1.75092171894721));
#49961=CARTESIAN_POINT('Ctrl Pts',(-24.3187568384009,0.459009263121902,
-1.90261953850665));
#49962=CARTESIAN_POINT('Ctrl Pts',(-24.3558056200267,-0.169786838899253,
-2.0543173580661));
#49963=CARTESIAN_POINT('Ctrl Pts',(-24.3928544016525,-0.881224274677385,
-1.86346214236683));
#49964=CARTESIAN_POINT('Ctrl Pts',(-24.4299031832783,-1.34966430819263,
-1.41741203153137));
#49965=CARTESIAN_POINT('Ctrl Pts',(-24.4599788914775,-1.72993769745277,
-1.05531448373128));
#49966=CARTESIAN_POINT('Ctrl Pts',(-24.4900545996766,-1.95007637030861,
-0.525044100419769));
#49967=CARTESIAN_POINT('Ctrl Pts',(-24.5201303078758,-1.95487751651067,
0.00168938103890723));
#49968=CARTESIAN_POINT('Ctrl Pts',(-24.6218696921242,-1.95459134654687,
0.00173615845593911));
#49969=CARTESIAN_POINT('Ctrl Pts',(-24.5923358399623,-1.94982408010155,
-0.515702526090927));
#49970=CARTESIAN_POINT('Ctrl Pts',(-24.5628019878004,-1.73839588982394,
-1.03658435362317));
#49971=CARTESIAN_POINT('Ctrl Pts',(-24.5332681356385,-1.37020143243401,
-1.39756878486734));
#49972=CARTESIAN_POINT('Ctrl Pts',(-24.4962193540127,-0.908319386945933,
-1.85040620310102));
#49973=CARTESIAN_POINT('Ctrl Pts',(-24.4591705723869,-0.199742376912028,
-2.05162136078813));
#49974=CARTESIAN_POINT('Ctrl Pts',(-24.4221217907611,0.431200134082752,
-1.90911417108742));
#49975=CARTESIAN_POINT('Ctrl Pts',(-24.3850730091353,1.06214264507754,-1.76660698138671));
#49976=CARTESIAN_POINT('Ctrl Pts',(-24.3480242275095,1.61545065703321,-1.2803774442982));
#49977=CARTESIAN_POINT('Ctrl Pts',(-24.3109754458837,1.83786434332024,-0.672982265317476));
#49978=CARTESIAN_POINT('Ctrl Pts',(-24.2739266642579,2.06027802960727,-0.0655870863367735));
#49979=CARTESIAN_POINT('Ctrl Pts',(-24.236877882632,1.95179739022569,0.662973734536121));
#49980=CARTESIAN_POINT('Ctrl Pts',(-24.1998291010062,1.5620761213606,1.17922375525377));
#49981=CARTESIAN_POINT('Ctrl Pts',(-24.1627803193804,1.17235485249551,1.69547377597143));
#49982=CARTESIAN_POINT('Ctrl Pts',(-24.1257315377547,0.501392954146918,
1.99941299653384));
#49983=CARTESIAN_POINT('Ctrl Pts',(-24.0886827561289,-0.143697277497468,
1.95192253081919));
#49984=CARTESIAN_POINT('Ctrl Pts',(-24.051633974503,-0.788787509141855,
1.90443206510455));
#49985=CARTESIAN_POINT('Ctrl Pts',(-24.0145851928772,-1.40800607408203,
1.50551191311285));
#49986=CARTESIAN_POINT('Ctrl Pts',(-23.9775364112514,-1.71792460509043,
0.937755578551621));
#49987=CARTESIAN_POINT('Ctrl Pts',(-23.958980838209,-1.87314471455058,0.65339955727551));
#49988=CARTESIAN_POINT('Ctrl Pts',(-23.9404252651666,-1.9507792730299,0.326692269225707));
#49989=CARTESIAN_POINT('Ctrl Pts',(-23.9218696921242,-1.95079271425855,
-9.01469875197685E-6));
#49990=CARTESIAN_POINT('Origin',(-14.8,0.,0.));
#49991=CARTESIAN_POINT('',(-23.1201303078758,-1.95433609681919,-0.00176506906220647));
#49992=CARTESIAN_POINT('',(-23.2218696921242,-1.9546244457153,-0.00173153506837734));
#49993=CARTESIAN_POINT('',(-14.8,-1.954,-2.39295984553393E-16));
#49994=CARTESIAN_POINT('Ctrl Pts',(-23.1201303078758,-1.95433609681919,
-0.00176506906220647));
#49995=CARTESIAN_POINT('Ctrl Pts',(-23.1491846684594,-1.94963188416492,
0.507443655012792));
#49996=CARTESIAN_POINT('Ctrl Pts',(-23.178239029043,-1.74573314374161,1.01999030244573));
#49997=CARTESIAN_POINT('Ctrl Pts',(-23.2072933896267,-1.38813175827656,
1.37976115092541));
#49998=CARTESIAN_POINT('Ctrl Pts',(-23.2443421712525,-0.932134951840372,
1.83852435661664));
#49999=CARTESIAN_POINT('Ctrl Pts',(-23.2813909528783,-0.226214953976298,
2.04887143884446));
#50000=CARTESIAN_POINT('Ctrl Pts',(-23.3184397345041,0.406514937820749,
1.91452245149217));
#50001=CARTESIAN_POINT('Ctrl Pts',(-23.3554885161299,1.03924482961779,1.78017346413987));
#50002=CARTESIAN_POINT('Ctrl Pts',(-23.3925372977557,1.59878461534781,1.30112840720746));
#50003=CARTESIAN_POINT('Ctrl Pts',(-23.4295860793815,1.82902206445513,0.696655510044444));
#50004=CARTESIAN_POINT('Ctrl Pts',(-23.4666348610073,2.05925951356244,0.0921826128814311));
#50005=CARTESIAN_POINT('Ctrl Pts',(-23.5036836426331,1.96019462604705,-0.637718124512181));
#50006=CARTESIAN_POINT('Ctrl Pts',(-23.5407324242589,1.57717132553757,-1.15895695426579));
#50007=CARTESIAN_POINT('Ctrl Pts',(-23.5777812058847,1.19414802502809,-1.68019578401941));
#50008=CARTESIAN_POINT('Ctrl Pts',(-23.6148299875105,0.527166311524505,
-1.99277270613302));
#50009=CARTESIAN_POINT('Ctrl Pts',(-23.6518787691363,-0.118483326715247,
-1.9536151906733));
#50010=CARTESIAN_POINT('Ctrl Pts',(-23.6889275507622,-0.76413296495499,
-1.91445767521357));
#50011=CARTESIAN_POINT('Ctrl Pts',(-23.725976332388,-1.3884505279309,-1.52356572218053));
#50012=CARTESIAN_POINT('Ctrl Pts',(-23.7630251140138,-1.70567373795216,
-0.95985817264806));
#50013=CARTESIAN_POINT('Ctrl Pts',(-23.7820601786344,-1.86865789119414,
-0.670234353412065));
#50014=CARTESIAN_POINT('Ctrl Pts',(-23.8010952432551,-1.95057717632143,
-0.334991741763903));
#50015=CARTESIAN_POINT('Ctrl Pts',(-23.8201303078758,-1.95080280993935,
0.000147472618682448));
#50016=CARTESIAN_POINT('Ctrl Pts',(-23.9218696921242,-1.95079271425855,
-9.01469875197685E-6));
#50017=CARTESIAN_POINT('Ctrl Pts',(-23.9033764835408,-1.95080611031183,
-0.325612270080274));
#50018=CARTESIAN_POINT('Ctrl Pts',(-23.8848832749574,-1.87371927457768,
-0.65120956162783));
#50019=CARTESIAN_POINT('Ctrl Pts',(-23.866390066374,-1.71949699819231,-0.934869267377753));
#50020=CARTESIAN_POINT('Ctrl Pts',(-23.8293412847482,-1.41053236320917,
-1.50314526161517));
#50021=CARTESIAN_POINT('Ctrl Pts',(-23.7922925031224,-0.791984596166251,
-1.90310473295927));
#50022=CARTESIAN_POINT('Ctrl Pts',(-23.7552437214965,-0.146975027061406,
-1.95167846104324));
#50023=CARTESIAN_POINT('Ctrl Pts',(-23.7181949398707,0.498034542043438,
-2.0002521891272));
#50024=CARTESIAN_POINT('Ctrl Pts',(-23.681146158245,1.16950591321021,-1.69744017395104));
#50025=CARTESIAN_POINT('Ctrl Pts',(-23.6440973766192,1.56009359464437,-1.18184535783215));
#50026=CARTESIAN_POINT('Ctrl Pts',(-23.6070485949934,1.95068127607854,-0.666250541713246));
#50027=CARTESIAN_POINT('Ctrl Pts',(-23.5699998133675,2.06038526778009,0.0621270753483966));
#50028=CARTESIAN_POINT('Ctrl Pts',(-23.5329510317417,1.83899192144002,0.66989490724899));
#50029=CARTESIAN_POINT('Ctrl Pts',(-23.4959022501159,1.61759857509995,1.27766273914958));
#50030=CARTESIAN_POINT('Ctrl Pts',(-23.4588534684901,1.06510789071826,1.76482078588912));
#50031=CARTESIAN_POINT('Ctrl Pts',(-23.4218046868643,0.434405588214972,
1.90838734506583));
#50032=CARTESIAN_POINT('Ctrl Pts',(-23.3847559052385,-0.196296714288328,
2.05195390424254));
#50033=CARTESIAN_POINT('Ctrl Pts',(-23.3477071236127,-0.905210634913233,
1.85192897585641));
#50034=CARTESIAN_POINT('Ctrl Pts',(-23.3106583419869,-1.36785249955185,
1.39986785567408));
#50035=CARTESIAN_POINT('Ctrl Pts',(-23.281062125366,-1.73743142341591,1.03874130166394));
#50036=CARTESIAN_POINT('Ctrl Pts',(-23.2514659087451,-1.94985119779761,
0.516777199996065));
#50037=CARTESIAN_POINT('Ctrl Pts',(-23.2218696921242,-1.9546244457153,-0.00173153506837734));
#50038=CARTESIAN_POINT('Origin',(-14.8,0.,0.));
#50039=CARTESIAN_POINT('',(-22.4201303078758,-1.95665010086297,0.000936523909256006));
#50040=CARTESIAN_POINT('',(-22.5218696921242,-1.95645680992384,0.00107881945475618));
#50041=CARTESIAN_POINT('',(-14.8,-1.954,-2.39295984553393E-16));
#50042=CARTESIAN_POINT('Ctrl Pts',(-22.4201303078758,-1.95665010086297,
0.000936523909256006));
#50043=CARTESIAN_POINT('Ctrl Pts',(-22.4231765304121,-1.95696499256108,
0.0541608219567786));
#50044=CARTESIAN_POINT('Ctrl Pts',(-22.4262227529484,-1.95498151245914,
0.107361291519809));
#50045=CARTESIAN_POINT('Ctrl Pts',(-22.4292689754847,-1.95062379148406,
0.160366567698355));
#50046=CARTESIAN_POINT('Ctrl Pts',(-22.4663177571105,-1.89762429756401,
0.805027579409392));
#50047=CARTESIAN_POINT('Ctrl Pts',(-22.5033665387363,-1.49342894609215,
1.42081573797912));
#50048=CARTESIAN_POINT('Ctrl Pts',(-22.5404153203621,-0.923045802063583,
1.72587283982099));
#50049=CARTESIAN_POINT('Ctrl Pts',(-22.5774641019879,-0.352662658034998,
2.03092994166288));
#50050=CARTESIAN_POINT('Ctrl Pts',(-22.6145128836137,0.383908278550297,
2.02525598677689));
#50051=CARTESIAN_POINT('Ctrl Pts',(-22.6515616652395,0.949524180064376,
1.71144805454681));
#50052=CARTESIAN_POINT('Ctrl Pts',(-22.6886104468653,1.51514008157843,1.39764012231674));
#50053=CARTESIAN_POINT('Ctrl Pts',(-22.7256592284911,1.90980094802129,0.775698212742586));
#50054=CARTESIAN_POINT('Ctrl Pts',(-22.762708010117,1.95286283342966,0.130297220799477));
#50055=CARTESIAN_POINT('Ctrl Pts',(-22.7997567917428,1.99592471883803,-0.515103771143664));
#50056=CARTESIAN_POINT('Ctrl Pts',(-22.8368055733686,1.68738762321189,-1.18396384545577));
#50057=CARTESIAN_POINT('Ctrl Pts',(-22.8738543549944,1.16847496941632,-1.57013275164443));
#50058=CARTESIAN_POINT('Ctrl Pts',(-22.9109031366202,0.64956231562076,-1.95630165783308));
#50059=CARTESIAN_POINT('Ctrl Pts',(-22.947951918246,-0.0797258963442268,
-2.0597793958983));
#50060=CARTESIAN_POINT('Ctrl Pts',(-22.9850006998718,-0.685580283396735,
-1.83320219478284));
#50061=CARTESIAN_POINT('Ctrl Pts',(-23.0220494814976,-1.29143467044925,
-1.60662499366738));
#50062=CARTESIAN_POINT('Ctrl Pts',(-23.0590982631234,-1.77385523258929,
-1.04999285337124));
#50063=CARTESIAN_POINT('Ctrl Pts',(-23.0961470447492,-1.91202870615516,
-0.418087118645856));
#50064=CARTESIAN_POINT('Ctrl Pts',(-23.1041414657914,-1.94184390860102,
-0.281733903218062));
#50065=CARTESIAN_POINT('Ctrl Pts',(-23.1121358868336,-1.95563047934473,
-0.141875842689035));
#50066=CARTESIAN_POINT('Ctrl Pts',(-23.1201303078758,-1.95433609681919,
-0.00176506906220647));
#50067=CARTESIAN_POINT('Ctrl Pts',(-23.2218696921242,-1.9546244457153,-0.00173153506837734));
#50068=CARTESIAN_POINT('Ctrl Pts',(-23.2144171271193,-1.9558263878705,-0.13229619822038));
#50069=CARTESIAN_POINT('Ctrl Pts',(-23.2069645621144,-1.94386202774871,
-0.262641765960804));
#50070=CARTESIAN_POINT('Ctrl Pts',(-23.1995119971095,-1.91792526049931,
-0.390145061507168));
#50071=CARTESIAN_POINT('Ctrl Pts',(-23.1624632154836,-1.78898634815583,
-1.02399954652756));
#50072=CARTESIAN_POINT('Ctrl Pts',(-23.1254144338578,-1.31473871481652,
-1.58761120458983));
#50073=CARTESIAN_POINT('Ctrl Pts',(-23.088365652232,-0.71225471584897,-1.82300403006431));
#50074=CARTESIAN_POINT('Ctrl Pts',(-23.0513168706062,-0.109770716881404,
-2.05839685553878));
#50075=CARTESIAN_POINT('Ctrl Pts',(-23.0142680889804,0.620949647714409,
-1.96557084842545));
#50076=CARTESIAN_POINT('Ctrl Pts',(-22.9772193073546,1.14544147077387,-1.58701427558519));
#50077=CARTESIAN_POINT('Ctrl Pts',(-22.9401705257288,1.66993329383333,-1.20845770274493));
#50078=CARTESIAN_POINT('Ctrl Pts',(-22.903121744103,1.98819657535644,-0.544170564177744));
#50079=CARTESIAN_POINT('Ctrl Pts',(-22.8660729624772,1.95455602823469,0.101790011156494));
#50080=CARTESIAN_POINT('Ctrl Pts',(-22.8290241808514,1.92091548111294,0.747750586490741));
#50081=CARTESIAN_POINT('Ctrl Pts',(-22.7919753992255,1.53537110534632,1.37538459859205));
#50082=CARTESIAN_POINT('Ctrl Pts',(-22.7549266175997,0.974394052002249,
1.69741176657358));
#50083=CARTESIAN_POINT('Ctrl Pts',(-22.7178778359739,0.413416998658181,
2.0194389345551));
#50084=CARTESIAN_POINT('Ctrl Pts',(-22.6808290543481,-0.322992732263332,
2.03585925841686));
#50085=CARTESIAN_POINT('Ctrl Pts',(-22.6437802727223,-0.897766100098563,
1.73915683691656));
#50086=CARTESIAN_POINT('Ctrl Pts',(-22.6067314910965,-1.4725394679338,1.44245441541625));
#50087=CARTESIAN_POINT('Ctrl Pts',(-22.5696827094707,-1.88567647268274,
0.832629248553874));
#50088=CARTESIAN_POINT('Ctrl Pts',(-22.5326339278449,-1.94807628092868,
0.188810162763719));
#50089=CARTESIAN_POINT('Ctrl Pts',(-22.5290458492713,-1.95411954079142,
0.126457951284427));
#50090=CARTESIAN_POINT('Ctrl Pts',(-22.5254577706977,-1.9568730888356,0.0637868965288276));
#50091=CARTESIAN_POINT('Ctrl Pts',(-22.5218696921242,-1.95645680992384,
0.00107881945475618));
#50092=CARTESIAN_POINT('Origin',(-14.8,0.,0.));
#50093=CARTESIAN_POINT('',(-21.7201303078758,-1.95153139402954,0.00117824056209609));
#50094=CARTESIAN_POINT('',(-21.8218696921242,-1.95136622811345,0.00105513229623864));
#50095=CARTESIAN_POINT('',(-14.8,-1.954,-2.39295984553393E-16));
#50096=CARTESIAN_POINT('Ctrl Pts',(-21.7201303078758,-1.95153139402954,
0.00117824056209609));
#50097=CARTESIAN_POINT('Ctrl Pts',(-21.7342171739906,-1.95289481947734,
0.248965950362388));
#50098=CARTESIAN_POINT('Ctrl Pts',(-21.7483040401054,-1.90914502437453,
0.496290125695869));
#50099=CARTESIAN_POINT('Ctrl Pts',(-21.7623909062202,-1.8180726917492,0.724749818526905));
#50100=CARTESIAN_POINT('Ctrl Pts',(-21.799439687846,-1.57855036392325,1.32560406112565));
#50101=CARTESIAN_POINT('Ctrl Pts',(-21.8364884694718,-1.01169705569096,
1.79597228425755));
#50102=CARTESIAN_POINT('Ctrl Pts',(-21.8735372510976,-0.376972538942942,
1.92055781397538));
#50103=CARTESIAN_POINT('Ctrl Pts',(-21.9105860327234,0.257751977805092,
2.04514334369321));
#50104=CARTESIAN_POINT('Ctrl Pts',(-21.9476348143492,0.960347703068863,
1.82394617999694));
#50105=CARTESIAN_POINT('Ctrl Pts',(-21.984683595975,1.4092229235059,1.35821256208462));
#50106=CARTESIAN_POINT('Ctrl Pts',(-22.0217323776008,1.85809814394294,0.89247894417229));
#50107=CARTESIAN_POINT('Ctrl Pts',(-22.0587811592266,2.05325285955324,0.182208872043921));
#50108=CARTESIAN_POINT('Ctrl Pts',(-22.0958299408524,1.90536096557519,-0.44749324330245));
#50109=CARTESIAN_POINT('Ctrl Pts',(-22.1328787224782,1.75746907159715,-1.0771953586488));
#50110=CARTESIAN_POINT('Ctrl Pts',(-22.169927504104,1.26653056803076,-1.62632951721315));
#50111=CARTESIAN_POINT('Ctrl Pts',(-22.2069762857299,0.657257545813419,
-1.84354634615198));
#50112=CARTESIAN_POINT('Ctrl Pts',(-22.2440250673557,0.0479845235960825,
-2.0607631750908));
#50113=CARTESIAN_POINT('Ctrl Pts',(-22.2810738489815,-0.679623017272208,
-1.94606267440411));
#50114=CARTESIAN_POINT('Ctrl Pts',(-22.3181226306073,-1.19252496952225,
-1.55194549163459));
#50115=CARTESIAN_POINT('Ctrl Pts',(-22.3521251896968,-1.66325513049339,
-1.19023338647936));
#50116=CARTESIAN_POINT('Ctrl Pts',(-22.3861277487863,-1.95313521531399,
-0.593163978528166));
#50117=CARTESIAN_POINT('Ctrl Pts',(-22.4201303078758,-1.95665010086297,
0.000936523909256006));
#50118=CARTESIAN_POINT('Ctrl Pts',(-22.5218696921242,-1.95645680992384,
0.00107881945475618));
#50119=CARTESIAN_POINT('Ctrl Pts',(-22.4884089890719,-1.95257479207838,
-0.583706687029066));
#50120=CARTESIAN_POINT('Ctrl Pts',(-22.4549482860197,-1.67302767328136,
-1.17171185228325));
#50121=CARTESIAN_POINT('Ctrl Pts',(-22.4214875829675,-1.21504174052394,
-1.53438067071518));
#50122=CARTESIAN_POINT('Ctrl Pts',(-22.3844388013417,-0.707944780130278,
-1.935939413686));
#50123=CARTESIAN_POINT('Ctrl Pts',(-22.3473900197159,0.0179117524000019,
-2.06124389490971));
#50124=CARTESIAN_POINT('Ctrl Pts',(-22.3103412380901,0.630289220332262,
-1.85293981893982));
#50125=CARTESIAN_POINT('Ctrl Pts',(-22.2732924564642,1.24266668826453,-1.64463574296993));
#50126=CARTESIAN_POINT('Ctrl Pts',(-22.2362436748384,1.74156509159877,-1.10272310980644));
#50127=CARTESIAN_POINT('Ctrl Pts',(-22.1991948932126,1.89862893863049,-0.475245859818517));
#50128=CARTESIAN_POINT('Ctrl Pts',(-22.1621461115868,2.05569278566222,0.152231390169393));
#50129=CARTESIAN_POINT('Ctrl Pts',(-22.125097329961,1.87092207639144,0.865273256981712));
#50130=CARTESIAN_POINT('Ctrl Pts',(-22.0880485483352,1.42888995413977,1.33750662534367));
#50131=CARTESIAN_POINT('Ctrl Pts',(-22.0509997667094,0.986857831888117,
1.80973999370563));
#50132=CARTESIAN_POINT('Ctrl Pts',(-22.0139509850836,0.287564296655561,
2.04116486361724));
#50133=CARTESIAN_POINT('Ctrl Pts',(-21.9769022034578,-0.348910414746983,
1.92585357604385));
#50134=CARTESIAN_POINT('Ctrl Pts',(-21.939853421832,-0.985385126149545,
1.81054228847046));
#50135=CARTESIAN_POINT('Ctrl Pts',(-21.9028046402062,-1.5590410137221,1.34849484341207));
#50136=CARTESIAN_POINT('Ctrl Pts',(-21.8657558585804,-1.80730463285085,
0.751199333037264));
#50137=CARTESIAN_POINT('Ctrl Pts',(-21.8511271364283,-1.90533159474615,
0.515357027824685));
#50138=CARTESIAN_POINT('Ctrl Pts',(-21.8364984142762,-1.95262770521904,
0.258428636149302));
#50139=CARTESIAN_POINT('Ctrl Pts',(-21.8218696921242,-1.95136622811345,
0.00105513229623864));
#50140=CARTESIAN_POINT('Origin',(-14.8,0.,0.));
#50141=CARTESIAN_POINT('',(-21.0201303078758,-1.95236395582867,-0.0015719214144061));
#50142=CARTESIAN_POINT('',(-21.1218696921242,-1.95260904431355,-0.00164165242779367));
#50143=CARTESIAN_POINT('',(-14.8,-1.954,-2.39295984553393E-16));
#50144=CARTESIAN_POINT('Ctrl Pts',(-21.0201303078758,-1.95236395582867,
-0.0015719214144061));
#50145=CARTESIAN_POINT('Ctrl Pts',(-21.045257817569,-1.94902866231054,0.43994669109059));
#50146=CARTESIAN_POINT('Ctrl Pts',(-21.0703853272623,-1.80070766903344,
0.883494201581255));
#50147=CARTESIAN_POINT('Ctrl Pts',(-21.0955128369556,-1.52600533535847,
1.22554409483969));
#50148=CARTESIAN_POINT('Ctrl Pts',(-21.1325616185814,-1.12097567278332,
1.72987309342132));
#50149=CARTESIAN_POINT('Ctrl Pts',(-21.1696104002072,-0.441199667669119,
2.01355164611284));
#50150=CARTESIAN_POINT('Ctrl Pts',(-21.206659181833,0.202175995891084,1.94673456809716));
#50151=CARTESIAN_POINT('Ctrl Pts',(-21.2437079634588,0.845551659451288,
1.87991749008148));
#50152=CARTESIAN_POINT('Ctrl Pts',(-21.2807567450847,1.4525269814575,1.46260478135859));
#50153=CARTESIAN_POINT('Ctrl Pts',(-21.3178055267105,1.74527756483232,0.885808576178816));
#50154=CARTESIAN_POINT('Ctrl Pts',(-21.3548543083363,2.03802814820715,0.309012370999024));
#50155=CARTESIAN_POINT('Ctrl Pts',(-21.391903089962,2.01655399295056,-0.427267330637652));
#50156=CARTESIAN_POINT('Ctrl Pts',(-21.4289518715879,1.6906842371191,-0.986021004997343));
#50157=CARTESIAN_POINT('Ctrl Pts',(-21.4660006532137,1.36481448128766,-1.54477467935702));
#50158=CARTESIAN_POINT('Ctrl Pts',(-21.5030494348395,0.734549124881337,
-1.9260023264397));
#50159=CARTESIAN_POINT('Ctrl Pts',(-21.5400982164653,0.0883728661966189,
-1.95520864576116));
#50160=CARTESIAN_POINT('Ctrl Pts',(-21.5771469980911,-0.557803392488099,
-1.98441496508261));
#50161=CARTESIAN_POINT('Ctrl Pts',(-21.6141957797169,-1.21989055345123,
-1.66159995664285));
#50162=CARTESIAN_POINT('Ctrl Pts',(-21.6512445613427,-1.59483846022299,
-1.13452232139017));
#50163=CARTESIAN_POINT('Ctrl Pts',(-21.6742064768537,-1.82722186875934,
-0.807852682138515));
#50164=CARTESIAN_POINT('Ctrl Pts',(-21.6971683923647,-1.94930897921542,
-0.402721421061367));
#50165=CARTESIAN_POINT('Ctrl Pts',(-21.7201303078758,-1.95153139402954,
0.00117824056209609));
#50166=CARTESIAN_POINT('Ctrl Pts',(-21.8218696921242,-1.95136622811345,
0.00105513229623864));
#50167=CARTESIAN_POINT('Ctrl Pts',(-21.7994496326504,-1.94943288141113,
-0.393396905507871));
#50168=CARTESIAN_POINT('Ctrl Pts',(-21.7770295731767,-1.83344361255741,
-0.788894458182419));
#50169=CARTESIAN_POINT('Ctrl Pts',(-21.7546095137029,-1.61122196613715,
-1.11113196773242));
#50170=CARTESIAN_POINT('Ctrl Pts',(-21.7175607320771,-1.24400432960976,
-1.6436241824361));
#50171=CARTESIAN_POINT('Ctrl Pts',(-21.6805119504513,-0.586697705870041,
-1.97606503615226));
#50172=CARTESIAN_POINT('Ctrl Pts',(-21.6434631688255,0.0598358933747139,
-1.95628989154058));
#50173=CARTESIAN_POINT('Ctrl Pts',(-21.6064143871997,0.706369492619478,
-1.9365147469289));
#50174=CARTESIAN_POINT('Ctrl Pts',(-21.5693656055739,1.34213006736929,-1.56452360398938));
#50175=CARTESIAN_POINT('Ctrl Pts',(-21.5323168239481,1.67611765113184,-1.01058403581497));
#50176=CARTESIAN_POINT('Ctrl Pts',(-21.4952680423223,2.0101052348944,-0.456644467640561));
#50177=CARTESIAN_POINT('Ctrl Pts',(-21.4582192606965,2.04231982766971,0.279243525768716));
#50178=CARTESIAN_POINT('Ctrl Pts',(-21.4211704790707,1.75801618448586,0.860249713144712));
#50179=CARTESIAN_POINT('Ctrl Pts',(-21.3841216974449,1.47371254130201,1.4412559005207));
#50180=CARTESIAN_POINT('Ctrl Pts',(-21.347072915819,0.872890662159003,1.86738028186339));
#50181=CARTESIAN_POINT('Ctrl Pts',(-21.3100241341932,0.230558393787886,
1.94357744917298));
#50182=CARTESIAN_POINT('Ctrl Pts',(-21.2729753525674,-0.411773874583241,
2.01977461648257));
#50183=CARTESIAN_POINT('Ctrl Pts',(-21.2359265709416,-1.09561653218248,
1.74604456975904));
#50184=CARTESIAN_POINT('Ctrl Pts',(-21.1988777893158,-1.50796150906827,
1.24767886936036));
#50185=CARTESIAN_POINT('Ctrl Pts',(-21.1732084235853,-1.79365603273008,
0.902384614874454));
#50186=CARTESIAN_POINT('Ctrl Pts',(-21.1475390578547,-1.94901931302901,
0.449255022826248));
#50187=CARTESIAN_POINT('Ctrl Pts',(-21.1218696921242,-1.95260904431355,
-0.00164165242779367));
#50188=CARTESIAN_POINT('Origin',(-14.8,0.,0.));
#50189=CARTESIAN_POINT('',(-20.3201303078758,-1.95715316974838,-0.000285904946947801));
#50190=CARTESIAN_POINT('',(-20.4218696921242,-1.95719692349308,-0.00011048144072509));
#50191=CARTESIAN_POINT('',(-14.8,-1.954,-2.39295984553393E-16));
#50192=CARTESIAN_POINT('Ctrl Pts',(-20.3201303078758,-1.95715316974838,
-0.000285904946947801));
#50193=CARTESIAN_POINT('Ctrl Pts',(-20.3562984611475,-1.95586198679419,
0.631220005407538));
#50194=CARTESIAN_POINT('Ctrl Pts',(-20.3924666144193,-1.62233085199216,
1.26389725429215));
#50195=CARTESIAN_POINT('Ctrl Pts',(-20.4286347676911,-1.10004748061862,
1.618810103849));
#50196=CARTESIAN_POINT('Ctrl Pts',(-20.4656835493169,-0.565047464792199,
1.98236443189616));
#50197=CARTESIAN_POINT('Ctrl Pts',(-20.5027323309427,0.168008229422955,
2.05446358282673));
#50198=CARTESIAN_POINT('Ctrl Pts',(-20.5397811125685,0.763585769125162,
1.8021063745319));
#50199=CARTESIAN_POINT('Ctrl Pts',(-20.5768298941943,1.35916330882738,1.54974916623707));
#50200=CARTESIAN_POINT('Ctrl Pts',(-20.6138786758201,1.81726269401663,0.972935598716842));
#50201=CARTESIAN_POINT('Ctrl Pts',(-20.6509274574459,1.92820293622857,0.335684448043843));
#50202=CARTESIAN_POINT('Ctrl Pts',(-20.6879762390717,2.03914317844051,-0.301566702629146));
#50203=CARTESIAN_POINT('Ctrl Pts',(-20.7250250206975,1.80292427767512,-0.999255436454915));
#50204=CARTESIAN_POINT('Ctrl Pts',(-20.7620738023233,1.32766821402631,-1.43803606540419));
#50205=CARTESIAN_POINT('Ctrl Pts',(-20.7991225839491,0.852412150377491,
-1.87681669435347));
#50206=CARTESIAN_POINT('Ctrl Pts',(-20.836171365575,0.138118923845247,-2.05668921842628));
#50207=CARTESIAN_POINT('Ctrl Pts',(-20.8732201472008,-0.488265578640686,
-1.89532248882707));
#50208=CARTESIAN_POINT('Ctrl Pts',(-20.9102689288266,-1.11465008112663,
-1.73395575922787));
#50209=CARTESIAN_POINT('Ctrl Pts',(-20.9473177104524,-1.65312585956624,
-1.23134977595664));
#50210=CARTESIAN_POINT('Ctrl Pts',(-20.9843664920782,-1.85722208876799,
-0.617557062085145));
#50211=CARTESIAN_POINT('Ctrl Pts',(-20.9962877640107,-1.92289460327309,
-0.420055564568475));
#50212=CARTESIAN_POINT('Ctrl Pts',(-21.0082090359432,-1.95394632278384,
-0.211042080104704));
#50213=CARTESIAN_POINT('Ctrl Pts',(-21.0201303078758,-1.95236395582867,
-0.0015719214144061));
#50214=CARTESIAN_POINT('Ctrl Pts',(-21.1218696921242,-1.95260904431355,
-0.00164165242779367));
#50215=CARTESIAN_POINT('Ctrl Pts',(-21.1104902762289,-1.9542003982125,-0.201527416936542));
#50216=CARTESIAN_POINT('Ctrl Pts',(-21.0991108603336,-1.92596501442508,
-0.40097436569691));
#50217=CARTESIAN_POINT('Ctrl Pts',(-21.0877314444384,-1.8660348537741,-0.590393426775798));
#50218=CARTESIAN_POINT('Ctrl Pts',(-21.0506826628126,-1.67091592542181,
-1.20709866843947));
#50219=CARTESIAN_POINT('Ctrl Pts',(-21.0136338811868,-1.13983077254491,
-1.717507797693));
#50220=CARTESIAN_POINT('Ctrl Pts',(-20.976585099561,-0.515867387431277,
-1.88799663995057));
#50221=CARTESIAN_POINT('Ctrl Pts',(-20.9395363179352,0.108095997682367,
-2.05848548220813));
#50222=CARTESIAN_POINT('Ctrl Pts',(-20.9024875363094,0.824937615032749,
-1.88905403746973));
#50223=CARTESIAN_POINT('Ctrl Pts',(-20.8654387546836,1.30654512970301,-1.45725436967234));
#50224=CARTESIAN_POINT('Ctrl Pts',(-20.8283899730577,1.78815264437328,-1.02545470187495));
#50225=CARTESIAN_POINT('Ctrl Pts',(-20.7913411914319,2.03452605636343,-0.331286811018583));
#50226=CARTESIAN_POINT('Ctrl Pts',(-20.7542924098061,1.9328954685122,0.307515173096853));
#50227=CARTESIAN_POINT('Ctrl Pts',(-20.7172436281803,1.83126488066097,0.94631715721227));
#50228=CARTESIAN_POINT('Ctrl Pts',(-20.6801948465545,1.38163029296839,1.52975323458676));
#50229=CARTESIAN_POINT('Ctrl Pts',(-20.6431460649287,0.789798191632178,
1.7907733777266));
#50230=CARTESIAN_POINT('Ctrl Pts',(-20.6060972833029,0.197966090295949,
2.05179352086645));
#50231=CARTESIAN_POINT('Ctrl Pts',(-20.5690485016771,-0.536063524683919,
1.99039772977163));
#50232=CARTESIAN_POINT('Ctrl Pts',(-20.5319997200513,-1.07631103795058,
1.63468805081139));
#50233=CARTESIAN_POINT('Ctrl Pts',(-20.4952897107422,-1.61161855336392,
1.28223096442644));
#50234=CARTESIAN_POINT('Ctrl Pts',(-20.4585797014332,-1.95667163342788,
0.640817766737759));
#50235=CARTESIAN_POINT('Ctrl Pts',(-20.4218696921242,-1.95719692349308,
-0.00011048144072509));
#50236=CARTESIAN_POINT('Origin',(-14.8,0.,0.));
#50237=CARTESIAN_POINT('',(-19.6201303078758,-1.95320120599967,0.00175035074057674));
#50238=CARTESIAN_POINT('',(-19.7218696921242,-1.95293192181713,0.00171055984299888));
#50239=CARTESIAN_POINT('',(-14.8,-1.954,-2.39295984553393E-16));
#50240=CARTESIAN_POINT('Ctrl Pts',(-19.6201303078758,-1.95320120599967,
0.00175035074057674));
#50241=CARTESIAN_POINT('Ctrl Pts',(-19.6302903231002,-1.95475089717379,
0.180079640908608));
#50242=CARTESIAN_POINT('Ctrl Pts',(-19.6404503383247,-1.93233867926486,
0.358026458337075));
#50243=CARTESIAN_POINT('Ctrl Pts',(-19.6506103535491,-1.88441164171196,
0.528813177331473));
#50244=CARTESIAN_POINT('Ctrl Pts',(-19.6876591351749,-1.70964434963189,
1.15159175756291));
#50245=CARTESIAN_POINT('Ctrl Pts',(-19.7247079168007,-1.19560222383916,
1.67916130870918));
#50246=CARTESIAN_POINT('Ctrl Pts',(-19.7617566984265,-0.57757233201673,
1.8700429976949));
#50247=CARTESIAN_POINT('Ctrl Pts',(-19.7988054800523,0.0404575598057107,
2.06092468668063));
#50248=CARTESIAN_POINT('Ctrl Pts',(-19.8358542616782,0.762475217657862,
1.9151185135058));
#50249=CARTESIAN_POINT('Ctrl Pts',(-19.872903043304,1.25799913232614,1.49936279632572));
#50250=CARTESIAN_POINT('Ctrl Pts',(-19.9099518249298,1.7535230469944,1.08360707914564));
#50251=CARTESIAN_POINT('Ctrl Pts',(-19.9470006065556,2.02255321847879,0.397901817960317));
#50252=CARTESIAN_POINT('Ctrl Pts',(-19.9840493881814,1.94194931062656,-0.243892367441067));
#50253=CARTESIAN_POINT('Ctrl Pts',(-20.0210981698072,1.86134540277432,-0.885686552842469));
#50254=CARTESIAN_POINT('Ctrl Pts',(-20.058146951433,1.43110741558543,-1.48356966245993));
#50255=CARTESIAN_POINT('Ctrl Pts',(-20.0951957330588,0.848163634373811,
-1.76387898146806));
#50256=CARTESIAN_POINT('Ctrl Pts',(-20.1322445146846,0.265219853162208,
-2.04418830047618));
#50257=CARTESIAN_POINT('Ctrl Pts',(-20.1692932963104,-0.470429722072116,
-2.00692382887498));
#50258=CARTESIAN_POINT('Ctrl Pts',(-20.2063420779362,-1.0220639886916,-1.66914223928304));
#50259=CARTESIAN_POINT('Ctrl Pts',(-20.243390859562,-1.5736982553111,-1.33136064969109));
#50260=CARTESIAN_POINT('Ctrl Pts',(-20.2804396411878,-1.94131721331576,
-0.693061942108369));
#50261=CARTESIAN_POINT('Ctrl Pts',(-20.3174884228136,-1.95665452359924,
-0.046407835735133));
#50262=CARTESIAN_POINT('Ctrl Pts',(-20.3183690511677,-1.95701908269451,
-0.0310372373959162));
#50263=CARTESIAN_POINT('Ctrl Pts',(-20.3192496795217,-1.95718460769079,
-0.0156619183757309));
#50264=CARTESIAN_POINT('Ctrl Pts',(-20.3201303078758,-1.95715316974838,
-0.000285904946947801));
#50265=CARTESIAN_POINT('Ctrl Pts',(-20.4218696921242,-1.95719692349308,
-0.00011048144072509));
#50266=CARTESIAN_POINT('Ctrl Pts',(-20.4215309198074,-1.95720177104653,
-0.00602518295147257));
#50267=CARTESIAN_POINT('Ctrl Pts',(-20.4211921474906,-1.95717727785765,
-0.0119398431628558));
#50268=CARTESIAN_POINT('Ctrl Pts',(-20.4208533751739,-1.95712332268219,
-0.01785423460159));
#50269=CARTESIAN_POINT('Ctrl Pts',(-20.383804593548,-1.9512226825937,-0.664663274228705));
#50270=CARTESIAN_POINT('Ctrl Pts',(-20.3467558119222,-1.59295599086327,
-1.30825778665728));
#50271=CARTESIAN_POINT('Ctrl Pts',(-20.3097070302964,-1.04630887262954,
-1.65405205992329));
#50272=CARTESIAN_POINT('Ctrl Pts',(-20.2726582486706,-0.499661754395827,
-1.99984633318929));
#50273=CARTESIAN_POINT('Ctrl Pts',(-20.2356094670448,0.235365790341175,
-2.04784036729274));
#50274=CARTESIAN_POINT('Ctrl Pts',(-20.198560685419,0.822337374387208,-1.77606636040598));
#50275=CARTESIAN_POINT('Ctrl Pts',(-20.1615119037932,1.40930895843324,-1.50429235351922));
#50276=CARTESIAN_POINT('Ctrl Pts',(-20.1244631221674,1.8482245817883,-0.91275030564226));
#50277=CARTESIAN_POINT('Ctrl Pts',(-20.0874143405416,1.93818403647784,-0.272200504448977));
#50278=CARTESIAN_POINT('Ctrl Pts',(-20.0503655589158,2.02814349116737,0.368349296744315));
#50279=CARTESIAN_POINT('Ctrl Pts',(-20.01331677729,1.76914677719136,1.05790685125393));
#50280=CARTESIAN_POINT('Ctrl Pts',(-19.9762679956642,1.279741722273,1.48084826979456));
#50281=CARTESIAN_POINT('Ctrl Pts',(-19.9392192140384,0.790336667354642,
1.90378968833517));
#50282=CARTESIAN_POINT('Ctrl Pts',(-19.9021704324125,0.070523271493932,
2.06011497090681));
#50283=CARTESIAN_POINT('Ctrl Pts',(-19.8651216507867,-0.550225889632995,
1.87827099862011));
#50284=CARTESIAN_POINT('Ctrl Pts',(-19.8280728691609,-1.17097505075993,
1.6964270263334));
#50285=CARTESIAN_POINT('Ctrl Pts',(-19.7910240875351,-1.69265997715308,
1.17641379918833));
#50286=CARTESIAN_POINT('Ctrl Pts',(-19.7539753059093,-1.87649534281188,
0.556251473962188));
#50287=CARTESIAN_POINT('Ctrl Pts',(-19.7432734346476,-1.92959782905559,
0.37711205089107));
#50288=CARTESIAN_POINT('Ctrl Pts',(-19.7325715633859,-1.95451032397123,
0.189616239253742));
#50289=CARTESIAN_POINT('Ctrl Pts',(-19.7218696921242,-1.95293192181713,
0.00171055984299888));
#50290=CARTESIAN_POINT('Origin',(-14.8,0.,0.));
#50291=CARTESIAN_POINT('',(-18.9201303078757,-1.95106696972105,-0.00075047970158143));
#50292=CARTESIAN_POINT('',(-19.0218696921242,-1.95118717389941,-0.00089009348416731));
#50293=CARTESIAN_POINT('',(-14.8,-1.954,-2.39295984553393E-16));
#50294=CARTESIAN_POINT('Ctrl Pts',(-18.9201303078757,-1.95106696972105,
-0.00075047970158143));
#50295=CARTESIAN_POINT('Ctrl Pts',(-18.9413309666787,-1.94977826652978,
0.372390924373151));
#50296=CARTESIAN_POINT('Ctrl Pts',(-18.9625316254816,-1.84685029020357,
0.74619065026788));
#50297=CARTESIAN_POINT('Ctrl Pts',(-18.9837322842846,-1.64683197629078,
1.05763654144758));
#50298=CARTESIAN_POINT('Ctrl Pts',(-19.0207810659104,-1.29729402550354,
1.60189749662951));
#50299=CARTESIAN_POINT('Ctrl Pts',(-19.0578298475362,-0.651255759954327,
1.95573855958341));
#50300=CARTESIAN_POINT('Ctrl Pts',(-19.094878629162,-0.0044214448872297,
1.95719980144187));
#50301=CARTESIAN_POINT('Ctrl Pts',(-19.1319274107878,0.642412870179858,
1.95866104330033));
#50302=CARTESIAN_POINT('Ctrl Pts',(-19.1689761924136,1.29004323476483,1.60774246406337));
#50303=CARTESIAN_POINT('Ctrl Pts',(-19.2060249740394,1.64203664896396,1.06506631502371));
#50304=CARTESIAN_POINT('Ctrl Pts',(-19.2430737556652,1.99403006316311,0.522390165984023));
#50305=CARTESIAN_POINT('Ctrl Pts',(-19.280122537291,2.05038652697639,-0.212043552858375));
#50306=CARTESIAN_POINT('Ctrl Pts',(-19.3171713189168,1.78531059203435,-0.802070259957907));
#50307=CARTESIAN_POINT('Ctrl Pts',(-19.3542201005426,1.52023465709232,-1.39209696705742));
#50308=CARTESIAN_POINT('Ctrl Pts',(-19.3912688821684,0.933726323394989,
-1.83771666241408));
#50309=CARTESIAN_POINT('Ctrl Pts',(-19.4283176637943,0.294241849842236,
-1.93496055405282));
#50310=CARTESIAN_POINT('Ctrl Pts',(-19.4653664454201,-0.345242623710509,
-2.03220444569156));
#50311=CARTESIAN_POINT('Ctrl Pts',(-19.5024152270459,-1.03770323711868,
-1.78107253361239));
#50312=CARTESIAN_POINT('Ctrl Pts',(-19.5394640086717,-1.46618731463906,
-1.29651277291452));
#50313=CARTESIAN_POINT('Ctrl Pts',(-19.566352775073,-1.77716672506918,-0.944835507397405));
#50314=CARTESIAN_POINT('Ctrl Pts',(-19.5932415414744,-1.94909990466747,
-0.47020313750915));
#50315=CARTESIAN_POINT('Ctrl Pts',(-19.6201303078758,-1.95320120599967,
0.00175035074057674));
#50316=CARTESIAN_POINT('Ctrl Pts',(-19.7218696921242,-1.95293192181713,
0.00171055984299888));
#50317=CARTESIAN_POINT('Ctrl Pts',(-19.6955227817601,-1.94904605746169,
-0.460893967091506));
#50318=CARTESIAN_POINT('Ctrl Pts',(-19.669175871396,-1.78460047078708,-0.925982677770864));
#50319=CARTESIAN_POINT('Ctrl Pts',(-19.6428289610319,-1.48494804682834,
-1.27498226344545));
#50320=CARTESIAN_POINT('Ctrl Pts',(-19.6057801794061,-1.06357958026152,
-1.76574225231978));
#50321=CARTESIAN_POINT('Ctrl Pts',(-19.5687313977803,-0.374856842203399,
-2.0269508067612));
#50322=CARTESIAN_POINT('Ctrl Pts',(-19.5316826161545,0.265978389769201,
-1.93904769669433));
#50323=CARTESIAN_POINT('Ctrl Pts',(-19.4946338345287,0.9068136217418,-1.85114458662745));
#50324=CARTESIAN_POINT('Ctrl Pts',(-19.4575850529028,1.49976134762888,-1.41412981205228));
#50325=CARTESIAN_POINT('Ctrl Pts',(-19.420536271277,1.77341787362209,-0.828033525527501));
#50326=CARTESIAN_POINT('Ctrl Pts',(-19.3834874896512,2.0470743996153,-0.241937239002725));
#50327=CARTESIAN_POINT('Ctrl Pts',(-19.3464387080254,2.00143972571464,0.493240559471652));
#50328=CARTESIAN_POINT('Ctrl Pts',(-19.3093899263996,1.65740172874576,1.04099470864667));
#50329=CARTESIAN_POINT('Ctrl Pts',(-19.2723411447738,1.31336373177689,1.58874885782166));
#50330=CARTESIAN_POINT('Ctrl Pts',(-19.235292363148,0.670922411739813,1.94907935769732));
#50331=CARTESIAN_POINT('Ctrl Pts',(-19.1982435815222,0.0241356420369828,
1.95705593805166));
#50332=CARTESIAN_POINT('Ctrl Pts',(-19.1611947998964,-0.622651127665885,
1.965032518406));
#50333=CARTESIAN_POINT('Ctrl Pts',(-19.1241460182706,-1.27378334703449,
1.62065517923901));
#50334=CARTESIAN_POINT('Ctrl Pts',(-19.0870972366448,-1.63122514919733,
1.08155211918147));
#50335=CARTESIAN_POINT('Ctrl Pts',(-19.0653547218046,-1.84099409022561,
0.765173124533693));
#50336=CARTESIAN_POINT('Ctrl Pts',(-19.0436122069644,-1.94961406105061,
0.381729271837227));
#50337=CARTESIAN_POINT('Ctrl Pts',(-19.0218696921242,-1.95118717389941,
-0.00089009348416731));
#50338=CARTESIAN_POINT('Origin',(-14.8,0.,0.));
#50339=CARTESIAN_POINT('',(-18.2201303078757,-1.955948595666,-0.0013580538473823));
#50340=CARTESIAN_POINT('',(-18.3218696921242,-1.9561856368743,-0.00124144867156942));
#50341=CARTESIAN_POINT('',(-14.8,-1.954,-2.39295984553393E-16));
#50342=CARTESIAN_POINT('Ctrl Pts',(-18.2201303078757,-1.955948595666,-0.0013580538473823));
#50343=CARTESIAN_POINT('Ctrl Pts',(-18.2523716102572,-1.95148176910926,
0.562500491288516));
#50344=CARTESIAN_POINT('Ctrl Pts',(-18.2846129126386,-1.69434583291202,
1.12991216153671));
#50345=CARTESIAN_POINT('Ctrl Pts',(-18.31685421502,-1.26476057883309,1.49366371388234));
#50346=CARTESIAN_POINT('Ctrl Pts',(-18.3539029966458,-0.771120152036655,
1.91165401928226));
#50347=CARTESIAN_POINT('Ctrl Pts',(-18.3909517782716,-0.0497686319888131,
2.06072085969571));
#50348=CARTESIAN_POINT('Ctrl Pts',(-18.4280005598974,0.569117376311475,
1.87263344622468));
#50349=CARTESIAN_POINT('Ctrl Pts',(-18.4650493415233,1.18800338461177,1.68454603275365));
#50350=CARTESIAN_POINT('Ctrl Pts',(-18.5020981231491,1.70442388116452,1.15930436539812));
#50351=CARTESIAN_POINT('Ctrl Pts',(-18.5391469047749,1.8820031717834,0.537321759596808));
#50352=CARTESIAN_POINT('Ctrl Pts',(-18.5761956864007,2.05958246240227,-0.0846608462045072));
#50353=CARTESIAN_POINT('Ctrl Pts',(-18.6132444680265,1.89832054708729,-0.803384390451597));
#50354=CARTESIAN_POINT('Ctrl Pts',(-18.6502932496523,1.47203013744235,-1.28987514372533));
#50355=CARTESIAN_POINT('Ctrl Pts',(-18.6873420312781,1.04573972779741,-1.77636589699906));
#50356=CARTESIAN_POINT('Ctrl Pts',(-18.7243908129039,0.354420823822513,
-2.03062385929941));
#50357=CARTESIAN_POINT('Ctrl Pts',(-18.7614395945297,-0.285496481327623,
-1.93627022160868));
#50358=CARTESIAN_POINT('Ctrl Pts',(-18.7984883761555,-0.92541378647776,
-1.84191658391795));
#50359=CARTESIAN_POINT('Ctrl Pts',(-18.8355371577813,-1.51392949280315,
-1.39895134623613));
#50360=CARTESIAN_POINT('Ctrl Pts',(-18.8725859394071,-1.78166852795321,
-0.810128303690238));
#50361=CARTESIAN_POINT('Ctrl Pts',(-18.88843406223,-1.89619756041618,-0.558251197623553));
#50362=CARTESIAN_POINT('Ctrl Pts',(-18.9042821850529,-1.95203031367405,
-0.279684774010249));
#50363=CARTESIAN_POINT('Ctrl Pts',(-18.9201303078757,-1.95106696972105,
-0.00075047970158143));
#50364=CARTESIAN_POINT('Ctrl Pts',(-19.0218696921242,-1.95118717389941,
-0.00089009348416731));
#50365=CARTESIAN_POINT('Ctrl Pts',(-19.0065634253386,-1.95229461179813,
-0.270245967263792));
#50366=CARTESIAN_POINT('Ctrl Pts',(-18.991257158553,-1.90035112825074,-0.539193236664031));
#50367=CARTESIAN_POINT('Ctrl Pts',(-18.9759508917673,-1.7932990566245,-0.784046533943919));
#50368=CARTESIAN_POINT('Ctrl Pts',(-18.9389021101415,-1.53417977693178,
-1.37671334606378));
#50369=CARTESIAN_POINT('Ctrl Pts',(-18.9018533285157,-0.952189832589261,
-1.82821818935548));
#50370=CARTESIAN_POINT('Ctrl Pts',(-18.8648045468899,-0.31371732790678,
-1.93189852529858));
#50371=CARTESIAN_POINT('Ctrl Pts',(-18.8277557652641,0.32475517677571,-2.03557886124168));
#50372=CARTESIAN_POINT('Ctrl Pts',(-18.7907069836383,1.01971024179817,-1.7914346898362));
#50373=CARTESIAN_POINT('Ctrl Pts',(-18.7536582020125,1.45305343245182,-1.31121554151855));
#50374=CARTESIAN_POINT('Ctrl Pts',(-18.7166094203867,1.88639662310545,-0.830996393200911));
#50375=CARTESIAN_POINT('Ctrl Pts',(-18.6795606387609,2.05812793939028,-0.114702267971124));
#50376=CARTESIAN_POINT('Ctrl Pts',(-18.6425118571351,1.88964262148106,0.509805097034146));
#50377=CARTESIAN_POINT('Ctrl Pts',(-18.6054630755093,1.72115730357184,1.13431246203942));
#50378=CARTESIAN_POINT('Ctrl Pts',(-18.5684142938834,1.21245535146857,1.66703306682015));
#50379=CARTESIAN_POINT('Ctrl Pts',(-18.5313655122576,0.596379531608711,
1.86413034097886));
#50380=CARTESIAN_POINT('Ctrl Pts',(-18.4943167306318,-0.0196962882511521,
2.06122761513757));
#50381=CARTESIAN_POINT('Ctrl Pts',(-18.457267949006,-0.743145975867633,
1.92270155867423));
#50382=CARTESIAN_POINT('Ctrl Pts',(-18.4202191673802,-1.24283255418279,
1.51195823888865));
#50383=CARTESIAN_POINT('Ctrl Pts',(-18.3874360089615,-1.6849875600356,1.14850598132321));
#50384=CARTESIAN_POINT('Ctrl Pts',(-18.3546528505428,-1.95193929414975,
0.571911551633334));
#50385=CARTESIAN_POINT('Ctrl Pts',(-18.3218696921242,-1.9561856368743,-0.00124144867156942));
#50386=CARTESIAN_POINT('Origin',(-14.8,0.,0.));
#50387=CARTESIAN_POINT('',(-17.5201303078758,-1.95526004210547,0.001601638831479));
#50388=CARTESIAN_POINT('',(-17.6218696921242,-1.95498100154377,0.00166857518573596));
#50389=CARTESIAN_POINT('',(-14.8,-1.954,-2.39295984553393E-16));
#50390=CARTESIAN_POINT('Ctrl Pts',(-17.5201303078758,-1.95526004210547,
0.001601638831479));
#50391=CARTESIAN_POINT('Ctrl Pts',(-17.5263634722099,-1.95622626701164,
0.110711495172787));
#50392=CARTESIAN_POINT('Ctrl Pts',(-17.532596636544,-1.94788014460328,0.219673489375271));
#50393=CARTESIAN_POINT('Ctrl Pts',(-17.5388298008781,-1.92969991498865,
0.32696918819943));
#50394=CARTESIAN_POINT('Ctrl Pts',(-17.5758785825039,-1.82163997612026,
0.964715074887744));
#50395=CARTESIAN_POINT('Ctrl Pts',(-17.6129273641297,-1.36615137395922,
1.54359249860331));
#50396=CARTESIAN_POINT('Ctrl Pts',(-17.6499761457555,-0.771720090856103,
1.79863801619671));
#50397=CARTESIAN_POINT('Ctrl Pts',(-17.6870249273813,-0.177288807752993,
2.0536835337901));
#50398=CARTESIAN_POINT('Ctrl Pts',(-17.7240737090071,0.556085156292187,
1.98489714526133));
#50399=CARTESIAN_POINT('Ctrl Pts',(-17.7611224906329,1.09272229009327,1.6237637170082));
#50400=CARTESIAN_POINT('Ctrl Pts',(-17.7981712722587,1.62935942389434,1.26263028875509));
#50401=CARTESIAN_POINT('Ctrl Pts',(-17.8352200538845,1.96925972745132,0.609149820777612));
#50402=CARTESIAN_POINT('Ctrl Pts',(-17.8722688355103,1.95684422831105,-0.0375669810430752));
#50403=CARTESIAN_POINT('Ctrl Pts',(-17.9093176171361,1.94442872917078,-0.68428378286379));
#50404=CARTESIAN_POINT('Ctrl Pts',(-17.9463663987619,1.57969742733327,-1.3242369185277));
#50405=CARTESIAN_POINT('Ctrl Pts',(-17.9834151803877,1.0295949255763,-1.66450740495995));
#50406=CARTESIAN_POINT('Ctrl Pts',(-18.0204639620136,0.479492423819356,
-2.00477789139219));
#50407=CARTESIAN_POINT('Ctrl Pts',(-18.0575127436394,-0.255981277857039,
-2.04536572859275));
#50408=CARTESIAN_POINT('Ctrl Pts',(-18.0945615252652,-0.840185577559581,
-1.76769307494255));
#50409=CARTESIAN_POINT('Ctrl Pts',(-18.131610306891,-1.42438987726213,-1.49002042129235));
#50410=CARTESIAN_POINT('Ctrl Pts',(-18.1686590885168,-1.85732477499085,
-0.894087276791399));
#50411=CARTESIAN_POINT('Ctrl Pts',(-18.2057078701426,-1.9408275570827,-0.252663819347713));
#50412=CARTESIAN_POINT('Ctrl Pts',(-18.210515349387,-1.95166294421661,-0.169432203537293));
#50413=CARTESIAN_POINT('Ctrl Pts',(-18.2153228286314,-1.95661464121546,
-0.0854346280639692));
#50414=CARTESIAN_POINT('Ctrl Pts',(-18.2201303078757,-1.955948595666,-0.0013580538473823));
#50415=CARTESIAN_POINT('Ctrl Pts',(-18.3218696921242,-1.9561856368743,-0.00124144867156942));
#50416=CARTESIAN_POINT('Ctrl Pts',(-18.317604068917,-1.95673815526926,-0.0758179952051893));
#50417=CARTESIAN_POINT('Ctrl Pts',(-18.3133384457099,-1.95284300545396,
-0.15033627747559));
#50418=CARTESIAN_POINT('Ctrl Pts',(-18.3090728225028,-1.94430742887076,
-0.224319183124746));
#50419=CARTESIAN_POINT('Ctrl Pts',(-18.272024040877,-1.87017225622972,-0.866892702244762));
#50420=CARTESIAN_POINT('Ctrl Pts',(-18.2349752592512,-1.44597844193375,
-1.46907915737697));
#50421=CARTESIAN_POINT('Ctrl Pts',(-18.1979264776254,-0.865887735938719,
-1.75524610884933));
#50422=CARTESIAN_POINT('Ctrl Pts',(-18.1608776959996,-0.285797029943679,
-2.04141306032169));
#50423=CARTESIAN_POINT('Ctrl Pts',(-18.1238289143738,0.450190567750422,
-2.01156050813421));
#50424=CARTESIAN_POINT('Ctrl Pts',(-18.086780132748,1.00519923505916,-1.6793525453925));
#50425=CARTESIAN_POINT('Ctrl Pts',(-18.0497313511221,1.56020790236788,-1.3471445826508));
#50426=CARTESIAN_POINT('Ctrl Pts',(-18.0126825694963,1.93423763929124,-0.712581209354875));
#50427=CARTESIAN_POINT('Ctrl Pts',(-17.9756337878705,1.95608776866446,-0.0661144096325921));
#50428=CARTESIAN_POINT('Ctrl Pts',(-17.9385850062447,1.97793789803769,0.580352390089681));
#50429=CARTESIAN_POINT('Ctrl Pts',(-17.9015362246189,1.64760841986083,1.23872261623831));
#50430=CARTESIAN_POINT('Ctrl Pts',(-17.8644874429931,1.11629755387044,1.60764742562002));
#50431=CARTESIAN_POINT('Ctrl Pts',(-17.8274386613673,0.584986687880032,
1.97657223500173));
#50432=CARTESIAN_POINT('Ctrl Pts',(-17.7903898797415,-0.147305565923918,
2.0560516276165));
#50433=CARTESIAN_POINT('Ctrl Pts',(-17.7533410981157,-0.745394816147864,
1.80970634135478));
#50434=CARTESIAN_POINT('Ctrl Pts',(-17.7162923164899,-1.34348406637179,
1.56336105509306));
#50435=CARTESIAN_POINT('Ctrl Pts',(-17.6792435348641,-1.80737031301573,
0.991191089954906));
#50436=CARTESIAN_POINT('Ctrl Pts',(-17.6421947532383,-1.92472380870155,
0.355089754987665));
#50437=CARTESIAN_POINT('Ctrl Pts',(-17.6354197328669,-1.94618395635101,
0.238767454670661));
#50438=CARTESIAN_POINT('Ctrl Pts',(-17.6286447124955,-1.95605585986643,
0.120307254488911));
#50439=CARTESIAN_POINT('Ctrl Pts',(-17.6218696921242,-1.95498100154377,
0.00166857518573596));
#50440=CARTESIAN_POINT('Origin',(-14.8,0.,0.));
#50441=CARTESIAN_POINT('',(-16.8201303078758,-1.95085314384129,0.000359159457361397));
#50442=CARTESIAN_POINT('',(-16.9218696921242,-1.9508121187761,0.000204457844419397));
#50443=CARTESIAN_POINT('',(-14.8,-1.954,-2.39295984553393E-16));
#50444=CARTESIAN_POINT('Ctrl Pts',(-16.8201303078758,-1.95085314384129,
0.000359159457361397));
#50445=CARTESIAN_POINT('Ctrl Pts',(-16.8374041157883,-1.95135253313437,
0.304469385080169));
#50446=CARTESIAN_POINT('Ctrl Pts',(-16.8546779237009,-1.88453897682348,
0.608371903822219));
#50447=CARTESIAN_POINT('Ctrl Pts',(-16.8719517316135,-1.74926193216667,
0.87791417838619));
#50448=CARTESIAN_POINT('Ctrl Pts',(-16.9090005132393,-1.4591203657074,1.45602717580853));
#50449=CARTESIAN_POINT('Ctrl Pts',(-16.9460492948651,-0.854036703785103,
1.87607800661458));
#50450=CARTESIAN_POINT('Ctrl Pts',(-16.9830980764909,-0.210969493905966,
1.9458012448809));
#50451=CARTESIAN_POINT('Ctrl Pts',(-17.0201468581168,0.432097715973189,
2.01552448314721));
#50452=CARTESIAN_POINT('Ctrl Pts',(-17.0571956397426,1.11314847380918,1.73492012887377));
#50453=CARTESIAN_POINT('Ctrl Pts',(-17.0942444213684,1.52045261642256,1.2324262465368));
#50454=CARTESIAN_POINT('Ctrl Pts',(-17.1312932029942,1.92775675903592,0.72993236419984));
#50455=CARTESIAN_POINT('Ctrl Pts',(-17.16834198462,2.06131428642669,0.00554895379934056));
#50456=CARTESIAN_POINT('Ctrl Pts',(-17.2053907662458,1.85999332357917,-0.609159624548341));
#50457=CARTESIAN_POINT('Ctrl Pts',(-17.2424395478716,1.65867236073165,-1.22386820289605));
#50458=CARTESIAN_POINT('Ctrl Pts',(-17.2794883294974,1.12247290764584,-1.72890194919093));
#50459=CARTESIAN_POINT('Ctrl Pts',(-17.3165371111232,0.496823871174823,
-1.89309710605923));
#50460=CARTESIAN_POINT('Ctrl Pts',(-17.353585892749,-0.128825165296163,
-2.05729226292753));
#50461=CARTESIAN_POINT('Ctrl Pts',(-17.3906346743748,-0.843923785152349,
-1.88064883036924));
#50462=CARTESIAN_POINT('Ctrl Pts',(-17.4276834560006,-1.32115745729256,
-1.44401993925958));
#50463=CARTESIAN_POINT('Ctrl Pts',(-17.4584990732923,-1.71810034054097,
-1.0808504039471));
#50464=CARTESIAN_POINT('Ctrl Pts',(-17.489314690584,-1.95048320399723,-0.537817409912763));
#50465=CARTESIAN_POINT('Ctrl Pts',(-17.5201303078758,-1.95526004210547,
0.001601638831479));
#50466=CARTESIAN_POINT('Ctrl Pts',(-17.6218696921242,-1.95498100154377,
0.00166857518573596));
#50467=CARTESIAN_POINT('Ctrl Pts',(-17.5915959308697,-1.95017806332973,
-0.528461056297915));
#50468=CARTESIAN_POINT('Ctrl Pts',(-17.5613221696153,-1.72680176835567,
-1.06215437001553));
#50469=CARTESIAN_POINT('Ctrl Pts',(-17.5310484083608,-1.34208584047146,
-1.42458979032064));
#50470=CARTESIAN_POINT('Ctrl Pts',(-17.493999626735,-0.871273631827864,
-1.86813529586539));
#50471=CARTESIAN_POINT('Ctrl Pts',(-17.4569508451092,-0.158828469813003,
-2.05519360215856));
#50472=CARTESIAN_POINT('Ctrl Pts',(-17.4199020634834,0.469149653676805,
-1.90014448827839));
#50473=CARTESIAN_POINT('Ctrl Pts',(-17.3828532818576,1.0971277771666,-1.74509537439822));
#50474=CARTESIAN_POINT('Ctrl Pts',(-17.3458045002318,1.64063886213135,-1.24793884034472));
#50475=CARTESIAN_POINT('Ctrl Pts',(-17.308755718606,1.85090732575802,-0.636233090411912));
#50476=CARTESIAN_POINT('Ctrl Pts',(-17.2717069369802,2.06117578938469,-0.0245273404790851));
#50477=CARTESIAN_POINT('Ctrl Pts',(-17.2346581553544,1.9382016316733,0.701727625333045));
#50478=CARTESIAN_POINT('Ctrl Pts',(-17.1976093737286,1.53827251372567,1.21011079963609));
#50479=CARTESIAN_POINT('Ctrl Pts',(-17.1605605921028,1.13834339577805,1.71849397393913));
#50480=CARTESIAN_POINT('Ctrl Pts',(-17.1235118104769,0.461459317594161,
2.00900535673306));
#50481=CARTESIAN_POINT('Ctrl Pts',(-17.0864630288511,-0.18255672787268,
1.94867224411603));
#50482=CARTESIAN_POINT('Ctrl Pts',(-17.0494142472253,-0.826572773339502,
1.88833913149901));
#50483=CARTESIAN_POINT('Ctrl Pts',(-17.0123654655995,-1.4377207860893,1.47716152347106));
#50484=CARTESIAN_POINT('Ctrl Pts',(-16.9753166839737,-1.73626644742514,
0.903343399502911));
#50485=CARTESIAN_POINT('Ctrl Pts',(-16.9575010200239,-1.87982823117732,
0.627411225316896));
#50486=CARTESIAN_POINT('Ctrl Pts',(-16.939685356074,-1.95110497856138,0.313870646854676));
#50487=CARTESIAN_POINT('Ctrl Pts',(-16.9218696921242,-1.9508121187761,0.000204457844419397));
#50488=CARTESIAN_POINT('Origin',(-14.8,0.,0.));
#50489=CARTESIAN_POINT('',(-16.1201303078758,-1.95394212134825,-0.00178662227266063));
#50490=CARTESIAN_POINT('',(-16.2218696921242,-1.95423044051614,-0.00177357873807178));
#50491=CARTESIAN_POINT('',(-14.8,-1.954,-2.39295984553393E-16));
#50492=CARTESIAN_POINT('Ctrl Pts',(-16.1201303078758,-1.95394212134825,
-0.00178662227266063));
#50493=CARTESIAN_POINT('Ctrl Pts',(-16.1484447593668,-1.94939007196124,
0.494710652380524));
#50494=CARTESIAN_POINT('Ctrl Pts',(-16.1767592108579,-1.75678535459633,
0.994349447558111));
#50495=CARTESIAN_POINT('Ctrl Pts',(-16.205073662349,-1.41534509418331,1.35183167454762));
#50496=CARTESIAN_POINT('Ctrl Pts',(-16.2421224439748,-0.968578691158015,
1.8195886066223));
#50497=CARTESIAN_POINT('Ctrl Pts',(-16.2791712256006,-0.266989530277769,
2.04395791762872));
#50498=CARTESIAN_POINT('Ctrl Pts',(-16.3162200072264,0.368291399188672,
1.92224141491713));
#50499=CARTESIAN_POINT('Ctrl Pts',(-16.3532687888522,1.00357232865512,1.80052491220555));
#50500=CARTESIAN_POINT('Ctrl Pts',(-16.390317570478,1.57254502670776,1.33272259577594));
#50501=CARTESIAN_POINT('Ctrl Pts',(-16.4273663521038,1.81477963556009,0.732956674228));
#50502=CARTESIAN_POINT('Ctrl Pts',(-16.4644151337296,2.05701424441242,0.13319075268005));
#50503=CARTESIAN_POINT('Ctrl Pts',(-16.5014639153554,1.97251076406445,-0.598538773986235));
#50504=CARTESIAN_POINT('Ctrl Pts',(-16.5385126969812,1.59994807918817,-1.12730508552081));
#50505=CARTESIAN_POINT('Ctrl Pts',(-16.5755614786071,1.22738539431189,-1.65607139705536));
#50506=CARTESIAN_POINT('Ctrl Pts',(-16.6126102602329,0.566763504907309,
-1.98187449345821));
#50507=CARTESIAN_POINT('Ctrl Pts',(-16.6496590418587,-0.0795381158151578,
-1.95558796786837));
#50508=CARTESIAN_POINT('Ctrl Pts',(-16.6867078234845,-0.725839736537652,
-1.92930144227853));
#50509=CARTESIAN_POINT('Ctrl Pts',(-16.7237566051103,-1.35782108857803,
-1.550925294696));
#50510=CARTESIAN_POINT('Ctrl Pts',(-16.7608053867361,-1.68621202910011,
-0.993649638885402));
#50511=CARTESIAN_POINT('Ctrl Pts',(-16.7805803604493,-1.86149234687336,
-0.69620095201697));
#50512=CARTESIAN_POINT('Ctrl Pts',(-16.8003553341625,-1.95028144533721,
-0.347784790506909));
#50513=CARTESIAN_POINT('Ctrl Pts',(-16.8201303078758,-1.95085314384129,
0.000359159457361397));
#50514=CARTESIAN_POINT('Ctrl Pts',(-16.9218696921242,-1.9508121187761,0.000204457844419397));
#50515=CARTESIAN_POINT('Ctrl Pts',(-16.9026365744482,-1.95049595841696,
-0.338417708648121));
#50516=CARTESIAN_POINT('Ctrl Pts',(-16.8834034567723,-1.86676867152405,
-0.677186268529284));
#50517=CARTESIAN_POINT('Ctrl Pts',(-16.8641703390963,-1.7005303973301,-0.968941092964963));
#50518=CARTESIAN_POINT('Ctrl Pts',(-16.8271215574705,-1.38030537597732,
-1.53094882155632));
#50519=CARTESIAN_POINT('Ctrl Pts',(-16.7900727758447,-0.753912023349896,
-1.91850563883067));
#50520=CARTESIAN_POINT('Ctrl Pts',(-16.7530239942189,-0.108062746390163,
-1.95421926014519));
#50521=CARTESIAN_POINT('Ctrl Pts',(-16.7159752125931,0.537786530569552,
-1.98993288145971));
#50522=CARTESIAN_POINT('Ctrl Pts',(-16.6789264309673,1.20309173186161,-1.67380330681439));
#50523=CARTESIAN_POINT('Ctrl Pts',(-16.6418776493414,1.58332974143817,-1.1505291842266));
#50524=CARTESIAN_POINT('Ctrl Pts',(-16.6048288677156,1.96356775101474,-0.627255061638789));
#50525=CARTESIAN_POINT('Ctrl Pts',(-16.5677800860898,2.05873856887587,0.103163608891498));
#50526=CARTESIAN_POINT('Ctrl Pts',(-16.530731304464,1.8252806627269,0.706400011434759));
#50527=CARTESIAN_POINT('Ctrl Pts',(-16.4936825228382,1.59182275657793,1.30963641397803));
#50528=CARTESIAN_POINT('Ctrl Pts',(-16.4566337412124,1.02973612641886,1.78569054853423));
#50529=CARTESIAN_POINT('Ctrl Pts',(-16.4195849595866,0.396298742980112,
1.91666318903248));
#50530=CARTESIAN_POINT('Ctrl Pts',(-16.3825361779608,-0.237138640458614,
2.04763582953073));
#50531=CARTESIAN_POINT('Ctrl Pts',(-16.345487396335,-0.941926777176993,
1.83352697597105));
#50532=CARTESIAN_POINT('Ctrl Pts',(-16.3084386147092,-1.39547044451608,
1.37233841029168));
#50533=CARTESIAN_POINT('Ctrl Pts',(-16.2795823071808,-1.74872350623489,
1.01313094122532));
#50534=CARTESIAN_POINT('Ctrl Pts',(-16.2507259996525,-1.94956070655241,
0.504034134293982));
#50535=CARTESIAN_POINT('Ctrl Pts',(-16.2218696921242,-1.95423044051614,
-0.00177357873807178));
#50536=CARTESIAN_POINT('Origin',(-14.8,0.,0.));
#50537=CARTESIAN_POINT('',(-15.4201303078757,-1.95687456006756,0.000726948241557314));
#50538=CARTESIAN_POINT('',(-15.5218696921242,-1.95671484857984,0.000882047759029596));
#50539=CARTESIAN_POINT('',(-14.8,-1.954,-2.39295984553393E-16));
#50540=CARTESIAN_POINT('Ctrl Pts',(-15.4201303078757,-1.95687456006756,
0.000726948241557314));
#50541=CARTESIAN_POINT('Ctrl Pts',(-15.4224366213195,-1.95706686879056,
0.0410111310332522));
#50542=CARTESIAN_POINT('Ctrl Pts',(-15.4247429347632,-1.95593068181528,
0.0812842614253603));
#50543=CARTESIAN_POINT('Ctrl Pts',(-15.427049248207,-1.95343159833963,0.121472641147085));
#50544=CARTESIAN_POINT('Ctrl Pts',(-15.4640980298328,-1.913286145342,0.767061604017206));
#50545=CARTESIAN_POINT('Ctrl Pts',(-15.5011468114586,-1.52143930925716,
1.39078028694765));
#50546=CARTESIAN_POINT('Ctrl Pts',(-15.5381955930844,-0.957246999683104,
1.70714053127933));
#50547=CARTESIAN_POINT('Ctrl Pts',(-15.5752443747102,-0.393054690109075,
2.023500775611));
#50548=CARTESIAN_POINT('Ctrl Pts',(-15.6122931563361,0.34348309295417,2.03250258134392));
#50549=CARTESIAN_POINT('Ctrl Pts',(-15.6493419379619,0.915238696889824,
1.73002564710885));
#50550=CARTESIAN_POINT('Ctrl Pts',(-15.6863907195877,1.4869943008255,1.42754871287377));
#50551=CARTESIAN_POINT('Ctrl Pts',(-15.7234395012135,1.89396772563359,0.81359303867069));
#50552=CARTESIAN_POINT('Ctrl Pts',(-15.7604882828393,1.94987932818113,0.169178064390397));
#50553=CARTESIAN_POINT('Ctrl Pts',(-15.7975370644651,2.00579093072867,-0.475236909889895));
#50554=CARTESIAN_POINT('Ctrl Pts',(-15.8345858460909,1.71064071101566,-1.15011118424738));
#50555=CARTESIAN_POINT('Ctrl Pts',(-15.8716346277167,1.19952465872418,-1.54654169198623));
#50556=CARTESIAN_POINT('Ctrl Pts',(-15.9086834093425,0.688408606432718,
-1.94297219972505));
#50557=CARTESIAN_POINT('Ctrl Pts',(-15.9457321909683,-0.0386732784372092,
-2.06095894084525));
#50558=CARTESIAN_POINT('Ctrl Pts',(-15.9827809725941,-0.648921491579182,
-1.84649709171329));
#50559=CARTESIAN_POINT('Ctrl Pts',(-16.0198297542199,-1.25916970472118,
-1.63203524258132));
#50560=CARTESIAN_POINT('Ctrl Pts',(-16.0568785358457,-1.75258424613523,
-1.08512480319718));
#50561=CARTESIAN_POINT('Ctrl Pts',(-16.0939273174715,-1.90331969425709,
-0.456097306933615));
#50562=CARTESIAN_POINT('Ctrl Pts',(-16.1026616476063,-1.93885590109382,
-0.307802718688236));
#50563=CARTESIAN_POINT('Ctrl Pts',(-16.111395977741,-1.95534631955948,-0.154944140057699));
#50564=CARTESIAN_POINT('Ctrl Pts',(-16.1201303078758,-1.95394212134825,
-0.00178662227266063));
#50565=CARTESIAN_POINT('Ctrl Pts',(-16.2218696921242,-1.95423044051614,
-0.00177357873807178));
#50566=CARTESIAN_POINT('Ctrl Pts',(-16.2136772180267,-1.95555620523854,
-0.14537534009457));
#50567=CARTESIAN_POINT('Ctrl Pts',(-16.2054847439292,-1.9410703771609,-0.288711992183037));
#50568=CARTESIAN_POINT('Ctrl Pts',(-16.1972922698318,-1.90977176526088,
-0.428278272262475));
#50569=CARTESIAN_POINT('Ctrl Pts',(-16.160243488206,-1.7682302207068,-1.05943811133816));
#50570=CARTESIAN_POINT('Ctrl Pts',(-16.1231947065801,-1.28284793363885,
-1.61348951169046));
#50571=CARTESIAN_POINT('Ctrl Pts',(-16.0861459249543,-0.675793806758042,
-1.83683238337832));
#50572=CARTESIAN_POINT('Ctrl Pts',(-16.0490971433285,-0.0687396798772465,
-2.06017525506617));
#50573=CARTESIAN_POINT('Ctrl Pts',(-16.0120483617027,0.659986286816407,
-1.9528095980896));
#50574=CARTESIAN_POINT('Ctrl Pts',(-15.9749995800769,1.17683206082491,-1.5638787595253));
#50575=CARTESIAN_POINT('Ctrl Pts',(-15.9379507984511,1.69367783483344,-1.17494792096097));
#50576=CARTESIAN_POINT('Ctrl Pts',(-15.9009020168253,1.9986434161568,-0.504451900808881));
#50577=CARTESIAN_POINT('Ctrl Pts',(-15.8638532351995,1.95214013341295,0.140710246244767));
#50578=CARTESIAN_POINT('Ctrl Pts',(-15.8268044535737,1.9056368506691,0.785872393298378));
#50579=CARTESIAN_POINT('Ctrl Pts',(-15.7897556719479,1.50766470385809,1.40570066725355));
#50580=CARTESIAN_POINT('Ctrl Pts',(-15.7527068903221,0.940383276298581,
1.71648762522126));
#50581=CARTESIAN_POINT('Ctrl Pts',(-15.7156581086963,0.373101848739073,
2.02727458318898));
#50582=CARTESIAN_POINT('Ctrl Pts',(-15.6786093270705,-0.363488859568931,
2.02902022516925));
#50583=CARTESIAN_POINT('Ctrl Pts',(-15.6415605454446,-0.932236971095907,
1.7209255369137));
#50584=CARTESIAN_POINT('Ctrl Pts',(-15.6045117638188,-1.5009850826229,1.41283084865815));
#50585=CARTESIAN_POINT('Ctrl Pts',(-15.567462982193,-1.90189059736886,0.794895830166782));
#50586=CARTESIAN_POINT('Ctrl Pts',(-15.5304142005672,-1.95145127252239,
0.149961344521046));
#50587=CARTESIAN_POINT('Ctrl Pts',(-15.5275660310862,-1.95526130881067,
0.100381233147203));
#50588=CARTESIAN_POINT('Ctrl Pts',(-15.5247178616052,-1.95699491471456,
0.0506415562763195));
#50589=CARTESIAN_POINT('Ctrl Pts',(-15.5218696921242,-1.95671484857984,
0.000882047759029596));
#50590=CARTESIAN_POINT('Origin',(-14.8,0.,0.));
#50591=CARTESIAN_POINT('',(-14.7201303078758,-1.95178645645483,0.00133170247388875));
#50592=CARTESIAN_POINT('',(-14.8218696921242,-1.95159637362084,0.00122105347580572));
#50593=CARTESIAN_POINT('',(-14.8,-1.954,-2.39295984553393E-16));
#50594=CARTESIAN_POINT('Ctrl Pts',(-14.7201303078758,-1.95178645645483,
0.00133170247388875));
#50595=CARTESIAN_POINT('Ctrl Pts',(-14.733477264898,-1.95325840706067,0.236027446913741));
#50596=CARTESIAN_POINT('Ctrl Pts',(-14.7468242219202,-1.91411010663923,
0.470248610705033));
#50597=CARTESIAN_POINT('Ctrl Pts',(-14.7601711789425,-1.83215096261091,
0.688384675993667));
#50598=CARTESIAN_POINT('Ctrl Pts',(-14.7972199605683,-1.60464693871359,
1.29389164167338));
#50599=CARTESIAN_POINT('Ctrl Pts',(-14.8342687421941,-1.04727724246687,
1.77545987161808));
#50600=CARTESIAN_POINT('Ctrl Pts',(-14.8713175238199,-0.415160812309883,
1.91266623117082));
#50601=CARTESIAN_POINT('Ctrl Pts',(-14.9083663054457,0.216955617847083,
2.04987259072355));
#50602=CARTESIAN_POINT('Ctrl Pts',(-14.9454150870715,0.923818781914313,
1.84271707988433));
#50603=CARTESIAN_POINT('Ctrl Pts',(-14.9824638686973,1.38188367690205,1.38601880054011));
#50604=CARTESIAN_POINT('Ctrl Pts',(-15.0195126503231,1.83994857188978,0.929320521195901));
#50605=CARTESIAN_POINT('Ctrl Pts',(-15.0565614319489,2.04921519779803,0.223079473346703));
#50606=CARTESIAN_POINT('Ctrl Pts',(-15.0936102135747,1.91389815435844,-0.409444094697087));
#50607=CARTESIAN_POINT('Ctrl Pts',(-15.1306589952005,1.77858111091886,-1.04196766274089));
#50608=CARTESIAN_POINT('Ctrl Pts',(-15.1677077768263,1.29868039813141,-1.60077375097929));
#50609=CARTESIAN_POINT('Ctrl Pts',(-15.2047565584522,0.693855895654001,
-1.83008595645264));
#50610=CARTESIAN_POINT('Ctrl Pts',(-15.241805340078,0.0890313931765885,
-2.05939816192598));
#50611=CARTESIAN_POINT('Ctrl Pts',(-15.2788541217038,-0.640716898990796,
-1.95921648463428));
#50612=CARTESIAN_POINT('Ctrl Pts',(-15.3159029033296,-1.16136901011926,
-1.57539602458353));
#50613=CARTESIAN_POINT('Ctrl Pts',(-15.3506453715116,-1.64961015088056,
-1.21546866568636));
#50614=CARTESIAN_POINT('Ctrl Pts',(-15.3853878396937,-1.95397760791726,
-0.606116819101585));
#50615=CARTESIAN_POINT('Ctrl Pts',(-15.4201303078757,-1.95687456006756,
0.000726948241557314));
#50616=CARTESIAN_POINT('Ctrl Pts',(-15.5218696921242,-1.95671484857984,
0.000882047759029596));
#50617=CARTESIAN_POINT('Ctrl Pts',(-15.4876690799794,-1.95335183478724,
-0.596626514374143));
#50618=CARTESIAN_POINT('Ctrl Pts',(-15.4534684678346,-1.65963680798056,
-1.19699460792317));
#50619=CARTESIAN_POINT('Ctrl Pts',(-15.4192678556898,-1.18423125427178,
-1.5582832894842));
#50620=CARTESIAN_POINT('Ctrl Pts',(-15.382219074064,-0.66923472530654,-1.9496594850436));
#50621=CARTESIAN_POINT('Ctrl Pts',(-15.3451702924382,0.0589741681850112,
-2.06047792336231));
#50622=CARTESIAN_POINT('Ctrl Pts',(-15.3081215108124,0.667080068155104,
-1.84001485226342));
#50623=CARTESIAN_POINT('Ctrl Pts',(-15.2710727291866,1.27518596812519,-1.61955178116453));
#50624=CARTESIAN_POINT('Ctrl Pts',(-15.2340239475608,1.76318887457379,-1.06780720064803));
#50625=CARTESIAN_POINT('Ctrl Pts',(-15.196975165935,1.90772037639653,-0.437325324399675));
#50626=CARTESIAN_POINT('Ctrl Pts',(-15.1599263843091,2.05225187821928,0.193156551848714));
#50627=CARTESIAN_POINT('Ctrl Pts',(-15.1228776026833,1.85331197541611,0.902375723828967));
#50628=CARTESIAN_POINT('Ctrl Pts',(-15.0858288210575,1.4019593264647,1.36570879795747));
#50629=CARTESIAN_POINT('Ctrl Pts',(-15.0487800394317,0.950606677513312,
1.82904187208595));
#50630=CARTESIAN_POINT('Ctrl Pts',(-15.0117312578059,0.246841282413703,
2.04648884836271));
#50631=CARTESIAN_POINT('Ctrl Pts',(-14.9746824761801,-0.387209764883699,
1.91852002122952));
#50632=CARTESIAN_POINT('Ctrl Pts',(-14.9376336945543,-1.02126081218112,
1.79055119409632));
#50633=CARTESIAN_POINT('Ctrl Pts',(-14.9005849129285,-1.58559751167634,
1.31716656355314));
#50634=CARTESIAN_POINT('Ctrl Pts',(-14.8635361313027,-1.82191199218985,
0.715043471821536));
#50635=CARTESIAN_POINT('Ctrl Pts',(-14.8496473182432,-1.91050134652424,
0.489320122958544));
#50636=CARTESIAN_POINT('Ctrl Pts',(-14.8357585051837,-1.9529923205933,0.245504601690091));
#50637=CARTESIAN_POINT('Ctrl Pts',(-14.8218696921242,-1.95159637362084,
0.00122105347580572));
#50638=CARTESIAN_POINT('Origin',(-14.8,0.,0.));
#50639=CARTESIAN_POINT('',(-14.0201303078758,-1.95205107141426,-0.00145700329680948));
#50640=CARTESIAN_POINT('',(-14.1218696921242,-1.9522775756875,-0.00154333085131984));
#50641=CARTESIAN_POINT('',(-14.8,-1.954,-2.39295984553393E-16));
#50642=CARTESIAN_POINT('Ctrl Pts',(-14.0201303078758,-1.95205107141426,
-0.00145700329680948));
#50643=CARTESIAN_POINT('Ctrl Pts',(-14.0445179084765,-1.94908269934858,
0.427233645472459));
#50644=CARTESIAN_POINT('Ctrl Pts',(-14.0689055090772,-1.81006537290534,
0.857674730656689));
#50645=CARTESIAN_POINT('Ctrl Pts',(-14.0932931096779,-1.55011885390173,
1.19489838510117));
#50646=CARTESIAN_POINT('Ctrl Pts',(-14.1303418913037,-1.15521728180249,
1.70719665245101));
#50647=CARTESIAN_POINT('Ctrl Pts',(-14.1673906729295,-0.481227900675196,
2.00436201468867));
#50648=CARTESIAN_POINT('Ctrl Pts',(-14.2044394545554,0.163351255607294,
1.95037611224874));
#50649=CARTESIAN_POINT('Ctrl Pts',(-14.2414882361812,0.807930411889783,
1.89639020980881));
#50650=CARTESIAN_POINT('Ctrl Pts',(-14.278537017807,1.42309934332747,1.49125304269128));
#50651=CARTESIAN_POINT('Ctrl Pts',(-14.3155857994328,1.72728327862235,0.920403763209719));
#50652=CARTESIAN_POINT('Ctrl Pts',(-14.3526345810586,2.03146721391722,0.349554483728171));
#50653=CARTESIAN_POINT('Ctrl Pts',(-14.3896833626844,2.02466615306931,-0.387006908117411));
#50654=CARTESIAN_POINT('Ctrl Pts',(-14.4267321443102,1.70999307375835,-0.952141953511904));
#50655=CARTESIAN_POINT('Ctrl Pts',(-14.463780925936,1.39531999444738,-1.51727699890641));
#50656=CARTESIAN_POINT('Ctrl Pts',(-14.5008297075618,0.772774896673343,
-1.91098569784982));
#50657=CARTESIAN_POINT('Ctrl Pts',(-14.5378784891876,0.127308766369077,
-1.95305992994188));
#50658=CARTESIAN_POINT('Ctrl Pts',(-14.5749272708134,-0.518157363935189,
-1.99513416203393));
#50659=CARTESIAN_POINT('Ctrl Pts',(-14.6119760524392,-1.18654452676969,
-1.68557392727462));
#50660=CARTESIAN_POINT('Ctrl Pts',(-14.649024834065,-1.57191893241295,-1.16607095918761));
#50661=CARTESIAN_POINT('Ctrl Pts',(-14.6727266586686,-1.8184608203896,-0.833720806489077));
#50662=CARTESIAN_POINT('Ctrl Pts',(-14.6964284832722,-1.94917253366878,
-0.415446246286262));
#50663=CARTESIAN_POINT('Ctrl Pts',(-14.7201303078758,-1.95178645645483,
0.00133170247388875));
#50664=CARTESIAN_POINT('Ctrl Pts',(-14.8218696921242,-1.95159637362084,
0.00122105347580572));
#50665=CARTESIAN_POINT('Ctrl Pts',(-14.7987097235579,-1.94926859457566,
-0.406128319985333));
#50666=CARTESIAN_POINT('Ctrl Pts',(-14.7755497549916,-1.82490683437804,
-0.814779110591518));
#50667=CARTESIAN_POINT('Ctrl Pts',(-14.7523897864253,-1.58876519036178,
-1.14301165513501));
#50668=CARTESIAN_POINT('Ctrl Pts',(-14.7153410047994,-1.2110116464884,-1.66808213743989));
#50669=CARTESIAN_POINT('Ctrl Pts',(-14.6782922231736,-0.547212297209818,
-1.98736154912963));
#50670=CARTESIAN_POINT('Ctrl Pts',(-14.6412434415478,0.09879899914816,-1.95470950057729));
#50671=CARTESIAN_POINT('Ctrl Pts',(-14.604194659922,0.744810295506157,-1.92205745202494));
#50672=CARTESIAN_POINT('Ctrl Pts',(-14.5671458782962,1.37303353894355,-1.5374739432305));
#50673=CARTESIAN_POINT('Ctrl Pts',(-14.5300970966704,1.69591874594352,-0.976990317780662));
#50674=CARTESIAN_POINT('Ctrl Pts',(-14.4930483150446,2.01880395294348,-0.416506692330825));
#50675=CARTESIAN_POINT('Ctrl Pts',(-14.4559995334188,2.03635112350602,0.319877049774405));
#50676=CARTESIAN_POINT('Ctrl Pts',(-14.418950751793,1.74052857676173,0.89510376345739));
#50677=CARTESIAN_POINT('Ctrl Pts',(-14.3819019701672,1.44470603001745,1.47033047714036));
#50678=CARTESIAN_POINT('Ctrl Pts',(-14.3448531885414,0.835513765966365,
1.8844001624011));
#50679=CARTESIAN_POINT('Ctrl Pts',(-14.3078044069156,0.191790919130116,
1.94778507983274));
#50680=CARTESIAN_POINT('Ctrl Pts',(-14.2707556252898,-0.451931927706151,
2.01116999726438));
#50681=CARTESIAN_POINT('Ctrl Pts',(-14.2337068436639,-1.13018535732759,
1.7238701468669));
#50682=CARTESIAN_POINT('Ctrl Pts',(-14.1966580620381,-1.53251959802447,
1.21738825177127));
#50683=CARTESIAN_POINT('Ctrl Pts',(-14.1717286054001,-1.80324304876393,
0.876585723654715));
#50684=CARTESIAN_POINT('Ctrl Pts',(-14.1467991487622,-1.94903853347043,
0.436544113465563));
#50685=CARTESIAN_POINT('Ctrl Pts',(-14.1218696921242,-1.9522775756875,-0.00154333085131984));
#50686=CARTESIAN_POINT('Origin',(-14.8,0.,0.));
#50687=CARTESIAN_POINT('',(-13.3201303078758,-1.95703609937262,-0.000519725096467805));
#50688=CARTESIAN_POINT('',(-13.4218696921242,-1.957128029801,-0.000349295805945385));
#50689=CARTESIAN_POINT('',(-14.8,-1.954,-2.39295984553393E-16));
#50690=CARTESIAN_POINT('Ctrl Pts',(-13.3201303078758,-1.95703609937262,
-0.000519725096467805));
#50691=CARTESIAN_POINT('Ctrl Pts',(-13.355558552055,-1.95484025103045,0.618166309907161));
#50692=CARTESIAN_POINT('Ctrl Pts',(-13.3909867962342,-1.63665153253831,
1.23879689579462));
#50693=CARTESIAN_POINT('Ctrl Pts',(-13.4264150404134,-1.13208054584297,
1.59657265718252));
#50694=CARTESIAN_POINT('Ctrl Pts',(-13.4634638220392,-0.604429776410676,
1.97071358236128));
#50695=CARTESIAN_POINT('Ctrl Pts',(-13.500512603665,0.127043995617411,2.05740302359373));
#50696=CARTESIAN_POINT('Ctrl Pts',(-13.5375613852908,0.727531013857885,
1.81696153944268));
#50697=CARTESIAN_POINT('Ctrl Pts',(-13.5746101669166,1.32801803209836,1.57652005529162));
#50698=CARTESIAN_POINT('Ctrl Pts',(-13.6116589485424,1.79751829655122,1.00894764575704));
#50699=CARTESIAN_POINT('Ctrl Pts',(-13.6487077301682,1.92113241481916,0.374033229366182));
#50700=CARTESIAN_POINT('Ctrl Pts',(-13.685756511794,2.04474653308709,-0.260881187024657));
#50701=CARTESIAN_POINT('Ctrl Pts',(-13.7228052934198,1.82247450517011,-0.963137610271772));
#50702=CARTESIAN_POINT('Ctrl Pts',(-13.7598540750457,1.35605455650233,-1.41129963215763));
#50703=CARTESIAN_POINT('Ctrl Pts',(-13.7969028566715,0.889634607834529,
-1.8594616540435));
#50704=CARTESIAN_POINT('Ctrl Pts',(-13.8339516382973,0.179066738415911,
-2.0535292745681));
#50705=CARTESIAN_POINT('Ctrl Pts',(-13.8710004199231,-0.450408333150168,
-1.90467397351039));
#50706=CARTESIAN_POINT('Ctrl Pts',(-13.9080492015489,-1.07988340471625,
-1.75581867245269));
#50707=CARTESIAN_POINT('Ctrl Pts',(-13.9450979831747,-1.62826567842979,
-1.26404044981269));
#50708=CARTESIAN_POINT('Ctrl Pts',(-13.9821467648005,-1.84454993375096,
-0.65443575226167));
#50709=CARTESIAN_POINT('Ctrl Pts',(-13.9948079458256,-1.91846367637156,
-0.446107297431768));
#50710=CARTESIAN_POINT('Ctrl Pts',(-14.0074691268507,-1.95359214536773,
-0.224018049653602));
#50711=CARTESIAN_POINT('Ctrl Pts',(-14.0201303078758,-1.95205107141426,
-0.00145700329680948));
#50712=CARTESIAN_POINT('Ctrl Pts',(-14.1218696921242,-1.9522775756875,-0.00154333085131984));
#50713=CARTESIAN_POINT('Ctrl Pts',(-14.1097503671363,-1.95385221912429,
-0.214517251135975));
#50714=CARTESIAN_POINT('Ctrl Pts',(-14.0976310421485,-1.92173553791281,
-0.427029330232189));
#50715=CARTESIAN_POINT('Ctrl Pts',(-14.0855117171607,-1.85390212817894,
-0.627453084312592));
#50716=CARTESIAN_POINT('Ctrl Pts',(-14.0484629355349,-1.64653536586419,
-1.24014858550701));
#50717=CARTESIAN_POINT('Ctrl Pts',(-14.0114141539091,-1.10538678946238,
-1.73987564810208));
#50718=CARTESIAN_POINT('Ctrl Pts',(-13.9743653722833,-0.478150615718903,
-1.89789948695062));
#50719=CARTESIAN_POINT('Ctrl Pts',(-13.9373165906575,0.149085558024587,
-2.05592332579916));
#50720=CARTESIAN_POINT('Ctrl Pts',(-13.9002678090317,0.862409329109737,
-1.87224394090116));
#50721=CARTESIAN_POINT('Ctrl Pts',(-13.8632190274059,1.33531854919931,-1.43093495521077));
#50722=CARTESIAN_POINT('Ctrl Pts',(-13.8261702457801,1.80822776928888,-0.989625969520384));
#50723=CARTESIAN_POINT('Ctrl Pts',(-13.7891214641543,2.04072243838287,-0.29068738303762));
#50724=CARTESIAN_POINT('Ctrl Pts',(-13.7520726825284,1.92638522957703,0.345963034365286));
#50725=CARTESIAN_POINT('Ctrl Pts',(-13.7150239009026,1.8120480207712,0.982613451768174));
#50726=CARTESIAN_POINT('Ctrl Pts',(-13.6779751192768,1.35087893406555,1.55697570009121));
#50727=CARTESIAN_POINT('Ctrl Pts',(-13.640926337651,0.753964019946039,1.80615301968205));
#50728=CARTESIAN_POINT('Ctrl Pts',(-13.6038775560252,0.157049105826529,
2.0553303392729));
#50729=CARTESIAN_POINT('Ctrl Pts',(-13.5668287743994,-0.575611635706843,
1.97932273013156));
#50730=CARTESIAN_POINT('Ctrl Pts',(-13.5297799927736,-1.10866514926791,
1.61292035162266));
#50731=CARTESIAN_POINT('Ctrl Pts',(-13.4938098925571,-1.62619872155089,
1.25718583901078));
#50732=CARTESIAN_POINT('Ctrl Pts',(-13.4578397923407,-1.95557905520156,
0.627720175010101));
#50733=CARTESIAN_POINT('Ctrl Pts',(-13.4218696921242,-1.957128029801,-0.000349295805945385));
#50734=CARTESIAN_POINT('Origin',(-14.8,0.,0.));
#50735=CARTESIAN_POINT('',(-12.6201303078758,-1.95358117384718,0.00178179146160605));
#50736=CARTESIAN_POINT('',(-12.7218696921242,-1.95330164162301,0.00176139094907822));
#50737=CARTESIAN_POINT('',(-14.8,-1.954,-2.39295984553393E-16));
#50738=CARTESIAN_POINT('Ctrl Pts',(-12.6201303078758,-1.95358117384718,
0.00178179146160605));
#50739=CARTESIAN_POINT('Ctrl Pts',(-12.6295504140077,-1.95506722451589,
0.167042362152062));
#50740=CARTESIAN_POINT('Ctrl Pts',(-12.6389705201395,-1.93584624707066,
0.331962304665006));
#50741=CARTESIAN_POINT('Ctrl Pts',(-12.6483906262714,-1.89457311803675,
0.491165259715588));
#50742=CARTESIAN_POINT('Ctrl Pts',(-12.6854394078972,-1.73224807379813,
1.11730210289686));
#50743=CARTESIAN_POINT('Ctrl Pts',(-12.722488189523,-1.22881869473678,1.65500815520059));
#50744=CARTESIAN_POINT('Ctrl Pts',(-12.7595369711488,-0.614714388174372,
1.85816491004173));
#50745=CARTESIAN_POINT('Ctrl Pts',(-12.7965857527747,-0.00061008161194781,
2.06132166488287));
#50746=CARTESIAN_POINT('Ctrl Pts',(-12.8336345344005,0.724169152451543,
1.92992912226141));
#50747=CARTESIAN_POINT('Ctrl Pts',(-12.8706833160263,1.22787777771923,1.52412820160322));
#50748=CARTESIAN_POINT('Ctrl Pts',(-12.9077320976521,1.73158640298692,1.11832728094503));
#50749=CARTESIAN_POINT('Ctrl Pts',(-12.9447808792779,2.01422441945881,0.438117982250111));
#50750=CARTESIAN_POINT('Ctrl Pts',(-12.9818296609037,1.94642291596085,-0.205154683498651));
#50751=CARTESIAN_POINT('Ctrl Pts',(-13.0188784425295,1.8786214124629,-0.848427349247394));
#50752=CARTESIAN_POINT('Ctrl Pts',(-13.0559272241553,1.46038038899512,-1.45476338204999));
#50753=CARTESIAN_POINT('Ctrl Pts',(-13.0929760057811,0.883136887501676,
-1.74663099991751));
#50754=CARTESIAN_POINT('Ctrl Pts',(-13.1300247874069,0.305893386008212,
-2.03849861778504));
#50755=CARTESIAN_POINT('Ctrl Pts',(-13.1670735690327,-0.430352593510932,
-2.01589782071748));
#50756=CARTESIAN_POINT('Ctrl Pts',(-13.2041223506585,-0.988606962590199,
-1.68917343261643));
#50757=CARTESIAN_POINT('Ctrl Pts',(-13.2411711322843,-1.54686133166947,
-1.36244904451537));
#50758=CARTESIAN_POINT('Ctrl Pts',(-13.2782199139102,-1.92712409030886,
-0.731601065380813));
#50759=CARTESIAN_POINT('Ctrl Pts',(-13.315268695536,-1.9553415862103,-0.0853808712510157));
#50760=CARTESIAN_POINT('Ctrl Pts',(-13.3168892329826,-1.95657583756084,
-0.0571147859067663));
#50761=CARTESIAN_POINT('Ctrl Pts',(-13.3185097704292,-1.9571365405474,-0.028819289769768));
#50762=CARTESIAN_POINT('Ctrl Pts',(-13.3201303078758,-1.95703609937262,
-0.000519725096467805));
#50763=CARTESIAN_POINT('Ctrl Pts',(-13.4218696921242,-1.957128029801,-0.000349295805945385));
#50764=CARTESIAN_POINT('Ctrl Pts',(-13.4207910107148,-1.95717448088382,
-0.0191840184745534));
#50765=CARTESIAN_POINT('Ctrl Pts',(-13.4197123293055,-1.95692611424454,
-0.0380174855509708));
#50766=CARTESIAN_POINT('Ctrl Pts',(-13.4186336478962,-1.95637916299247,
-0.0568422773001921));
#50767=CARTESIAN_POINT('Ctrl Pts',(-13.3815848662704,-1.93759337756717,
-0.703405379837554));
#50768=CARTESIAN_POINT('Ctrl Pts',(-13.3445360846446,-1.56657552112786,
-1.33973443703577));
#50769=CARTESIAN_POINT('Ctrl Pts',(-13.3074873030187,-1.01314767462749,
-1.67456927694159));
#50770=CARTESIAN_POINT('Ctrl Pts',(-13.2704385213929,-0.459719828127115,
-2.00940411684742));
#50771=CARTESIAN_POINT('Ctrl Pts',(-13.2333897397671,0.276118008434306,
-2.04274473946083));
#50772=CARTESIAN_POINT('Ctrl Pts',(-13.1963409581413,0.857558561552295,
-1.7593304940767));
#50773=CARTESIAN_POINT('Ctrl Pts',(-13.1592921765155,1.43899911467027,-1.47591624869258));
#50774=CARTESIAN_POINT('Ctrl Pts',(-13.1222433948897,1.86604238434483,-0.875747135310894));
#50775=CARTESIAN_POINT('Ctrl Pts',(-13.0851946132639,1.94322236953466,-0.233532217092017));
#50776=CARTESIAN_POINT('Ctrl Pts',(-13.0481458316381,2.02040235472448,0.40868270112686));
#50777=CARTESIAN_POINT('Ctrl Pts',(-13.0110970500123,1.74771905542961,1.09294342418297));
#50778=CARTESIAN_POINT('Ctrl Pts',(-12.9740482683865,1.2499849153739,1.50605052545307));
#50779=CARTESIAN_POINT('Ctrl Pts',(-12.9369994867607,0.75225077531818,1.91915762672319));
#50780=CARTESIAN_POINT('Ctrl Pts',(-12.8999507051349,0.029465794501616,
2.06111110620728));
#50781=CARTESIAN_POINT('Ctrl Pts',(-12.862901923509,-0.587537299234008,
1.86693609850166));
#50782=CARTESIAN_POINT('Ctrl Pts',(-12.8258531418832,-1.20454039296963,
1.67276109079604));
#50783=CARTESIAN_POINT('Ctrl Pts',(-12.7888043602574,-1.7157615996243,1.14245759590073));
#50784=CARTESIAN_POINT('Ctrl Pts',(-12.7517555786316,-1.88720504100882,
0.518755826059528));
#50785=CARTESIAN_POINT('Ctrl Pts',(-12.7417936164625,-1.93330407591021,
0.351050083432241));
#50786=CARTESIAN_POINT('Ctrl Pts',(-12.7318316542933,-1.95483697372639,
0.176591589270381));
#50787=CARTESIAN_POINT('Ctrl Pts',(-12.7218696921242,-1.95330164162301,
0.00176139094907822));
#50788=CARTESIAN_POINT('Origin',(-14.8,0.,0.));
#50789=CARTESIAN_POINT('',(-11.9201303078758,-1.95093708226589,-0.000550973528005427));
#50790=CARTESIAN_POINT('',(-12.0218696921242,-1.95102823519099,-0.000697989405693117));
#50791=CARTESIAN_POINT('',(-14.8,-1.954,-2.39295984553393E-16));
#50792=CARTESIAN_POINT('Ctrl Pts',(-11.9201303078758,-1.95093708226589,
-0.000550973528005427));
#50793=CARTESIAN_POINT('Ctrl Pts',(-11.9405910575861,-1.95002744544509,
0.359627574766655));
#50794=CARTESIAN_POINT('Ctrl Pts',(-11.9610518072965,-1.85458725485174,
0.720254388310455));
#50795=CARTESIAN_POINT('Ctrl Pts',(-11.9815125570069,-1.66757630645233,
1.02461694017705));
#50796=CARTESIAN_POINT('Ctrl Pts',(-12.0185613386327,-1.3289509927683,1.57573368217324));
#50797=CARTESIAN_POINT('Ctrl Pts',(-12.0556101202585,-0.690090496095906,
1.9423754749052));
#50798=CARTESIAN_POINT('Ctrl Pts',(-12.0926589018843,-0.0434136774160742,
1.95672324679608));
#50799=CARTESIAN_POINT('Ctrl Pts',(-12.1297076835101,0.603263141263758,
1.97107101868696));
#50800=CARTESIAN_POINT('Ctrl Pts',(-12.1667564651359,1.25775628195103,1.63312476973678));
#50801=CARTESIAN_POINT('Ctrl Pts',(-12.2038052467617,1.62049151879134,1.09756906364216));
#50802=CARTESIAN_POINT('Ctrl Pts',(-12.2408540283875,1.98322675563165,0.562013357547537));
#50803=CARTESIAN_POINT('Ctrl Pts',(-12.2779028100133,2.05420408862499,-0.171151805691514));
#50804=CARTESIAN_POINT('Ctrl Pts',(-12.3149515916392,1.80093581352688,-0.766342487074322));
#50805=CARTESIAN_POINT('Ctrl Pts',(-12.352000373265,1.54766753842878,-1.36153316845711));
#50806=CARTESIAN_POINT('Ctrl Pts',(-12.3890491548908,0.970153655239247,
-1.81874936798367));
#50807=CARTESIAN_POINT('Ctrl Pts',(-12.4260979365166,0.332733488118346,
-1.92871434842581));
#50808=CARTESIAN_POINT('Ctrl Pts',(-12.4631467181424,-0.304686679002573,
-2.03867932886795));
#50809=CARTESIAN_POINT('Ctrl Pts',(-12.5001954997682,-1.00201313005487,
-1.80139309022565));
#50810=CARTESIAN_POINT('Ctrl Pts',(-12.537244281394,-1.44006600087307,-1.32546615387509));
#50811=CARTESIAN_POINT('Ctrl Pts',(-12.5648729568879,-1.76673856838838,
-0.970549465492388));
#50812=CARTESIAN_POINT('Ctrl Pts',(-12.5925016323818,-1.94922266544841,
-0.482918764521644));
#50813=CARTESIAN_POINT('Ctrl Pts',(-12.6201303078758,-1.95358117384718,
0.00178179146160605));
#50814=CARTESIAN_POINT('Ctrl Pts',(-12.7218696921242,-1.95330164162301,
0.00176139094907822));
#50815=CARTESIAN_POINT('Ctrl Pts',(-12.6947828726675,-1.94912703597966,
-0.473606206025261));
#50816=CARTESIAN_POINT('Ctrl Pts',(-12.6676960532109,-1.77440682962847,
-0.951721846927492));
#50817=CARTESIAN_POINT('Ctrl Pts',(-12.6406092337542,-1.45925195975997,
-1.30431368612634));
#50818=CARTESIAN_POINT('Ctrl Pts',(-12.6035604521284,-1.02818976101222,
-1.786581383684));
#50819=CARTESIAN_POINT('Ctrl Pts',(-12.5665116705026,-0.334399687402313,
-2.03401673401225));
#50820=CARTESIAN_POINT('Ctrl Pts',(-12.5294628888768,0.30455706556366,-1.93336377014132));
#50821=CARTESIAN_POINT('Ctrl Pts',(-12.492414107251,0.943513818529596,-1.83271080627039));
#50822=CARTESIAN_POINT('Ctrl Pts',(-12.4553653256252,1.52763725085163,-1.38396952820033));
#50823=CARTESIAN_POINT('Ctrl Pts',(-12.4183165439994,1.78956271932274,-0.792537536959608));
#50824=CARTESIAN_POINT('Ctrl Pts',(-12.3812677623736,2.05148818779385,-0.20110554571887));
#50825=CARTESIAN_POINT('Ctrl Pts',(-12.3442189807477,1.99121569241405,0.533017158692502));
#50826=CARTESIAN_POINT('Ctrl Pts',(-12.3071701991219,1.63633312528064,1.07380835207642));
#50827=CARTESIAN_POINT('Ctrl Pts',(-12.2701214174961,1.28145055814724,1.61459954546034));
#50828=CARTESIAN_POINT('Ctrl Pts',(-12.2330726358703,0.631957919260208,
1.96205922781676));
#50829=CARTESIAN_POINT('Ctrl Pts',(-12.1960238542445,-0.0148593923487363,
1.95714835215392));
#50830=CARTESIAN_POINT('Ctrl Pts',(-12.1589750726187,-0.661676703957681,
1.95223747649109));
#50831=CARTESIAN_POINT('Ctrl Pts',(-12.1219262909929,-1.30581868828856,
1.59495604280899));
#50832=CARTESIAN_POINT('Ctrl Pts',(-12.0848775093671,-1.65244904485148,
1.04883870449618));
#50833=CARTESIAN_POINT('Ctrl Pts',(-12.0638749036195,-1.84895053287836,
0.739249923294692));
#50834=CARTESIAN_POINT('Ctrl Pts',(-12.0428722978718,-1.94984221352703,
0.368975902315217));
#50835=CARTESIAN_POINT('Ctrl Pts',(-12.0218696921242,-1.95102823519099,
-0.000697989405693117));
#50836=CARTESIAN_POINT('Origin',(-14.8,0.,0.));
#50837=CARTESIAN_POINT('',(-11.2201303078758,-1.95560116054388,-0.00149635199143683));
#50838=CARTESIAN_POINT('',(-11.3218696921242,-1.95585802078492,-0.00139750151859497));
#50839=CARTESIAN_POINT('',(-14.8,-1.954,-2.39295984553393E-16));
#50840=CARTESIAN_POINT('Ctrl Pts',(-11.2201303078758,-1.95560116054388,
-0.00149635199143683));
#50841=CARTESIAN_POINT('Ctrl Pts',(-11.2516317011646,-1.95092725946121,
0.549677370997484));
#50842=CARTESIAN_POINT('Ctrl Pts',(-11.2831330944535,-1.70683034372718,
1.10447412907545));
#50843=CARTESIAN_POINT('Ctrl Pts',(-11.3146344877423,-1.29426767174851,
1.4681695425957));
#50844=CARTESIAN_POINT('Ctrl Pts',(-11.3516832693681,-0.809052805188828,
1.89591163737426));
#50845=CARTESIAN_POINT('Ctrl Pts',(-11.388732050994,-0.0908143044123737,
2.05932031030366));
#50846=CARTESIAN_POINT('Ctrl Pts',(-11.4257808326198,0.531696114981536,
1.8836002371131));
#50847=CARTESIAN_POINT('Ctrl Pts',(-11.4628296142456,1.15420653437546,1.70788016392253));
#50848=CARTESIAN_POINT('Ctrl Pts',(-11.4998783958714,1.68098887238684,1.19303134461199));
#50849=CARTESIAN_POINT('Ctrl Pts',(-11.5369271774972,1.87092461868595,0.574710086159801));
#50850=CARTESIAN_POINT('Ctrl Pts',(-11.573975959123,2.06086036498506,-0.0436111722923718));
#50851=CARTESIAN_POINT('Ctrl Pts',(-11.6110247407488,1.91394951957191,-0.765404869886186));
#50852=CARTESIAN_POINT('Ctrl Pts',(-11.6480735223746,1.49743603054664,-1.26029200836937));
#50853=CARTESIAN_POINT('Ctrl Pts',(-11.6851223040004,1.08092254152136,-1.75517914685256));
#50854=CARTESIAN_POINT('Ctrl Pts',(-11.7221710856262,0.394806408883924,
-2.02315972622511));
#50855=CARTESIAN_POINT('Ctrl Pts',(-11.759219867252,-0.246863683730499,
-1.94157382903509));
#50856=CARTESIAN_POINT('Ctrl Pts',(-11.7962686488778,-0.888533776344921,
-1.85998793184507));
#50857=CARTESIAN_POINT('Ctrl Pts',(-11.8333174305036,-1.48575782893633,
-1.42883555809249));
#50858=CARTESIAN_POINT('Ctrl Pts',(-11.8703662121295,-1.76517478988419,
-0.845463525585991));
#50859=CARTESIAN_POINT('Ctrl Pts',(-11.8869542440449,-1.8902795102696,-0.584267516725894));
#50860=CARTESIAN_POINT('Ctrl Pts',(-11.9035422759603,-1.95167454715981,
-0.292556561736662));
#50861=CARTESIAN_POINT('Ctrl Pts',(-11.9201303078758,-1.95093708226589,
-0.000550973528005427));
#50862=CARTESIAN_POINT('Ctrl Pts',(-12.0218696921242,-1.95102823519099,
-0.000697989405693117));
#50863=CARTESIAN_POINT('Ctrl Pts',(-12.005823516246,-1.95193436619415,-0.283132100458183));
#50864=CARTESIAN_POINT('Ctrl Pts',(-11.9897773403678,-1.89464136026534,
-0.565215910381814));
#50865=CARTESIAN_POINT('Ctrl Pts',(-11.9737311644897,-1.77732263479807,
-0.819618646514493));
#50866=CARTESIAN_POINT('Ctrl Pts',(-11.9366823828639,-1.50644713938678,
-1.40700541626888));
#50867=CARTESIAN_POINT('Ctrl Pts',(-11.8996336012381,-0.915577419769245,
-1.84682571283413));
#50868=CARTESIAN_POINT('Ctrl Pts',(-11.8625848196122,-0.275166025913142,
-1.93776524173156));
#50869=CARTESIAN_POINT('Ctrl Pts',(-11.8255360379864,0.365245367942961,
-2.02870477062899));
#50870=CARTESIAN_POINT('Ctrl Pts',(-11.7884872563606,1.05519843603763,-1.7707635318586));
#50871=CARTESIAN_POINT('Ctrl Pts',(-11.7514384747348,1.47888825483371,-1.2820062416364));
#50872=CARTESIAN_POINT('Ctrl Pts',(-11.714389693109,1.90257807362979,-0.793248951414214));
#50873=CARTESIAN_POINT('Ctrl Pts',(-11.6773409114832,2.06000464312729,-0.0736756097402326));
#50874=CARTESIAN_POINT('Ctrl Pts',(-11.6402921298574,1.87911076401531,0.547351085174407));
#50875=CARTESIAN_POINT('Ctrl Pts',(-11.6032433482316,1.69821688490332,1.16837778008906));
#50876=CARTESIAN_POINT('Ctrl Pts',(-11.5661945666058,1.17900255718184,1.69085782824438));
#50877=CARTESIAN_POINT('Ctrl Pts',(-11.52914578498,0.559122265841095,1.87564196096177));
#50878=CARTESIAN_POINT('Ctrl Pts',(-11.4920970033542,-0.060758025499648,
2.06042609367916));
#50879=CARTESIAN_POINT('Ctrl Pts',(-11.4550482217284,-0.781304280459649,
1.90751431095864));
#50880=CARTESIAN_POINT('Ctrl Pts',(-11.4179994401025,-1.27270847951518,
1.48689730649092));
#50881=CARTESIAN_POINT('Ctrl Pts',(-11.3859561907764,-1.69772076276046,
1.1231084056549));
#50882=CARTESIAN_POINT('Ctrl Pts',(-11.3539129414503,-1.95132545851315,
0.559065099150166));
#50883=CARTESIAN_POINT('Ctrl Pts',(-11.3218696921242,-1.95585802078492,
-0.00139750151859497));
#50884=CARTESIAN_POINT('Origin',(-14.8,0.,0.));
#50885=CARTESIAN_POINT('',(-10.5201303078758,-1.95562737994549,0.00148708654483385));
#50886=CARTESIAN_POINT('',(-10.6218696921242,-1.95536008754156,0.00157356082676479));
#50887=CARTESIAN_POINT('',(-14.8,-1.954,-2.39295984553393E-16));
#50888=CARTESIAN_POINT('Ctrl Pts',(-10.5201303078758,-1.95562737994549,
0.00148708654483385));
#50889=CARTESIAN_POINT('Ctrl Pts',(-10.5256235631173,-1.95643899330848,
0.0975981474980406));
#50890=CARTESIAN_POINT('Ctrl Pts',(-10.5311168183588,-1.94996615192806,
0.19359947904084));
#50891=CARTESIAN_POINT('Ctrl Pts',(-10.5366100736004,-1.935831083387,0.288459058675073));
#50892=CARTESIAN_POINT('Ctrl Pts',(-10.5736588552262,-1.84049834448853,
0.928231233179569));
#50893=CARTESIAN_POINT('Ctrl Pts',(-10.610707636852,-1.39663306929388,1.51606841800423));
#50894=CARTESIAN_POINT('Ctrl Pts',(-10.6477564184778,-0.807401017585439,
1.78290611327152));
#50895=CARTESIAN_POINT('Ctrl Pts',(-10.6848052001036,-0.218168965877002,
2.04974380853882));
#50896=CARTESIAN_POINT('Ctrl Pts',(-10.7218539817294,0.516429862345236,
1.99558201424877));
#50897=CARTESIAN_POINT('Ctrl Pts',(-10.7589027633552,1.06015531176482,1.64521163589242));
#50898=CARTESIAN_POINT('Ctrl Pts',(-10.795951544981,1.60388076118439,1.29484125753609));
#50899=CARTESIAN_POINT('Ctrl Pts',(-10.8330003266068,1.95673283180133,0.648262295113474));
#50900=CARTESIAN_POINT('Ctrl Pts',(-10.8700491082326,1.95720427575482,0.00142650133218715));
#50901=CARTESIAN_POINT('Ctrl Pts',(-10.9070978898584,1.9576757197083,-0.645409292449136));
#50902=CARTESIAN_POINT('Ctrl Pts',(-10.9441466714843,1.60576653699831,-1.29250191758911));
#50903=CARTESIAN_POINT('Ctrl Pts',(-10.9811954531101,1.06255239737241,-1.64366450797512));
#50904=CARTESIAN_POINT('Ctrl Pts',(-11.0182442347359,0.519338257746561,
-1.99482709836111));
#50905=CARTESIAN_POINT('Ctrl Pts',(-11.0552930163617,-0.215180838795228,
-2.05005965399313));
#50906=CARTESIAN_POINT('Ctrl Pts',(-11.0923417979875,-0.804801231675591,
-1.78408116111135));
#50907=CARTESIAN_POINT('Ctrl Pts',(-11.1293905796133,-1.394421624556,-1.51810266822956));
#50908=CARTESIAN_POINT('Ctrl Pts',(-11.1664393612391,-1.839143313775,-0.930913126833975));
#50909=CARTESIAN_POINT('Ctrl Pts',(-11.2034881428649,-1.93540854221306,
-0.291280597822286));
#50910=CARTESIAN_POINT('Ctrl Pts',(-11.2090355312019,-1.94982252783031,
-0.195507137112811));
#50911=CARTESIAN_POINT('Ctrl Pts',(-11.2145829195388,-1.95642423348279,
-0.0985579217609101));
#50912=CARTESIAN_POINT('Ctrl Pts',(-11.2201303078758,-1.95560116054388,
-0.00149635199143683));
#50913=CARTESIAN_POINT('Ctrl Pts',(-11.3218696921242,-1.95585802078492,
-0.00139750151859497));
#50914=CARTESIAN_POINT('Ctrl Pts',(-11.3168641598245,-1.95656606030428,
-0.088948349494719));
#50915=CARTESIAN_POINT('Ctrl Pts',(-11.3118586275248,-1.95119621341652,
-0.17641182068154));
#50916=CARTESIAN_POINT('Ctrl Pts',(-11.3068530952251,-1.93945243087164,
-0.26301091662872));
#50917=CARTESIAN_POINT('Ctrl Pts',(-11.2698043135993,-1.85253004002152,
-0.903979909065702));
#50918=CARTESIAN_POINT('Ctrl Pts',(-11.2327555319735,-1.41642311517025,
-1.49759566772477));
#50919=CARTESIAN_POINT('Ctrl Pts',(-11.1957067503477,-0.830746268420352,
-1.77214872721943));
#50920=CARTESIAN_POINT('Ctrl Pts',(-11.1586579687219,-0.245069421670441,
-2.0467017867141));
#50921=CARTESIAN_POINT('Ctrl Pts',(-11.1216091870961,0.490177346978098,
-2.00219214704436));
#50922=CARTESIAN_POINT('Ctrl Pts',(-11.0845604054703,1.03845730728765,-1.65899273501142));
#50923=CARTESIAN_POINT('Ctrl Pts',(-11.0475116238445,1.58673726759721,-1.31579332297848));
#50924=CARTESIAN_POINT('Ctrl Pts',(-11.0104628422187,1.94805041956778,-0.673904138582339));
#50925=CARTESIAN_POINT('Ctrl Pts',(-10.9734140605929,1.95701671402278,-0.027130332015815));
#50926=CARTESIAN_POINT('Ctrl Pts',(-10.936365278967,1.96598300847778,0.61964347455069));
#50927=CARTESIAN_POINT('Ctrl Pts',(-10.8993164973412,1.62260244541722,1.27130190328758));
#50928=CARTESIAN_POINT('Ctrl Pts',(-10.8622677157154,1.08404697968283,1.62956823107237));
#50929=CARTESIAN_POINT('Ctrl Pts',(-10.8252189340896,0.545491513948429,
1.98783455885716));
#50930=CARTESIAN_POINT('Ctrl Pts',(-10.7881701524638,-0.188238854459824,
2.05270878568984));
#50931=CARTESIAN_POINT('Ctrl Pts',(-10.751121370838,-0.781301481154613,
1.79449671758557));
#50932=CARTESIAN_POINT('Ctrl Pts',(-10.7140725892122,-1.37436410784942,
1.5362846494813));
#50933=CARTESIAN_POINT('Ctrl Pts',(-10.6770238075864,-1.82675899283075,
0.954986286440074));
#50934=CARTESIAN_POINT('Ctrl Pts',(-10.6399750259606,-1.93141620820529,
0.316673182574209));
#50935=CARTESIAN_POINT('Ctrl Pts',(-10.6339399146818,-1.9484644865345,0.212694308141715));
#50936=CARTESIAN_POINT('Ctrl Pts',(-10.627904803403,-1.95628546906628,0.107202534980138));
#50937=CARTESIAN_POINT('Ctrl Pts',(-10.6218696921242,-1.95536008754156,
0.00157356082676479));
#50938=CARTESIAN_POINT('Origin',(-14.8,0.,0.));
#50939=CARTESIAN_POINT('',(-9.82013030787577,-1.95094521463585,0.000565864204244704));
#50940=CARTESIAN_POINT('',(-9.92186969212419,-1.95087369540874,0.000415097647679855));
#50941=CARTESIAN_POINT('',(-14.8,-1.954,-2.39295984553393E-16));
#50942=CARTESIAN_POINT('Ctrl Pts',(-9.82013030787577,-1.95094521463585,
0.000565864204244704));
#50943=CARTESIAN_POINT('Ctrl Pts',(-9.8366642066958,-1.95170031682729,0.291615497447128));
#50944=CARTESIAN_POINT('Ctrl Pts',(-9.85319810551582,-1.89072216247003,
0.582364427271289));
#50945=CARTESIAN_POINT('Ctrl Pts',(-9.86973200433584,-1.76640533997838,
0.842889546046716));
#50946=CARTESIAN_POINT('Ctrl Pts',(-9.90678078596165,-1.48783905267716,
1.42666826264686));
#50947=CARTESIAN_POINT('Ctrl Pts',(-9.94382956758744,-0.891244121992129,
1.85869074709312));
#50948=CARTESIAN_POINT('Ctrl Pts',(-9.98087834921325,-0.249693638224819,
1.941211915008));
#50949=CARTESIAN_POINT('Ctrl Pts',(-10.0179271308391,0.391856845542454,
2.02373308292288));
#50950=CARTESIAN_POINT('Ctrl Pts',(-10.0549759124649,1.07836288239199,1.75675293430644));
#50951=CARTESIAN_POINT('Ctrl Pts',(-10.0920246940907,1.4955973219558,1.26247347001733));
#50952=CARTESIAN_POINT('Ctrl Pts',(-10.1290734757165,1.91283176151965,0.768194005728199));
#50953=CARTESIAN_POINT('Ctrl Pts',(-10.1661222573423,2.06079460379773,0.0466152257663319));
#50954=CARTESIAN_POINT('Ctrl Pts',(-10.2031710389681,1.87176038128685,-0.57198224359142));
#50955=CARTESIAN_POINT('Ctrl Pts',(-10.2402198205939,1.68272615877597,-1.19057971294919));
#50956=CARTESIAN_POINT('Ctrl Pts',(-10.2772686022197,1.15669487147614,-1.70619587170287));
#50957=CARTESIAN_POINT('Ctrl Pts',(-10.3143173838455,0.534441259215129,
-1.88282318670329));
#50958=CARTESIAN_POINT('Ctrl Pts',(-10.3513661654713,-0.0878123530458442,
-2.0594505017037));
#50959=CARTESIAN_POINT('Ctrl Pts',(-10.3884149470971,-0.806288290267959,
-1.89708897295088));
#50960=CARTESIAN_POINT('Ctrl Pts',(-10.4254637287229,-1.29212615757787,
-1.47005462648231));
#50961=CARTESIAN_POINT('Ctrl Pts',(-10.4570192551072,-1.70592841955826,
-1.10633703589916));
#50962=CARTESIAN_POINT('Ctrl Pts',(-10.4885747814915,-1.9509651376568,-0.550614533783712));
#50963=CARTESIAN_POINT('Ctrl Pts',(-10.5201303078758,-1.95562737994549,
0.00148708654483385));
#50964=CARTESIAN_POINT('Ctrl Pts',(-10.6218696921242,-1.95536008754156,
0.00157356082676479));
#50965=CARTESIAN_POINT('Ctrl Pts',(-10.5908560217772,-1.95060466941801,
-0.541240321494284));
#50966=CARTESIAN_POINT('Ctrl Pts',(-10.5598423514302,-1.71487513271243,
-1.08767740974916));
#50967=CARTESIAN_POINT('Ctrl Pts',(-10.5288286810832,-1.31343749192923,
-1.45104528829201));
#50968=CARTESIAN_POINT('Ctrl Pts',(-10.4917798994573,-0.833882014510803,
-1.885122810602));
#50969=CARTESIAN_POINT('Ctrl Pts',(-10.4547311178315,-0.117851513906124,
-2.05795001053151));
#50970=CARTESIAN_POINT('Ctrl Pts',(-10.4176823362057,0.506912938860662,
-1.89042052102051));
#50971=CARTESIAN_POINT('Ctrl Pts',(-10.3806335545799,1.13167739162745,-1.72289103150951));
#50972=CARTESIAN_POINT('Ctrl Pts',(-10.3435847729541,1.66517579655636,-1.21500485255799));
#50973=CARTESIAN_POINT('Ctrl Pts',(-10.3065359913283,1.86321556901111,-0.599231355383206));
#50974=CARTESIAN_POINT('Ctrl Pts',(-10.2694872097025,2.06125534146585,0.0165421417915641));
#50975=CARTESIAN_POINT('Ctrl Pts',(-10.2324384280767,1.92383648144648,0.740202957189575));
#50976=CARTESIAN_POINT('Ctrl Pts',(-10.1953896464509,1.51385827092997,1.24051747646566));
#50977=CARTESIAN_POINT('Ctrl Pts',(-10.1583408648251,1.10388006041343,1.74083199574176));
#50978=CARTESIAN_POINT('Ctrl Pts',(-10.1212920831993,0.421342499399717,
2.01780021889587));
#50979=CARTESIAN_POINT('Ctrl Pts',(-10.0842433015735,-0.221343710231941,
1.94464840930708));
#50980=CARTESIAN_POINT('Ctrl Pts',(-10.0471945199477,-0.864029919863581,
1.87149659971829));
#50981=CARTESIAN_POINT('Ctrl Pts',(-10.0101457383219,-1.46686477811318,
1.44822475738663));
#50982=CARTESIAN_POINT('Ctrl Pts',(-9.97309695669604,-1.75391905860483,
0.868572627787997));
#50983=CARTESIAN_POINT('Ctrl Pts',(-9.95602120183876,-1.88622215493648,
0.601411408628383));
#50984=CARTESIAN_POINT('Ctrl Pts',(-9.93894544698147,-1.95144458357273,
0.301030622392327));
#50985=CARTESIAN_POINT('Ctrl Pts',(-9.92186969212419,-1.95087369540874,
0.000415097647679855));
#50986=CARTESIAN_POINT('Origin',(-14.8,0.,0.));
#50987=CARTESIAN_POINT('',(-9.12013030787577,-1.9535529839402,-0.00178040573474675));
#50988=CARTESIAN_POINT('',(-9.22186969212419,-1.95383722770402,-0.00178766236736636));
#50989=CARTESIAN_POINT('',(-14.8,-1.954,-2.39295984553393E-16));
#50990=CARTESIAN_POINT('Ctrl Pts',(-9.12013030787577,-1.9535529839402,-0.00178040573474675));
#50991=CARTESIAN_POINT('Ctrl Pts',(-9.14770485027428,-1.94921168804754,
0.481988254547837));
#50992=CARTESIAN_POINT('Ctrl Pts',(-9.17527939267279,-1.76751241565099,
0.968669397052054));
#50993=CARTESIAN_POINT('Ctrl Pts',(-9.2028539350713,-1.4419965923978,1.32336557286795));
#50994=CARTESIAN_POINT('Ctrl Pts',(-9.2399027166971,-1.00463794190191,1.79993054977301));
#50995=CARTESIAN_POINT('Ctrl Pts',(-9.27695149832291,-0.307658121980692,
2.03823302355113));
#50996=CARTESIAN_POINT('Ctrl Pts',(-9.31400027994872,0.329921663003375,
1.92919732226127));
#50997=CARTESIAN_POINT('Ctrl Pts',(-9.35104906157453,0.967501447987441,
1.82016162097141));
#50998=CARTESIAN_POINT('Ctrl Pts',(-9.38809784320034,1.54568119803435,1.36378774461357));
#50999=CARTESIAN_POINT('Ctrl Pts',(-9.42514662482614,1.79981680878709,0.768966882737124));
#51000=CARTESIAN_POINT('Ctrl Pts',(-9.46219540645195,2.05395241953981,0.174146020860696));
#51001=CARTESIAN_POINT('Ctrl Pts',(-9.49924418807775,1.98404389099838,-0.559121826534324));
#51002=CARTESIAN_POINT('Ctrl Pts',(-9.53629296970356,1.62208971484511,-1.09520571991416));
#51003=CARTESIAN_POINT('Ctrl Pts',(-9.57334175132937,1.26013553869183,-1.63128961329401));
#51004=CARTESIAN_POINT('Ctrl Pts',(-9.61039053295519,0.606135714926695,
-1.97018955265867));
#51005=CARTESIAN_POINT('Ctrl Pts',(-9.64743931458099,-0.0405613313352086,
-1.95678445168069));
#51006=CARTESIAN_POINT('Ctrl Pts',(-9.6844880962068,-0.687258377597112,
-1.94337935070271));
#51007=CARTESIAN_POINT('Ctrl Pts',(-9.7215368778326,-1.32665264635579,-1.57766920938208));
#51008=CARTESIAN_POINT('Ctrl Pts',(-9.75858565945841,-1.66608095877641,
-1.02704666434474));
#51009=CARTESIAN_POINT('Ctrl Pts',(-9.77910054226419,-1.8540313243405,-0.722152508964587));
#51010=CARTESIAN_POINT('Ctrl Pts',(-9.79961542506998,-1.95000830113878,
-0.360561851747099));
#51011=CARTESIAN_POINT('Ctrl Pts',(-9.82013030787577,-1.95094521463585,
0.000565864204244704));
#51012=CARTESIAN_POINT('Ctrl Pts',(-9.92186969212419,-1.95087369540874,
0.000415097647679855));
#51013=CARTESIAN_POINT('Ctrl Pts',(-9.90189666535567,-1.95020594369431,
-0.351206366407061));
#51014=CARTESIAN_POINT('Ctrl Pts',(-9.88192363858714,-1.85952426139783,
-0.703148983685942));
#51015=CARTESIAN_POINT('Ctrl Pts',(-9.86195061181862,-1.68088875115348,
-1.00262828611878));
#51016=CARTESIAN_POINT('Ctrl Pts',(-9.82490183019282,-1.34953046047678,
-1.55814465356138));
#51017=CARTESIAN_POINT('Ctrl Pts',(-9.78785304856701,-0.715540176389686,
-1.93314497158098));
#51018=CARTESIAN_POINT('Ctrl Pts',(-9.7508042669412,-0.0691075689552816,
-1.95598430918883));
#51019=CARTESIAN_POINT('Ctrl Pts',(-9.71375548531539,0.577325038479105,
-1.97882364679667));
#51020=CARTESIAN_POINT('Ctrl Pts',(-9.67670670368958,1.23619996926078,-1.64950200399279));
#51021=CARTESIAN_POINT('Ctrl Pts',(-9.63965792206377,1.60593736708061,-1.11875629468351));
#51022=CARTESIAN_POINT('Ctrl Pts',(-9.60260914043797,1.97567476490046,-0.588010585374225));
#51023=CARTESIAN_POINT('Ctrl Pts',(-9.56556035881216,2.05627462975842,0.14415919044051));
#51024=CARTESIAN_POINT('Ctrl Pts',(-9.52851157718636,1.81084483763096,0.742624701922234));
#51025=CARTESIAN_POINT('Ctrl Pts',(-9.49146279556055,1.56541504550351,1.34109021340394));
#51026=CARTESIAN_POINT('Ctrl Pts',(-9.45441401393473,0.993955596390669,
1.80585146055268));
#51027=CARTESIAN_POINT('Ctrl Pts',(-9.41736523230892,0.358034582351254,
1.92417819125994));
#51028=CARTESIAN_POINT('Ctrl Pts',(-9.38031645068311,-0.277886431688179,
2.04250492196719));
#51029=CARTESIAN_POINT('Ctrl Pts',(-9.34326766905731,-0.978269010654174,
1.81439713623294));
#51030=CARTESIAN_POINT('Ctrl Pts',(-9.30621888743151,-1.42253444126134,
1.34426419922019));
#51031=CARTESIAN_POINT('Ctrl Pts',(-9.27810248899574,-1.75968841259436,
0.987479322774409));
#51032=CARTESIAN_POINT('Ctrl Pts',(-9.24998609055996,-1.94933621795992,
0.491304318172266));
#51033=CARTESIAN_POINT('Ctrl Pts',(-9.22186969212419,-1.95383722770402,
-0.00178766236736636));
#51034=CARTESIAN_POINT('Origin',(-14.8,0.,0.));
#51035=CARTESIAN_POINT('',(-8.42013030787577,-1.95704676357205,0.000502930207441042));
#51036=CARTESIAN_POINT('',(-8.52186969212418,-1.95692604939057,0.000668243846604161));
#51037=CARTESIAN_POINT('',(-14.8,-1.954,-2.39295984553393E-16));
#51038=CARTESIAN_POINT('Ctrl Pts',(-8.42013030787577,-1.95704676357205,
0.000502930207441042));
#51039=CARTESIAN_POINT('Ctrl Pts',(-8.42169671222696,-1.95714101498148,
0.0278567662564005));
#51040=CARTESIAN_POINT('Ctrl Pts',(-8.42326311657814,-1.95661716157646,
0.0552069111146564));
#51041=CARTESIAN_POINT('Ctrl Pts',(-8.42482952092933,-1.95546396780841,
0.0825304946185233));
#51042=CARTESIAN_POINT('Ctrl Pts',(-8.46187830255513,-1.92818849193753,
0.728791134602187));
#51043=CARTESIAN_POINT('Ctrl Pts',(-8.49892708418095,-1.54884571939758,
1.36019274950974));
#51044=CARTESIAN_POINT('Ctrl Pts',(-8.53597586580676,-0.991068206975607,
1.6877305534537));
#51045=CARTESIAN_POINT('Ctrl Pts',(-8.57302464743257,-0.433290694553603,
2.01526835739768));
#51046=CARTESIAN_POINT('Ctrl Pts',(-8.61007342905837,0.302921557750443,
2.03894235037805));
#51047=CARTESIAN_POINT('Ctrl Pts',(-8.64712221068418,0.880589899072553,
1.74791648587407));
#51048=CARTESIAN_POINT('Ctrl Pts',(-8.68417099230999,1.45825824039463,1.45689062137012));
#51049=CARTESIAN_POINT('Ctrl Pts',(-8.7212197739358,1.8773826707348,0.851164899381864));
#51050=CARTESIAN_POINT('Ctrl Pts',(-8.75826855556161,1.94612179566075,0.207991750781512));
#51051=CARTESIAN_POINT('Ctrl Pts',(-8.79531733718741,2.0148609205867,-0.435181397818841));
#51052=CARTESIAN_POINT('Ctrl Pts',(-8.83236611881321,1.73321474009845,-1.11580197303129));
#51053=CARTESIAN_POINT('Ctrl Pts',(-8.86941490043902,1.23009818277112,-1.52233671462071));
#51054=CARTESIAN_POINT('Ctrl Pts',(-8.90646368206483,0.726981625443756,
-1.92887145621015));
#51055=CARTESIAN_POINT('Ctrl Pts',(-8.94351246369065,0.00239469127729805,
-2.06132036417651));
#51056=CARTESIAN_POINT('Ctrl Pts',(-8.98056124531646,-0.612005102830212,
-1.8590590001527));
#51057=CARTESIAN_POINT('Ctrl Pts',(-9.01761002694226,-1.22640489693769,
-1.6567976361289));
#51058=CARTESIAN_POINT('Ctrl Pts',(-9.05465880856807,-1.73061755098623,
-1.11982600011496));
#51059=CARTESIAN_POINT('Ctrl Pts',(-9.09170759019387,-1.89385513747523,
-0.493926442092014));
#51060=CARTESIAN_POINT('Ctrl Pts',(-9.10118182942117,-1.93559880291891,
-0.333869298921619));
#51061=CARTESIAN_POINT('Ctrl Pts',(-9.11065606864847,-1.95504459439919,
-0.167996763995528));
#51062=CARTESIAN_POINT('Ctrl Pts',(-9.12013030787577,-1.9535529839402,-0.00178040573474675));
#51063=CARTESIAN_POINT('Ctrl Pts',(-9.22186969212419,-1.95383722770402,
-0.00178766236736636));
#51064=CARTESIAN_POINT('Ctrl Pts',(-9.21293730893415,-1.95526716702816,
-0.158439536830396));
#51065=CARTESIAN_POINT('Ctrl Pts',(-9.20400492574411,-1.93801045369618,
-0.314780245228718));
#51066=CARTESIAN_POINT('Ctrl Pts',(-9.19507254255408,-1.90086016391406,
-0.466241472977706));
#51067=CARTESIAN_POINT('Ctrl Pts',(-9.15802376092827,-1.7467721737113,-1.09445611987165));
#51068=CARTESIAN_POINT('Ctrl Pts',(-9.12097497930247,-1.25044791105744,
-1.63872732536828));
#51069=CARTESIAN_POINT('Ctrl Pts',(-9.08392619767666,-0.639064633457673,
-1.84993158471966));
#51070=CARTESIAN_POINT('Ctrl Pts',(-9.04687741605085,-0.0276813558578867,
-2.06113584407105));
#51071=CARTESIAN_POINT('Ctrl Pts',(-9.00982863442504,0.698760936687822,
-1.93927315727717));
#51072=CARTESIAN_POINT('Ctrl Pts',(-8.97277985279923,1.20775549370569,-1.54012244360749));
#51073=CARTESIAN_POINT('Ctrl Pts',(-8.93573107117342,1.71675005072351,-1.14097172993785));
#51074=CARTESIAN_POINT('Ctrl Pts',(-8.89868228954762,2.00829687221353,-0.464532989392456));
#51075=CARTESIAN_POINT('Ctrl Pts',(-8.86163350792181,1.94894931386644,0.179574624764523));
#51076=CARTESIAN_POINT('Ctrl Pts',(-8.824584726296,1.88960175551935,0.823682238921539));
#51077=CARTESIAN_POINT('Ctrl Pts',(-8.7875359446702,1.4793598173351,1.43545872669014));
#51078=CARTESIAN_POINT('Ctrl Pts',(-8.75048716304439,0.905999204518953,
1.73488210414737));
#51079=CARTESIAN_POINT('Ctrl Pts',(-8.71343838141858,0.332638591702826,
2.0343054816046));
#51080=CARTESIAN_POINT('Ctrl Pts',(-8.67638959979277,-0.403840695745188,
2.02137574875049));
#51081=CARTESIAN_POINT('Ctrl Pts',(-8.63934081816697,-0.966337779787842,
1.70201109550863));
#51082=CARTESIAN_POINT('Ctrl Pts',(-8.60229203654116,-1.52883486383051,
1.38264644226677));
#51083=CARTESIAN_POINT('Ctrl Pts',(-8.56524325491535,-1.91734974446781,
0.756846868637128));
#51084=CARTESIAN_POINT('Ctrl Pts',(-8.52819447328954,-1.95405161284264,
0.111052997378969));
#51085=CARTESIAN_POINT('Ctrl Pts',(-8.52608621290109,-1.95614013213751,
0.0743041063727897));
#51086=CARTESIAN_POINT('Ctrl Pts',(-8.52397795251263,-1.9570894184881,0.0374904702839609));
#51087=CARTESIAN_POINT('Ctrl Pts',(-8.52186969212418,-1.95692604939057,
0.000668243846604161));
#51088=CARTESIAN_POINT('Origin',(-14.8,0.,0.));
#51089=CARTESIAN_POINT('',(-7.72013030787578,-1.95207303808925,0.00146614720672802));
#51090=CARTESIAN_POINT('',(-7.82186969212419,-1.95186016998754,0.00136964534846597));
#51091=CARTESIAN_POINT('',(-14.8,-1.954,-2.39295984553393E-16));
#51092=CARTESIAN_POINT('Ctrl Pts',(-7.72013030787578,-1.95207303808925,
0.00146614720672802));
#51093=CARTESIAN_POINT('Ctrl Pts',(-7.73273735580545,-1.95361829365223,
0.223069353944344));
#51094=CARTESIAN_POINT('Ctrl Pts',(-7.74534440373512,-1.91879720445243,
0.444201465762539));
#51095=CARTESIAN_POINT('Ctrl Pts',(-7.75795145166479,-1.84550193984431,
0.651746271159146));
#51096=CARTESIAN_POINT('Ctrl Pts',(-7.7950002332906,-1.63010653024322,1.26166559688908));
#51097=CARTESIAN_POINT('Ctrl Pts',(-7.8320490149164,-1.08244170036397,1.75424266953811));
#51098=CARTESIAN_POINT('Ctrl Pts',(-7.86909779654221,-0.453184282765084,
1.90401539326595));
#51099=CARTESIAN_POINT('Ctrl Pts',(-7.90614657816802,0.176073134833824,
2.05378811699378));
#51100=CARTESIAN_POINT('Ctrl Pts',(-7.94319535979383,0.886923140152381,
1.8607564918004));
#51101=CARTESIAN_POINT('Ctrl Pts',(-7.98024414141964,1.35399587550455,1.41327484271661));
#51102=CARTESIAN_POINT('Ctrl Pts',(-8.01729292304545,1.82106861085671,0.965793193632821));
#51103=CARTESIAN_POINT('Ctrl Pts',(-8.05434170467126,2.04436407624249,0.263861520658632));
#51104=CARTESIAN_POINT('Ctrl Pts',(-8.09139048629706,1.92167559901516,-0.371232412497511));
#51105=CARTESIAN_POINT('Ctrl Pts',(-8.12843926792287,1.79898712178783,-1.00632634565364));
#51106=CARTESIAN_POINT('Ctrl Pts',(-8.16548804954867,1.33031470194742,-1.57458253899172));
#51107=CARTESIAN_POINT('Ctrl Pts',(-8.20253683117448,0.730178811328908,
-1.81589909285326));
#51108=CARTESIAN_POINT('Ctrl Pts',(-8.23958561280029,0.130042920710383,
-2.0572156467148));
#51109=CARTESIAN_POINT('Ctrl Pts',(-8.27663439442611,-0.601556440686245,
-1.97159256109978));
#51110=CARTESIAN_POINT('Ctrl Pts',(-8.31368317605191,-1.12975203178366,
-1.59822118576237));
#51111=CARTESIAN_POINT('Ctrl Pts',(-8.34916555332654,-1.63561577184945,
-1.24063576940312));
#51112=CARTESIAN_POINT('Ctrl Pts',(-8.38464793060115,-1.95491176945909,
-0.619119410514391));
#51113=CARTESIAN_POINT('Ctrl Pts',(-8.42013030787577,-1.95704676357205,
0.000502930207441042));
#51114=CARTESIAN_POINT('Ctrl Pts',(-8.52186969212418,-1.95692604939057,
0.000668243846604161));
#51115=CARTESIAN_POINT('Ctrl Pts',(-8.48692917088682,-1.95421850839941,
-0.609592135700733));
#51116=CARTESIAN_POINT('Ctrl Pts',(-8.45198864964947,-1.64589857568518,
-1.22221202102663));
#51117=CARTESIAN_POINT('Ctrl Pts',(-8.41704812841211,-1.15295067365337,
-1.58156732958228));
#51118=CARTESIAN_POINT('Ctrl Pts',(-8.37999934678631,-0.630259009976949,
-1.96260561639862));
#51119=CARTESIAN_POINT('Ctrl Pts',(-8.34295056516051,0.100013173488252,
-2.05889402114469));
#51120=CARTESIAN_POINT('Ctrl Pts',(-8.3059017835347,0.703606110788312,-1.82635947029634));
#51121=CARTESIAN_POINT('Ctrl Pts',(-8.26885300190889,1.30719904808841,-1.59382491944798));
#51122=CARTESIAN_POINT('Ctrl Pts',(-8.23180422028307,1.78411273922334,-1.03246741300516));
#51123=CARTESIAN_POINT('Ctrl Pts',(-8.19475543865726,1.91605452237685,-0.399231187608135));
#51124=CARTESIAN_POINT('Ctrl Pts',(-8.15770665703146,2.04799630553036,0.234005037788894));
#51125=CARTESIAN_POINT('Ctrl Pts',(-8.12065787540566,1.83496618070244,0.939119982140134));
#51126=CARTESIAN_POINT('Ctrl Pts',(-8.08360909377985,1.3744721747335,1.3933688365839));
#51127=CARTESIAN_POINT('Ctrl Pts',(-8.04656031215404,0.913978168764561,
1.84761769102765));
#51128=CARTESIAN_POINT('Ctrl Pts',(-8.00951153052823,0.206020281654609,
2.05100045556395));
#51129=CARTESIAN_POINT('Ctrl Pts',(-7.97246274890242,-0.425355407601904,
1.91042488758486));
#51130=CARTESIAN_POINT('Ctrl Pts',(-7.93541396727661,-1.05673109685843,
1.76984931960576));
#51131=CARTESIAN_POINT('Ctrl Pts',(-7.89836518565081,-1.61152458826152,
1.28531541911125));
#51132=CARTESIAN_POINT('Ctrl Pts',(-7.861316404025,-1.83579612237898,0.678603765785385));
#51133=CARTESIAN_POINT('Ctrl Pts',(-7.84816750005806,-1.91539185360739,
0.463277028572364));
#51134=CARTESIAN_POINT('Ctrl Pts',(-7.83501859609112,-1.95335517386918,
0.232560831431699));
#51135=CARTESIAN_POINT('Ctrl Pts',(-7.82186969212419,-1.95186016998754,
0.00136964534846597));
#51136=CARTESIAN_POINT('Origin',(-14.8,0.,0.));
#51137=CARTESIAN_POINT('',(-7.02013030787579,-1.95176668991016,-0.00132109256869101));
#51138=CARTESIAN_POINT('',(-7.12186969212419,-1.9519719800925,-0.00142259664250751));
#51139=CARTESIAN_POINT('',(-14.8,-1.954,-2.39295984553393E-16));
#51140=CARTESIAN_POINT('Ctrl Pts',(-7.02013030787579,-1.95176668991016,
-0.00132109256869101));
#51141=CARTESIAN_POINT('Ctrl Pts',(-7.04377799938394,-1.94918116590277,
0.414515544669262));
#51142=CARTESIAN_POINT('Ctrl Pts',(-7.0674256908921,-1.81911222147843,0.831829046295296));
#51143=CARTESIAN_POINT('Ctrl Pts',(-7.09107338240025,-1.57361703474163,
1.16377834655484));
#51144=CARTESIAN_POINT('Ctrl Pts',(-7.12812216402606,-1.18900031388915,
1.68384251991882));
#51145=CARTESIAN_POINT('Ctrl Pts',(-7.16517094565186,-0.521065104670545,
1.99437672845672));
#51146=CARTESIAN_POINT('Ctrl Pts',(-7.20221972727767,0.124461671143169,
1.95324343192425));
#51147=CARTESIAN_POINT('Ctrl Pts',(-7.23926850890348,0.769988446956902,
1.91211013539178));
#51148=CARTESIAN_POINT('Ctrl Pts',(-7.2763172905293,1.39310678936575,1.51930933378892));
#51149=CARTESIAN_POINT('Ctrl Pts',(-7.31336607215511,1.70860332723064,0.954633585264722));
#51150=CARTESIAN_POINT('Ctrl Pts',(-7.35041485378091,2.02409986509553,0.389957836740521));
#51151=CARTESIAN_POINT('Ctrl Pts',(-7.38746363540671,2.03197459841647,-0.346592858705026));
#51152=CARTESIAN_POINT('Ctrl Pts',(-7.42451241703252,1.72862310876371,-0.917884938206884));
#51153=CARTESIAN_POINT('Ctrl Pts',(-7.46156119865832,1.42527161911097,-1.48917701770873));
#51154=CARTESIAN_POINT('Ctrl Pts',(-7.49860998028414,0.810693906484552,
-1.89521048126689));
#51155=CARTESIAN_POINT('Ctrl Pts',(-7.53565876190995,0.166194129846451,
-1.95013592427388));
#51156=CARTESIAN_POINT('Ctrl Pts',(-7.57270754353575,-0.478305646791669,
-2.00506136728088));
#51157=CARTESIAN_POINT('Ctrl Pts',(-7.60975632516156,-1.15272748744147,
-1.70887878973669));
#51158=CARTESIAN_POINT('Ctrl Pts',(-7.64680510678737,-1.54837541310491,
-1.19715671155917));
#51159=CARTESIAN_POINT('Ctrl Pts',(-7.6712468404835,-1.80939131732991,-0.859564644765363));
#51160=CARTESIAN_POINT('Ctrl Pts',(-7.69568857417964,-1.94907719598778,
-0.428163897471984));
#51161=CARTESIAN_POINT('Ctrl Pts',(-7.72013030787578,-1.95207303808925,
0.00146614720672802));
#51162=CARTESIAN_POINT('Ctrl Pts',(-7.82186969212419,-1.95186016998754,
0.00136964534846597));
#51163=CARTESIAN_POINT('Ctrl Pts',(-7.79796981446532,-1.94914280206391,
-0.418851011604582));
#51164=CARTESIAN_POINT('Ctrl Pts',(-7.77406993680645,-1.81606347314505,
-0.840640931605373));
#51165=CARTESIAN_POINT('Ctrl Pts',(-7.75017005914758,-1.56567773577053,
-1.17443761077048));
#51166=CARTESIAN_POINT('Ctrl Pts',(-7.71312127752177,-1.17753823821277,
-1.69187792784332));
#51167=CARTESIAN_POINT('Ctrl Pts',(-7.67607249589596,-0.507509666265409,
-1.99786915583173));
#51168=CARTESIAN_POINT('Ctrl Pts',(-7.63902371427015,0.137722885510151,
-1.95235316494904));
#51169=CARTESIAN_POINT('Ctrl Pts',(-7.60197493264435,0.782955437285656,
-1.90683717406636));
#51170=CARTESIAN_POINT('Ctrl Pts',(-7.56492615101854,1.40339196888934,-1.50981396431264));
#51171=CARTESIAN_POINT('Ctrl Pts',(-7.52787736939273,1.7150466260894,-0.943008772079646));
#51172=CARTESIAN_POINT('Ctrl Pts',(-7.49082858776692,2.02670128328947,-0.376203579846622));
#51173=CARTESIAN_POINT('Ctrl Pts',(-7.45377980614111,2.02957406608585,0.360383594865731));
#51174=CARTESIAN_POINT('Ctrl Pts',(-7.41673102451531,1.72235004598079,0.929602491923175));
#51175=CARTESIAN_POINT('Ctrl Pts',(-7.3796822428895,1.41512602587571,1.49882138898064));
#51176=CARTESIAN_POINT('Ctrl Pts',(-7.34263346126368,0.797805202869196,
1.90067200838321));
#51177=CARTESIAN_POINT('Ctrl Pts',(-7.30558467963788,0.152947310836807,
1.95121951455688));
#51178=CARTESIAN_POINT('Ctrl Pts',(-7.26853589801207,-0.491910581195545,
2.00176702073054));
#51179=CARTESIAN_POINT('Ctrl Pts',(-7.23148711638627,-1.16430554225374,
1.70101141367534));
#51180=CARTESIAN_POINT('Ctrl Pts',(-7.19443833476046,-1.55646933550666,
1.18661437776021));
#51181=CARTESIAN_POINT('Ctrl Pts',(-7.17024878721504,-1.81251728920985,
0.850759026748462));
#51182=CARTESIAN_POINT('Ctrl Pts',(-7.14605923966961,-1.94910481502684,
0.423829950049081));
#51183=CARTESIAN_POINT('Ctrl Pts',(-7.12186969212419,-1.9519719800925,-0.00142259664250751));
#51184=CARTESIAN_POINT('Origin',(-14.8,0.,0.));
#51185=CARTESIAN_POINT('',(-6.32013030787579,-1.95685981962429,-0.000742816091480747));
#51186=CARTESIAN_POINT('',(-6.4218696921242,-1.95699436955386,-0.000580667263057569));
#51187=CARTESIAN_POINT('',(-14.8,-1.954,-2.39295984553393E-16));
#51188=CARTESIAN_POINT('Ctrl Pts',(-6.32013030787579,-1.95685981962429,
-0.000742816091480747));
#51189=CARTESIAN_POINT('Ctrl Pts',(-6.35481864296243,-1.9539129004879,0.60516754541605));
#51190=CARTESIAN_POINT('Ctrl Pts',(-6.38950697804907,-1.65062025506416,
1.21362467071175));
#51191=CARTESIAN_POINT('Ctrl Pts',(-6.42419531313571,-1.16366421853117,
1.57370143243539));
#51192=CARTESIAN_POINT('Ctrl Pts',(-6.46124409476151,-0.643572152601299,
1.95828043515508));
#51193=CARTESIAN_POINT('Ctrl Pts',(-6.49829287638732,0.0860293302205446,
2.05952575430774));
#51194=CARTESIAN_POINT('Ctrl Pts',(-6.53534165801313,0.691187456695122,
1.83109544034338));
#51195=CARTESIAN_POINT('Ctrl Pts',(-6.57239043963894,1.29634558316972,1.60266512637901));
#51196=CARTESIAN_POINT('Ctrl Pts',(-6.60943922126475,1.77706035329704,1.04455917929761));
#51197=CARTESIAN_POINT('Ctrl Pts',(-6.64648800289056,1.9132992775594,0.412233533849047));
#51198=CARTESIAN_POINT('Ctrl Pts',(-6.68353678451637,2.04953820182175,-0.22009211159951));
#51199=CARTESIAN_POINT('Ctrl Pts',(-6.72058556614217,1.84130128021915,-0.926637455415224));
#51200=CARTESIAN_POINT('Ctrl Pts',(-6.75763434776798,1.38390259735436,-1.384002967112));
#51201=CARTESIAN_POINT('Ctrl Pts',(-6.79468312939378,0.926503914489585,
-1.84136847880877));
#51202=CARTESIAN_POINT('Ctrl Pts',(-6.83173191101959,0.219943470362641,
-2.04955415838662));
#51203=CARTESIAN_POINT('Ctrl Pts',(-6.8687806926454,-0.412372292834584,
-1.91326937571303));
#51204=CARTESIAN_POINT('Ctrl Pts',(-6.90582947427121,-1.04468805603181,
-1.77698459303944));
#51205=CARTESIAN_POINT('Ctrl Pts',(-6.94287825589702,-1.60275913829931,
-1.2962293481144));
#51206=CARTESIAN_POINT('Ctrl Pts',(-6.97992703752283,-1.8311455631899,-0.691054656556856));
#51207=CARTESIAN_POINT('Ctrl Pts',(-6.99332812764048,-1.91375629766748,
-0.472154055171452));
#51208=CARTESIAN_POINT('Ctrl Pts',(-7.00672921775813,-1.95323190017021,
-0.23697471854422));
#51209=CARTESIAN_POINT('Ctrl Pts',(-7.02013030787579,-1.95176668991016,
-0.00132109256869101));
#51210=CARTESIAN_POINT('Ctrl Pts',(-7.12186969212419,-1.9519719800925,-0.00142259664250751));
#51211=CARTESIAN_POINT('Ctrl Pts',(-7.1090104580438,-1.95349617341018,-0.227488091704733));
#51212=CARTESIAN_POINT('Ctrl Pts',(-7.09615122396341,-1.91723077036094,
-0.453079796598166));
#51213=CARTESIAN_POINT('Ctrl Pts',(-7.08329198988303,-1.84103347457747,
-0.66426366705173));
#51214=CARTESIAN_POINT('Ctrl Pts',(-7.04624320825722,-1.62150119494774,
-1.27270621117352));
#51215=CARTESIAN_POINT('Ctrl Pts',(-7.00919442663142,-1.07050401024064,
-1.76155283464202));
#51216=CARTESIAN_POINT('Ctrl Pts',(-6.97214564500561,-0.440244036559741,
-1.90704894068122));
#51217=CARTESIAN_POINT('Ctrl Pts',(-6.9350968633798,0.190015937121125,-2.05254504672042));
#51218=CARTESIAN_POINT('Ctrl Pts',(-6.89804808175399,0.899538699775802,
-1.85469063533038));
#51219=CARTESIAN_POINT('Ctrl Pts',(-6.86099930012818,1.36356189847091,-1.40404751448026));
#51220=CARTESIAN_POINT('Ctrl Pts',(-6.82395051850237,1.82758509716603,-0.95340439363013));
#51221=CARTESIAN_POINT('Ctrl Pts',(-6.78690173687657,2.04610873190157,-0.249972563319941));
#51222=CARTESIAN_POINT('Ctrl Pts',(-6.74985295525077,1.91911028962563,0.384273561584486));
#51223=CARTESIAN_POINT('Ctrl Pts',(-6.71280417362496,1.79211184734969,1.0185196864889));
#51224=CARTESIAN_POINT('Ctrl Pts',(-6.67575539199914,1.31959132806222,1.58358010598756));
#51225=CARTESIAN_POINT('Ctrl Pts',(-6.63870661037333,0.717830553475292,
1.82081568819503));
#51226=CARTESIAN_POINT('Ctrl Pts',(-6.60165782874752,0.11606977888833,2.05805127040252));
#51227=CARTESIAN_POINT('Ctrl Pts',(-6.56460904712172,-0.614931250998082,
1.96746201531886));
#51228=CARTESIAN_POINT('Ctrl Pts',(-6.52756026549591,-1.14057916306319,
1.59051238494576));
#51229=CARTESIAN_POINT('Ctrl Pts',(-6.49233007437201,-1.64042492298516,
1.23206584664237));
#51230=CARTESIAN_POINT('Ctrl Pts',(-6.45709988324811,-1.95458285395145,
0.614681742887991));
#51231=CARTESIAN_POINT('Ctrl Pts',(-6.4218696921242,-1.95699436955386,-0.000580667263057569));
#51232=CARTESIAN_POINT('Origin',(-14.8,0.,0.));
#51233=CARTESIAN_POINT('',(-5.62013030787578,-1.95397084692293,0.00178599170134505));
#51234=CARTESIAN_POINT('',(-5.7218696921242,-1.9536847040016,0.00178561523945243));
#51235=CARTESIAN_POINT('',(-14.8,-1.954,-2.39295984553393E-16));
#51236=CARTESIAN_POINT('Ctrl Pts',(-5.62013030787578,-1.95397084692293,
0.00178599170134505));
#51237=CARTESIAN_POINT('Ctrl Pts',(-5.6288105049151,-1.95536772671579,0.153988559362694));
#51238=CARTESIAN_POINT('Ctrl Pts',(-5.63749070195442,-1.93908361863309,
0.305895547971744));
#51239=CARTESIAN_POINT('Ctrl Pts',(-5.64617089899374,-1.90398252153289,
0.45332236833873));
#51240=CARTESIAN_POINT('Ctrl Pts',(-5.68321968061955,-1.75416416194949,
1.08256892216945));
#51241=CARTESIAN_POINT('Ctrl Pts',(-5.72026846224536,-1.26154737176521,
1.63019802696095));
#51242=CARTESIAN_POINT('Ctrl Pts',(-5.75731724387117,-0.651612426307885,
1.84554920222142));
#51243=CARTESIAN_POINT('Ctrl Pts',(-5.79436602549697,-0.0416774808505747,
2.06090037748189));
#51244=CARTESIAN_POINT('Ctrl Pts',(-5.83141480712278,0.68557561987972,1.94397362321138));
#51245=CARTESIAN_POINT('Ctrl Pts',(-5.86846358874859,1.19726900275107,1.54828858646908));
#51246=CARTESIAN_POINT('Ctrl Pts',(-5.9055123703744,1.70896238562244,1.15260354972677));
#51247=CARTESIAN_POINT('Ctrl Pts',(-5.94256115200021,2.00509605063479,0.478160230512601));
#51248=CARTESIAN_POINT('Ctrl Pts',(-5.97960993362602,1.95012386608632,-0.166335561019096));
#51249=CARTESIAN_POINT('Ctrl Pts',(-6.01665871525182,1.89515168153785,-0.810831352550793));
#51250=CARTESIAN_POINT('Ctrl Pts',(-6.05370749687763,1.48907364742859,-1.42537961640006));
#51251=CARTESIAN_POINT('Ctrl Pts',(-6.09075627850344,0.917759569173183,
-1.72868967288233));
#51252=CARTESIAN_POINT('Ctrl Pts',(-6.12780506012924,0.346445490917778,
-2.0319997293646));
#51253=CARTESIAN_POINT('Ctrl Pts',(-6.16485384175505,-0.390104631483775,
-2.02407157847987));
#51254=CARTESIAN_POINT('Ctrl Pts',(-6.20190262338086,-0.954757497459811,
-1.7085340889146));
#51255=CARTESIAN_POINT('Ctrl Pts',(-6.23895140500667,-1.51941036343583,
-1.39299659934935));
#51256=CARTESIAN_POINT('Ctrl Pts',(-6.27600018663248,-1.91216597298635,
-0.769849771103581));
#51257=CARTESIAN_POINT('Ctrl Pts',(-6.31304896825829,-1.95325245324266,
-0.124320013837331));
#51258=CARTESIAN_POINT('Ctrl Pts',(-6.31540941479745,-1.95587014904456,
-0.0831921166541531));
#51259=CARTESIAN_POINT('Ctrl Pts',(-6.31776986133662,-1.95706034942947,
-0.0419733626799344));
#51260=CARTESIAN_POINT('Ctrl Pts',(-6.32013030787579,-1.95685981962429,
-0.000742816091480747));
#51261=CARTESIAN_POINT('Ctrl Pts',(-6.4218696921242,-1.95699436955386,-0.000580667263057569));
#51262=CARTESIAN_POINT('Ctrl Pts',(-6.4200511016223,-1.95711885253933,-0.032340653217794));
#51263=CARTESIAN_POINT('Ctrl Pts',(-6.4182325111204,-1.95641264107839,-0.0640949856060214));
#51264=CARTESIAN_POINT('Ctrl Pts',(-6.41641392061849,-1.95485839584589,
-0.0958077557958485));
#51265=CARTESIAN_POINT('Ctrl Pts',(-6.37936513899268,-1.92319492231974,
-0.741868260501935));
#51266=CARTESIAN_POINT('Ctrl Pts',(-6.34231635736687,-1.53957318102366,
-1.3706792642516));
#51267=CARTESIAN_POINT('Ctrl Pts',(-6.30526757574106,-0.979584295875341,
-1.69442175421417));
#51268=CARTESIAN_POINT('Ctrl Pts',(-6.26821879411526,-0.419595410727051,
-2.01816424417671));
#51269=CARTESIAN_POINT('Ctrl Pts',(-6.23117001248945,0.316760618273472,
-2.03683822035221));
#51270=CARTESIAN_POINT('Ctrl Pts',(-6.19412123086365,0.892439330875022,
-1.74189624105086));
#51271=CARTESIAN_POINT('Ctrl Pts',(-6.15707244923784,1.46811804347659,-1.44695426174951));
#51272=CARTESIAN_POINT('Ctrl Pts',(-6.12002366761203,1.88311943967917,-0.838396326971331));
#51273=CARTESIAN_POINT('Ctrl Pts',(-6.08297488598622,1.94748931787675,-0.194771226406078));
#51274=CARTESIAN_POINT('Ctrl Pts',(-6.04592610436041,2.01185919607434,0.448853874159157));
#51275=CARTESIAN_POINT('Ctrl Pts',(-6.00887732273461,1.72559755626691,1.12754614051143));
#51276=CARTESIAN_POINT('Ctrl Pts',(-5.9718285411088,1.21973191242823,1.53065493684369));
#51277=CARTESIAN_POINT('Ctrl Pts',(-5.93477975948299,0.713866268589532,
1.93376373317597));
#51278=CARTESIAN_POINT('Ctrl Pts',(-5.89773097785719,-0.0116033792804625,
2.06128905948823));
#51279=CARTESIAN_POINT('Ctrl Pts',(-5.86068219623138,-0.624615479072405,
1.85486009639081));
#51280=CARTESIAN_POINT('Ctrl Pts',(-5.82363341460557,-1.23762757886435,
1.6484311332934));
#51281=CARTESIAN_POINT('Ctrl Pts',(-5.78658463297976,-1.73818213057826,
1.10804788078631));
#51282=CARTESIAN_POINT('Ctrl Pts',(-5.74953585135395,-1.89716559122094,
0.481054251999797));
#51283=CARTESIAN_POINT('Ctrl Pts',(-5.74031379827737,-1.93673919790939,
0.32498519197648));
#51284=CARTESIAN_POINT('Ctrl Pts',(-5.73109174520078,-1.95514925643464,
0.163549802899745));
#51285=CARTESIAN_POINT('Ctrl Pts',(-5.7218696921242,-1.9536847040016,0.00178561523945243));
#51286=CARTESIAN_POINT('Origin',(-14.8,0.,0.));
#51287=CARTESIAN_POINT('',(-4.9201303078758,-1.95084803715115,-0.000343805551916709));
#51288=CARTESIAN_POINT('',(-5.0218696921242,-1.95090916188199,-0.000496152702984699));
#51289=CARTESIAN_POINT('',(-14.8,-1.954,-2.39295984553393E-16));
#51290=CARTESIAN_POINT('Ctrl Pts',(-4.9201303078758,-1.95084803715115,-0.000343805551916709));
#51291=CARTESIAN_POINT('Ctrl Pts',(-4.9398511484936,-1.95030235658804,0.346849383744408));
#51292=CARTESIAN_POINT('Ctrl Pts',(-4.9595719891114,-1.86202658127011,0.694301680604123));
#51293=CARTESIAN_POINT('Ctrl Pts',(-4.97929282972921,-1.68765867280898,
0.991190605298301));
#51294=CARTESIAN_POINT('Ctrl Pts',(-5.01634161135502,-1.36008041748383,
1.54894436190979));
#51295=CARTESIAN_POINT('Ctrl Pts',(-5.05339039298082,-0.728651292790854,
1.92824134169696));
#51296=CARTESIAN_POINT('Ctrl Pts',(-5.09043917460663,-0.0823886763808118,
1.95546994810536));
#51297=CARTESIAN_POINT('Ctrl Pts',(-5.12748795623243,0.563873940029249,
1.98269855451377));
#51298=CARTESIAN_POINT('Ctrl Pts',(-5.16453673785825,1.2249700481564,1.65785878754338));
#51299=CARTESIAN_POINT('Ctrl Pts',(-5.20158551948405,1.59830311566784,1.12963611945859));
#51300=CARTESIAN_POINT('Ctrl Pts',(-5.23863430110986,1.97163618317925,0.601413451373826));
#51301=CARTESIAN_POINT('Ctrl Pts',(-5.27568308273567,2.05720621007502,-0.130192117825276));
#51302=CARTESIAN_POINT('Ctrl Pts',(-5.31273186436147,1.81584613260757,-0.730310505629698));
#51303=CARTESIAN_POINT('Ctrl Pts',(-5.34978064598728,1.57448605514012,-1.33042889343414));
#51304=CARTESIAN_POINT('Ctrl Pts',(-5.38682942761309,1.00619587330941,-1.79906009984386));
#51305=CARTESIAN_POINT('Ctrl Pts',(-5.4238782092389,0.371093043967381,-1.92170251721176));
#51306=CARTESIAN_POINT('Ctrl Pts',(-5.46092699086471,-0.264009785374633,
-2.04434493457966));
#51307=CARTESIAN_POINT('Ctrl Pts',(-5.49797577249051,-0.965925262227987,
-1.82099856290576));
#51308=CARTESIAN_POINT('Ctrl Pts',(-5.53502455411632,-1.4133730361634,-1.35389337563386));
#51309=CARTESIAN_POINT('Ctrl Pts',(-5.5633931387028,-1.75598781230169,-0.996226741687653));
#51310=CARTESIAN_POINT('Ctrl Pts',(-5.5917617232893,-1.94940557007707,-0.495641819605568));
#51311=CARTESIAN_POINT('Ctrl Pts',(-5.62013030787578,-1.95397084692293,
0.00178599170134505));
#51312=CARTESIAN_POINT('Ctrl Pts',(-5.7218696921242,-1.9536847040016,0.00178561523945243));
#51313=CARTESIAN_POINT('Ctrl Pts',(-5.69404296357498,-1.94926554672048,
-0.486323496866887));
#51314=CARTESIAN_POINT('Ctrl Pts',(-5.66621623502575,-1.76389259084126,
-0.977426245064707));
#51315=CARTESIAN_POINT('Ctrl Pts',(-5.63838950647653,-1.43297660565845,
-1.33312734632344));
#51316=CARTESIAN_POINT('Ctrl Pts',(-5.60134072485072,-0.99239178988181,
-1.80671131079422));
#51317=CARTESIAN_POINT('Ctrl Pts',(-5.56429194322491,-0.293809788757061,
-2.04027523466985));
#51318=CARTESIAN_POINT('Ctrl Pts',(-5.5272431615991,0.343014843889603,-1.92691237235926));
#51319=CARTESIAN_POINT('Ctrl Pts',(-5.4901943799733,0.979839476536231,-1.81354951004867));
#51320=CARTESIAN_POINT('Ctrl Pts',(-5.45314559834749,1.55490674070476,-1.35325986155189));
#51321=CARTESIAN_POINT('Ctrl Pts',(-5.41609681672169,1.8049971772935,-0.756726941401114));
#51322=CARTESIAN_POINT('Ctrl Pts',(-5.37904803509588,2.05508761388226,-0.160194021250283));
#51323=CARTESIAN_POINT('Ctrl Pts',(-5.34199925347006,1.98020122289115,0.572582170554614));
#51324=CARTESIAN_POINT('Ctrl Pts',(-5.30495047184425,1.61461496035463,1.10619573479508));
#51325=CARTESIAN_POINT('Ctrl Pts',(-5.26790169021845,1.24902869781812,1.63980929903553));
#51326=CARTESIAN_POINT('Ctrl Pts',(-5.23085290859264,0.592742563736288,
1.97426023571157));
#51327=CARTESIAN_POINT('Ctrl Pts',(-5.19380412696683,-0.0538485281259382,
1.95646385346074));
#51328=CARTESIAN_POINT('Ctrl Pts',(-5.15675534534103,-0.700439619988128,
1.93866747120991));
#51329=CARTESIAN_POINT('Ctrl Pts',(-5.11970656371521,-1.33733566963071,
1.56862377003217));
#51330=CARTESIAN_POINT('Ctrl Pts',(-5.08265778208941,-1.67301698164315,
1.01570894109161));
#51331=CARTESIAN_POINT('Ctrl Pts',(-5.06239508543434,-1.85660759649205,
0.713309105975045));
#51332=CARTESIAN_POINT('Ctrl Pts',(-5.04213238877927,-1.95009861576432,
0.356208711437961));
#51333=CARTESIAN_POINT('Ctrl Pts',(-5.0218696921242,-1.95090916188199,-0.000496152702984699));
#51334=CARTESIAN_POINT('Origin',(-14.8,0.,0.));
#51335=CARTESIAN_POINT('',(-4.22013030787579,-1.95523249314758,-0.00160897937940108));
#51336=CARTESIAN_POINT('',(-4.32186969212421,-1.95550425013349,-0.00152907383372617));
#51337=CARTESIAN_POINT('',(-14.8,-1.954,-2.39295984553393E-16));
#51338=CARTESIAN_POINT('Ctrl Pts',(-4.22013030787579,-1.95523249314758,
-0.00160897937940108));
#51339=CARTESIAN_POINT('Ctrl Pts',(-4.25089179207208,-1.95045093383183,
0.536882135883852));
#51340=CARTESIAN_POINT('Ctrl Pts',(-4.28165327626837,-1.71897769238846,
1.07898378182717));
#51341=CARTESIAN_POINT('Ctrl Pts',(-4.31241476046466,-1.3232609900624,1.44209256433779));
#51342=CARTESIAN_POINT('Ctrl Pts',(-4.34946354209047,-0.846664295422686,
1.87941665129689));
#51343=CARTESIAN_POINT('Ctrl Pts',(-4.38651232371628,-0.131823927041808,
2.05710228976936));
#51344=CARTESIAN_POINT('Ctrl Pts',(-4.42356110534209,0.494063790696452,
1.89381931098549));
#51345=CARTESIAN_POINT('Ctrl Pts',(-4.46060988696789,1.11995150843469,1.73053633220162));
#51346=CARTESIAN_POINT('Ctrl Pts',(-4.4976586685937,1.6568865755303,1.22628473616144));
#51347=CARTESIAN_POINT('Ctrl Pts',(-4.53470745021951,1.85910338030663,0.611870274871573));
#51348=CARTESIAN_POINT('Ctrl Pts',(-4.57175623184532,2.06132018508296,-0.00254418641831178));
#51349=CARTESIAN_POINT('Ctrl Pts',(-4.60880501347113,1.92881872753997,-0.727121512957918));
#51350=CARTESIAN_POINT('Ctrl Pts',(-4.64585379509694,1.52224749900685,-1.23020858544655));
#51351=CARTESIAN_POINT('Ctrl Pts',(-4.68290257672275,1.11567627047375,-1.73329565793517));
#51352=CARTESIAN_POINT('Ctrl Pts',(-4.71995135834855,0.435035270950569,
-2.01489247637288));
#51353=CARTESIAN_POINT('Ctrl Pts',(-4.75700013997436,-0.20813289072373,
-1.9461067061541));
#51354=CARTESIAN_POINT('Ctrl Pts',(-4.79404892160016,-0.851301052398028,
-1.87732093593532));
#51355=CARTESIAN_POINT('Ctrl Pts',(-4.83109770322597,-1.45699637622342,
-1.45815257706005));
#51356=CARTESIAN_POINT('Ctrl Pts',(-4.86814648485178,-1.74798034515745,
-0.880463130904529));
#51357=CARTESIAN_POINT('Ctrl Pts',(-4.88547442585978,-1.88407532120525,
-0.610274255463677));
#51358=CARTESIAN_POINT('Ctrl Pts',(-4.90280236686779,-1.95132750558711,
-0.305409051963234));
#51359=CARTESIAN_POINT('Ctrl Pts',(-4.9201303078758,-1.95084803715115,-0.000343805551916709));
#51360=CARTESIAN_POINT('Ctrl Pts',(-5.0218696921242,-1.95090916188199,-0.000496152702984699));
#51361=CARTESIAN_POINT('Ctrl Pts',(-5.00508360715346,-1.95158063696922,
-0.295998684319199));
#51362=CARTESIAN_POINT('Ctrl Pts',(-4.98829752218272,-1.88864691667946,
-0.591229769456263));
#51363=CARTESIAN_POINT('Ctrl Pts',(-4.97151143721199,-1.76064068408562,
-0.854865401933136));
#51364=CARTESIAN_POINT('Ctrl Pts',(-4.93446265558618,-1.47811650013332,
-1.43673895931385));
#51365=CARTESIAN_POINT('Ctrl Pts',(-4.89741387396037,-0.878601557846366,
-1.86470011737183));
#51366=CARTESIAN_POINT('Ctrl Pts',(-4.86036509233456,-0.236505493565925,
-1.94286273972016));
#51367=CARTESIAN_POINT('Ctrl Pts',(-4.82331631070875,0.405590570714517,
-2.02102536206849));
#51368=CARTESIAN_POINT('Ctrl Pts',(-4.78626752908294,1.09026775698847,-1.74938944870716));
#51369=CARTESIAN_POINT('Ctrl Pts',(-4.74921874745714,1.50413601532688,-1.25228803446986));
#51370=CARTESIAN_POINT('Ctrl Pts',(-4.71216996583133,1.91800427366528,-0.755186620232563));
#51371=CARTESIAN_POINT('Ctrl Pts',(-4.67512118420552,2.06106360406817,-0.032619705119299));
#51372=CARTESIAN_POINT('Ctrl Pts',(-4.63807240257972,1.8678329716821,0.584679795937079));
#51373=CARTESIAN_POINT('Ctrl Pts',(-4.60102362095391,1.67460233929601,1.20197929699349));
#51374=CARTESIAN_POINT('Ctrl Pts',(-4.5639748393281,1.14508174412095,1.71401138399298));
#51375=CARTESIAN_POINT('Ctrl Pts',(-4.52692605770229,0.521643049988718,
1.88640902305896));
#51376=CARTESIAN_POINT('Ctrl Pts',(-4.48987727607648,-0.101795644143479,
2.05880666212493));
#51377=CARTESIAN_POINT('Ctrl Pts',(-4.45282849445068,-0.819152437232826,
1.89156985325739));
#51378=CARTESIAN_POINT('Ctrl Pts',(-4.41577971282487,-1.302079188418,1.46124613291825));
#51379=CARTESIAN_POINT('Ctrl Pts',(-4.38447637259131,-1.71011474955787,
1.09765604338717));
#51380=CARTESIAN_POINT('Ctrl Pts',(-4.35317303235776,-1.95079219889668,
0.546249885634487));
#51381=CARTESIAN_POINT('Ctrl Pts',(-4.32186969212421,-1.95550425013349,
-0.00152907383372617));
#51382=CARTESIAN_POINT('Origin',(-14.8,0.,0.));
#51383=CARTESIAN_POINT('',(-3.5201303078758,-1.95597299937839,0.001346970720391));
#51384=CARTESIAN_POINT('',(-3.6218696921242,-1.95572226229912,0.0014520242175467));
#51385=CARTESIAN_POINT('',(-14.8,-1.954,-2.39295984553393E-16));
#51386=CARTESIAN_POINT('Ctrl Pts',(-3.5201303078758,-1.95597299937839,0.001346970720391));
#51387=CARTESIAN_POINT('Ctrl Pts',(-3.52488365402476,-1.95662759721798,
0.0844741162826126));
#51388=CARTESIAN_POINT('Ctrl Pts',(-3.52963700017373,-1.95178720852235,
0.167524479998186));
#51389=CARTESIAN_POINT('Ctrl Pts',(-3.5343903463227,-1.94119380112327,0.249834421968559));
#51390=CARTESIAN_POINT('Ctrl Pts',(-3.57143912794851,-1.85862610563013,
0.891378919281443));
#51391=CARTESIAN_POINT('Ctrl Pts',(-3.60848790957432,-1.42656035489239,
1.48794251641861));
#51392=CARTESIAN_POINT('Ctrl Pts',(-3.64553669120012,-0.842761437094918,
1.76646646503613));
#51393=CARTESIAN_POINT('Ctrl Pts',(-3.68258547282593,-0.25896251929748,
2.04499041365363));
#51394=CARTESIAN_POINT('Ctrl Pts',(-3.71963425445174,0.476569565559663,
2.00547471375154));
#51395=CARTESIAN_POINT('Ctrl Pts',(-3.75668303607755,1.02716749245939,1.66600646888654));
#51396=CARTESIAN_POINT('Ctrl Pts',(-3.79373181770335,1.57776541935914,1.32653822402154));
#51397=CARTESIAN_POINT('Ctrl Pts',(-3.83078059932916,1.94342918830146,0.68711743419361));
#51398=CARTESIAN_POINT('Ctrl Pts',(-3.86782938095497,1.95678738820298,0.0404194174418129));
#51399=CARTESIAN_POINT('Ctrl Pts',(-3.90487816258078,1.97014558810449,-0.606278599309984));
#51400=CARTESIAN_POINT('Ctrl Pts',(-3.94192694420659,1.6311982189652,-1.26025384298565));
#51401=CARTESIAN_POINT('Ctrl Pts',(-3.9789757258324,1.0950880766397,-1.62216913925226));
#51402=CARTESIAN_POINT('Ctrl Pts',(-4.0160245074582,0.558977934314219,-1.98408443551887));
#51403=CARTESIAN_POINT('Ctrl Pts',(-4.05307328908401,-0.174294981197453,
-2.05393978437644));
#51404=CARTESIAN_POINT('Ctrl Pts',(-4.09012207070982,-0.769097410584957,
-1.79976103551835));
#51405=CARTESIAN_POINT('Ctrl Pts',(-4.12717085233562,-1.36389983997248,
-1.54558228666025));
#51406=CARTESIAN_POINT('Ctrl Pts',(-4.16421963396143,-1.82023178323582,
-0.967369440086464));
#51407=CARTESIAN_POINT('Ctrl Pts',(-4.20126841558724,-1.92922124441822,
-0.329781749076715));
#51408=CARTESIAN_POINT('Ctrl Pts',(-4.20755571301676,-1.94771710660494,
-0.221581066763726));
#51409=CARTESIAN_POINT('Ctrl Pts',(-4.21384301044628,-1.95620978947708,
-0.11167043750699));
#51410=CARTESIAN_POINT('Ctrl Pts',(-4.22013030787579,-1.95523249314758,
-0.00160897937940108));
#51411=CARTESIAN_POINT('Ctrl Pts',(-4.32186969212421,-1.95550425013349,
-0.00152907383372617));
#51412=CARTESIAN_POINT('Ctrl Pts',(-4.31612425073195,-1.95636910398029,
-0.102068884730967));
#51413=CARTESIAN_POINT('Ctrl Pts',(-4.3103788093397,-1.94928493475609,-0.202486505327942));
#51414=CARTESIAN_POINT('Ctrl Pts',(-4.30463336794745,-1.93382754467879,
-0.301598244891043));
#51415=CARTESIAN_POINT('Ctrl Pts',(-4.26758458632164,-1.83415244047339,
-0.940708270550516));
#51416=CARTESIAN_POINT('Ctrl Pts',(-4.23053580469583,-1.38630552278153,
-1.52551769005868));
#51417=CARTESIAN_POINT('Ctrl Pts',(-4.19348702307002,-0.795275026511071,
-1.78834787054631));
#51418=CARTESIAN_POINT('Ctrl Pts',(-4.15643824144421,-0.204244530240643,
-2.05117805103393));
#51419=CARTESIAN_POINT('Ctrl Pts',(-4.11938945981841,0.529969544608357,
-1.99202899250104));
#51420=CARTESIAN_POINT('Ctrl Pts',(-4.0823406781926,1.07130315181323,-1.63797436817403));
#51421=CARTESIAN_POINT('Ctrl Pts',(-4.04529189656679,1.61263675901812,-1.283919743847));
#51422=CARTESIAN_POINT('Ctrl Pts',(-4.00824311494098,1.96108989857888,-0.634959553725796));
#51423=CARTESIAN_POINT('Ctrl Pts',(-3.97119433331517,1.95716879884085,0.0118645153018863));
#51424=CARTESIAN_POINT('Ctrl Pts',(-3.93414555168936,1.95324769910283,0.65868858432955));
#51425=CARTESIAN_POINT('Ctrl Pts',(-3.89709677006356,1.59695236006608,1.30337653226371));
#51426=CARTESIAN_POINT('Ctrl Pts',(-3.86004798843775,1.05136608044181,1.65084216046714));
#51427=CARTESIAN_POINT('Ctrl Pts',(-3.82299920681194,0.505779800817546,
1.99830778867057));
#51428=CARTESIAN_POINT('Ctrl Pts',(-3.78595042518614,-0.229097419394216,
2.04855109714326));
#51429=CARTESIAN_POINT('Ctrl Pts',(-3.74890164356033,-0.816897999454004,
1.77857474747893));
#51430=CARTESIAN_POINT('Ctrl Pts',(-3.71185286193452,-1.40469857951381,
1.50859839781459));
#51431=CARTESIAN_POINT('Ctrl Pts',(-3.67480408030871,-1.84542251942161,
0.918402390013208));
#51432=CARTESIAN_POINT('Ctrl Pts',(-3.6377552986829,-1.93734190958681,0.278130903058121));
#51433=CARTESIAN_POINT('Ctrl Pts',(-3.63246009649667,-1.95047950101089,
0.186620013125221));
#51434=CARTESIAN_POINT('Ctrl Pts',(-3.62716489431044,-1.95649185444208,
0.0940862015967139));
#51435=CARTESIAN_POINT('Ctrl Pts',(-3.6218696921242,-1.95572226229912,0.00145202421754669));
#51436=CARTESIAN_POINT('Origin',(-14.8,0.,0.));
#51437=CARTESIAN_POINT('',(-2.8201303078758,-1.95107804107358,0.000764698408270981));
#51438=CARTESIAN_POINT('',(-2.92186969212421,-1.95097678997586,0.000619975964519355));
#51439=CARTESIAN_POINT('',(-14.8,-1.954,-2.39295984553393E-16));
#51440=CARTESIAN_POINT('Ctrl Pts',(-2.8201303078758,-1.95107804107358,0.000764698408270981));
#51441=CARTESIAN_POINT('Ctrl Pts',(-2.83592429760325,-1.95205660270951,
0.278742283343092));
#51442=CARTESIAN_POINT('Ctrl Pts',(-2.85171828733071,-1.89661935698062,
0.556347448730421));
#51443=CARTESIAN_POINT('Ctrl Pts',(-2.86751227705816,-1.78284755244559,
0.807530318679176));
#51444=CARTESIAN_POINT('Ctrl Pts',(-2.90456105868397,-1.51596712424919,
1.39674301651317));
#51445=CARTESIAN_POINT('Ctrl Pts',(-2.94160984030977,-0.928097750495292,
1.84056565868186));
#51446=CARTESIAN_POINT('Ctrl Pts',(-2.97865862193558,-0.288318663858768,
1.93585199861038));
#51447=CARTESIAN_POINT('Ctrl Pts',(-3.01570740356139,0.351460422777774,
2.0311383385389));
#51448=CARTESIAN_POINT('Ctrl Pts',(-3.0527561851872,1.04314922229697,1.77788837622724));
#51449=CARTESIAN_POINT('Ctrl Pts',(-3.08980496681301,1.47014833279873,1.29201953991286));
#51450=CARTESIAN_POINT('Ctrl Pts',(-3.12685374843881,1.8971474433005,0.806150703598486));
#51451=CARTESIAN_POINT('Ctrl Pts',(-3.16390253006462,2.05945686478485,0.0876629932813832));
#51452=CARTESIAN_POINT('Ctrl Pts',(-3.20095131169043,1.88278442191711,-0.534577807599872));
#51453=CARTESIAN_POINT('Ctrl Pts',(-3.23800009331624,1.70611197904937,-1.15681860848111));
#51454=CARTESIAN_POINT('Ctrl Pts',(-3.27504887494204,1.19045767182961,-1.68281249992648));
#51455=CARTESIAN_POINT('Ctrl Pts',(-3.31209765656785,0.571846494599176,
-1.87180185880745));
#51456=CARTESIAN_POINT('Ctrl Pts',(-3.34914643819366,-0.0467646826312976,
-2.06079121768844));
#51457=CARTESIAN_POINT('Ctrl Pts',(-3.38619521981947,-0.768332729872451,
-1.91277604400494));
#51458=CARTESIAN_POINT('Ctrl Pts',(-3.42324400144528,-1.26258193336873,
-1.49550575841888));
#51459=CARTESIAN_POINT('Ctrl Pts',(-3.45553943692212,-1.6934191312612,-1.13177110931077));
#51460=CARTESIAN_POINT('Ctrl Pts',(-3.48783487239896,-1.95152549616082,
-0.563439872430474));
#51461=CARTESIAN_POINT('Ctrl Pts',(-3.5201303078758,-1.95597299937839,0.001346970720391));
#51462=CARTESIAN_POINT('Ctrl Pts',(-3.6218696921242,-1.95572226229912,0.00145202421754669));
#51463=CARTESIAN_POINT('Ctrl Pts',(-3.59011611268463,-1.9511072722783,-0.554044556796195));
#51464=CARTESIAN_POINT('Ctrl Pts',(-3.55836253324505,-1.70261318298284,
-1.11315029877843));
#51465=CARTESIAN_POINT('Ctrl Pts',(-3.52660895380548,-1.28426775910331,
-1.47692477696249));
#51466=CARTESIAN_POINT('Ctrl Pts',(-3.48956017217967,-0.796159378032062,
-1.90136200391921));
#51467=CARTESIAN_POINT('Ctrl Pts',(-3.45251139055387,-0.0768277754669797,
-2.05988949172389));
#51468=CARTESIAN_POINT('Ctrl Pts',(-3.41546260892806,0.54447499906108,-1.87994612935844));
#51469=CARTESIAN_POINT('Ctrl Pts',(-3.37841382730225,1.16577777358918,-1.70000276699299));
#51470=CARTESIAN_POINT('Ctrl Pts',(-3.34136504567644,1.68905172008024,-1.18158855445736));
#51471=CARTESIAN_POINT('Ctrl Pts',(-3.30431626405063,1.87478418717573,-0.561991748494958));
#51472=CARTESIAN_POINT('Ctrl Pts',(-3.26726748242482,2.06051665427121,0.0576050574674037));
#51473=CARTESIAN_POINT('Ctrl Pts',(-3.23021870079902,1.90870764197117,0.778384456856518));
#51474=CARTESIAN_POINT('Ctrl Pts',(-3.19316991917321,1.48884308449759,1.2704317154486));
#51475=CARTESIAN_POINT('Ctrl Pts',(-3.1561211375474,1.06897852702399,1.7624789740407));
#51476=CARTESIAN_POINT('Ctrl Pts',(-3.11907235592159,0.381058424376826,
2.02579409183575));
#51477=CARTESIAN_POINT('Ctrl Pts',(-3.08202357429578,-0.260042827644615,
1.93985262371964));
#51478=CARTESIAN_POINT('Ctrl Pts',(-3.04497479266997,-0.901144079666002,
1.85391115560354));
#51479=CARTESIAN_POINT('Ctrl Pts',(-3.00792601104417,-1.49542648106167,
1.41871310157634));
#51480=CARTESIAN_POINT('Ctrl Pts',(-2.97087722941836,-1.77087543119594,
0.833457066032298));
#51481=CARTESIAN_POINT('Ctrl Pts',(-2.95454138365365,-1.89232859019302,
0.575401283629502));
#51482=CARTESIAN_POINT('Ctrl Pts',(-2.93820553788893,-1.95179494190022,
0.288171601355809));
#51483=CARTESIAN_POINT('Ctrl Pts',(-2.92186969212421,-1.95097678997586,
0.000619975964519356));
#51484=CARTESIAN_POINT('Origin',(-14.8,0.,0.));
#51485=CARTESIAN_POINT('',(-2.12013030787579,-1.95317394526965,-0.00174698022608888));
#51486=CARTESIAN_POINT('',(-2.22186969212422,-1.95345029075282,-0.00177409282837831));
#51487=CARTESIAN_POINT('',(-14.8,-1.954,-2.39295984553393E-16));
#51488=CARTESIAN_POINT('Ctrl Pts',(-2.12013030787579,-1.95317394526965,
-0.00174698022608888));
#51489=CARTESIAN_POINT('Ctrl Pts',(-2.14696494118173,-1.94909320466695,
0.469273060468867));
#51490=CARTESIAN_POINT('Ctrl Pts',(-2.17379957448768,-1.77791707428167,
0.942952854675103));
#51491=CARTESIAN_POINT('Ctrl Pts',(-2.20063420779362,-1.4680756635552,1.29437413531823));
#51492=CARTESIAN_POINT('Ctrl Pts',(-2.23768298941942,-1.04029837165924,
1.77955796983428));
#51493=CARTESIAN_POINT('Ctrl Pts',(-2.27473177104523,-0.348204585851633,
2.03169902986245));
#51494=CARTESIAN_POINT('Ctrl Pts',(-2.31178055267104,0.291420955456007,
1.93538741782563));
#51495=CARTESIAN_POINT('Ctrl Pts',(-2.34882933429685,0.931046496763703,
1.83907580578881));
#51496=CARTESIAN_POINT('Ctrl Pts',(-2.38587811592266,1.51820379357145,1.39431152168696));
#51497=CARTESIAN_POINT('Ctrl Pts',(-2.42292689754847,1.78413952649653,0.804671837994208));
#51498=CARTESIAN_POINT('Ctrl Pts',(-2.45997567917427,2.05007525942159,0.215032154301494));
#51499=CARTESIAN_POINT('Ctrl Pts',(-2.49702446080008,1.99478942846401,-0.519482928982077));
#51500=CARTESIAN_POINT('Ctrl Pts',(-2.53407324242589,1.64358744171328,-1.06267159813429));
#51501=CARTESIAN_POINT('Ctrl Pts',(-2.57112202405169,1.29238545496256,-1.6058602672865));
#51502=CARTESIAN_POINT('Ctrl Pts',(-2.6081708056775,0.645267312418673,-1.95772252230736));
#51503=CARTESIAN_POINT('Ctrl Pts',(-2.64521958730331,-0.00156844481900884,
-1.95720416795535));
#51504=CARTESIAN_POINT('Ctrl Pts',(-2.68226836892912,-0.648404202056746,
-1.95668581360334));
#51505=CARTESIAN_POINT('Ctrl Pts',(-2.71931715055492,-1.29495757398828,
-1.60378684987845));
#51506=CARTESIAN_POINT('Ctrl Pts',(-2.75636593218073,-1.6452885186346,-1.06003599126631));
#51507=CARTESIAN_POINT('Ctrl Pts',(-2.77762072407909,-1.84627249158189,
-0.748087505049368));
#51508=CARTESIAN_POINT('Ctrl Pts',(-2.79887551597744,-1.9497611398795,-0.373324168442596));
#51509=CARTESIAN_POINT('Ctrl Pts',(-2.8201303078758,-1.95107804107358,0.000764698408270981));
#51510=CARTESIAN_POINT('Ctrl Pts',(-2.92186969212421,-1.95097678997586,
0.000619975964519356));
#51511=CARTESIAN_POINT('Ctrl Pts',(-2.90115675626312,-1.94993941924049,
-0.363979351138944));
#51512=CARTESIAN_POINT('Ctrl Pts',(-2.88044382040203,-1.85198375439503,
-0.729096260305443));
#51513=CARTESIAN_POINT('Ctrl Pts',(-2.85973088454094,-1.66057985668843,
-1.03591747424635));
#51514=CARTESIAN_POINT('Ctrl Pts',(-2.82268210291513,-1.31821983317378,
-1.58472196191997));
#51515=CARTESIAN_POINT('Ctrl Pts',(-2.78563332128933,-0.676884287271719,
-1.94701692020621));
#51516=CARTESIAN_POINT('Ctrl Pts',(-2.74858453966352,-0.0301249583795292,
-1.95697290765036));
#51517=CARTESIAN_POINT('Ctrl Pts',(-2.71153575803771,0.616634370512606,
-1.9669288950945));
#51518=CARTESIAN_POINT('Ctrl Pts',(-2.6744869764119,1.26881748239483,-1.6245459116965));
#51519=CARTESIAN_POINT('Ctrl Pts',(-2.6374381947861,1.62790749704489,-1.08653930156781));
#51520=CARTESIAN_POINT('Ctrl Pts',(-2.60038941316029,1.98699751169498,-0.548532691439077));
#51521=CARTESIAN_POINT('Ctrl Pts',(-2.56334063153448,2.05299442911292,0.185097545420415));
#51522=CARTESIAN_POINT('Ctrl Pts',(-2.52629184990867,1.79569017693857,0.778554598418215));
#51523=CARTESIAN_POINT('Ctrl Pts',(-2.48924306828286,1.53838592476424,1.372011651416));
#51524=CARTESIAN_POINT('Ctrl Pts',(-2.45219428665705,0.957780502997632,
1.82529552055212));
#51525=CARTESIAN_POINT('Ctrl Pts',(-2.41514550503124,0.319628295127426,
1.93092936949567));
#51526=CARTESIAN_POINT('Ctrl Pts',(-2.37809672340544,-0.31852391274278,
2.03656321843921));
#51527=CARTESIAN_POINT('Ctrl Pts',(-2.34104794177963,-1.01422290671656,
1.79454704719021));
#51528=CARTESIAN_POINT('Ctrl Pts',(-2.30399916015382,-1.4490337452698,1.31565636510377));
#51529=CARTESIAN_POINT('Ctrl Pts',(-2.27662267081062,-1.77032890709691,
0.961789245069641));
#51530=CARTESIAN_POINT('Ctrl Pts',(-2.24924618146742,-1.94917421396601,
0.478584173078087));
#51531=CARTESIAN_POINT('Ctrl Pts',(-2.22186969212422,-1.95345029075282,
-0.00177409282837831));
#51532=CARTESIAN_POINT('Origin',(-14.8,0.,0.));
#51533=CARTESIAN_POINT('',(-1.42013030787581,-1.95716002788236,0.00026938582704918));
#51534=CARTESIAN_POINT('',(-1.52186969212421,-1.95708308893297,0.00044115932539827));
#51535=CARTESIAN_POINT('',(-14.8,-1.954,-2.39295984553393E-16));
#51536=CARTESIAN_POINT('Ctrl Pts',(-1.42013030787581,-1.95716002788236,
0.00026938582704918));
#51537=CARTESIAN_POINT('Ctrl Pts',(-1.42095680313442,-1.95718785457129,
0.0147001219979106));
#51538=CARTESIAN_POINT('Ctrl Pts',(-1.42178329839304,-1.95704207475312,
0.0291302803216468));
#51539=CARTESIAN_POINT('Ctrl Pts',(-1.42260979365165,-1.95672097128892,
0.0435565347292863));
#51540=CARTESIAN_POINT('Ctrl Pts',(-1.45965857527746,-1.94232706884309,
0.690233141347453));
#51541=CARTESIAN_POINT('Ctrl Pts',(-1.49670735690327,-1.57563723982012,
1.32906520577453));
#51542=CARTESIAN_POINT('Ctrl Pts',(-1.53375613852908,-1.02449553657502,
1.66765011296634));
#51543=CARTESIAN_POINT('Ctrl Pts',(-1.57080492015488,-0.4733538333299,2.00623502015817));
#51544=CARTESIAN_POINT('Ctrl Pts',(-1.60785370178069,0.262239744137332,
2.04457277011474));
#51545=CARTESIAN_POINT('Ctrl Pts',(-1.6449024834065,0.845591298174233,1.76511373086623));
#51546=CARTESIAN_POINT('Ctrl Pts',(-1.68195126503231,1.42894285221115,1.48565469161772));
#51547=CARTESIAN_POINT('Ctrl Pts',(-1.71900004665812,1.86005238281769,0.888398863164098));
#51548=CARTESIAN_POINT('Ctrl Pts',(-1.75604882828392,1.94159185503945,0.246722734698324));
#51549=CARTESIAN_POINT('Ctrl Pts',(-1.79309760990973,2.02313132726121,-0.394953393767413));
#51550=CARTESIAN_POINT('Ctrl Pts',(-1.83014639153554,1.75510074109823,-1.08104982224532));
#51551=CARTESIAN_POINT('Ctrl Pts',(-1.86719517316134,1.26018333797668,-1.49752735559181));
#51552=CARTESIAN_POINT('Ctrl Pts',(-1.90424395478715,0.765265934855106,
-1.91400488893831));
#51553=CARTESIAN_POINT('Ctrl Pts',(-1.94129273641296,0.0434617147749864,
-2.06086352715338));
#51554=CARTESIAN_POINT('Ctrl Pts',(-1.97834151803877,-0.574845736284208,
-1.87088297156715));
#51555=CARTESIAN_POINT('Ctrl Pts',(-2.01539029966458,-1.19315318734342,
-1.68090241598091));
#51556=CARTESIAN_POINT('Ctrl Pts',(-2.05243908129039,-1.70796386938168,
-1.15408266659332));
#51557=CARTESIAN_POINT('Ctrl Pts',(-2.08948786291619,-1.88363881140861,
-0.531559487397536));
#51558=CARTESIAN_POINT('Ctrl Pts',(-2.09970201123606,-1.93207144090963,
-0.359933220464345));
#51559=CARTESIAN_POINT('Ctrl Pts',(-2.10991615955593,-1.95472721001136,
-0.181032774909288));
#51560=CARTESIAN_POINT('Ctrl Pts',(-2.12013030787579,-1.95317394526965,
-0.00174698022608888));
#51561=CARTESIAN_POINT('Ctrl Pts',(-2.22186969212422,-1.95345029075282,
-0.00177409282837831));
#51562=CARTESIAN_POINT('Ctrl Pts',(-2.21219739984161,-1.9549610565777,-0.171487801915292));
#51563=CARTESIAN_POINT('Ctrl Pts',(-2.20252510755901,-1.9346811310198,-0.34084615700999));
#51564=CARTESIAN_POINT('Ctrl Pts',(-2.1928528152764,-1.89119399620921,-0.504019590408433));
#51565=CARTESIAN_POINT('Ctrl Pts',(-2.15580403365059,-1.72462072546273,
-1.12903967091033));
#51566=CARTESIAN_POINT('Ctrl Pts',(-2.11875525202478,-1.21755150083708,
-1.66331463899026));
#51567=CARTESIAN_POINT('Ctrl Pts',(-2.08170647039897,-0.602081771860848,
-1.86229644050529));
#51568=CARTESIAN_POINT('Ctrl Pts',(-2.04465768877316,0.013387957115369,
-2.06127824202032));
#51569=CARTESIAN_POINT('Ctrl Pts',(-2.00760890714736,0.737258190442158,
-1.92496687697051));
#51570=CARTESIAN_POINT('Ctrl Pts',(-1.97056012552155,1.23819948608823,-1.51575474619958));
#51571=CARTESIAN_POINT('Ctrl Pts',(-1.93351134389574,1.73914078173428,-1.10654261542867));
#51572=CARTESIAN_POINT('Ctrl Pts',(-1.89646256226994,2.01715313969961,-0.424429718936621));
#51573=CARTESIAN_POINT('Ctrl Pts',(-1.85941378064413,1.944984851277,0.218367696264819));
#51574=CARTESIAN_POINT('Ctrl Pts',(-1.82236499901832,1.87281656285439,0.861165111466315));
#51575=CARTESIAN_POINT('Ctrl Pts',(-1.78531621739251,1.45046762804381,1.46464704537719));
#51576=CARTESIAN_POINT('Ctrl Pts',(-1.7482674357667,0.871255457195034,1.75258794478866));
#51577=CARTESIAN_POINT('Ctrl Pts',(-1.71121865414089,0.29204328634627,2.04052884420011));
#51578=CARTESIAN_POINT('Ctrl Pts',(-1.67416987251508,-0.444032120540709,
2.01292870911214));
#51579=CARTESIAN_POINT('Ctrl Pts',(-1.63712109088927,-1.00005493501247,
1.68242093857152));
#51580=CARTESIAN_POINT('Ctrl Pts',(-1.60007230926347,-1.55607774948418,
1.35191316803094));
#51581=CARTESIAN_POINT('Ctrl Pts',(-1.56302352763766,-1.93204797154073,
0.718497762037816));
#51582=CARTESIAN_POINT('Ctrl Pts',(-1.52597474601186,-1.95587637322525,
0.0721007232658861));
#51583=CARTESIAN_POINT('Ctrl Pts',(-1.52460639471597,-1.95675644600748,
0.048226841673994));
#51584=CARTESIAN_POINT('Ctrl Pts',(-1.52323804342009,-1.95715616086527,
0.0243352517901117));
#51585=CARTESIAN_POINT('Ctrl Pts',(-1.52186969212421,-1.95708308893297,
0.00044115932539827));
#51586=CARTESIAN_POINT('Origin',(-14.8,0.,0.));
#51587=CARTESIAN_POINT('',(-0.720130307875805,-1.95236950710743,0.00155959742907545));
#51588=CARTESIAN_POINT('',(-0.821869692124218,-1.95215209727744,0.00149476428280041));
#51589=CARTESIAN_POINT('',(-14.8,-1.954,-2.39295984553393E-16));
#51590=CARTESIAN_POINT('Ctrl Pts',(-0.720130307875805,-1.95236950710743,
0.00155959742907545));
#51591=CARTESIAN_POINT('Ctrl Pts',(-0.731997446712908,-1.95397811762504,
0.210098641876465));
#51592=CARTESIAN_POINT('Ctrl Pts',(-0.74386458555001,-1.9232378714622,0.418181660990822));
#51593=CARTESIAN_POINT('Ctrl Pts',(-0.755731724387113,-1.85816191132805,
0.61489403534867));
#51594=CARTESIAN_POINT('Ctrl Pts',(-0.79278050601292,-1.65499709888296,
1.22902300954524));
#51595=CARTESIAN_POINT('Ctrl Pts',(-0.829829287638726,-1.11717375820457,
1.73232617588306));
#51596=CARTESIAN_POINT('Ctrl Pts',(-0.866878069264533,-0.491005984724849,
1.89458512275237));
#51597=CARTESIAN_POINT('Ctrl Pts',(-0.90392685089034,0.135161788754873,
2.05684406962167));
#51598=CARTESIAN_POINT('Ctrl Pts',(-0.940975632516148,0.849673995035926,
1.87805879702246));
#51599=CARTESIAN_POINT('Ctrl Pts',(-0.978024414141956,1.32555909087577,
1.43998228306123));
#51600=CARTESIAN_POINT('Ctrl Pts',(-1.01507319576777,1.80144418671564,1.00190576909997));
#51601=CARTESIAN_POINT('Ctrl Pts',(-1.05212197739358,2.03870217211428,0.304538013776658));
#51602=CARTESIAN_POINT('Ctrl Pts',(-1.08917075901938,1.92869625712718,-0.332879891399014));
#51603=CARTESIAN_POINT('Ctrl Pts',(-1.12621954064519,1.81869034214009,-0.97029779657465));
#51604=CARTESIAN_POINT('Ctrl Pts',(-1.163268322271,1.36142052676731,-1.54776585160265));
#51605=CARTESIAN_POINT('Ctrl Pts',(-1.2003171038968,0.766208696269818,-1.8009879562628));
#51606=CARTESIAN_POINT('Ctrl Pts',(-1.23736588552261,0.170996865772328,
-2.05421006092295));
#51607=CARTESIAN_POINT('Ctrl Pts',(-1.27441466714842,-0.562156979849869,
-1.98318621521523));
#51608=CARTESIAN_POINT('Ctrl Pts',(-1.31146344877423,-1.09768491472663,
-1.62041371795675));
#51609=CARTESIAN_POINT('Ctrl Pts',(-1.34768573514142,-1.62126613288,-1.26573405764948));
#51610=CARTESIAN_POINT('Ctrl Pts',(-1.38390802150861,-1.95594048513913,
-0.632177385793262));
#51611=CARTESIAN_POINT('Ctrl Pts',(-1.42013030787581,-1.95716002788236,
0.00026938582704918));
#51612=CARTESIAN_POINT('Ctrl Pts',(-1.52186969212421,-1.95708308893297,
0.00044115932539827));
#51613=CARTESIAN_POINT('Ctrl Pts',(-1.48618926179428,-1.95517770250362,
-0.622609006263858));
#51614=CARTESIAN_POINT('Ctrl Pts',(-1.45050883146436,-1.63180984023605,
-1.24736075456756));
#51615=CARTESIAN_POINT('Ctrl Pts',(-1.41482840113443,-1.12121221885139,
-1.60422384641027));
#51616=CARTESIAN_POINT('Ctrl Pts',(-1.37777961950862,-0.591033081480647,
-1.97477270576364));
#51617=CARTESIAN_POINT('Ctrl Pts',(-1.34073083788282,0.141011774573193,
-2.05649175291963));
#51618=CARTESIAN_POINT('Ctrl Pts',(-1.30368205625701,0.739852474057205,
-1.81197852634512));
#51619=CARTESIAN_POINT('Ctrl Pts',(-1.2666332746312,1.3386931735412,-1.56746529977062));
#51620=CARTESIAN_POINT('Ctrl Pts',(-1.2295844930054,1.80432971645534,-0.996719799465619));
#51621=CARTESIAN_POINT('Ctrl Pts',(-1.19253571137959,1.92362878104123,-0.360979650549547));
#51622=CARTESIAN_POINT('Ctrl Pts',(-1.15548692975378,2.04292784562714,0.274760498366579));
#51623=CARTESIAN_POINT('Ctrl Pts',(-1.11843814812797,1.81588943188477,0.975495295893765));
#51624=CARTESIAN_POINT('Ctrl Pts',(-1.08138936650216,1.34643805442864,1.42047781403675));
#51625=CARTESIAN_POINT('Ctrl Pts',(-1.04434058487635,0.87698667697254,1.8654603321797));
#51626=CARTESIAN_POINT('Ctrl Pts',(-1.00729180325054,0.165122335802693,
2.05469057093846));
#51627=CARTESIAN_POINT('Ctrl Pts',(-0.970243021624738,-0.463329621498074,
1.90156748386759));
#51628=CARTESIAN_POINT('Ctrl Pts',(-0.933194239998929,-1.09178157879888,
1.7484443967967));
#51629=CARTESIAN_POINT('Ctrl Pts',(-0.896145458373119,-1.63682115223063,
1.25296798389613));
#51630=CARTESIAN_POINT('Ctrl Pts',(-0.85909667674731,-1.84895641765906,
0.641902107360681));
#51631=CARTESIAN_POINT('Ctrl Pts',(-0.846687681872946,-1.92000829320952,
0.437233748589477));
#51632=CARTESIAN_POINT('Ctrl Pts',(-0.834278686998582,-1.95371411099365,
0.219598267788578));
#51633=CARTESIAN_POINT('Ctrl Pts',(-0.821869692124218,-1.95215209727744,
0.00149476428280041));
#51634=CARTESIAN_POINT('Origin',(-30.9400562256037,0.,0.));
#51635=CARTESIAN_POINT('',(-0.490056225603759,-1.55420203086265,0.00124153214009217));
#51636=CARTESIAN_POINT('',(-0.351943774396335,-1.55328744883452,-0.00161118505867947));
#51637=CARTESIAN_POINT('',(-30.9400562256037,-1.5555,7.38654183493349E-13));
#51638=CARTESIAN_POINT('',(-0.199999999999997,1.3381997242603,-0.79799174809645));
#51639=CARTESIAN_POINT('Ctrl Pts',(-0.490056225603758,-1.55420203086265,
0.00124153214009213));
#51640=CARTESIAN_POINT('Ctrl Pts',(-0.464874582815045,-1.55148475084143,
-0.351024583825932));
#51641=CARTESIAN_POINT('Ctrl Pts',(-0.402644158400524,-1.25822046322886,
-1.2256057899134));
#51642=CARTESIAN_POINT('Ctrl Pts',(-0.305958749865941,0.154235008178209,
-1.81221901823593));
#51643=CARTESIAN_POINT('Ctrl Pts',(-0.234454984120064,1.09063722427217,
-1.20829039445635));
#51644=CARTESIAN_POINT('Ctrl Pts',(-0.199999999999997,1.33821259954898,
-0.797996165556926));
#51645=CARTESIAN_POINT('',(-0.199999999999996,-0.319621170202251,-1.52230829911636));
#51646=CARTESIAN_POINT('Origin',(-0.2,0.,0.));
#51647=CARTESIAN_POINT('Ctrl Pts',(-0.351943774396335,-1.55328744883452,
-0.00161118505867953));
#51648=CARTESIAN_POINT('Ctrl Pts',(-0.338344631223361,-1.5543673293507,
-0.192088933053909));
#51649=CARTESIAN_POINT('Ctrl Pts',(-0.287696706424579,-1.4337686830043,
-0.899654195900291));
#51650=CARTESIAN_POINT('Ctrl Pts',(-0.237048781625798,-0.82586340403187,
-1.41601857102626));
#51651=CARTESIAN_POINT('Ctrl Pts',(-0.199999999999991,-0.319621170202164,
-1.52230829911638));
#51652=CARTESIAN_POINT('Origin',(-30.9400562256037,0.,0.));
#51653=CARTESIAN_POINT('',(-1.19005622560375,-1.55801556979069,0.000214447110768814));
#51654=CARTESIAN_POINT('',(-1.05194377439633,-1.55402895973136,0.00118992110716552));
#51655=CARTESIAN_POINT('',(-30.9400562256037,-1.5555,7.38654183493349E-13));
#51656=CARTESIAN_POINT('Ctrl Pts',(-1.19005622560375,-1.55801556979069,
0.000214447110768934));
#51657=CARTESIAN_POINT('Ctrl Pts',(-1.15383393923655,-1.55704474136851,
-0.503250728557323));
#51658=CARTESIAN_POINT('Ctrl Pts',(-1.08056287124355,-1.01812443290281,
-1.52345605568379));
#51659=CARTESIAN_POINT('Ctrl Pts',(-0.970243021624738,0.719757641542406,
-1.69181235504817));
#51660=CARTESIAN_POINT('Ctrl Pts',(-0.859096676747318,1.81179939867516,
-0.312715794767707));
#51661=CARTESIAN_POINT('Ctrl Pts',(-0.747950331869893,1.24518507479472,
1.35272260350057));
#51662=CARTESIAN_POINT('Ctrl Pts',(-0.636803986992467,-0.461197325722433,
1.77969367544763));
#51663=CARTESIAN_POINT('Ctrl Pts',(-0.550839284903758,-1.45461374558017,
0.850039657502599));
#51664=CARTESIAN_POINT('Ctrl Pts',(-0.501923364440855,-1.55548258033043,
0.167250991524811));
#51665=CARTESIAN_POINT('Ctrl Pts',(-0.490056225603758,-1.55420203086265,
0.00124153214009213));
#51666=CARTESIAN_POINT('Ctrl Pts',(-1.05194377439633,-1.55402895973136,
0.00118992110716549));
#51667=CARTESIAN_POINT('Ctrl Pts',(-1.02730398764487,-1.55155990544438,
-0.343563383414919));
#51668=CARTESIAN_POINT('Ctrl Pts',(-0.965615419267606,-1.26824253586962,
-1.21037106719846));
#51669=CARTESIAN_POINT('Ctrl Pts',(-0.866878069264529,0.165833894051307,
-1.83098644971143));
#51670=CARTESIAN_POINT('Ctrl Pts',(-0.755731724387107,1.62851911260145,
-0.853729469588644));
#51671=CARTESIAN_POINT('Ctrl Pts',(-0.644585379509683,1.60003419765428,
0.9056105153729));
#51672=CARTESIAN_POINT('Ctrl Pts',(-0.533439034632261,0.107502597833407,
1.83487847835014));
#51673=CARTESIAN_POINT('Ctrl Pts',(-0.435891832927811,-1.28993868652504,
1.17800533567591));
#51674=CARTESIAN_POINT('Ctrl Pts',(-0.375393412849168,-1.55142536036654,
0.326838502321218));
#51675=CARTESIAN_POINT('Ctrl Pts',(-0.351943774396335,-1.55328744883452,
-0.00161118505867953));
#51676=CARTESIAN_POINT('Origin',(-30.9400562256037,0.,0.));
#51677=CARTESIAN_POINT('',(-1.89005622560376,-1.55484241139557,-0.00139069996956104));
#51678=CARTESIAN_POINT('',(-1.75194377439633,-1.55795432181946,0.000351189013561961));
#51679=CARTESIAN_POINT('',(-30.9400562256037,-1.5555,7.38654183493349E-13));
#51680=CARTESIAN_POINT('Ctrl Pts',(-1.89005622560376,-1.55484241139557,
-0.00139069996956129));
#51681=CARTESIAN_POINT('Ctrl Pts',(-1.87984207728388,-1.55607890234021,
-0.144112835911223));
#51682=CARTESIAN_POINT('Ctrl Pts',(-1.8325791473382,-1.47262574984037,-0.803097578304466));
#51683=CARTESIAN_POINT('Ctrl Pts',(-1.74826743576671,-0.540000904300196,
-1.75747790595217));
#51684=CARTESIAN_POINT('Ctrl Pts',(-1.63712109088928,1.1837961238493,-1.40675332292743));
#51685=CARTESIAN_POINT('Ctrl Pts',(-1.52597474601186,1.82390089883899,0.231767139453362));
#51686=CARTESIAN_POINT('Ctrl Pts',(-1.41482840113443,0.794334560776014,
1.65812042680182));
#51687=CARTESIAN_POINT('Ctrl Pts',(-1.30368205625701,-0.962393908646208,
1.56656305209763));
#51688=CARTESIAN_POINT('Ctrl Pts',(-1.22875799774678,-1.55271959931364,
0.538121710656146));
#51689=CARTESIAN_POINT('Ctrl Pts',(-1.19088272086236,-1.55803772148702,
0.0117021697892325));
#51690=CARTESIAN_POINT('Ctrl Pts',(-1.19005622560375,-1.55801556979069,
0.000214447110768934));
#51691=CARTESIAN_POINT('Ctrl Pts',(-1.75194377439633,-1.55795432181946,
0.000351189013562063));
#51692=CARTESIAN_POINT('Ctrl Pts',(-1.71626334406638,-1.55643752110799,
-0.495633730420732));
#51693=CARTESIAN_POINT('Ctrl Pts',(-1.64353413211064,-1.03172538405955,
-1.50938575475204));
#51694=CARTESIAN_POINT('Ctrl Pts',(-1.53375613852907,0.695004907338835,
-1.70214273260888));
#51695=CARTESIAN_POINT('Ctrl Pts',(-1.42260979365165,1.80702789992282,-0.339100830268501));
#51696=CARTESIAN_POINT('Ctrl Pts',(-1.31146344877422,1.26481973322455,1.33437866444013));
#51697=CARTESIAN_POINT('Ctrl Pts',(-1.2003171038968,-0.43523909383229,1.78629417578513));
#51698=CARTESIAN_POINT('Ctrl Pts',(-1.11381054577083,-1.44833041407964,
0.865328290434377));
#51699=CARTESIAN_POINT('Ctrl Pts',(-1.06435276927068,-1.55527241537895,
0.174813257700223));
#51700=CARTESIAN_POINT('Ctrl Pts',(-1.05194377439633,-1.55402895973136,
0.00118992110716549));
#51701=CARTESIAN_POINT('Origin',(-30.9400562256037,0.,0.));
#51702=CARTESIAN_POINT('',(-2.59005622560375,-1.5531739472313,0.00060874532998613));
#51703=CARTESIAN_POINT('',(-2.45194377439633,-1.55506239880552,-0.00141228321026893));
#51704=CARTESIAN_POINT('',(-30.9400562256037,-1.5555,7.38654183493349E-13));
#51705=CARTESIAN_POINT('Ctrl Pts',(-2.59005622560375,-1.5531739472313,0.000608745329986182));
#51706=CARTESIAN_POINT('Ctrl Pts',(-2.56880143370539,-1.5521256157025,-0.297188200620199));
#51707=CARTESIAN_POINT('Ctrl Pts',(-2.51049786018122,-1.32614224219593,
-1.11554156078284));
#51708=CARTESIAN_POINT('Ctrl Pts',(-2.41514550503125,-0.00147337065513613,
-1.83856659218734));
#51709=CARTESIAN_POINT('Ctrl Pts',(-2.30399916015382,1.54396000303022,-0.998256861862604));
#51710=CARTESIAN_POINT('Ctrl Pts',(-2.1928528152764,1.67599241355422,0.755895971373255));
#51711=CARTESIAN_POINT('Ctrl Pts',(-2.08170647039897,0.273756218286524,
1.81807229264321));
#51712=CARTESIAN_POINT('Ctrl Pts',(-1.98077427384143,-1.22719369529558,
1.27125174603469));
#51713=CARTESIAN_POINT('Ctrl Pts',(-1.91689085890969,-1.55159389962086,
0.373569214718623));
#51714=CARTESIAN_POINT('Ctrl Pts',(-1.89005622560376,-1.55484241139557,
-0.00139069996956129));
#51715=CARTESIAN_POINT('Ctrl Pts',(-2.45194377439633,-1.55506239880552,
-0.00141228321026872));
#51716=CARTESIAN_POINT('Ctrl Pts',(-2.44227148211371,-1.55626505808943,
-0.136514470766642));
#51717=CARTESIAN_POINT('Ctrl Pts',(-2.39555040820528,-1.4782829057982,-0.78774610379817));
#51718=CARTESIAN_POINT('Ctrl Pts',(-2.31178055267104,-0.565586069932105,
-1.74941178802327));
#51719=CARTESIAN_POINT('Ctrl Pts',(-2.20063420779361,1.16314496579956,-1.42387597174662));
#51720=CARTESIAN_POINT('Ctrl Pts',(-2.08948786291619,1.82708798956902,0.205131106799974));
#51721=CARTESIAN_POINT('Ctrl Pts',(-1.97834151803877,0.818443514495715,
1.64635344282621));
#51722=CARTESIAN_POINT('Ctrl Pts',(-1.86719517316135,-0.939435649392642,
1.58043940475681));
#51723=CARTESIAN_POINT('Ctrl Pts',(-1.79172925861386,-1.54907896162025,
0.55334352462763));
#51724=CARTESIAN_POINT('Ctrl Pts',(-1.75331212569219,-1.55801249141551,
0.0193723050976691));
#51725=CARTESIAN_POINT('Ctrl Pts',(-1.75194377439633,-1.55795432181946,
0.000351189013562063));
#51726=CARTESIAN_POINT('Origin',(-30.9400562256037,0.,0.));
#51727=CARTESIAN_POINT('',(-3.29005622560375,-1.55707062463311,0.00107226865735175));
#51728=CARTESIAN_POINT('',(-3.15194377439632,-1.5530933453467,0.000493537673696837));
#51729=CARTESIAN_POINT('',(-30.9400562256037,-1.5555,7.38654183493349E-13));
#51730=CARTESIAN_POINT('Ctrl Pts',(-3.29005622560375,-1.55707062463311,
0.00107226865735168));
#51731=CARTESIAN_POINT('Ctrl Pts',(-3.25776079012691,-1.55353014804423,
-0.448531587290127));
#51732=CARTESIAN_POINT('Ctrl Pts',(-3.18841657302425,-1.11235272993948,
-1.41997182206607));
#51733=CARTESIAN_POINT('Ctrl Pts',(-3.08202357429579,0.537183538203758,
-1.75834101421655));
#51734=CARTESIAN_POINT('Ctrl Pts',(-2.97087722941836,1.76865785992407,-0.502173923924951));
#51735=CARTESIAN_POINT('Ctrl Pts',(-2.85973088454094,1.38103405472633,1.21370268825252));
#51736=CARTESIAN_POINT('Ctrl Pts',(-2.74858453966351,-0.27084198568111,
1.81850870111212));
#51737=CARTESIAN_POINT('Ctrl Pts',(-2.65869298668446,-1.4063004296344,0.961273762251427));
#51738=CARTESIAN_POINT('Ctrl Pts',(-2.6058502153312,-1.55395294038616,0.221895405189746));
#51739=CARTESIAN_POINT('Ctrl Pts',(-2.59005622560375,-1.5531739472313,0.000608745329986182));
#51740=CARTESIAN_POINT('Ctrl Pts',(-3.15194377439632,-1.5530933453467,0.000493537673696715));
#51741=CARTESIAN_POINT('Ctrl Pts',(-3.13123083853522,-1.55226753665755,
-0.289749171287345));
#51742=CARTESIAN_POINT('Ctrl Pts',(-3.0734691210483,-1.33481050756564,-1.1002917617943));
#51743=CARTESIAN_POINT('Ctrl Pts',(-2.97865862193558,-0.0282989084957232,
-1.83834934851334));
#51744=CARTESIAN_POINT('Ctrl Pts',(-2.86751227705816,1.52923051402139,-1.02067780704635));
#51745=CARTESIAN_POINT('Ctrl Pts',(-2.75636593218073,1.6868429066166,0.731361855340862));
#51746=CARTESIAN_POINT('Ctrl Pts',(-2.64521958730331,0.300253755811285,
1.81388446297849));
#51747=CARTESIAN_POINT('Ctrl Pts',(-2.54374553470851,-1.21661465163989,
1.28620411926705));
#51748=CARTESIAN_POINT('Ctrl Pts',(-2.47932026373952,-1.55165838783199,
0.380981413113712));
#51749=CARTESIAN_POINT('Ctrl Pts',(-2.45194377439633,-1.55506239880552,
-0.00141228321026872));
#51750=CARTESIAN_POINT('Origin',(-30.9400562256037,0.,0.));
#51751=CARTESIAN_POINT('',(-3.99005622560375,-1.55648113771292,-0.00128084310329906));
#51752=CARTESIAN_POINT('',(-3.85194377439632,-1.5568710230329,0.00115589747807187));
#51753=CARTESIAN_POINT('',(-30.9400562256037,-1.5555,7.38654183493349E-13));
#51754=CARTESIAN_POINT('Ctrl Pts',(-3.99005622560375,-1.55648113771292,
-0.00128084310329882));
#51755=CARTESIAN_POINT('Ctrl Pts',(-3.98376892817423,-1.55725912360882,
-0.0888962976159076));
#51756=CARTESIAN_POINT('Ctrl Pts',(-3.9404328491189,-1.51066019062247,-0.691970511541442));
#51757=CARTESIAN_POINT('Ctrl Pts',(-3.86004798843775,-0.72247792391575,
-1.69066700601096));
#51758=CARTESIAN_POINT('Ctrl Pts',(-3.74890164356033,1.02870839145545,-1.52383999196612));
#51759=CARTESIAN_POINT('Ctrl Pts',(-3.63775529868291,1.83817507420302,0.0379693604454949));
#51760=CARTESIAN_POINT('Ctrl Pts',(-3.52660895380548,0.964904870636465,
1.56502008497577));
#51761=CARTESIAN_POINT('Ctrl Pts',(-3.41546260892806,-0.791676743481206,
1.65939061393862));
#51762=CARTESIAN_POINT('Ctrl Pts',(-3.33661169952748,-1.52370538518956,
0.648661022529862));
#51763=CARTESIAN_POINT('Ctrl Pts',(-3.29480957175271,-1.55759172337387,
0.0672464114013962));
#51764=CARTESIAN_POINT('Ctrl Pts',(-3.29005622560375,-1.55707062463311,
0.00107226865735168));
#51765=CARTESIAN_POINT('Ctrl Pts',(-3.85194377439632,-1.5568710230329,0.0011558974780719));
#51766=CARTESIAN_POINT('Ctrl Pts',(-3.82019019495673,-1.55319721700584,
-0.441052358288231));
#51767=CARTESIAN_POINT('Ctrl Pts',(-3.75138783389134,-1.12457747294624,
-1.40543650404529));
#51768=CARTESIAN_POINT('Ctrl Pts',(-3.64553669120012,0.511471188869394,
-1.7659916129257));
#51769=CARTESIAN_POINT('Ctrl Pts',(-3.5343903463227,1.76114256619831,-0.527926145782834));
#51770=CARTESIAN_POINT('Ctrl Pts',(-3.42324400144528,1.3985956082158,1.19342342803983));
#51771=CARTESIAN_POINT('Ctrl Pts',(-3.31209765656785,-0.244280112870538,
1.82226682475983));
#51772=CARTESIAN_POINT('Ctrl Pts',(-3.22166424755154,-1.39904427633039,
0.976623212198346));
#51773=CARTESIAN_POINT('Ctrl Pts',(-3.16827962016103,-1.55374464284829,
0.229401702103439));
#51774=CARTESIAN_POINT('Ctrl Pts',(-3.15194377439632,-1.5530933453467,0.000493537673696715));
#51775=CARTESIAN_POINT('Origin',(-30.9400562256037,0.,0.));
#51776=CARTESIAN_POINT('',(-4.69005622560375,-1.55299085045476,-0.000273689629153198));
#51777=CARTESIAN_POINT('',(-4.55194377439633,-1.55669747240667,-0.00121723354483211));
#51778=CARTESIAN_POINT('',(-30.9400562256037,-1.5555,7.38654183493349E-13));
#51779=CARTESIAN_POINT('Ctrl Pts',(-4.69005622560374,-1.55299085045476,
-0.000273689629153306));
#51780=CARTESIAN_POINT('Ctrl Pts',(-4.67272828459573,-1.55337253579367,
-0.243123736094311));
#51781=CARTESIAN_POINT('Ctrl Pts',(-4.61835156196192,-1.38536919465911,
-1.00471048981168));
#51782=CARTESIAN_POINT('Ctrl Pts',(-4.52692605770229,-0.195516740427347,
-1.82814181068467));
#51783=CARTESIAN_POINT('Ctrl Pts',(-4.41577971282487,1.42997518601849,-1.15563845692861));
#51784=CARTESIAN_POINT('Ctrl Pts',(-4.30463336794744,1.74641226463907,0.57478124332561));
#51785=CARTESIAN_POINT('Ctrl Pts',(-4.19348702307002,0.464115698312818,
1.77902385996933));
#51786=CARTESIAN_POINT('Ctrl Pts',(-4.08862797562212,-1.14647988477387,
1.37868314453131));
#51787=CARTESIAN_POINT('Ctrl Pts',(-4.02081770980003,-1.55267473263827,
0.42739005238893));
#51788=CARTESIAN_POINT('Ctrl Pts',(-3.99005622560375,-1.55648113771292,
-0.00128084310329882));
#51789=CARTESIAN_POINT('Ctrl Pts',(-4.55194377439633,-1.55669747240667,
-0.00121723354483209));
#51790=CARTESIAN_POINT('Ctrl Pts',(-4.54619833300405,-1.55738594741117,
-0.0812528916058229));
#51791=CARTESIAN_POINT('Ctrl Pts',(-4.50340410998597,-1.51538141740202,
-0.676664269333276));
#51792=CARTESIAN_POINT('Ctrl Pts',(-4.42356110534208,-0.747068761626052,
-1.67994565963717));
#51793=CARTESIAN_POINT('Ctrl Pts',(-4.31241476046467,1.00636520985961,-1.53868717363749));
#51794=CARTESIAN_POINT('Ctrl Pts',(-4.20126841558724,1.83853336531533,0.0111453377239352));
#51795=CARTESIAN_POINT('Ctrl Pts',(-4.09012207070981,0.987636640845155,
1.55077497387288));
#51796=CARTESIAN_POINT('Ctrl Pts',(-3.9789757258324,-0.767381039870437,
1.6707649426488));
#51797=CARTESIAN_POINT('Ctrl Pts',(-3.89958296039456,-1.5192100806146,0.663952155285627));
#51798=CARTESIAN_POINT('Ctrl Pts',(-3.85723897658254,-1.55748366406581,
0.0748982019370303));
#51799=CARTESIAN_POINT('Ctrl Pts',(-3.85194377439632,-1.5568710230329,0.0011558974780719));
#51800=CARTESIAN_POINT('Origin',(-30.9400562256037,0.,0.));
#51801=CARTESIAN_POINT('',(-5.39005622560374,-1.55547679241997,0.00142175542085012));
#51802=CARTESIAN_POINT('',(-5.25194377439632,-1.55303950936921,-0.000394967004932745));
#51803=CARTESIAN_POINT('',(-30.9400562256037,-1.5555,7.38654183493349E-13));
#51804=CARTESIAN_POINT('Ctrl Pts',(-5.39005622560374,-1.55547679241997,
0.00142175542085003));
#51805=CARTESIAN_POINT('Ctrl Pts',(-5.36168764101725,-1.55184256103128,
-0.394560312382684));
#51806=CARTESIAN_POINT('Ctrl Pts',(-5.29627027480494,-1.19678629005817,
-1.31348222412533));
#51807=CARTESIAN_POINT('Ctrl Pts',(-5.19380412696683,0.348598926865315,
-1.80521690218908));
#51808=CARTESIAN_POINT('Ctrl Pts',(-5.08265778208941,1.70577709140633,-0.686042119839725));
#51809=CARTESIAN_POINT('Ctrl Pts',(-4.97151143721198,1.50142062748163,1.06116227558912));
#51810=CARTESIAN_POINT('Ctrl Pts',(-4.86036509233456,-0.0773946174390751,
1.83693749184676));
#51811=CARTESIAN_POINT('Ctrl Pts',(-4.76654668846515,-1.35026498281733,
1.072329293764));
#51812=CARTESIAN_POINT('Ctrl Pts',(-4.70977706622154,-1.55255645633192,
0.276112700314716));
#51813=CARTESIAN_POINT('Ctrl Pts',(-4.69005622560374,-1.55299085045476,
-0.000273689629153306));
#51814=CARTESIAN_POINT('Ctrl Pts',(-5.25194377439632,-1.55303950936921,
-0.000394967004932641));
#51815=CARTESIAN_POINT('Ctrl Pts',(-5.23515768942556,-1.55357404340117,
-0.235632524798968));
#51816=CARTESIAN_POINT('Ctrl Pts',(-5.181322822829,-1.39290097570194,-0.989372871163793));
#51817=CARTESIAN_POINT('Ctrl Pts',(-5.09043917460663,-0.22216951407526,
-1.82509448000564));
#51818=CARTESIAN_POINT('Ctrl Pts',(-4.9792928297292,1.4129615451609,-1.17637954157153));
#51819=CARTESIAN_POINT('Ctrl Pts',(-4.86814648485178,1.75461270448817,0.549238938150095));
#51820=CARTESIAN_POINT('Ctrl Pts',(-4.75700013997435,0.490023217597568,
1.7720627528806));
#51821=CARTESIAN_POINT('Ctrl Pts',(-4.65159923648921,-1.13459408569634,
1.39331703519712));
#51822=CARTESIAN_POINT('Ctrl Pts',(-4.58324711462986,-1.55294639988908,
0.434847337311016));
#51823=CARTESIAN_POINT('Ctrl Pts',(-4.55194377439633,-1.55669747240667,
-0.00121723354483209));
#51824=CARTESIAN_POINT('Origin',(-30.9400562256037,0.,0.));
#51825=CARTESIAN_POINT('',(-6.09005622560374,-1.55777658619528,-0.000591325705981328));
#51826=CARTESIAN_POINT('',(-5.95194377439632,-1.5552490056676,0.00142145573523295));
#51827=CARTESIAN_POINT('',(-30.9400562256037,-1.5555,7.38654183493349E-13));
#51828=CARTESIAN_POINT('Ctrl Pts',(-6.09005622560374,-1.55777658619529,
-0.00059132570598132));
#51829=CARTESIAN_POINT('Ctrl Pts',(-6.08769577906457,-1.55793621982475,
-0.0334132884585462));
#51830=CARTESIAN_POINT('Ctrl Pts',(-6.04828655089958,-1.54211757398053,
-0.581241099247826));
#51831=CARTESIAN_POINT('Ctrl Pts',(-5.9718285411088,-0.896884068407809,
-1.60496985753535));
#51832=CARTESIAN_POINT('Ctrl Pts',(-5.86068219623137,0.862128800674478,
-1.62390369382189));
#51833=CARTESIAN_POINT('Ctrl Pts',(-5.74953585135396,1.83191546708753,-0.156252991031506));
#51834=CARTESIAN_POINT('Ctrl Pts',(-5.63838950647652,1.12469553475403,1.45443777105284));
#51835=CARTESIAN_POINT('Ctrl Pts',(-5.5272431615991,-0.612114390813121,
1.73367968446316));
#51836=CARTESIAN_POINT('Ctrl Pts',(-5.44446540130818,-1.4882965528505,0.759651063044836));
#51837=CARTESIAN_POINT('Ctrl Pts',(-5.39873642264305,-1.55658879166139,
0.122584034846145));
#51838=CARTESIAN_POINT('Ctrl Pts',(-5.39005622560374,-1.55547679241997,
0.00142175542085003));
#51839=CARTESIAN_POINT('Ctrl Pts',(-5.95194377439632,-1.5552490056676,0.0014214557352331));
#51840=CARTESIAN_POINT('Ctrl Pts',(-5.92411704584707,-1.55173109412698,
-0.387142374296427));
#51841=CARTESIAN_POINT('Ctrl Pts',(-5.85924153567202,-1.20768988464287,
-1.2985999419321));
#51842=CARTESIAN_POINT('Ctrl Pts',(-5.75731724387117,0.322222710510533,
-1.81011095758319));
#51843=CARTESIAN_POINT('Ctrl Pts',(-5.64617089899375,1.69558575464707,-0.710857301129708));
#51844=CARTESIAN_POINT('Ctrl Pts',(-5.53502455411632,1.51674371597785,1.03914274956487));
#51845=CARTESIAN_POINT('Ctrl Pts',(-5.4238782092389,-0.0505844542846405,
1.83787115079273));
#51846=CARTESIAN_POINT('Ctrl Pts',(-5.32951794933223,-1.34189057390848,
1.08760790747833));
#51847=CARTESIAN_POINT('Ctrl Pts',(-5.27220647105137,-1.55239426654098,
0.283563280779469));
#51848=CARTESIAN_POINT('Ctrl Pts',(-5.25194377439632,-1.55303950936921,
-0.000394967004932641));
#51849=CARTESIAN_POINT('Origin',(-30.9400562256037,0.,0.));
#51850=CARTESIAN_POINT('',(-6.79005622560374,-1.55372215258713,-0.00105166811141202));
#51851=CARTESIAN_POINT('',(-6.65194377439632,-1.55788369592683,-0.000462245611997092));
#51852=CARTESIAN_POINT('',(-30.9400562256037,-1.5555,7.38654183493349E-13));
#51853=CARTESIAN_POINT('Ctrl Pts',(-6.79005622560374,-1.55372215258713,
-0.00105166811141207));
#51854=CARTESIAN_POINT('Ctrl Pts',(-6.77665513548608,-1.55488854693699,
-0.188645944060803));
#51855=CARTESIAN_POINT('Ctrl Pts',(-6.72620526374262,-1.4365859816325,-0.89344377020468));
#51856=CARTESIAN_POINT('Ctrl Pts',(-6.63870661037334,-0.387375999329962,
-1.79729494265797));
#51857=CARTESIAN_POINT('Ctrl Pts',(-6.5275602654959,1.30001617698454,-1.30011046274511));
#51858=CARTESIAN_POINT('Ctrl Pts',(-6.4164139206185,1.79732303197884,0.387245651336726));
#51859=CARTESIAN_POINT('Ctrl Pts',(-6.30526757574106,0.649290547434899,
1.72010204952278));
#51860=CARTESIAN_POINT('Ctrl Pts',(-6.19648167740282,-1.05612350019664,
1.48344519834433));
#51861=CARTESIAN_POINT('Ctrl Pts',(-6.12474456069037,-1.55543066361753,
0.481749292167505));
#51862=CARTESIAN_POINT('Ctrl Pts',(-6.09005622560374,-1.55777658619529,
-0.00059132570598132));
#51863=CARTESIAN_POINT('Ctrl Pts',(-6.65194377439632,-1.55788369592683,
-0.000462245611997049));
#51864=CARTESIAN_POINT('Ctrl Pts',(-6.6501251838944,-1.55798279177326,-0.0257450798766383));
#51865=CARTESIAN_POINT('Ctrl Pts',(-6.61125781176667,-1.54596760635299,
-0.565999964779691));
#51866=CARTESIAN_POINT('Ctrl Pts',(-6.53534165801313,-0.920205969547918,
-1.59171295387702));
#51867=CARTESIAN_POINT('Ctrl Pts',(-6.42419531313571,0.838343369925463,
-1.63630973474875));
#51868=CARTESIAN_POINT('Ctrl Pts',(-6.31304896825829,1.82944061423442,-0.182965004634956));
#51869=CARTESIAN_POINT('Ctrl Pts',(-6.20190262338086,1.14579683626047,1.43787299993672));
#51870=CARTESIAN_POINT('Ctrl Pts',(-6.09075627850344,-0.586753886249875,
1.74242619094817));
#51871=CARTESIAN_POINT('Ctrl Pts',(-6.00743666217526,-1.48288220531212,
0.774993702200644));
#51872=CARTESIAN_POINT('Ctrl Pts',(-5.96116582747288,-1.55641487634798,
0.130195352308992));
#51873=CARTESIAN_POINT('Ctrl Pts',(-5.95194377439632,-1.5552490056676,0.0014214557352331));
#51874=CARTESIAN_POINT('Origin',(-30.9400562256037,0.,0.));
#51875=CARTESIAN_POINT('',(-7.49005622560373,-1.55396602392417,0.00116714021534956));
#51876=CARTESIAN_POINT('',(-7.35194377439631,-1.5538855757594,-0.00113247137955699));
#51877=CARTESIAN_POINT('',(-30.9400562256037,-1.5555,7.38654183493349E-13));
#51878=CARTESIAN_POINT('Ctrl Pts',(-7.49005622560373,-1.55396602392417,
0.00116714021534962));
#51879=CARTESIAN_POINT('Ctrl Pts',(-7.46561449190759,-1.5515811557621,-0.34084388051028));
#51880=CARTESIAN_POINT('Ctrl Pts',(-7.40412397658564,-1.271828585896,-1.20482146261895));
#51881=CARTESIAN_POINT('Ctrl Pts',(-7.30558467963788,0.156120132828023,
-1.83192679435794));
#51882=CARTESIAN_POINT('Ctrl Pts',(-7.19443833476045,1.62384116454318,-0.862246570359003));
#51883=CARTESIAN_POINT('Ctrl Pts',(-7.08329198988304,1.60503489891277,0.896767667254413));
#51884=CARTESIAN_POINT('Ctrl Pts',(-6.97214564500561,0.116917322223582,
1.83484593781736));
#51885=CARTESIAN_POINT('Ctrl Pts',(-6.87440039024584,-1.28590137517143,
1.1826521502983));
#51886=CARTESIAN_POINT('Ctrl Pts',(-6.81370391711189,-1.55166392198648,
0.329978981439988));
#51887=CARTESIAN_POINT('Ctrl Pts',(-6.79005622560374,-1.55372215258713,
-0.00105166811141207));
#51888=CARTESIAN_POINT('Ctrl Pts',(-7.35194377439631,-1.5538855757594,-0.00113247137955713));
#51889=CARTESIAN_POINT('Ctrl Pts',(-7.3390845403159,-1.55509892412473,-0.181094025918854));
#51890=CARTESIAN_POINT('Ctrl Pts',(-7.28917652460969,-1.44305374746564,
-0.878079590738082));
#51891=CARTESIAN_POINT('Ctrl Pts',(-7.20221972727767,-0.413558273857659,
-1.79145156452956));
#51892=CARTESIAN_POINT('Ctrl Pts',(-7.09107338240025,1.28090844667878,-1.31893999300895));
#51893=CARTESIAN_POINT('Ctrl Pts',(-6.97992703752282,1.80278180465922,0.360980496316825));
#51894=CARTESIAN_POINT('Ctrl Pts',(-6.8687806926454,0.674318650485929,1.71044541320042));
#51895=CARTESIAN_POINT('Ctrl Pts',(-6.7594529382699,-1.04287764167063,1.49764197438319));
#51896=CARTESIAN_POINT('Ctrl Pts',(-6.68717396552021,-1.5559639863464,0.489323158169705));
#51897=CARTESIAN_POINT('Ctrl Pts',(-6.65194377439632,-1.55788369592683,
-0.000462245611997049));
#51898=CARTESIAN_POINT('Origin',(-30.9400562256037,0.,0.));
#51899=CARTESIAN_POINT('',(-8.19005622560374,-1.5579254046757,0.000400362302149405));
#51900=CARTESIAN_POINT('',(-8.05194377439631,-1.55379656827821,0.0010903190078327));
#51901=CARTESIAN_POINT('',(-30.9400562256037,-1.5555,7.38654183493349E-13));
#51902=CARTESIAN_POINT('Ctrl Pts',(-8.19005622560374,-1.5579254046757,0.000400362302149489));
#51903=CARTESIAN_POINT('Ctrl Pts',(-8.15457384832911,-1.55622582261712,
-0.492855805043272));
#51904=CARTESIAN_POINT('Ctrl Pts',(-8.08204268942866,-1.03664772187573,
-1.50422548004318));
#51905=CARTESIAN_POINT('Ctrl Pts',(-7.97246274890243,0.685918408299438,
-1.70582684142229));
#51906=CARTESIAN_POINT('Ctrl Pts',(-7.86131640402499,1.80519161566156,-0.348729847455048));
#51907=CARTESIAN_POINT('Ctrl Pts',(-7.75017005914758,1.27192227624375,1.32760799898003));
#51908=CARTESIAN_POINT('Ctrl Pts',(-7.63902371427015,-0.425714136150784,
1.7886018981434));
#51909=CARTESIAN_POINT('Ctrl Pts',(-7.55231910308887,-1.44601574804416,
0.870928982546018));
#51910=CARTESIAN_POINT('Ctrl Pts',(-7.5026632735334,-1.55519613908698,0.17757644834238));
#51911=CARTESIAN_POINT('Ctrl Pts',(-7.49005622560373,-1.55396602392417,
0.00116714021534962));
#51912=CARTESIAN_POINT('Ctrl Pts',(-8.05194377439631,-1.55379656827821,
0.00109031900783265));
#51913=CARTESIAN_POINT('Ctrl Pts',(-8.02804389673742,-1.55163338209354,
-0.333430270496251));
#51914=CARTESIAN_POINT('Ctrl Pts',(-7.96709523745272,-1.28147121141093,
-1.18969909365111));
#51915=CARTESIAN_POINT('Ctrl Pts',(-7.86909779654222,0.12937469692319,-1.83400963512396));
#51916=CARTESIAN_POINT('Ctrl Pts',(-7.75795145166479,1.61108763178959,-0.885847501902045));
#51917=CARTESIAN_POINT('Ctrl Pts',(-7.64680510678736,1.61794834873923,0.873253854697203));
#51918=CARTESIAN_POINT('Ctrl Pts',(-7.53565876190995,0.143676280899092,
1.83294470190416));
#51919=CARTESIAN_POINT('Ctrl Pts',(-7.43737165111292,-1.27633745275613,
1.19778662186747));
#51920=CARTESIAN_POINT('Ctrl Pts',(-7.37613332194171,-1.55160314215653,
0.33739380107606));
#51921=CARTESIAN_POINT('Ctrl Pts',(-7.35194377439631,-1.5538855757594,-0.00113247137955713));
#51922=CARTESIAN_POINT('Origin',(-30.9400562256037,0.,0.));
#51923=CARTESIAN_POINT('',(-8.89005622560373,-1.55514414867911,-0.00141730865890474));
#51924=CARTESIAN_POINT('',(-8.75194377439631,-1.557829309021,0.000531961773406163));
#51925=CARTESIAN_POINT('',(-30.9400562256037,-1.5555,7.38654183493349E-13));
#51926=CARTESIAN_POINT('Ctrl Pts',(-8.89005622560373,-1.55514414867911,
-0.00141730865890458));
#51927=CARTESIAN_POINT('Ctrl Pts',(-8.88058198637642,-1.55633155915456,
-0.133735397335899));
#51928=CARTESIAN_POINT('Ctrl Pts',(-8.83405896552331,-1.48031737464662,
-0.782136131627296));
#51929=CARTESIAN_POINT('Ctrl Pts',(-8.75048716304438,-0.574907898574367,
-1.74637057462545));
#51930=CARTESIAN_POINT('Ctrl Pts',(-8.63934081816696,1.15553474640397,-1.43005899375302));
#51931=CARTESIAN_POINT('Ctrl Pts',(-8.52819447328953,1.82815598552823,0.195384155801151));
#51932=CARTESIAN_POINT('Ctrl Pts',(-8.41704812841212,0.827212201402232,
1.64196505736636));
#51933=CARTESIAN_POINT('Ctrl Pts',(-8.30590178353469,-0.930993773713778,
1.58542734588091));
#51934=CARTESIAN_POINT('Ctrl Pts',(-8.2302378159319,-1.54772004707537,0.558909923790492));
#51935=CARTESIAN_POINT('Ctrl Pts',(-8.19162262995491,-1.55800043439288,
0.022175639668584));
#51936=CARTESIAN_POINT('Ctrl Pts',(-8.19005622560374,-1.5579254046757,0.000400362302149489));
#51937=CARTESIAN_POINT('Ctrl Pts',(-8.75194377439631,-1.557829309021,0.000531961773406219));
#51938=CARTESIAN_POINT('Ctrl Pts',(-8.71700325315893,-1.55567394565809,
-0.485271528700681));
#51939=CARTESIAN_POINT('Ctrl Pts',(-8.64501395029575,-1.04998245345796,
-1.49006113550599));
#51940=CARTESIAN_POINT('Ctrl Pts',(-8.53597586580675,0.660956434360724,
-1.71565315428517));
#51941=CARTESIAN_POINT('Ctrl Pts',(-8.42482952092933,1.79991126531332,-0.375031453253858));
#51942=CARTESIAN_POINT('Ctrl Pts',(-8.31368317605192,1.29115738736595,1.30890861215818));
#51943=CARTESIAN_POINT('Ctrl Pts',(-8.20253683117448,-0.399572131671196,
1.79462287557114));
#51944=CARTESIAN_POINT('Ctrl Pts',(-8.11529036395596,-1.43961378644524,
0.886293114185729));
#51945=CARTESIAN_POINT('Ctrl Pts',(-8.06509267836323,-1.5549866801194,0.185132227888066));
#51946=CARTESIAN_POINT('Ctrl Pts',(-8.05194377439631,-1.55379656827821,
0.00109031900783265));
#51947=CARTESIAN_POINT('Origin',(-30.9400562256037,0.,0.));
#51948=CARTESIAN_POINT('',(-9.59005622560373,-1.55306820950157,0.00045046149979706));
#51949=CARTESIAN_POINT('',(-9.45194377439631,-1.55537042358935,-0.00142308536877606));
#51950=CARTESIAN_POINT('',(-30.9400562256037,-1.5555,7.38654183493349E-13));
#51951=CARTESIAN_POINT('Ctrl Pts',(-9.59005622560373,-1.55306820950157,
0.000450461499797109));
#51952=CARTESIAN_POINT('Ctrl Pts',(-9.56954134279794,-1.55232237073773,
-0.287028638890437));
#51953=CARTESIAN_POINT('Ctrl Pts',(-9.51197767836633,-1.33793859553732,
-1.09471369792781));
#51954=CARTESIAN_POINT('Ctrl Pts',(-9.41736523230892,-0.0381026721077461,
-1.83817231568183));
#51955=CARTESIAN_POINT('Ctrl Pts',(-9.30621888743151,1.5237653819353,-1.02881890368343));
#51956=CARTESIAN_POINT('Ctrl Pts',(-9.19507254255407,1.6907193985366,0.722355308122558));
#51957=CARTESIAN_POINT('Ctrl Pts',(-9.08392619767666,0.309923183800838,
1.81225740332426));
#51958=CARTESIAN_POINT('Ctrl Pts',(-8.98225409202653,-1.21270388908303,
1.29166012383535));
#51959=CARTESIAN_POINT('Ctrl Pts',(-8.91763076800223,-1.55168821942565,
0.383691264048035));
#51960=CARTESIAN_POINT('Ctrl Pts',(-8.89005622560373,-1.55514414867911,
-0.00141730865890458));
#51961=CARTESIAN_POINT('Ctrl Pts',(-9.45194377439631,-1.55537042358935,
-0.00142308536877613));
#51962=CARTESIAN_POINT('Ctrl Pts',(-9.44301139120625,-1.55650874018037,
-0.126127277143475));
#51963=CARTESIAN_POINT('Ctrl Pts',(-9.39703022639039,-1.48579298819755,
-0.766791032011734));
#51964=CARTESIAN_POINT('Ctrl Pts',(-9.31400027994872,-0.600327192984703,
-1.73779642515878));
#51965=CARTESIAN_POINT('Ctrl Pts',(-9.20285393507129,1.13454637823559,-1.44676662581219));
#51966=CARTESIAN_POINT('Ctrl Pts',(-9.09170759019388,1.83081211133877,0.168689557788168));
#51967=CARTESIAN_POINT('Ctrl Pts',(-8.98056124531644,0.851081300419372,
1.62972076565527));
#51968=CARTESIAN_POINT('Ctrl Pts',(-8.86941490043904,-0.907762402178502,
1.59884226086334));
#51969=CARTESIAN_POINT('Ctrl Pts',(-8.79320907679898,-1.54392384656025,
0.574146475722241));
#51970=CARTESIAN_POINT('Ctrl Pts',(-8.75405203478474,-1.55795936052109,
0.0298446399836376));
#51971=CARTESIAN_POINT('Ctrl Pts',(-8.75194377439631,-1.557829309021,0.000531961773406219));
#51972=CARTESIAN_POINT('Origin',(-30.9400562256037,0.,0.));
#51973=CARTESIAN_POINT('',(-10.2900562256037,-1.55679549104668,0.001183809171597));
#51974=CARTESIAN_POINT('',(-10.1519437743963,-1.55301127595102,0.000330442370898021));
#51975=CARTESIAN_POINT('',(-30.9400562256037,-1.5555,7.38654183493349E-13));
#51976=CARTESIAN_POINT('Ctrl Pts',(-10.2900562256037,-1.55679549104668,
0.00118380917159693));
#51977=CARTESIAN_POINT('Ctrl Pts',(-10.2585006992194,-1.5530840694091,-0.438321856345931));
#51978=CARTESIAN_POINT('Ctrl Pts',(-10.1898963912094,-1.12899939113678,
-1.40010995221672));
#51979=CARTESIAN_POINT('Ctrl Pts',(-10.0842433015735,0.502045652602867,
-1.76869427501289));
#51980=CARTESIAN_POINT('Ctrl Pts',(-9.97309695669603,1.75830205085506,-0.537311058624067));
#51981=CARTESIAN_POINT('Ctrl Pts',(-9.86195061181863,1.40494043187336,1.1859475783728));
#51982=CARTESIAN_POINT('Ctrl Pts',(-9.75080426694118,-0.234558248248651,
1.82354372142247));
#51983=CARTESIAN_POINT('Ctrl Pts',(-9.66017280486957,-1.39635476617201,
0.982232150910424));
#51984=CARTESIAN_POINT('Ctrl Pts',(-9.60659012442374,-1.55366931567284,
0.232143247840176));
#51985=CARTESIAN_POINT('Ctrl Pts',(-9.59005622560373,-1.55306820950157,
0.000450461499797109));
#51986=CARTESIAN_POINT('Ctrl Pts',(-10.1519437743963,-1.55301127595102,
0.000330442370898004));
#51987=CARTESIAN_POINT('Ctrl Pts',(-10.1319707476278,-1.55247970594514,
-0.279581117167299));
#51988=CARTESIAN_POINT('Ctrl Pts',(-10.0749489392334,-1.34638723470874,
-1.07944192578539));
#51989=CARTESIAN_POINT('Ctrl Pts',(-9.98087834921326,-0.0649185555153559,
-1.83742067450035));
#51990=CARTESIAN_POINT('Ctrl Pts',(-9.86973200433583,1.50859212232134,-1.05094194054737));
#51991=CARTESIAN_POINT('Ctrl Pts',(-9.75858565945843,1.70107895413302,0.697609880762318));
#51992=CARTESIAN_POINT('Ctrl Pts',(-9.64743931458098,0.33633201488792,1.80754251117172));
#51993=CARTESIAN_POINT('Ctrl Pts',(-9.54522535289363,-1.20188312644262,
1.30656081858063));
#51994=CARTESIAN_POINT('Ctrl Pts',(-9.48006017283206,-1.55178735262855,
0.391107403745289));
#51995=CARTESIAN_POINT('Ctrl Pts',(-9.45194377439631,-1.55537042358935,
-0.00142308536877613));
#51996=CARTESIAN_POINT('Origin',(-30.9400562256037,0.,0.));
#51997=CARTESIAN_POINT('',(-10.9900562256037,-1.55677461884647,-0.00119118501635344));
#51998=CARTESIAN_POINT('',(-10.8519437743963,-1.55658271042523,0.00125264783408005));
#51999=CARTESIAN_POINT('',(-30.9400562256037,-1.5555,7.38654183493349E-13));
#52000=CARTESIAN_POINT('Ctrl Pts',(-10.9900562256037,-1.55677461884647,
-0.00119118501635364));
#52001=CARTESIAN_POINT('Ctrl Pts',(-10.9845088372668,-1.55742983376792,
-0.0784579566522596));
#52002=CARTESIAN_POINT('Ctrl Pts',(-10.941912667304,-1.51707611203411,-0.671071724150687));
#52003=CARTESIAN_POINT('Ctrl Pts',(-10.8622677157155,-0.756017527849028,
-1.67593758038474));
#52004=CARTESIAN_POINT('Ctrl Pts',(-10.751121370838,0.998144889762121,-1.54403240082667));
#52005=CARTESIAN_POINT('Ctrl Pts',(-10.6399750259606,1.83856669176645,0.00134003275348477));
#52006=CARTESIAN_POINT('Ctrl Pts',(-10.5288286810832,0.99589310551582,1.54548574828332));
#52007=CARTESIAN_POINT('Ctrl Pts',(-10.4176823362057,-0.758459725548137,
1.67483375905857));
#52008=CARTESIAN_POINT('Ctrl Pts',(-10.3380915177126,-1.51753643586647,
0.669543322081447));
#52009=CARTESIAN_POINT('Ctrl Pts',(-10.2955494808453,-1.55744158346535,
0.0776939193622526));
#52010=CARTESIAN_POINT('Ctrl Pts',(-10.2900562256037,-1.55679549104668,
0.00118380917159693));
#52011=CARTESIAN_POINT('Ctrl Pts',(-10.8519437743963,-1.55658271042523,
0.00125264783408));
#52012=CARTESIAN_POINT('Ctrl Pts',(-10.8209301040493,-1.55279711529182,
-0.430859426859307));
#52013=CARTESIAN_POINT('Ctrl Pts',(-10.7528676520765,-1.14097100020651,
-1.38550035281079));
#52014=CARTESIAN_POINT('Ctrl Pts',(-10.6477564184778,0.476185984549256,
-1.77583109051801));
#52015=CARTESIAN_POINT('Ctrl Pts',(-10.5366100736004,1.7502751895651,-0.562908442576898));
#52016=CARTESIAN_POINT('Ctrl Pts',(-10.4254637287229,1.4220944780604,1.16532246584438));
#52017=CARTESIAN_POINT('Ctrl Pts',(-10.3143173838456,-0.207926774994991,
1.82677190972811));
#52018=CARTESIAN_POINT('Ctrl Pts',(-10.2231440657366,-1.38889345108409,
0.99757311028931));
#52019=CARTESIAN_POINT('Ctrl Pts',(-10.1690195292536,-1.55346573682043,
0.239638246229552));
#52020=CARTESIAN_POINT('Ctrl Pts',(-10.1519437743963,-1.55301127595102,
0.000330442370898004));
#52021=CARTESIAN_POINT('Origin',(-30.9400562256037,0.,0.));
#52022=CARTESIAN_POINT('',(-11.6900562256037,-1.5530617356523,-0.000438607636642084));
#52023=CARTESIAN_POINT('',(-11.5519437743963,-1.55697909484695,-0.00111249417114406));
#52024=CARTESIAN_POINT('',(-30.9400562256037,-1.5555,7.38654183493349E-13));
#52025=CARTESIAN_POINT('Ctrl Pts',(-11.6900562256037,-1.5530617356523,-0.000438607636642063));
#52026=CARTESIAN_POINT('Ctrl Pts',(-11.6734681936883,-1.55364880148782,
-0.232892390880623));
#52027=CARTESIAN_POINT('Ctrl Pts',(-11.619831380147,-1.39561614963909,-0.983765069282232));
#52028=CARTESIAN_POINT('Ctrl Pts',(-11.52914578498,-0.231899833827511,-1.82388369772625));
#52029=CARTESIAN_POINT('Ctrl Pts',(-11.4179994401025,1.40666768559556,-1.18389834785848));
#52030=CARTESIAN_POINT('Ctrl Pts',(-11.3068530952251,1.75751694870754,0.539873550719585));
#52031=CARTESIAN_POINT('Ctrl Pts',(-11.1957067503477,0.499466907597081,
1.7694242238582));
#52032=CARTESIAN_POINT('Ctrl Pts',(-11.0901077938073,-1.13020370428311,
1.39865279944782));
#52033=CARTESIAN_POINT('Ctrl Pts',(-11.0215576188926,-1.55305391611653,
0.437575819133659));
#52034=CARTESIAN_POINT('Ctrl Pts',(-10.9900562256037,-1.55677461884647,
-0.00119118501635364));
#52035=CARTESIAN_POINT('Ctrl Pts',(-11.5519437743963,-1.55697909484695,
-0.00111249417114408));
#52036=CARTESIAN_POINT('Ctrl Pts',(-11.5469382420966,-1.55754273633745,
-0.0708081666518759));
#52037=CARTESIAN_POINT('Ctrl Pts',(-11.5048839281711,-1.52162841675364,
-0.655776625116939));
#52038=CARTESIAN_POINT('Ctrl Pts',(-11.4257808326198,-0.780389884361033,
-1.66472844101327));
#52039=CARTESIAN_POINT('Ctrl Pts',(-11.3146344877423,0.975510343836714,
-1.55843149448383));
#52040=CARTESIAN_POINT('Ctrl Pts',(-11.2034881428649,1.83839049924661,-0.0254858041131052));
#52041=CARTESIAN_POINT('Ctrl Pts',(-11.0923417979875,1.01833655988029,1.53079058160895));
#52042=CARTESIAN_POINT('Ctrl Pts',(-10.9811954531101,-0.733942234478493,
1.68572178913967));
#52043=CARTESIAN_POINT('Ctrl Pts',(-10.9010627785797,-1.51287298574345,
0.684845816257308));
#52044=CARTESIAN_POINT('Ctrl Pts',(-10.8579788856751,-1.5573193690545,0.0853395819666858));
#52045=CARTESIAN_POINT('Ctrl Pts',(-10.8519437743963,-1.55658271042523,
0.00125264783408));
#52046=CARTESIAN_POINT('Origin',(-30.9400562256037,0.,0.));
#52047=CARTESIAN_POINT('',(-12.3900562256037,-1.55516658951858,0.00141841178062525));
#52048=CARTESIAN_POINT('',(-12.2519437743963,-1.55313429879201,-0.000555641002405599));
#52049=CARTESIAN_POINT('',(-30.9400562256037,-1.5555,7.38654183493349E-13));
#52050=CARTESIAN_POINT('Ctrl Pts',(-12.3900562256037,-1.55516658951858,
0.00141841178062522));
#52051=CARTESIAN_POINT('Ctrl Pts',(-12.3624275501098,-1.55169695808864,
-0.3844320052266));
#52052=CARTESIAN_POINT('Ctrl Pts',(-12.29775009299,-1.21163085071126,-1.29315050173403));
#52053=CARTESIAN_POINT('Ctrl Pts',(-12.1960238542445,0.312564567770197,
-1.81180370535426));
#52054=CARTESIAN_POINT('Ctrl Pts',(-12.0848775093671,1.69177057386242,-0.719889992411354));
#52055=CARTESIAN_POINT('Ctrl Pts',(-11.9737311644897,1.52226406188029,1.0310389913425));
#52056=CARTESIAN_POINT('Ctrl Pts',(-11.8625848196122,-0.0407821208305537,
1.83811482078279));
#52057=CARTESIAN_POINT('Ctrl Pts',(-11.7680265066503,-1.33878984124311,
1.09318869047629));
#52058=CARTESIAN_POINT('Ctrl Pts',(-11.7105169753141,-1.55233761074191,
0.286284898950973));
#52059=CARTESIAN_POINT('Ctrl Pts',(-11.6900562256037,-1.5530617356523,-0.000438607636642063));
#52060=CARTESIAN_POINT('Ctrl Pts',(-12.2519437743963,-1.553134298792,-0.000555641002405547));
#52061=CARTESIAN_POINT('Ctrl Pts',(-12.2358975985181,-1.55385563286349,
-0.225389960215645));
#52062=CARTESIAN_POINT('Ctrl Pts',(-12.1828026410141,-1.40294188872054,
-0.968418244866292));
#52063=CARTESIAN_POINT('Ctrl Pts',(-12.0926589018843,-0.258486605724834,
-1.82030597114671));
#52064=CARTESIAN_POINT('Ctrl Pts',(-11.9815125570069,1.38924419891378,-1.20429635460542));
#52065=CARTESIAN_POINT('Ctrl Pts',(-11.8703662121295,1.76520688394983,0.514172938599101));
#52066=CARTESIAN_POINT('Ctrl Pts',(-11.759219867252,0.525230599245605,1.76194834531198));
#52067=CARTESIAN_POINT('Ctrl Pts',(-11.6530790546743,-1.11806540396333,
1.41321386829771));
#52068=CARTESIAN_POINT('Ctrl Pts',(-11.5839870237224,-1.55337090620096,
0.445049008049826));
#52069=CARTESIAN_POINT('Ctrl Pts',(-11.5519437743963,-1.55697909484695,
-0.00111249417114408));
#52070=CARTESIAN_POINT('Origin',(-30.9400562256037,0.,0.));
#52071=CARTESIAN_POINT('',(-13.0900562256037,-1.55791691533987,-0.000413732030063911));
#52072=CARTESIAN_POINT('',(-12.9519437743963,-1.55494406527359,0.00140217176205479));
#52073=CARTESIAN_POINT('',(-30.9400562256037,-1.5555,7.38654183493349E-13));
#52074=CARTESIAN_POINT('Ctrl Pts',(-13.0900562256037,-1.55791691533987,
-0.000413732030063846));
#52075=CARTESIAN_POINT('Ctrl Pts',(-13.0884356881571,-1.55799687247773,
-0.0229418655251971));
#52076=CARTESIAN_POINT('Ctrl Pts',(-13.0497663690847,-1.54734598542797,
-0.560431660655591));
#52077=CARTESIAN_POINT('Ctrl Pts',(-12.9740482683865,-0.928681719728038,
-1.58678276370895));
#52078=CARTESIAN_POINT('Ctrl Pts',(-12.8629019235091,0.829604801984373,
-1.64075749222281));
#52079=CARTESIAN_POINT('Ctrl Pts',(-12.7517555786316,1.82843885316793,-0.192719059739105));
#52080=CARTESIAN_POINT('Ctrl Pts',(-12.6406092337542,1.15344893307288,1.43174188824448));
#52081=CARTESIAN_POINT('Ctrl Pts',(-12.5294628888768,-0.577452958307463,
1.74553068053895));
#52082=CARTESIAN_POINT('Ctrl Pts',(-12.4459452194933,-1.48087035346453,
0.780602884632271));
#52083=CARTESIAN_POINT('Ctrl Pts',(-12.3994763317356,-1.55634957407083,
0.132975636810733));
#52084=CARTESIAN_POINT('Ctrl Pts',(-12.3900562256037,-1.55516658951858,
0.00141841178062522));
#52085=CARTESIAN_POINT('Ctrl Pts',(-12.9519437743963,-1.55494406527359,
0.001402171762055));
#52086=CARTESIAN_POINT('Ctrl Pts',(-12.9248569549396,-1.55162083135455,
-0.377018655819353));
#52087=CARTESIAN_POINT('Ctrl Pts',(-12.8607213538571,-1.22229200510013,
-1.27821529541056));
#52088=CARTESIAN_POINT('Ctrl Pts',(-12.7595369711488,0.286096082776584,
-1.81617129846043));
#52089=CARTESIAN_POINT('Ctrl Pts',(-12.6483906262714,1.6810868693329,-0.74449720730706));
#52090=CARTESIAN_POINT('Ctrl Pts',(-12.537244281394,1.53714541606292,1.00871855530086));
#52091=CARTESIAN_POINT('Ctrl Pts',(-12.4260979365166,-0.0139586777784811,
1.83851415802169));
#52092=CARTESIAN_POINT('Ctrl Pts',(-12.3309977675173,-1.33019666661088,
1.10844624262991));
#52093=CARTESIAN_POINT('Ctrl Pts',(-12.2729463801439,-1.55219015513867,
0.293726722647215));
#52094=CARTESIAN_POINT('Ctrl Pts',(-12.2519437743963,-1.553134298792,-0.000555641002405547));
#52095=CARTESIAN_POINT('Origin',(-30.9400562256037,0.,0.));
#52096=CARTESIAN_POINT('',(-13.7900562256037,-1.55394853714682,-0.00115986111943391));
#52097=CARTESIAN_POINT('',(-13.6519437743963,-1.55799009741835,-0.000278060196764462));
#52098=CARTESIAN_POINT('',(-30.9400562256037,-1.5555,7.38654183493349E-13));
#52099=CARTESIAN_POINT('Ctrl Pts',(-13.7900562256037,-1.55394853714682,
-0.00115986111943394));
#52100=CARTESIAN_POINT('Ctrl Pts',(-13.7773950445786,-1.55517532350031,
-0.178331666446028));
#52101=CARTESIAN_POINT('Ctrl Pts',(-13.7276850819277,-1.44538251435531,
-0.872463892850537));
#52102=CARTESIAN_POINT('Ctrl Pts',(-13.640926337651,-0.423106453057855,
-1.78922055799212));
#52103=CARTESIAN_POINT('Ctrl Pts',(-13.5297799927736,1.27385616856038,-1.32575251747129));
#52104=CARTESIAN_POINT('Ctrl Pts',(-13.4186336478962,1.8046813570327,0.351360890452264));
#52105=CARTESIAN_POINT('Ctrl Pts',(-13.3074873030187,0.683431109300355,
1.70682488691761));
#52106=CARTESIAN_POINT('Ctrl Pts',(-13.1979614955879,-1.03798850696033,
1.50281360125476));
#52107=CARTESIAN_POINT('Ctrl Pts',(-13.1254844697829,-1.55616888970194,
0.492097080379339));
#52108=CARTESIAN_POINT('Ctrl Pts',(-13.0900562256037,-1.55791691533987,
-0.000413732030063846));
#52109=CARTESIAN_POINT('Ctrl Pts',(-13.6519437743963,-1.55799009741835,
-0.000278060196764374));
#52110=CARTESIAN_POINT('Ctrl Pts',(-13.6508650929869,-1.55802707523786,
-0.0152716175721371));
#52111=CARTESIAN_POINT('Ctrl Pts',(-13.6127376299518,-1.55103858389315,
-0.545203987085675));
#52112=CARTESIAN_POINT('Ctrl Pts',(-13.5375613852908,-0.951734875856344,
-1.57306385121844));
#52113=CARTESIAN_POINT('Ctrl Pts',(-13.4264150404134,0.805576927784317,
-1.65268719585804));
#52114=CARTESIAN_POINT('Ctrl Pts',(-13.315268695536,1.82543231055633,-0.219376465256566));
#52115=CARTESIAN_POINT('Ctrl Pts',(-13.2041223506585,1.1742160279774,1.41476000564494));
#52116=CARTESIAN_POINT('Ctrl Pts',(-13.0929760057811,-0.55192323148034,
1.75377019603021));
#52117=CARTESIAN_POINT('Ctrl Pts',(-13.0089164803604,-1.47527528717852,
0.795952296887006));
#52118=CARTESIAN_POINT('Ctrl Pts',(-12.9619057365654,-1.55616628077341,
0.140577388490967));
#52119=CARTESIAN_POINT('Ctrl Pts',(-12.9519437743963,-1.55494406527359,
0.001402171762055));
#52120=CARTESIAN_POINT('Origin',(-30.9400562256037,0.,0.));
#52121=CARTESIAN_POINT('',(-14.4900562256037,-1.55373788793014,0.00106011422664349));
#52122=CARTESIAN_POINT('',(-14.3519437743963,-1.55412884799482,-0.00122858297720713));
#52123=CARTESIAN_POINT('',(-30.9400562256037,-1.5555,7.38654183493349E-13));
#52124=CARTESIAN_POINT('Ctrl Pts',(-14.4900562256037,-1.55373788793014,
0.00106011422664335));
#52125=CARTESIAN_POINT('Ctrl Pts',(-14.4663544010001,-1.55165705021594,
-0.330719875177941));
#52126=CARTESIAN_POINT('Ctrl Pts',(-14.4056037947708,-1.28495349846119,
-1.18416527816597));
#52127=CARTESIAN_POINT('Ctrl Pts',(-14.3078044069155,0.119591838376424,
-1.83467355896208));
#52128=CARTESIAN_POINT('Ctrl Pts',(-14.1966580620381,1.60634040478516,-0.894427067857099));
#52129=CARTESIAN_POINT('Ctrl Pts',(-14.0855117171607,1.62258254933333,0.864612714664634));
#52130=CARTESIAN_POINT('Ctrl Pts',(-13.9743653722833,0.153449581803269,
1.83215242313658));
#52131=CARTESIAN_POINT('Ctrl Pts',(-13.875880208431,-1.27279954501849,1.2033118949607));
#52132=CARTESIAN_POINT('Ctrl Pts',(-13.8144438262044,-1.55158553676384,
0.340103344694499));
#52133=CARTESIAN_POINT('Ctrl Pts',(-13.7900562256037,-1.55394853714682,
-0.00115986111943394));
#52134=CARTESIAN_POINT('Ctrl Pts',(-14.3519437743963,-1.55412884799482,
-0.00122858297720718));
#52135=CARTESIAN_POINT('Ctrl Pts',(-14.3398244494084,-1.55538235764995,
-0.170768466806927));
#52136=CARTESIAN_POINT('Ctrl Pts',(-14.2906563427948,-1.45165790061733,
-0.857100278990044));
#52137=CARTESIAN_POINT('Ctrl Pts',(-14.2044394545554,-0.449167113826005,
-1.78285671263529));
#52138=CARTESIAN_POINT('Ctrl Pts',(-14.0932931096779,1.25437709178756,-1.34419762889618));
#52139=CARTESIAN_POINT('Ctrl Pts',(-13.9821467648005,1.80961576800425,0.324992193939892));
#52140=CARTESIAN_POINT('Ctrl Pts',(-13.8710004199231,0.708261856483432,
1.69667153467668));
#52141=CARTESIAN_POINT('Ctrl Pts',(-13.760932756455,-1.02448130719353,1.51691348615434));
#52142=CARTESIAN_POINT('Ctrl Pts',(-13.6879138746128,-1.5567570216814,0.499702524170623));
#52143=CARTESIAN_POINT('Ctrl Pts',(-13.6519437743963,-1.55799009741835,
-0.000278060196764374));
#52144=CARTESIAN_POINT('Origin',(-30.9400562256037,0.,0.));
#52145=CARTESIAN_POINT('',(-15.1900562256037,-1.5577883204632,0.000578693956271592));
#52146=CARTESIAN_POINT('',(-15.0519437743963,-1.55358657070994,0.000972031055979372));
#52147=CARTESIAN_POINT('',(-30.9400562256037,-1.5555,7.38654183493349E-13));
#52148=CARTESIAN_POINT('Ctrl Pts',(-15.1900562256037,-1.5577883204632,0.00057869395627152));
#52149=CARTESIAN_POINT('Ctrl Pts',(-15.1553137574216,-1.55548217457295,
-0.482504970374552));
#52150=CARTESIAN_POINT('Ctrl Pts',(-15.0835225076138,-1.05480877594759,
-1.48486659917243));
#52151=CARTESIAN_POINT('Ctrl Pts',(-14.9746824761801,0.651797236720689,
-1.71915375634761));
#52152=CARTESIAN_POINT('Ctrl Pts',(-14.8635361313027,1.79788560735673,-0.384625296386388));
#52153=CARTESIAN_POINT('Ctrl Pts',(-14.7523897864252,1.29811963509442,1.30200410473359));
#52154=CARTESIAN_POINT('Ctrl Pts',(-14.6412434415478,-0.389995490350614,
1.79672835822976));
#52155=CARTESIAN_POINT('Ctrl Pts',(-14.553798921274,-1.43723851868735,0.891908855350462));
#52156=CARTESIAN_POINT('Ctrl Pts',(-14.5034031826259,-1.55490964799528,
0.187891859608462));
#52157=CARTESIAN_POINT('Ctrl Pts',(-14.4900562256037,-1.55373788793014,
0.00106011422664335));
#52158=CARTESIAN_POINT('Ctrl Pts',(-15.0519437743963,-1.55358657070994,
0.000972031055979285));
#52159=CARTESIAN_POINT('Ctrl Pts',(-15.02878380583,-1.55173352040061,-0.323302252679583));
#52160=CARTESIAN_POINT('Ctrl Pts',(-14.9685750556378,-1.29436586684795,
-1.16900831967119));
#52161=CARTESIAN_POINT('Ctrl Pts',(-14.8713175238199,0.0928102146840508,
-1.83622313948545));
#52162=CARTESIAN_POINT('Ctrl Pts',(-14.7601711789425,1.59311920419314,-0.917769227618005));
#52163=CARTESIAN_POINT('Ctrl Pts',(-14.649024834065,1.63502497258126,0.840846295684967));
#52164=CARTESIAN_POINT('Ctrl Pts',(-14.5378784891876,0.180165351192192,
1.82971844833059));
#52165=CARTESIAN_POINT('Ctrl Pts',(-14.438851469298,-1.2630037891826,1.21840966606724));
#52166=CARTESIAN_POINT('Ctrl Pts',(-14.3768732310343,-1.5515503781028,0.347515029937033));
#52167=CARTESIAN_POINT('Ctrl Pts',(-14.3519437743963,-1.55412884799482,
-0.00122858297720718));
#52168=CARTESIAN_POINT('Origin',(-30.9400562256037,0.,0.));
#52169=CARTESIAN_POINT('',(-15.8900562256037,-1.55545392515721,-0.00142225739221978));
#52170=CARTESIAN_POINT('',(-15.7519437743963,-1.55766118063764,0.0007021623802533));
#52171=CARTESIAN_POINT('',(-30.9400562256037,-1.5555,7.38654183493349E-13));
#52172=CARTESIAN_POINT('Ctrl Pts',(-15.8900562256037,-1.55545392515721,
-0.00142225739221964));
#52173=CARTESIAN_POINT('Ctrl Pts',(-15.881321895469,-1.55657175029418,-0.123344733807148));
#52174=CARTESIAN_POINT('Ctrl Pts',(-15.8355387837084,-1.48776154766086,
-0.761183597128199));
#52175=CARTESIAN_POINT('Ctrl Pts',(-15.7527068903221,-0.609586569357517,
-1.73457011683579));
#52176=CARTESIAN_POINT('Ctrl Pts',(-15.6415605454446,1.12681446224207,-1.45279676604917));
#52177=CARTESIAN_POINT('Ctrl Pts',(-15.5304142005672,1.83168575205326,0.158923193668888));
#52178=CARTESIAN_POINT('Ctrl Pts',(-15.4192678556898,0.859760733185979,
1.6251586868464));
#52179=CARTESIAN_POINT('Ctrl Pts',(-15.3081215108124,-0.899222667358879,
1.60366077156884));
#52180=CARTESIAN_POINT('Ctrl Pts',(-15.231717634117,-1.54250743087965,0.579718025313162));
#52181=CARTESIAN_POINT('Ctrl Pts',(-15.1923625390475,-1.55794140962319,
0.0326472949451707));
#52182=CARTESIAN_POINT('Ctrl Pts',(-15.1900562256037,-1.5577883204632,0.00057869395627152));
#52183=CARTESIAN_POINT('Ctrl Pts',(-15.7519437743963,-1.55766118063764,
0.000702162380253313));
#52184=CARTESIAN_POINT('Ctrl Pts',(-15.7177431622515,-1.55498402201236,
-0.474950124415379));
#52185=CARTESIAN_POINT('Ctrl Pts',(-15.6464937684809,-1.06788313969608,
-1.47060850547255));
#52186=CARTESIAN_POINT('Ctrl Pts',(-15.5381955930844,0.626644448535124,
-1.72848080378452));
#52187=CARTESIAN_POINT('Ctrl Pts',(-15.427049248207,1.79208230060405,-0.410816481890913));
#52188=CARTESIAN_POINT('Ctrl Pts',(-15.3159029033296,1.31697838226697,1.28292521004654));
#52189=CARTESIAN_POINT('Ctrl Pts',(-15.2047565584522,-0.363738719182501,
1.80222731587859));
#52190=CARTESIAN_POINT('Ctrl Pts',(-15.1167701821411,-1.43064249288966,
0.907272496897055));
#52191=CARTESIAN_POINT('Ctrl Pts',(-15.0658325874558,-1.55469782737086,
0.195436237425902));
#52192=CARTESIAN_POINT('Ctrl Pts',(-15.0519437743963,-1.55358657070994,
0.000972031055979285));
#52193=CARTESIAN_POINT('Origin',(-30.9400562256037,0.,0.));
#52194=CARTESIAN_POINT('',(-16.5900562256037,-1.55299491568328,0.00028591225007826));
#52195=CARTESIAN_POINT('',(-16.4519437743963,-1.55568344433103,-0.00141187396391018));
#52196=CARTESIAN_POINT('',(-30.9400562256037,-1.5555,7.38654183493349E-13));
#52197=CARTESIAN_POINT('Ctrl Pts',(-16.5900562256037,-1.55299491568328,
0.000285912250078488));
#52198=CARTESIAN_POINT('Ctrl Pts',(-16.5702812518905,-1.55253980973498,
-0.276857339627901));
#52199=CARTESIAN_POINT('Ctrl Pts',(-16.5134574965514,-1.34943550918954,
-1.07385631818032));
#52200=CARTESIAN_POINT('Ctrl Pts',(-16.4195849595866,-0.0747168460009575,
-1.83704835774251));
#52201=CARTESIAN_POINT('Ctrl Pts',(-16.3084386147092,1.50296588015394,-1.05897253923504));
#52202=CARTESIAN_POINT('Ctrl Pts',(-16.1972922698318,1.70477524097488,0.688527888701595));
#52203=CARTESIAN_POINT('Ctrl Pts',(-16.0861459249543,0.345967106142554,
1.80572313415655));
#52204=CARTESIAN_POINT('Ctrl Pts',(-15.9837339102117,-1.19788362025332,
1.31199725711552));
#52205=CARTESIAN_POINT('Ctrl Pts',(-15.9183706770948,-1.55183022361081,
0.393819047993088));
#52206=CARTESIAN_POINT('Ctrl Pts',(-15.8900562256037,-1.55545392515721,
-0.00142225739221964));
#52207=CARTESIAN_POINT('Ctrl Pts',(-16.4519437743963,-1.55568344433103,
-0.00141187396391032));
#52208=CARTESIAN_POINT('Ctrl Pts',(-16.4437513002988,-1.55673883175469,
-0.115727400980526));
#52209=CARTESIAN_POINT('Ctrl Pts',(-16.3985100445755,-1.4930580543659,-0.745845982010793));
#52210=CARTESIAN_POINT('Ctrl Pts',(-16.3162200072264,-0.634829996541143,
-1.72549124292854));
#52211=CARTESIAN_POINT('Ctrl Pts',(-16.205073662349,1.10549739525827,-1.46908293265175));
#52212=CARTESIAN_POINT('Ctrl Pts',(-16.0939273174715,1.83380951667369,0.132180976273241));
#52213=CARTESIAN_POINT('Ctrl Pts',(-15.9827809725941,0.883381152756941,
1.61244128354657));
#52214=CARTESIAN_POINT('Ctrl Pts',(-15.8716346277167,-0.875728642698206,
1.61661018748783));
#52215=CARTESIAN_POINT('Ctrl Pts',(-15.7946888949841,-1.53855244475298,
0.59496787199439));
#52216=CARTESIAN_POINT('Ctrl Pts',(-15.7547919438773,-1.55788412990709,
0.0403136851530925));
#52217=CARTESIAN_POINT('Ctrl Pts',(-15.7519437743963,-1.55766118063764,
0.000702162380253313));
#52218=CARTESIAN_POINT('Origin',(-30.9400562256037,0.,0.));
#52219=CARTESIAN_POINT('',(-17.2900562256037,-1.55650306831887,0.00127499959212149));
#52220=CARTESIAN_POINT('',(-17.1519437743963,-1.55296225729592,0.000162760582741173));
#52221=CARTESIAN_POINT('',(-30.9400562256037,-1.5555,7.38654183493349E-13));
#52222=CARTESIAN_POINT('Ctrl Pts',(-17.2900562256037,-1.55650306831887,
0.00127499959212141));
#52223=CARTESIAN_POINT('Ctrl Pts',(-17.259240608312,-1.55270042160587,-0.428134586038267));
#52224=CARTESIAN_POINT('Ctrl Pts',(-17.1913762093945,-1.14530073562805,
-1.38014743223044));
#52225=CARTESIAN_POINT('Ctrl Pts',(-17.0864630288511,0.466708474190256,
-1.7783454321025));
#52226=CARTESIAN_POINT('Ctrl Pts',(-16.9753166839737,1.74724826325126,-0.572234901352823));
#52227=CARTESIAN_POINT('Ctrl Pts',(-16.8641703390963,1.42828910175244,1.15772169262565));
#52228=CARTESIAN_POINT('Ctrl Pts',(-16.7530239942189,-0.19818140052057,
1.82785486520361));
#52229=CARTESIAN_POINT('Ctrl Pts',(-16.6616526230547,-1.38612848041481,
1.00317856130571));
#52230=CARTESIAN_POINT('Ctrl Pts',(-16.6073300335163,-1.55339245920696,
0.242375705472255));
#52231=CARTESIAN_POINT('Ctrl Pts',(-16.5900562256037,-1.55299491568328,
0.000285912250078488));
#52232=CARTESIAN_POINT('Ctrl Pts',(-17.1519437743963,-1.55296225729592,
0.000162760582741381));
#52233=CARTESIAN_POINT('Ctrl Pts',(-17.1327106567203,-1.5527105748812,-0.269400586387375));
#52234=CARTESIAN_POINT('Ctrl Pts',(-17.0764287574185,-1.35766705289621,
-1.05856521250988));
#52235=CARTESIAN_POINT('Ctrl Pts',(-16.9830980764909,-0.101512432092709,
-1.83576261538962));
#52236=CARTESIAN_POINT('Ctrl Pts',(-16.8719517316135,1.48735487692949,-1.08078888965679));
#52237=CARTESIAN_POINT('Ctrl Pts',(-16.7608053867361,1.71463973954429,0.663580980368641));
#52238=CARTESIAN_POINT('Ctrl Pts',(-16.6496590418587,0.372276761224383,
1.80048303712748));
#52239=CARTESIAN_POINT('Ctrl Pts',(-16.5467051710787,-1.18681899835157,
1.32684253683931));
#52240=CARTESIAN_POINT('Ctrl Pts',(-16.4808000819246,-1.55196605887505,
0.401241093088767));
#52241=CARTESIAN_POINT('Ctrl Pts',(-16.4519437743963,-1.55568344433103,
-0.00141187396391032));
#52242=CARTESIAN_POINT('Origin',(-30.9400562256037,0.,0.));
#52243=CARTESIAN_POINT('',(-17.9900562256037,-1.55705119782931,-0.00108109148358255));
#52244=CARTESIAN_POINT('',(-17.8519437743963,-1.5562809354664,0.00132828490436523));
#52245=CARTESIAN_POINT('',(-30.9400562256037,-1.5555,7.38654183493349E-13));
#52246=CARTESIAN_POINT('Ctrl Pts',(-17.9900562256037,-1.55705119782931,
-0.00108109148358261));
#52247=CARTESIAN_POINT('Ctrl Pts',(-17.9852487463593,-1.55758140962675,
-0.0680110357998723));
#52248=CARTESIAN_POINT('Ctrl Pts',(-17.9433924854891,-1.52326178500861,
-0.650188269130915));
#52249=CARTESIAN_POINT('Ctrl Pts',(-17.8644874429931,-0.789257021834459,
-1.66054287184818));
#52250=CARTESIAN_POINT('Ctrl Pts',(-17.7533410981157,0.967185162849705,
-1.56361188807332));
#52251=CARTESIAN_POINT('Ctrl Pts',(-17.6421947532383,1.83822846890144,-0.0352898268780593));
#52252=CARTESIAN_POINT('Ctrl Pts',(-17.5310484083608,1.0264860090507,1.52533791304877));
#52253=CARTESIAN_POINT('Ctrl Pts',(-17.4199020634834,-0.724941628214821,
1.68961205945094));
#52254=CARTESIAN_POINT('Ctrl Pts',(-17.3395713358977,-1.51113746563686,
0.690441018192311));
#52255=CARTESIAN_POINT('Ctrl Pts',(-17.2962893899378,-1.55727224070449,
0.0881329225904781));
#52256=CARTESIAN_POINT('Ctrl Pts',(-17.2900562256037,-1.55650306831887,
0.00127499959212141));
#52257=CARTESIAN_POINT('Ctrl Pts',(-17.8519437743963,-1.5562809354664,0.00132828490436524));
#52258=CARTESIAN_POINT('Ctrl Pts',(-17.8216700131418,-1.55245751151989,
-0.420686373116763));
#52259=CARTESIAN_POINT('Ctrl Pts',(-17.7543474702616,-1.15702108826059,
-1.36546780177549));
#52260=CARTESIAN_POINT('Ctrl Pts',(-17.6499761457555,0.440711752671261,
-1.78496563131869));
#52261=CARTESIAN_POINT('Ctrl Pts',(-17.5388298008781,1.73871302083308,-0.59766728630315));
#52262=CARTESIAN_POINT('Ctrl Pts',(-17.4276834560006,1.44502883098667,1.1367589153153));
#52263=CARTESIAN_POINT('Ctrl Pts',(-17.3165371111232,-0.171490898207203,
1.83055183640442));
#52264=CARTESIAN_POINT('Ctrl Pts',(-17.2246238839218,-1.37845942243566,
1.0185088936086));
#52265=CARTESIAN_POINT('Ctrl Pts',(-17.1697594383461,-1.55319539107061,
0.249859667954793));
#52266=CARTESIAN_POINT('Ctrl Pts',(-17.1519437743963,-1.55296225729592,
0.000162760582741381));
#52267=CARTESIAN_POINT('Origin',(-30.9400562256037,0.,0.));
#52268=CARTESIAN_POINT('',(-18.6900562256037,-1.55316513377742,-0.000597426394639434));
#52269=CARTESIAN_POINT('',(-18.5519437743963,-1.55723989670315,-0.000988266840771385));
#52270=CARTESIAN_POINT('',(-30.9400562256037,-1.5555,7.38654183493349E-13));
#52271=CARTESIAN_POINT('Ctrl Pts',(-18.6900562256037,-1.55316513377742,
-0.000597426394639451));
#52272=CARTESIAN_POINT('Ctrl Pts',(-18.6742081027808,-1.55393201275337,
-0.22264568371156));
#52273=CARTESIAN_POINT('Ctrl Pts',(-18.6213111983321,-1.40558222477181,
-0.962807460992807));
#52274=CARTESIAN_POINT('Ctrl Pts',(-18.5313655122577,-0.268190871892204,
-1.8189015729265));
#52275=CARTESIAN_POINT('Ctrl Pts',(-18.4202191673802,1.38280179207861,-1.21168827657323));
#52276=CARTESIAN_POINT('Ctrl Pts',(-18.3090728225028,1.76792396598735,0.504751549030178));
#52277=CARTESIAN_POINT('Ctrl Pts',(-18.1979264776254,0.534619847684823,
1.75912219422707));
#52278=CARTESIAN_POINT('Ctrl Pts',(-18.0915876119923,-1.11358239234271,
1.41852223227391));
#52279=CARTESIAN_POINT('Ctrl Pts',(-18.0222975279851,-1.55349533871507,
0.447783784135027));
#52280=CARTESIAN_POINT('Ctrl Pts',(-17.9900562256037,-1.55705119782931,
-0.00108109148358261));
#52281=CARTESIAN_POINT('Ctrl Pts',(-18.5519437743963,-1.55723989670315,
-0.000988266840771402));
#52282=CARTESIAN_POINT('Ctrl Pts',(-18.5476781511891,-1.55767973414606,
-0.0603556251486268));
#52283=CARTESIAN_POINT('Ctrl Pts',(-18.5063637463562,-1.52764743145507,
-0.634904927561926));
#52284=CARTESIAN_POINT('Ctrl Pts',(-18.4280005598975,-0.813401222257357,
-1.64885038907772));
#52285=CARTESIAN_POINT('Ctrl Pts',(-18.31685421502,0.94426823764005,-1.57755717782769));
#52286=CARTESIAN_POINT('Ctrl Pts',(-18.2057078701426,1.83751786269281,-0.0621068290635167));
#52287=CARTESIAN_POINT('Ctrl Pts',(-18.0945615252652,1.04863223837752,1.51019852422351));
#52288=CARTESIAN_POINT('Ctrl Pts',(-17.9834151803877,-0.700212082183364,
1.70000946876656));
#52289=CARTESIAN_POINT('Ctrl Pts',(-17.9025425967648,-1.5063035789731,0.705754202625275));
#52290=CARTESIAN_POINT('Ctrl Pts',(-17.8587187947676,-1.55713658650058,
0.0957717166626119));
#52291=CARTESIAN_POINT('Ctrl Pts',(-17.8519437743963,-1.5562809354664,0.00132828490436524));
#52292=CARTESIAN_POINT('Origin',(-30.9400562256037,0.,0.));
#52293=CARTESIAN_POINT('',(-19.3900562256037,-1.55486411255501,0.00139338310010585));
#52294=CARTESIAN_POINT('',(-19.2519437743963,-1.55326082343937,-0.000708567253318582));
#52295=CARTESIAN_POINT('',(-30.9400562256037,-1.5555,7.38654183493349E-13));
#52296=CARTESIAN_POINT('Ctrl Pts',(-19.3900562256037,-1.55486411255501,
0.00139338310010598));
#52297=CARTESIAN_POINT('Ctrl Pts',(-19.3631674592023,-1.55159923321925,
-0.374309611256368));
#52298=CARTESIAN_POINT('Ctrl Pts',(-19.2992299111752,-1.22614475638912,
-1.2727471902601));
#52299=CARTESIAN_POINT('Ctrl Pts',(-19.1982435815222,0.276406132535501,
-1.81767129197156));
#52300=CARTESIAN_POINT('Ctrl Pts',(-19.0870972366448,1.67709248831789,-0.75345209627986));
#52301=CARTESIAN_POINT('Ctrl Pts',(-18.9759508917673,1.5425032158592,1.0005064241797));
#52302=CARTESIAN_POINT('Ctrl Pts',(-18.8648045468899,-0.00415343528496038,
1.83856248866775));
#52303=CARTESIAN_POINT('Ctrl Pts',(-18.7695063248354,-1.32701551155171,
1.11401883828569));
#52304=CARTESIAN_POINT('Ctrl Pts',(-18.7112568844066,-1.55213924953272,
0.296445282939095));
#52305=CARTESIAN_POINT('Ctrl Pts',(-18.6900562256037,-1.55316513377742,
-0.000597426394639451));
#52306=CARTESIAN_POINT('Ctrl Pts',(-19.2519437743963,-1.55326082343937,
-0.000708567253318564));
#52307=CARTESIAN_POINT('Ctrl Pts',(-19.2366375076107,-1.55414240975036,
-0.215131833202483));
#52308=CARTESIAN_POINT('Ctrl Pts',(-19.1842824591992,-1.41270450480641,
-0.947453497569264));
#52309=CARTESIAN_POINT('Ctrl Pts',(-19.094878629162,-0.29470108811063,-1.81479487066663));
#52310=CARTESIAN_POINT('Ctrl Pts',(-18.9837322842846,1.36497537602827,-1.23173510819818));
#52311=CARTESIAN_POINT('Ctrl Pts',(-18.8725859394071,1.77510034401367,0.478902832121552));
#52312=CARTESIAN_POINT('Ctrl Pts',(-18.7614395945297,0.560229484500028,
1.75113451186034));
#52313=CARTESIAN_POINT('Ctrl Pts',(-18.6545588728594,-1.10118975965476,
1.43300616103721));
#52314=CARTESIAN_POINT('Ctrl Pts',(-18.5847269328149,-1.55385955580829,
0.45527554686127));
#52315=CARTESIAN_POINT('Ctrl Pts',(-18.5519437743963,-1.55723989670315,
-0.000988266840771402));
#52316=CARTESIAN_POINT('Origin',(-30.9400562256037,0.,0.));
#52317=CARTESIAN_POINT('',(-20.0900562256037,-1.55801011030891,-0.000227597310305756));
#52318=CARTESIAN_POINT('',(-19.9519437743963,-1.55464974635955,0.00136170718391795));
#52319=CARTESIAN_POINT('',(-30.9400562256037,-1.5555,7.38654183493349E-13));
#52320=CARTESIAN_POINT('Ctrl Pts',(-20.0900562256037,-1.55801011030891,
-0.000227597310305798));
#52321=CARTESIAN_POINT('Ctrl Pts',(-20.0891755972497,-1.55803513677739,
-0.0124678168029296));
#52322=CARTESIAN_POINT('Ctrl Pts',(-20.0512461872698,-1.55235978918751,
-0.539640640879765));
#52323=CARTESIAN_POINT('Ctrl Pts',(-19.9762679956642,-0.960110720041205,
-1.56796577801391));
#52324=CARTESIAN_POINT('Ctrl Pts',(-19.8651216507867,0.796751482021758,
-1.65695997285902));
#52325=CARTESIAN_POINT('Ctrl Pts',(-19.7539753059093,1.82423641918512,-0.229108626375055));
#52326=CARTESIAN_POINT('Ctrl Pts',(-19.6428289610319,1.18174445642581,1.40847765884577));
#52327=CARTESIAN_POINT('Ctrl Pts',(-19.5316826161545,-0.542562299135568,
1.75668876791466));
#52328=CARTESIAN_POINT('Ctrl Pts',(-19.4474250376784,-1.4731969311599,0.801563749043876));
#52329=CARTESIAN_POINT('Ctrl Pts',(-19.4002162408281,-1.55609775872762,
0.143354084664209));
#52330=CARTESIAN_POINT('Ctrl Pts',(-19.3900562256037,-1.55486411255501,
0.00139338310010598));
#52331=CARTESIAN_POINT('Ctrl Pts',(-19.9519437743963,-1.55464974635955,
0.00136170718391808));
#52332=CARTESIAN_POINT('Ctrl Pts',(-19.9255968640322,-1.55155636764689,
-0.366898958960946));
#52333=CARTESIAN_POINT('Ctrl Pts',(-19.8622011720423,-1.23656566776766,
-1.25776274828745));
#52334=CARTESIAN_POINT('Ctrl Pts',(-19.7617566984265,0.249855885875982,
-1.82151068902289));
#52335=CARTESIAN_POINT('Ctrl Pts',(-19.6506103535491,1.66592065703884,-0.777841576661194));
#52336=CARTESIAN_POINT('Ctrl Pts',(-19.5394640086717,1.55693692840167,0.977893938477322));
#52337=CARTESIAN_POINT('Ctrl Pts',(-19.4283176637942,0.0226726397870904,
1.83842734567798));
#52338=CARTESIAN_POINT('Ctrl Pts',(-19.3324775857025,-1.31820105276063,
1.12925261793028));
#52339=CARTESIAN_POINT('Ctrl Pts',(-19.2736862892365,-1.55200853222309,
0.303879161895605));
#52340=CARTESIAN_POINT('Ctrl Pts',(-19.2519437743963,-1.55326082343937,
-0.000708567253318564));
#52341=CARTESIAN_POINT('Origin',(-30.9400562256037,0.,0.));
#52342=CARTESIAN_POINT('',(-20.7900562256037,-1.55419761171519,-0.00125134276329026));
#52343=CARTESIAN_POINT('',(-20.6519437743963,-1.55804494088714,-8.79497847153243E-5));
#52344=CARTESIAN_POINT('',(-30.9400562256037,-1.5555,7.38654183493349E-13));
#52345=CARTESIAN_POINT('Ctrl Pts',(-20.7900562256037,-1.55419761171519,
-0.00125134276329025));
#52346=CARTESIAN_POINT('Ctrl Pts',(-20.7781349536712,-1.5554572697494,-0.168002024361493));
#52347=CARTESIAN_POINT('Ctrl Pts',(-20.7291649001128,-1.45391681712917,
-0.85148506976451));
#52348=CARTESIAN_POINT('Ctrl Pts',(-20.6431460649287,-0.458668949759455,
-1.78043592142131));
#52349=CARTESIAN_POINT('Ctrl Pts',(-20.5319997200512,1.24719048811815,-1.35086829932027));
#52350=CARTESIAN_POINT('Ctrl Pts',(-20.4208533751738,1.81132329283767,0.315336652776849));
#52351=CARTESIAN_POINT('Ctrl Pts',(-20.3097070302964,0.717300375240254,
1.69287018032718));
#52352=CARTESIAN_POINT('Ctrl Pts',(-20.199441313773,-1.0194963881048,1.52204881850683));
#52353=CARTESIAN_POINT('Ctrl Pts',(-20.1262243788755,-1.55698225202566,
0.502488596935498));
#52354=CARTESIAN_POINT('Ctrl Pts',(-20.0900562256037,-1.55801011030891,
-0.000227597310305798));
#52355=CARTESIAN_POINT('Ctrl Pts',(-20.6519437743963,-1.55804494088714,
-8.79497847151454E-5));
#52356=CARTESIAN_POINT('Ctrl Pts',(-20.6516050020795,-1.55804879982747,
-0.0047964033161587));
#52357=CARTESIAN_POINT('Ctrl Pts',(-20.6142174481369,-1.55589696007643,
-0.524426616553616));
#52358=CARTESIAN_POINT('Ctrl Pts',(-20.5397811125685,-0.982885979939318,
-1.55379030257311));
#52359=CARTESIAN_POINT('Ctrl Pts',(-20.4286347676911,0.772490702514734,
-1.66840860356802));
#52360=CARTESIAN_POINT('Ctrl Pts',(-20.3174884228136,1.82069938029707,-0.255700841839434));
#52361=CARTESIAN_POINT('Ctrl Pts',(-20.2063420779362,1.20216910098862,1.3910854059186));
#52362=CARTESIAN_POINT('Ctrl Pts',(-20.0951957330588,-0.516873484366524,
1.76441802164065));
#52363=CARTESIAN_POINT('Ctrl Pts',(-20.0103962985455,-1.46741867778411,
0.816918777233318));
#52364=CARTESIAN_POINT('Ctrl Pts',(-19.962645645658,-1.55590624817661,0.150945783091283));
#52365=CARTESIAN_POINT('Ctrl Pts',(-19.9519437743963,-1.55464974635955,
0.00136170718391808));
#52366=CARTESIAN_POINT('Origin',(-30.9400562256037,0.,0.));
#52367=CARTESIAN_POINT('',(-21.4900562256037,-1.55353484309772,0.000937949434483771));
#52368=CARTESIAN_POINT('',(-21.3519437743963,-1.55439271669893,-0.00130685278909096));
#52369=CARTESIAN_POINT('',(-30.9400562256037,-1.5555,7.38654183493349E-13));
#52370=CARTESIAN_POINT('Ctrl Pts',(-21.4900562256037,-1.55353484309772,
0.000937949434483658));
#52371=CARTESIAN_POINT('Ctrl Pts',(-21.4670943100927,-1.55176566897119,
-0.320590158884561));
#52372=CARTESIAN_POINT('Ctrl Pts',(-21.4070836129559,-1.29776443387202,
-1.16346243513487));
#52373=CARTESIAN_POINT('Ctrl Pts',(-21.3100241341932,0.0830160705540191,
-1.83669202856401));
#52374=CARTESIAN_POINT('Ctrl Pts',(-21.1988777893158,1.58820198952549,-0.926252512130515));
#52375=CARTESIAN_POINT('Ctrl Pts',(-21.0877314444384,1.6394860967441,0.832114544004366));
#52376=CARTESIAN_POINT('Ctrl Pts',(-20.976585099561,0.189920927787188,1.82873161424777));
#52377=CARTESIAN_POINT('Ctrl Pts',(-20.8773600266161,-1.25938071046584,
1.22392092946362));
#52378=CARTESIAN_POINT('Ctrl Pts',(-20.815183735297,-1.55154252007364,0.350223683721566));
#52379=CARTESIAN_POINT('Ctrl Pts',(-20.7900562256037,-1.55419761171519,
-0.00125134276329025));
#52380=CARTESIAN_POINT('Ctrl Pts',(-21.3519437743963,-1.55439271669893,
-0.00130685278909071));
#52381=CARTESIAN_POINT('Ctrl Pts',(-21.340564358501,-1.55565952887394,-0.160427787637493));
#52382=CARTESIAN_POINT('Ctrl Pts',(-21.2921361609799,-1.46000236816005,
-0.836123537875991));
#52383=CARTESIAN_POINT('Ctrl Pts',(-21.206659181833,-0.484597651685728,
-1.77355413503851));
#52384=CARTESIAN_POINT('Ctrl Pts',(-21.0955128369556,1.2273477973243,-1.36892166990471));
#52385=CARTESIAN_POINT('Ctrl Pts',(-20.9843664920782,1.81573138332858,0.288874882132692));
#52386=CARTESIAN_POINT('Ctrl Pts',(-20.8732201472008,0.741923909701551,
1.68222414265896));
#52387=CARTESIAN_POINT('Ctrl Pts',(-20.7624125746401,-1.00572644221501,
1.53604696707474));
#52388=CARTESIAN_POINT('Ctrl Pts',(-20.6886537837053,-1.55762677881088,
0.510128984729696));
#52389=CARTESIAN_POINT('Ctrl Pts',(-20.6519437743963,-1.55804494088714,
-8.79497847151454E-5));
#52390=CARTESIAN_POINT('Origin',(-30.9400562256037,0.,0.));
#52391=CARTESIAN_POINT('',(-22.1900562256037,-1.55760963761123,0.000745528629259664));
#52392=CARTESIAN_POINT('',(-22.0519437743963,-1.55340336122338,0.000839947947065753));
#52393=CARTESIAN_POINT('',(-30.9400562256037,-1.5555,7.38654183493349E-13));
#52394=CARTESIAN_POINT('Ctrl Pts',(-22.1900562256037,-1.55760963761123,
0.00074552862925974));
#52395=CARTESIAN_POINT('Ctrl Pts',(-22.1560536665142,-1.55481158005176,
-0.472193740327524));
#52396=CARTESIAN_POINT('Ctrl Pts',(-22.0850023257989,-1.0726145744547,-1.46538056385827));
#52397=CARTESIAN_POINT('Ctrl Pts',(-21.9769022034578,0.617417326649948,
-1.73179823319959));
#52398=CARTESIAN_POINT('Ctrl Pts',(-21.8657558585803,1.78986590745487,-0.420368063834038));
#52399=CARTESIAN_POINT('Ctrl Pts',(-21.7546095137029,1.32380169026185,1.27588336481854));
#52400=CARTESIAN_POINT('Ctrl Pts',(-21.6434631688255,-0.35412203130582,
1.80414158610255));
#52401=CARTESIAN_POINT('Ctrl Pts',(-21.5552787394591,-1.4281958244136,0.912887756867582));
#52402=CARTESIAN_POINT('Ctrl Pts',(-21.5041430917185,-1.55462021069444,
0.198191676453029));
#52403=CARTESIAN_POINT('Ctrl Pts',(-21.4900562256037,-1.55353484309772,
0.000937949434483658));
#52404=CARTESIAN_POINT('Ctrl Pts',(-22.0519437743963,-1.55340336122338,
0.00083994794706577));
#52405=CARTESIAN_POINT('Ctrl Pts',(-22.0295237149225,-1.55186430247459,
-0.313167290949957));
#52406=CARTESIAN_POINT('Ctrl Pts',(-21.970054873823,-1.30694896568139,-1.14827399755797));
#52407=CARTESIAN_POINT('Ctrl Pts',(-21.8735372510976,0.056208890351046,
-1.83770773372074));
#52408=CARTESIAN_POINT('Ctrl Pts',(-21.7623909062202,1.57451836940432,-0.949326634167536));
#52409=CARTESIAN_POINT('Ctrl Pts',(-21.6512445613427,1.65145255424892,0.808104952958591));
#52410=CARTESIAN_POINT('Ctrl Pts',(-21.5400982164653,0.216582902754202,
1.82576586674362));
#52411=CARTESIAN_POINT('Ctrl Pts',(-21.4403312874831,-1.24935076014862,
1.23897870805919));
#52412=CARTESIAN_POINT('Ctrl Pts',(-21.3776131401268,-1.55153507749042,
0.357633668376339));
#52413=CARTESIAN_POINT('Ctrl Pts',(-21.3519437743963,-1.55439271669893,
-0.00130685278909071));
#52414=CARTESIAN_POINT('Origin',(-30.9400562256037,0.,0.));
#52415=CARTESIAN_POINT('',(-22.8900562256037,-1.5557675530206,-0.00140509975720526));
#52416=CARTESIAN_POINT('',(-22.7519437743963,-1.55745576654889,0.000858804331327935));
#52417=CARTESIAN_POINT('',(-30.9400562256037,-1.5555,7.38654183493349E-13));
#52418=CARTESIAN_POINT('Ctrl Pts',(-22.8900562256037,-1.5557675530206,-0.00140509975720522));
#52419=CARTESIAN_POINT('Ctrl Pts',(-22.8820618045615,-1.55679795835249,
-0.112941593296949));
#52420=CARTESIAN_POINT('Ctrl Pts',(-22.8370186018936,-1.49496159300788,
-0.740241469970251));
#52421=CARTESIAN_POINT('Ctrl Pts',(-22.7549266175997,-0.644023257663918,
-1.72208110126926));
#52422=CARTESIAN_POINT('Ctrl Pts',(-22.6437802727223,1.09764687597715,-1.47495783377641));
#52423=CARTESIAN_POINT('Ctrl Pts',(-22.5326339278449,1.83448840962079,0.122399145126971));
#52424=CARTESIAN_POINT('Ctrl Pts',(-22.4214875829675,0.891967972949703,
1.6077071906889));
#52425=CARTESIAN_POINT('Ctrl Pts',(-22.3103412380901,-0.867094604110294,
1.6212576054667));
#52426=CARTESIAN_POINT('Ctrl Pts',(-22.2331974523021,-1.53707761145306,
0.600544227981854));
#52427=CARTESIAN_POINT('Ctrl Pts',(-22.19310244814,-1.55786031009659,0.0431152295569864));
#52428=CARTESIAN_POINT('Ctrl Pts',(-22.1900562256037,-1.55760963761123,
0.00074552862925974));
#52429=CARTESIAN_POINT('Ctrl Pts',(-22.7519437743963,-1.55745576654889,
0.000858804331327978));
#52430=CARTESIAN_POINT('Ctrl Pts',(-22.718483071344,-1.55436544988659,-0.464665174858028));
#52431=CARTESIAN_POINT('Ctrl Pts',(-22.647973586666,-1.08543011851931,-1.45103340573419));
#52432=CARTESIAN_POINT('Ctrl Pts',(-22.5404153203621,0.592083708909288,
-1.74062231273063));
#52433=CARTESIAN_POINT('Ctrl Pts',(-22.4292689754847,1.78354194798782,-0.446438432148635));
#52434=CARTESIAN_POINT('Ctrl Pts',(-22.3181226306072,1.34227658728578,1.25643253585536));
#52435=CARTESIAN_POINT('Ctrl Pts',(-22.2069762857299,-0.327760916379816,
1.80911634109733));
#52436=CARTESIAN_POINT('Ctrl Pts',(-22.1182500003262,-1.42140316864343,
0.928249222998958));
#52437=CARTESIAN_POINT('Ctrl Pts',(-22.0665724965483,-1.55440757188741,
0.205724536095963));
#52438=CARTESIAN_POINT('Ctrl Pts',(-22.0519437743963,-1.55340336122338,
0.00083994794706577));
#52439=CARTESIAN_POINT('Origin',(-30.9400562256037,0.,0.));
#52440=CARTESIAN_POINT('',(-23.5900562256037,-1.55295484690924,0.000117396959615165));
#52441=CARTESIAN_POINT('',(-23.4519437743963,-1.55599709585984,-0.00137840470682826));
#52442=CARTESIAN_POINT('',(-30.9400562256037,-1.5555,7.38654183493349E-13));
#52443=CARTESIAN_POINT('Ctrl Pts',(-23.5900562256037,-1.55295484690924,
0.000117396959615351));
#52444=CARTESIAN_POINT('Ctrl Pts',(-23.5710211609831,-1.55277522915461,
-0.266673313363955));
#52445=CARTESIAN_POINT('Ctrl Pts',(-23.5149373147366,-1.36063644227694,
-1.05297300594233));
#52446=CARTESIAN_POINT('Ctrl Pts',(-23.4218046868643,-0.111301360173381,
-1.83519516209704));
#52447=CARTESIAN_POINT('Ctrl Pts',(-23.3106583419868,1.48156975859047,-1.08870580332383));
#52448=CARTESIAN_POINT('Ctrl Pts',(-23.1995119971095,1.7181543530587,0.654427150129224));
#52449=CARTESIAN_POINT('Ctrl Pts',(-23.088365652232,0.381873692818719,1.79847206219441));
#52450=CARTESIAN_POINT('Ctrl Pts',(-22.9852137283968,-1.1827299709617,1.33225802021393));
#52451=CARTESIAN_POINT('Ctrl Pts',(-22.9191105861873,-1.55202272048022,
0.403955273988205));
#52452=CARTESIAN_POINT('Ctrl Pts',(-22.8900562256037,-1.5557675530206,-0.00140509975720522));
#52453=CARTESIAN_POINT('Ctrl Pts',(-23.4519437743963,-1.55599709585984,
-0.00137840470682786));
#52454=CARTESIAN_POINT('Ctrl Pts',(-23.4444912093914,-1.55695391316923,
-0.105315627600081));
#52455=CARTESIAN_POINT('Ctrl Pts',(-23.3999898627606,-1.50008141400989,
-0.724912339526726));
#52456=CARTESIAN_POINT('Ctrl Pts',(-23.3184397345041,-0.669080796948889,
-1.71250110688599));
#52457=CARTESIAN_POINT('Ctrl Pts',(-23.2072933896267,1.07600957223555,-1.49081606993921));
#52458=CARTESIAN_POINT('Ctrl Pts',(-23.0961470447492,1.83607896999803,0.0956199239828239));
#52459=CARTESIAN_POINT('Ctrl Pts',(-22.9850006998718,0.91533033667428,1.59452172412145));
#52460=CARTESIAN_POINT('Ctrl Pts',(-22.8738543549944,-0.843347252550528,
1.633736381901));
#52461=CARTESIAN_POINT('Ctrl Pts',(-22.7961687131692,-1.53296174585945,
0.615807054296229));
#52462=CARTESIAN_POINT('Ctrl Pts',(-22.7555318529698,-1.5577871492752,0.0507781563724314));
#52463=CARTESIAN_POINT('Ctrl Pts',(-22.7519437743963,-1.55745576654889,
0.000858804331327978));
#52464=CARTESIAN_POINT('Origin',(-30.9400562256037,0.,0.));
#52465=CARTESIAN_POINT('',(-24.2900562256037,-1.55619855523662,0.00134484759808584));
#52466=CARTESIAN_POINT('',(-24.1519437743963,-1.55294665859264,-7.17666052784641E-6));
#52467=CARTESIAN_POINT('',(-30.9400562256037,-1.5555,7.38654183493349E-13));
#52468=CARTESIAN_POINT('Ctrl Pts',(-24.2900562256037,-1.55619855523662,
0.00134484759808597));
#52469=CARTESIAN_POINT('Ctrl Pts',(-24.2599805174046,-1.55237655783788,
-0.417966273389163));
#52470=CARTESIAN_POINT('Ctrl Pts',(-24.1928560275796,-1.16125933967721,
-1.36009004702387));
#52471=CARTESIAN_POINT('Ctrl Pts',(-24.0886827561288,0.431186030422094,
-1.78729065429483));
#52472=CARTESIAN_POINT('Ctrl Pts',(-23.9775364112514,1.73550088513296,-0.606931588783731));
#52473=CARTESIAN_POINT('Ctrl Pts',(-23.866390066374,1.45107079566491,1.12903623579104));
#52474=CARTESIAN_POINT('Ctrl Pts',(-23.7552437214966,-0.161725882381191,
1.83144042074233));
#52475=CARTESIAN_POINT('Ctrl Pts',(-23.6631324412398,-1.37561804845037,
1.02411005643153));
#52476=CARTESIAN_POINT('Ctrl Pts',(-23.6080699426089,-1.55312482707299,
0.252593154260171));
#52477=CARTESIAN_POINT('Ctrl Pts',(-23.5900562256037,-1.55295484690924,
0.000117396959615351));
#52478=CARTESIAN_POINT('Ctrl Pts',(-24.1519437743963,-1.55294681014799,
-7.1762345521878E-6));
#52479=CARTESIAN_POINT('Ctrl Pts',(-24.1334505658129,-1.55295747420179,
-0.259206697087362));
#52480=CARTESIAN_POINT('Ctrl Pts',(-24.0779085756037,-1.36865343867832,
-1.03766509684273));
#52481=CARTESIAN_POINT('Ctrl Pts',(-23.9853178037686,-0.138066012129827,
-1.83337582896308));
#52482=CARTESIAN_POINT('Ctrl Pts',(-23.8741714588912,1.46552720872477,-1.11020680704943));
#52483=CARTESIAN_POINT('Ctrl Pts',(-23.7630251140138,1.7275198787737,0.629288663788884));
#52484=CARTESIAN_POINT('Ctrl Pts',(-23.6518787691364,0.408073727971786,
1.79270884040625));
#52485=CARTESIAN_POINT('Ctrl Pts',(-23.5481849892639,-1.17141938223886,
1.34704401839563));
#52486=CARTESIAN_POINT('Ctrl Pts',(-23.4815399910172,-1.55219730715134,
0.411385329884918));
#52487=CARTESIAN_POINT('Ctrl Pts',(-23.4519437743963,-1.55599709585984,
-0.00137840470682786));
#52488=CARTESIAN_POINT('Origin',(-30.9400562256037,0.,0.));
#52489=CARTESIAN_POINT('',(-24.9900562256037,-1.55730549994698,-0.000951908650860188));
#52490=CARTESIAN_POINT('',(-24.8519437743963,-1.55597074695684,0.00138208519957782));
#52491=CARTESIAN_POINT('',(-30.9400562256037,-1.5555,7.38654183493349E-13));
#52492=CARTESIAN_POINT('Ctrl Pts',(-24.9900562256037,-1.55730549994698,
-0.000951908650860013));
#52493=CARTESIAN_POINT('Ctrl Pts',(-24.9859886554519,-1.55771297063508,
-0.0575565832609528));
#52494=CARTESIAN_POINT('Ctrl Pts',(-24.9448723036742,-1.52922029296496,
-0.629320969721004));
#52495=CARTESIAN_POINT('Ctrl Pts',(-24.8667071702708,-0.822183211067854,
-1.64448899151042));
#52496=CARTESIAN_POINT('Ctrl Pts',(-24.7555608253933,0.935841500540801,
-1.58257068139984));
#52497=CARTESIAN_POINT('Ctrl Pts',(-24.644414480516,1.8371605398714,-0.071905677802479));
#52498=CARTESIAN_POINT('Ctrl Pts',(-24.5332681356385,1.05667143702865,1.50458457719352));
#52499=CARTESIAN_POINT('Ctrl Pts',(-24.4221217907611,-0.691135756872815,
1.70371964869008));
#52500=CARTESIAN_POINT('Ctrl Pts',(-24.3410511540828,-1.50450533882819,
0.711353178426976));
#52501=CARTESIAN_POINT('Ctrl Pts',(-24.2970292990304,-1.55708468793618,
0.0985624165376092));
#52502=CARTESIAN_POINT('Ctrl Pts',(-24.2900562256037,-1.55619855523662,
0.00134484759808597));
#52503=CARTESIAN_POINT('Ctrl Pts',(-24.8519437743963,-1.55597074695684,
0.00138208519957779));
#52504=CARTESIAN_POINT('Ctrl Pts',(-24.8224099222344,-1.5521757198559,-0.41052982565668));
#52505=CARTESIAN_POINT('Ctrl Pts',(-24.7558272884467,-1.17273038095177,
-1.3453445318586));
#52506=CARTESIAN_POINT('Ctrl Pts',(-24.6521958730331,0.405062575138557,
-1.79339160925706));
#52507=CARTESIAN_POINT('Ctrl Pts',(-24.5410495281557,1.72646064975028,-0.632188879050662));
#52508=CARTESIAN_POINT('Ctrl Pts',(-24.4299031832783,1.46738956291618,1.10774411511692));
#52509=CARTESIAN_POINT('Ctrl Pts',(-24.3187568384009,-0.134986946113292,
1.83360510424424));
#52510=CARTESIAN_POINT('Ctrl Pts',(-24.2261037021069,-1.36773867089657,
1.03942751774699));
#52511=CARTESIAN_POINT('Ctrl Pts',(-24.1704993474387,-1.55293611013191,
0.260066440522905));
#52512=CARTESIAN_POINT('Ctrl Pts',(-24.1519437743963,-1.55294681014799,
-7.1762345521878E-6));
#52513=CARTESIAN_POINT('Origin',(-30.9400562256037,0.,0.));
#52514=CARTESIAN_POINT('',(-25.6900562256037,-1.55329993577148,-0.000747905064743873));
#52515=CARTESIAN_POINT('',(-25.5519437743963,-1.55747437566469,-0.000846187651558084));
#52516=CARTESIAN_POINT('',(-30.9400562256037,-1.5555,7.38654183493349E-13));
#52517=CARTESIAN_POINT('Ctrl Pts',(-25.6900562256037,-1.55329993577148,
-0.000747905064743624));
#52518=CARTESIAN_POINT('Ctrl Pts',(-25.6749480118734,-1.55421977858412,
-0.21238335774611));
#52519=CARTESIAN_POINT('Ctrl Pts',(-25.6227910165173,-1.41527094711558,
-0.941840467750138));
#52520=CARTESIAN_POINT('Ctrl Pts',(-25.5335852395354,-0.304375448471892,
-1.81319741399803));
#52521=CARTESIAN_POINT('Ctrl Pts',(-25.4224388946579,1.35838697931157,-1.23899721153737));
#52522=CARTESIAN_POINT('Ctrl Pts',(-25.3112925497805,1.77762918529204,0.469429180344255));
#52523=CARTESIAN_POINT('Ctrl Pts',(-25.200146204903,0.569560564207642,1.74812186058649));
#52524=CARTESIAN_POINT('Ctrl Pts',(-25.0930674301775,-1.09661346171798,
1.43828552764103));
#52525=CARTESIAN_POINT('Ctrl Pts',(-25.0230374370777,-1.55400159210223,
0.458017617145497));
#52526=CARTESIAN_POINT('Ctrl Pts',(-24.9900562256037,-1.55730549994698,
-0.000951908650860013));
#52527=CARTESIAN_POINT('Ctrl Pts',(-25.5519437743963,-1.55747437566469,
-0.000846187651558162));
#52528=CARTESIAN_POINT('Ctrl Pts',(-25.5484180602817,-1.55779615002965,
-0.0498963460263509));
#52529=CARTESIAN_POINT('Ctrl Pts',(-25.5078435645413,-1.53344150154939,
-0.614049915219279));
#52530=CARTESIAN_POINT('Ctrl Pts',(-25.4302202871752,-0.846089671080599,
-1.63231780680796));
#52531=CARTESIAN_POINT('Ctrl Pts',(-25.3190739422977,0.912651293186798,
-1.59605663150652));
#52532=CARTESIAN_POINT('Ctrl Pts',(-25.2079275974203,1.83591580205738,-0.0987031999860136));
#52533=CARTESIAN_POINT('Ctrl Pts',(-25.0967812525428,1.07851165011462,1.48900697597377));
#52534=CARTESIAN_POINT('Ctrl Pts',(-24.9856349076655,-0.666203972560349,
1.7136223098677));
#52535=CARTESIAN_POINT('Ctrl Pts',(-24.9040224149499,-1.4994986854534,0.726676294106424));
#52536=CARTESIAN_POINT('Ctrl Pts',(-24.8594587038602,-1.55693639684298,
0.10619363969844));
#52537=CARTESIAN_POINT('Ctrl Pts',(-24.8519437743963,-1.55597074695684,
0.00138208519957779));
#52538=CARTESIAN_POINT('Origin',(-30.9400562256037,0.,0.));
#52539=CARTESIAN_POINT('',(-26.3900562256037,-1.55457327774435,0.00134739417963825));
#52540=CARTESIAN_POINT('',(-26.2519437743963,-1.5534177173597,-0.000851565729181603));
#52541=CARTESIAN_POINT('',(-30.9400562256037,-1.5555,7.38654183493349E-13));
#52542=CARTESIAN_POINT('Ctrl Pts',(-26.3900562256037,-1.55457327774435,
0.00134739417963841));
#52543=CARTESIAN_POINT('Ctrl Pts',(-26.3639073682949,-1.55154654523881,
-0.364190570873877));
#52544=CARTESIAN_POINT('Ctrl Pts',(-26.3007097293602,-1.2403310165763,-1.25227730661038));
#52545=CARTESIAN_POINT('Ctrl Pts',(-26.2004633087999,0.240137974670818,
-1.8228173328443));
#52546=CARTESIAN_POINT('Ctrl Pts',(-26.0893169639224,1.66174866141038,-0.786715108572567));
#52547=CARTESIAN_POINT('Ctrl Pts',(-25.978170619045,1.56213005525038,0.969576694355506));
#52548=CARTESIAN_POINT('Ctrl Pts',(-25.8670242741676,0.032476899015307,
1.8382803177961));
#52549=CARTESIAN_POINT('Ctrl Pts',(-25.7709861430205,-1.3149385586997,1.13481601539216));
#52550=CARTESIAN_POINT('Ctrl Pts',(-25.7119967934992,-1.55196411447294,
0.306594981495643));
#52551=CARTESIAN_POINT('Ctrl Pts',(-25.6900562256037,-1.55329993577148,
-0.000747905064743624));
#52552=CARTESIAN_POINT('Ctrl Pts',(-26.2519437743963,-1.5534177173597,-0.00085156572918162));
#52553=CARTESIAN_POINT('Ctrl Pts',(-26.2373774167032,-1.55443203746226,
-0.204857978458031));
#52554=CARTESIAN_POINT('Ctrl Pts',(-26.1857622773843,-1.42219235049638,
-0.926481326314944));
#52555=CARTESIAN_POINT('Ctrl Pts',(-26.0970983564397,-0.330798585473345,
-1.80856336626222));
#52556=CARTESIAN_POINT('Ctrl Pts',(-25.9859520115622,1.340164710296,-1.25868491021684));
#52557=CARTESIAN_POINT('Ctrl Pts',(-25.8748056666848,1.78428915735557,0.443442619595842));
#52558=CARTESIAN_POINT('Ctrl Pts',(-25.7636593218074,0.595005980146546,
1.7396255452028));
#52559=CARTESIAN_POINT('Ctrl Pts',(-25.6560386910445,-1.08396473869043,
1.4526878959));
#52560=CARTESIAN_POINT('Ctrl Pts',(-25.5854668419075,-1.55441489227795,
0.465530755344284));
#52561=CARTESIAN_POINT('Ctrl Pts',(-25.5519437743963,-1.55747437566469,
-0.000846187651558162));
#52562=CARTESIAN_POINT('Origin',(-30.9400562256037,0.,0.));
#52563=CARTESIAN_POINT('',(-27.0900562256037,-1.5580501213287,-3.65571210202475E-5));
#52564=CARTESIAN_POINT('',(-26.9519437743963,-1.55436975637195,0.00130097926851286));
#52565=CARTESIAN_POINT('',(-30.9400562256037,-1.5555,7.38654183493349E-13));
#52566=CARTESIAN_POINT('Ctrl Pts',(-27.0900562256037,-1.5580501213287,-3.65571210204235E-5));
#52567=CARTESIAN_POINT('Ctrl Pts',(-27.0899155063422,-1.55805079701309,
-0.00199233735013099));
#52568=CARTESIAN_POINT('Ctrl Pts',(-27.0527260054549,-1.55716171500239,
-0.518868284418442));
#52569=CARTESIAN_POINT('Ctrl Pts',(-26.9784877229418,-0.991158593083783,
-1.54852636916561));
#52570=CARTESIAN_POINT('Ctrl Pts',(-26.8673413780644,0.763581882211757,
-1.67250470444365));
#52571=CARTESIAN_POINT('Ctrl Pts',(-26.756195033187,1.81930983338734,-0.265407245427431));
#52572=CARTESIAN_POINT('Ctrl Pts',(-26.6450486883096,1.20957087255313,1.38465431773148));
#52573=CARTESIAN_POINT('Ctrl Pts',(-26.5339023434321,-0.507456263538371,
1.76714951732695));
#52574=CARTESIAN_POINT('Ctrl Pts',(-26.4489048558636,-1.4652729107266,0.82253205856728));
#52575=CARTESIAN_POINT('Ctrl Pts',(-26.4009561499207,-1.55583494493112,
0.153718723718826));
#52576=CARTESIAN_POINT('Ctrl Pts',(-26.3900562256037,-1.55457327774435,
0.00134739417963841));
#52577=CARTESIAN_POINT('Ctrl Pts',(-26.9519437743963,-1.55436975637195,
0.00130097926851296));
#52578=CARTESIAN_POINT('Ctrl Pts',(-26.9263367731247,-1.55153485082019,
-0.356780851543248));
#52579=CARTESIAN_POINT('Ctrl Pts',(-26.8636809902274,-1.25051393155525,
-1.23724720927912));
#52580=CARTESIAN_POINT('Ctrl Pts',(-26.7639764257042,0.213516505753145,
-1.82612700980389));
#52581=CARTESIAN_POINT('Ctrl Pts',(-26.6528300808268,1.65009313818133,-0.810877172722089));
#52582=CARTESIAN_POINT('Ctrl Pts',(-26.5416837359494,1.5761103965168,0.946681135265884));
#52583=CARTESIAN_POINT('Ctrl Pts',(-26.4305373910719,0.0592949571880597,
1.83761074823246));
#52584=CARTESIAN_POINT('Ctrl Pts',(-26.3339574038876,-1.30590031967722,
1.15002320221466));
#52585=CARTESIAN_POINT('Ctrl Pts',(-26.274426198329,-1.55185216644918,0.314021840005712));
#52586=CARTESIAN_POINT('Ctrl Pts',(-26.2519437743963,-1.5534177173597,-0.00085156572918162));
#52587=CARTESIAN_POINT('Origin',(-30.9400562256037,0.,0.));
#52588=CARTESIAN_POINT('',(-27.7900562256037,-1.55446647382692,-0.00132458884794142));
#52589=CARTESIAN_POINT('',(-27.6519437743963,-1.55804245891508,0.000104104215403816));
#52590=CARTESIAN_POINT('',(-30.9400562256037,-1.5555,7.38654183493349E-13));
#52591=CARTESIAN_POINT('Ctrl Pts',(-27.7900562256037,-1.55446647382692,
-0.00132458884794144));
#52592=CARTESIAN_POINT('Ctrl Pts',(-27.7788748627637,-1.5557324439126,-0.157657369512062));
#52593=CARTESIAN_POINT('Ctrl Pts',(-27.730644718298,-1.46219237042214,-0.830509405833625));
#52594=CARTESIAN_POINT('Ctrl Pts',(-27.6453657922064,-0.494049365075557,
-1.77094447718388));
#52595=CARTESIAN_POINT('Ctrl Pts',(-27.534219447329,1.22002971701301,-1.37544786085574));
#52596=CARTESIAN_POINT('Ctrl Pts',(-27.4230731024515,1.81724620484857,0.279187250412826));
#52597=CARTESIAN_POINT('Ctrl Pts',(-27.3119267575741,0.750884899378822,
1.67824346299867));
#52598=CARTESIAN_POINT('Ctrl Pts',(-27.2009211319582,-1.00064524107714,
1.54114421983883));
#52599=CARTESIAN_POINT('Ctrl Pts',(-27.126964287968,-1.55787290179637,0.512928462058482));
#52600=CARTESIAN_POINT('Ctrl Pts',(-27.0900562256037,-1.5580501213287,-3.65571210204235E-5));
#52601=CARTESIAN_POINT('Ctrl Pts',(-27.6519437743963,-1.55804245891508,
0.000104104215403655));
#52602=CARTESIAN_POINT('Ctrl Pts',(-27.6152961295462,-1.5575504591777,-0.509248245460903));
#52603=CARTESIAN_POINT('Ctrl Pts',(-27.5415997030704,-1.00732110649725,
-1.53443975582773));
#52604=CARTESIAN_POINT('Ctrl Pts',(-27.4308544949688,0.739097826986148,
-1.68346772023046));
#52605=CARTESIAN_POINT('Ctrl Pts',(-27.3197081500913,1.81524370282257,-0.291923713345362));
#52606=CARTESIAN_POINT('Ctrl Pts',(-27.2085618052139,1.22964495869491,1.36685859779542));
#52607=CARTESIAN_POINT('Ctrl Pts',(-27.0974154603365,-0.48161855815431,
1.77436544145867));
#52608=CARTESIAN_POINT('Ctrl Pts',(-27.0118761167306,-1.45930897725486,
0.83789144882417));
#52609=CARTESIAN_POINT('Ctrl Pts',(-26.9633855547505,-1.55563645551818,
0.161299942581343));
#52610=CARTESIAN_POINT('Ctrl Pts',(-26.9519437743963,-1.55436975637195,
0.00130097926851296));
#52611=CARTESIAN_POINT('Origin',(-30.9400562256037,0.,0.));
#52612=CARTESIAN_POINT('',(-28.4900562256037,-1.55335883765056,0.000804378038691873));
#52613=CARTESIAN_POINT('',(-28.3519437743963,-1.55467403768283,-0.00136587788398465));
#52614=CARTESIAN_POINT('',(-30.9400562256037,-1.5555,7.38654183493349E-13));
#52615=CARTESIAN_POINT('Ctrl Pts',(-28.4900562256037,-1.55335883765056,
0.000804378038691943));
#52616=CARTESIAN_POINT('Ctrl Pts',(-28.4678342191853,-1.5519039872972,-0.310451991356807));
#52617=CARTESIAN_POINT('Ctrl Pts',(-28.408563431141,-1.31026523547163,-1.14272024251096));
#52618=CARTESIAN_POINT('Ctrl Pts',(-28.3122438614709,0.046407699775919,
-1.83797936794685));
#52619=CARTESIAN_POINT('Ctrl Pts',(-28.2010975165935,1.56943293437681,-0.95771133892945));
#52620=CARTESIAN_POINT('Ctrl Pts',(-28.089951171716,1.65573892814966,0.799286617882397));
#52621=CARTESIAN_POINT('Ctrl Pts',(-27.9788048268387,0.226316831424914,
1.82458457360074));
#52622=CARTESIAN_POINT('Ctrl Pts',(-27.8788398448012,-1.24564163566608,
1.24447484849783));
#52623=CARTESIAN_POINT('Ctrl Pts',(-27.8159236443895,-1.55153772722909,
0.360342013449946));
#52624=CARTESIAN_POINT('Ctrl Pts',(-27.7900562256037,-1.55446647382692,
-0.00132458884794144));
#52625=CARTESIAN_POINT('Ctrl Pts',(-28.3519437743963,-1.55467403768283,
-0.0013658778839847));
#52626=CARTESIAN_POINT('Ctrl Pts',(-28.3413042675936,-1.55592857918768,
-0.150072444919674));
#52627=CARTESIAN_POINT('Ctrl Pts',(-28.293615979165,-1.46809072386952,-0.815151663224704));
#52628=CARTESIAN_POINT('Ctrl Pts',(-28.2088789091108,-0.519835724455463,
-1.76354724094302));
#52629=CARTESIAN_POINT('Ctrl Pts',(-28.0977325642333,1.19983124114152,-1.39310245061395));
#52630=CARTESIAN_POINT('Ctrl Pts',(-27.9865862193559,1.82112625016851,0.252642976453954));
#52631=CARTESIAN_POINT('Ctrl Pts',(-27.8754398744784,0.775291433296788,
1.66710893100567));
#52632=CARTESIAN_POINT('Ctrl Pts',(-27.764293529601,-0.980275235800491,
1.55543873831543));
#52633=CARTESIAN_POINT('Ctrl Pts',(-27.6897948295736,-1.55549560212386,
0.526177148100607));
#52634=CARTESIAN_POINT('Ctrl Pts',(-27.6523449111721,-1.55804784423217,
0.00567935905418177));
#52635=CARTESIAN_POINT('Ctrl Pts',(-27.6519437743963,-1.55804245891508,
0.000104104215403655));
#52636=CARTESIAN_POINT('Origin',(-30.9400562256037,0.,0.));
#52637=CARTESIAN_POINT('',(-29.1900562256037,-1.55737653422887,0.00100621910560842));
#52638=CARTESIAN_POINT('',(-29.0519437743963,-1.55324480116086,0.000708030066551985));
#52639=CARTESIAN_POINT('',(-30.9400562256037,-1.5555,7.38654183493349E-13));
#52640=CARTESIAN_POINT('Ctrl Pts',(-29.1900562256037,-1.55737653422887,
0.00100621910560853));
#52641=CARTESIAN_POINT('Ctrl Pts',(-29.1567935756068,-1.55418812333816,
-0.461781077921097));
#52642=CARTESIAN_POINT('Ctrl Pts',(-29.086482143984,-1.09009726042822,-1.44594760124546));
#52643=CARTESIAN_POINT('Ctrl Pts',(-28.9791219307355,0.582808968573894,
-1.74365887083216));
#52644=CARTESIAN_POINT('Ctrl Pts',(-28.867975585858,1.78112695043666,-0.455994626000207));
#52645=CARTESIAN_POINT('Ctrl Pts',(-28.7568292409806,1.34896284622222,1.24928278177877));
#52646=CARTESIAN_POINT('Ctrl Pts',(-28.6456828961032,-0.318110417184717,
1.81082463803951));
#52647=CARTESIAN_POINT('Ctrl Pts',(-28.5567585576442,-1.41888362636568,
0.933866456267556));
#52648=CARTESIAN_POINT('Ctrl Pts',(-28.5048830008111,-1.55432953033886,
0.208478164733725));
#52649=CARTESIAN_POINT('Ctrl Pts',(-28.4900562256037,-1.55335883765056,
0.000804378038691943));
#52650=CARTESIAN_POINT('Ctrl Pts',(-29.0519437743963,-1.55324480116087,
0.00070803006655188));
#52651=CARTESIAN_POINT('Ctrl Pts',(-29.0302636240151,-1.55202060661361,
-0.303017220285967));
#52652=CARTESIAN_POINT('Ctrl Pts',(-28.971534692008,-1.31923084685054,-1.12752040336955));
#52653=CARTESIAN_POINT('Ctrl Pts',(-28.8757569783753,0.0195899148733162,
-1.83844939731259));
#52654=CARTESIAN_POINT('Ctrl Pts',(-28.7646106334978,1.55529006052317,-0.980514255533821));
#52655=CARTESIAN_POINT('Ctrl Pts',(-28.6534642886204,1.6672258610176,0.775046535726967));
#52656=CARTESIAN_POINT('Ctrl Pts',(-28.542317943743,0.252913801877688,1.82108657460817));
#52657=CARTESIAN_POINT('Ctrl Pts',(-28.4418111056683,-1.23537493202417,
1.25948986433566));
#52658=CARTESIAN_POINT('Ctrl Pts',(-28.3783530492194,-1.55156002760766,
0.367752039860246));
#52659=CARTESIAN_POINT('Ctrl Pts',(-28.3519437743963,-1.55467403768283,
-0.0013658778839847));
#52660=CARTESIAN_POINT('Origin',(-0.2,2.59090492670967E-16,0.));
#52661=CARTESIAN_POINT('',(-0.2,0.0853826423430817,1.95213365433479));
#52662=CARTESIAN_POINT('Ctrl Pts',(-0.200000000000004,1.33821259954893,
-0.797996165557001));
#52663=CARTESIAN_POINT('Ctrl Pts',(-0.200000000000003,1.36083146673087,
-0.769266098091291));
#52664=CARTESIAN_POINT('Ctrl Pts',(-0.199999999999999,1.38232620666805,
-0.739737377686227));
#52665=CARTESIAN_POINT('Ctrl Pts',(-0.199999999999999,1.40263605993815,
-0.709452586790428));
#52666=CARTESIAN_POINT('Ctrl Pts',(-0.2,1.43566749400714,-0.660198165280631));
#52667=CARTESIAN_POINT('Ctrl Pts',(-0.199999999999991,1.46556712027168,
-0.608945988984861));
#52668=CARTESIAN_POINT('Ctrl Pts',(-0.199999999999987,1.49239176656985,
-0.556021150339029));
#52669=CARTESIAN_POINT('Ctrl Pts',(-0.199999999999985,1.50784007518276,
-0.525541746003136));
#52670=CARTESIAN_POINT('Ctrl Pts',(-0.199999999999994,1.52226790514226,
-0.494506807866819));
#52671=CARTESIAN_POINT('Ctrl Pts',(-0.199999999999996,1.53568068894636,
-0.462973130619356));
#52672=CARTESIAN_POINT('Ctrl Pts',(-0.199999999999997,1.54263081553624,
-0.446633267700872));
#52673=CARTESIAN_POINT('Ctrl Pts',(-0.199999999999989,1.54930985473548,
-0.4301550048461));
#52674=CARTESIAN_POINT('Ctrl Pts',(-0.199999999999989,1.55570791547876,
-0.413573830206026));
#52675=CARTESIAN_POINT('Ctrl Pts',(-0.199999999999988,1.57814412154956,
-0.355428297356665));
#52676=CARTESIAN_POINT('Ctrl Pts',(-0.199999999999984,1.59715451942584,
-0.295963114431022));
#52677=CARTESIAN_POINT('Ctrl Pts',(-0.199999999999987,1.6127982700493,-0.235533509212285));
#52678=CARTESIAN_POINT('Ctrl Pts',(-0.19999999999999,1.62482864572664,-0.189061862462472));
#52679=CARTESIAN_POINT('Ctrl Pts',(-0.199999999999983,1.63486727068506,
-0.142018843352932));
#52680=CARTESIAN_POINT('Ctrl Pts',(-0.199999999999983,1.64292447455769,
-0.0945533019233128));
#52681=CARTESIAN_POINT('Ctrl Pts',(-0.199999999999983,1.64689952531549,
-0.0711360048793496));
#52682=CARTESIAN_POINT('Ctrl Pts',(-0.199999999999985,1.65039207440413,
-0.047615726128019));
#52683=CARTESIAN_POINT('Ctrl Pts',(-0.199999999999984,1.65340199272743,
-0.0240096709125676));
#52684=CARTESIAN_POINT('Ctrl Pts',(-0.199999999999984,1.65494614856356,
-0.0118992333479225));
#52685=CARTESIAN_POINT('Ctrl Pts',(-0.199999999999997,1.65636206949049,
0.000224531212346389));
#52686=CARTESIAN_POINT('Ctrl Pts',(-0.199999999999996,1.65765003815761,
0.0123570392677572));
#52687=CARTESIAN_POINT('Ctrl Pts',(-0.199999999999995,1.66448973811924,
0.0767861802857205));
#52688=CARTESIAN_POINT('Ctrl Pts',(-0.199999999999997,1.66772693008277,
0.141478210488262));
#52689=CARTESIAN_POINT('Ctrl Pts',(-0.199999999999996,1.6674177087189,0.206071916622556));
#52690=CARTESIAN_POINT('Ctrl Pts',(-0.199999999999995,1.66710248839164,
0.271918755053447));
#52691=CARTESIAN_POINT('Ctrl Pts',(-0.199999999999987,1.66310228737439,
0.337664448069482));
#52692=CARTESIAN_POINT('Ctrl Pts',(-0.199999999999986,1.65542859034139,
0.402950019404703));
#52693=CARTESIAN_POINT('Ctrl Pts',(-0.199999999999985,1.65047305117389,
0.445110298137822));
#52694=CARTESIAN_POINT('Ctrl Pts',(-0.199999999999992,1.64398454736424,
0.487079135065034));
#52695=CARTESIAN_POINT('Ctrl Pts',(-0.199999999999993,1.63595477654208,
0.528761747087024));
#52696=CARTESIAN_POINT('Ctrl Pts',(-0.199999999999993,1.6314372854833,0.552212083502153));
#52697=CARTESIAN_POINT('Ctrl Pts',(-0.199999999999989,1.62643180252044,
0.575571836727543));
#52698=CARTESIAN_POINT('Ctrl Pts',(-0.199999999999988,1.62093554824454,
0.598824048775656));
#52699=CARTESIAN_POINT('Ctrl Pts',(-0.199999999999988,1.61825461164952,
0.610165901438495));
#52700=CARTESIAN_POINT('Ctrl Pts',(-0.199999999999994,1.61545644305892,
0.621483904474924));
#52701=CARTESIAN_POINT('Ctrl Pts',(-0.199999999999994,1.61254205914868,
0.632770588829928));
#52702=CARTESIAN_POINT('Ctrl Pts',(-0.199999999999993,1.59558819313177,
0.698428697103724));
#52703=CARTESIAN_POINT('Ctrl Pts',(-0.199999999999995,1.57477263017097,
0.762771028666577));
#52704=CARTESIAN_POINT('Ctrl Pts',(-0.199999999999997,1.55012986044755,
0.82542185568922));
#52705=CARTESIAN_POINT('Ctrl Pts',(-0.199999999999998,1.54138328915035,
0.847658801111062));
#52706=CARTESIAN_POINT('Ctrl Pts',(-0.199999999999995,1.5321541065797,0.86968277159213));
#52707=CARTESIAN_POINT('Ctrl Pts',(-0.199999999999995,1.52244229463082,
0.891477201154086));
#52708=CARTESIAN_POINT('Ctrl Pts',(-0.199999999999995,1.49604924959517,
0.950706247596028));
#52709=CARTESIAN_POINT('Ctrl Pts',(-0.199999999999994,1.4660955787197,1.00824097839801));
#52710=CARTESIAN_POINT('Ctrl Pts',(-0.199999999999996,1.43287445271699,
1.06395280437091));
#52711=CARTESIAN_POINT('Ctrl Pts',(-0.199999999999997,1.41494791261197,
1.09401561086777));
#52712=CARTESIAN_POINT('Ctrl Pts',(-0.199999999999993,1.39606904617647,
1.123547433112));
#52713=CARTESIAN_POINT('Ctrl Pts',(-0.199999999999994,1.37627808156598,
1.15252619254564));
#52714=CARTESIAN_POINT('Ctrl Pts',(-0.199999999999995,1.3622243467481,1.17310425978223));
#52715=CARTESIAN_POINT('Ctrl Pts',(-0.199999999999992,1.34771059846554,
1.19340341412927));
#52716=CARTESIAN_POINT('Ctrl Pts',(-0.199999999999993,1.3327501250156,1.21341519986235));
#52717=CARTESIAN_POINT('Ctrl Pts',(-0.199999999999993,1.32597618088804,
1.22247632475938));
#52718=CARTESIAN_POINT('Ctrl Pts',(-0.199999999999993,1.31910926376118,
1.23148028792388));
#52719=CARTESIAN_POINT('Ctrl Pts',(-0.199999999999993,1.31215500866612,
1.24042055272821));
#52720=CARTESIAN_POINT('Ctrl Pts',(-0.199999999999992,1.27060407929176,
1.29383767740876));
#52721=CARTESIAN_POINT('Ctrl Pts',(-0.199999999999984,1.22606300839517,
1.3448257906629));
#52722=CARTESIAN_POINT('Ctrl Pts',(-0.199999999999985,1.17887277817311,
1.39325604164226));
#52723=CARTESIAN_POINT('Ctrl Pts',(-0.199999999999986,1.13064656854509,
1.44274949452599));
#52724=CARTESIAN_POINT('Ctrl Pts',(-0.199999999999989,1.07965311599888,
1.48957227465749));
#52725=CARTESIAN_POINT('Ctrl Pts',(-0.199999999999988,1.02620391534963,
1.5335686727213));
#52726=CARTESIAN_POINT('Ctrl Pts',(-0.199999999999988,0.97226644704798,
1.57796698545803));
#52727=CARTESIAN_POINT('Ctrl Pts',(-0.199999999999996,0.915827484062048,
1.61948781404837));
#52728=CARTESIAN_POINT('Ctrl Pts',(-0.199999999999996,0.857163347037397,
1.65794145013127));
#52729=CARTESIAN_POINT('Ctrl Pts',(-0.199999999999997,0.834333137919339,
1.67290637755794));
#52730=CARTESIAN_POINT('Ctrl Pts',(-0.200000000000002,0.81116551130864,
1.68740639452663));
#52731=CARTESIAN_POINT('Ctrl Pts',(-0.200000000000001,0.787675332375756,
1.70142872353338));
#52732=CARTESIAN_POINT('Ctrl Pts',(-0.200000000000001,0.778712552141178,
1.70677900433045));
#52733=CARTESIAN_POINT('Ctrl Pts',(-0.199999999999995,0.769704701380117,
1.71205854430649));
#52734=CARTESIAN_POINT('Ctrl Pts',(-0.199999999999995,0.760660445012377,
1.71726235891511));
#52735=CARTESIAN_POINT('Ctrl Pts',(-0.199999999999992,0.698085449280864,
1.75326627827364));
#52736=CARTESIAN_POINT('Ctrl Pts',(-0.19999999999998,0.633667777713838,
1.78570985411892));
#52737=CARTESIAN_POINT('Ctrl Pts',(-0.199999999999981,0.567740838726636,
1.81443271252908));
#52738=CARTESIAN_POINT('Ctrl Pts',(-0.199999999999982,0.501663825842382,
1.84322095470136));
#52739=CARTESIAN_POINT('Ctrl Pts',(-0.199999999999981,0.434069865483067,
1.86827227177555));
#52740=CARTESIAN_POINT('Ctrl Pts',(-0.199999999999979,0.365255754338618,
1.88939040512503));
#52741=CARTESIAN_POINT('Ctrl Pts',(-0.199999999999978,0.297913662913918,
1.91005679524601));
#52742=CARTESIAN_POINT('Ctrl Pts',(-0.199999999999988,0.229402198343265,
1.92695702889807));
#52743=CARTESIAN_POINT('Ctrl Pts',(-0.199999999999987,0.159974824830696,
1.93986449335383));
#52744=CARTESIAN_POINT('Ctrl Pts',(-0.199999999999987,0.135223669558322,
1.94446605957698));
#52745=CARTESIAN_POINT('Ctrl Pts',(-0.199999999999991,0.110355935852113,
1.9485597226482));
#52746=CARTESIAN_POINT('Ctrl Pts',(-0.199999999999991,0.0853826423429707,
1.9521336543348));
#52747=CARTESIAN_POINT('',(-0.200000000000025,-1.49576935231745,1.26229836271313));
#52748=CARTESIAN_POINT('Origin',(-0.2,0.,0.));
#52749=CARTESIAN_POINT('Ctrl Pts',(-0.199999999999997,-1.49578438409795,
1.26230645381927));
#52750=CARTESIAN_POINT('Ctrl Pts',(-0.199999999999997,-1.52168996012369,
1.22501433090188));
#52751=CARTESIAN_POINT('Ctrl Pts',(-0.199999999999991,-1.5461641556753,
1.18681013346276));
#52752=CARTESIAN_POINT('Ctrl Pts',(-0.199999999999995,-1.5691243985238,
1.14772495209047));
#52753=CARTESIAN_POINT('Ctrl Pts',(-0.199999999999999,-1.60551023262156,
1.08578541014067));
#52754=CARTESIAN_POINT('Ctrl Pts',(-0.199999999999998,-1.63809649512831,
1.02163357061851));
#52755=CARTESIAN_POINT('Ctrl Pts',(-0.199999999999997,-1.6668721870644,
0.955646304386221));
#52756=CARTESIAN_POINT('Ctrl Pts',(-0.199999999999997,-1.68055611898491,
0.924266858819843));
#52757=CARTESIAN_POINT('Ctrl Pts',(-0.199999999999998,-1.69337759315812,
0.892472194507605));
#52758=CARTESIAN_POINT('Ctrl Pts',(-0.199999999999999,-1.70533138078191,
0.860302523849142));
#52759=CARTESIAN_POINT('Ctrl Pts',(-0.199999999999999,-1.71156562096785,
0.843525125764171));
#52760=CARTESIAN_POINT('Ctrl Pts',(-0.200000000000005,-1.71756381466397,
0.826645730493394));
#52761=CARTESIAN_POINT('Ctrl Pts',(-0.200000000000006,-1.72332494158841,
0.809670073695925));
#52762=CARTESIAN_POINT('Ctrl Pts',(-0.200000000000007,-1.72807906609128,
0.795661636285706));
#52763=CARTESIAN_POINT('Ctrl Pts',(-0.2,-1.73266865506746,0.781596710180168));
#52764=CARTESIAN_POINT('Ctrl Pts',(-0.200000000000001,-1.73709291763167,
0.767481383246849));
#52765=CARTESIAN_POINT('Ctrl Pts',(-0.200000000000004,-1.75844509037697,
0.699358640832162));
#52766=CARTESIAN_POINT('Ctrl Pts',(-0.200000000000006,-1.77595779613622,
0.63004133653378));
#52767=CARTESIAN_POINT('Ctrl Pts',(-0.200000000000013,-1.78961532543345,
0.5599012489287));
#52768=CARTESIAN_POINT('Ctrl Pts',(-0.200000000000018,-1.79936972654671,
0.509806203644238));
#52769=CARTESIAN_POINT('Ctrl Pts',(-0.200000000000009,-1.80715648654673,
0.459291207712322));
#52770=CARTESIAN_POINT('Ctrl Pts',(-0.200000000000011,-1.81295369990729,
0.408493543644497));
#52771=CARTESIAN_POINT('Ctrl Pts',(-0.200000000000012,-1.81629536353796,
0.379212457029137));
#52772=CARTESIAN_POINT('Ctrl Pts',(-0.200000000000004,-1.8189757195653,
0.349837501668433));
#52773=CARTESIAN_POINT('Ctrl Pts',(-0.200000000000005,-1.8209885736095,
0.320395678757213));
#52774=CARTESIAN_POINT('Ctrl Pts',(-0.200000000000006,-1.82184695550393,
0.30784020917476));
#52775=CARTESIAN_POINT('Ctrl Pts',(-0.199999999999998,-1.822583285484,0.295281755485384));
#52776=CARTESIAN_POINT('Ctrl Pts',(-0.199999999999999,-1.82319746824128,
0.282724832221508));
#52777=CARTESIAN_POINT('Ctrl Pts',(-0.200000000000001,-1.82659875079537,
0.21318584968782));
#52778=CARTESIAN_POINT('Ctrl Pts',(-0.200000000000006,-1.82625986266907,
0.14366821824979));
#52779=CARTESIAN_POINT('Ctrl Pts',(-0.200000000000005,-1.82216318737456,
0.0745161284520812));
#52780=CARTESIAN_POINT('Ctrl Pts',(-0.200000000000004,-1.8181675098021,
0.00706888540006578));
#52781=CARTESIAN_POINT('Ctrl Pts',(-0.199999999999997,-1.81059674010245,
-0.0600315443553361));
#52782=CARTESIAN_POINT('Ctrl Pts',(-0.199999999999997,-1.79938824077835,
-0.126450987847281));
#52783=CARTESIAN_POINT('Ctrl Pts',(-0.199999999999997,-1.79202556984101,
-0.170080780929468));
#52784=CARTESIAN_POINT('Ctrl Pts',(-0.199999999999998,-1.7830923059571,
-0.213416399555303));
#52785=CARTESIAN_POINT('Ctrl Pts',(-0.199999999999999,-1.77256029454147,
-0.256356695069847));
#52786=CARTESIAN_POINT('Ctrl Pts',(-0.2,-1.76373011398598,-0.292358418533345));
#52787=CARTESIAN_POINT('Ctrl Pts',(-0.199999999999999,-1.75377596763092,
-0.328082194465782));
#52788=CARTESIAN_POINT('Ctrl Pts',(-0.199999999999999,-1.74267690704633,
-0.363464633981315));
#52789=CARTESIAN_POINT('Ctrl Pts',(-0.199999999999999,-1.73916265124264,
-0.374667649089508));
#52790=CARTESIAN_POINT('Ctrl Pts',(-0.200000000000003,-1.73553328373527,
-0.385837013750726));
#52791=CARTESIAN_POINT('Ctrl Pts',(-0.200000000000003,-1.73179339095667,
-0.39695567446876));
#52792=CARTESIAN_POINT('Ctrl Pts',(-0.200000000000004,-1.71101919172734,
-0.458717143739095));
#52793=CARTESIAN_POINT('Ctrl Pts',(-0.200000000000014,-1.6868039610115,
-0.519028807441265));
#52794=CARTESIAN_POINT('Ctrl Pts',(-0.20000000000001,-1.65909894074285,
-0.577585106880837));
#52795=CARTESIAN_POINT('Ctrl Pts',(-0.200000000000009,-1.65117900452078,
-0.594324389237043));
#52796=CARTESIAN_POINT('Ctrl Pts',(-0.200000000000001,-1.64297360684206,
-0.610920057491285));
#52797=CARTESIAN_POINT('Ctrl Pts',(-0.2,-1.63448095046,-0.62736452868523));
#52798=CARTESIAN_POINT('Ctrl Pts',(-0.199999999999999,-1.60296311633544,
-0.688393032846946));
#52799=CARTESIAN_POINT('Ctrl Pts',(-0.200000000000001,-1.56749183029575,
-0.74734272741049));
#52800=CARTESIAN_POINT('Ctrl Pts',(-0.2,-1.5283794937604,-0.803982051774627));
#52801=CARTESIAN_POINT('Ctrl Pts',(-0.2,-1.49327907548277,-0.854811640396796));
#52802=CARTESIAN_POINT('Ctrl Pts',(-0.199999999999996,-1.45524503473326,
-0.903780293871229));
#52803=CARTESIAN_POINT('Ctrl Pts',(-0.199999999999995,-1.41448352477257,
-0.950684824964385));
#52804=CARTESIAN_POINT('Ctrl Pts',(-0.199999999999995,-1.40761144044724,
-0.958592576498201));
#52805=CARTESIAN_POINT('Ctrl Pts',(-0.199999999999988,-1.40066422860217,
-0.966438706603342));
#52806=CARTESIAN_POINT('Ctrl Pts',(-0.199999999999989,-1.39364858464507,
-0.974216310602531));
#52807=CARTESIAN_POINT('Ctrl Pts',(-0.199999999999992,-1.35023790133332,
-1.0223417722419));
#52808=CARTESIAN_POINT('Ctrl Pts',(-0.199999999999999,-1.30414795222187,
-1.06791839072618));
#52809=CARTESIAN_POINT('Ctrl Pts',(-0.199999999999998,-1.25565993752712,
-1.11077072511639));
#52810=CARTESIAN_POINT('Ctrl Pts',(-0.199999999999997,-1.20735062750674,
-1.15346512537564));
#52811=CARTESIAN_POINT('Ctrl Pts',(-0.199999999999999,-1.15665986722067,
-1.19345575039044));
#52812=CARTESIAN_POINT('Ctrl Pts',(-0.199999999999997,-1.1038422938188,
-1.23052351620657));
#52813=CARTESIAN_POINT('Ctrl Pts',(-0.199999999999995,-1.05209684405534,
-1.26683885767989));
#52814=CARTESIAN_POINT('Ctrl Pts',(-0.199999999999999,-0.998309111883527,
-1.30034906703051));
#52815=CARTESIAN_POINT('Ctrl Pts',(-0.199999999999999,-0.9427105013579,
-1.33079909790533));
#52816=CARTESIAN_POINT('Ctrl Pts',(-0.199999999999999,-0.932046150008153,
-1.33663970839523));
#52817=CARTESIAN_POINT('Ctrl Pts',(-0.199999999999994,-0.921315174052189,
-1.34236757763251));
#52818=CARTESIAN_POINT('Ctrl Pts',(-0.199999999999994,-0.91051921515542,
-1.34798068133527));
#52819=CARTESIAN_POINT('Ctrl Pts',(-0.199999999999994,-0.901279475695472,
-1.35278466551778));
#52820=CARTESIAN_POINT('Ctrl Pts',(-0.199999999999999,-0.891995974411387,
-1.35750253557107));
#52821=CARTESIAN_POINT('Ctrl Pts',(-0.199999999999998,-0.882676839298332,
-1.36212988869321));
#52822=CARTESIAN_POINT('Ctrl Pts',(-0.199999999999997,-0.827091003392099,
-1.3897306572417));
#52823=CARTESIAN_POINT('Ctrl Pts',(-0.199999999999994,-0.770163374407926,
-1.41415423536456));
#52824=CARTESIAN_POINT('Ctrl Pts',(-0.199999999999995,-0.712128380617553,
-1.43521182130048));
#52825=CARTESIAN_POINT('Ctrl Pts',(-0.199999999999996,-0.65513448315741,
-1.45589165281601));
#52826=CARTESIAN_POINT('Ctrl Pts',(-0.199999999999996,-0.59707173077213,
-1.47332538287411));
#52827=CARTESIAN_POINT('Ctrl Pts',(-0.199999999999998,-0.538158279106556,
-1.48728460270676));
#52828=CARTESIAN_POINT('Ctrl Pts',(-0.200000000000001,-0.481127237836991,
-1.5007977957019));
#52829=CARTESIAN_POINT('Ctrl Pts',(-0.200000000000002,-0.42329831589911,
-1.51105499616133));
#52830=CARTESIAN_POINT('Ctrl Pts',(-0.200000000000004,-0.36487685774904,
-1.5178005978696));
#52831=CARTESIAN_POINT('Ctrl Pts',(-0.200000000000005,-0.34982964427313,
-1.51953801614265));
#52832=CARTESIAN_POINT('Ctrl Pts',(-0.199999999999997,-0.33474319067558,
-1.52104222117722));
#52833=CARTESIAN_POINT('Ctrl Pts',(-0.199999999999998,-0.319621170202251,
-1.52230829911636));
#52834=CARTESIAN_POINT('Ctrl Pts',(-29.8760740822721,-0.685825729128414,
1.3961458803669));
#52835=CARTESIAN_POINT('Ctrl Pts',(-29.8390253006463,-1.15011276588657,
1.16807516083303));
#52836=CARTESIAN_POINT('Ctrl Pts',(-29.7649277373946,-1.82525787394022,
0.216325049098126));
#52837=CARTESIAN_POINT('Ctrl Pts',(-29.6537813925172,-1.17030516464274,
-1.4195844951461));
#52838=CARTESIAN_POINT('Ctrl Pts',(-29.5426350476398,0.557509249428845,
-1.75143349164469));
#52839=CARTESIAN_POINT('Ctrl Pts',(-29.4314887027624,1.77417745764817,-0.482217988040945));
#52840=CARTESIAN_POINT('Ctrl Pts',(-29.320342357885,1.36710299288539,1.22961697865478));
#52841=CARTESIAN_POINT('Ctrl Pts',(-29.2091960130075,-0.291685088526501,
1.81519477428025));
#52842=CARTESIAN_POINT('Ctrl Pts',(-29.0980496681302,-1.68334061031966,
0.739397471666864));
#52843=CARTESIAN_POINT('Ctrl Pts',(-28.9869033232526,-1.534059973681,-1.01344370290772));
#52844=CARTESIAN_POINT('Ctrl Pts',(-28.8757569783753,0.0195899148733162,
-1.83844939731259));
#52845=CARTESIAN_POINT('Ctrl Pts',(-28.7646106334978,1.55529006052317,-0.980514255533821));
#52846=CARTESIAN_POINT('Ctrl Pts',(-28.6534642886204,1.6672258610176,0.775046535726967));
#52847=CARTESIAN_POINT('Ctrl Pts',(-28.542317943743,0.252913801877688,1.82108657460817));
#52848=CARTESIAN_POINT('Ctrl Pts',(-28.4311715988656,-1.39292299951968,
1.20004005839424));
#52849=CARTESIAN_POINT('Ctrl Pts',(-28.3200252539881,-1.76362521504133,
-0.519573359220225));
#52850=CARTESIAN_POINT('Ctrl Pts',(-28.2088789091108,-0.519835724455463,
-1.76354724094302));
#52851=CARTESIAN_POINT('Ctrl Pts',(-28.0977325642333,1.19983124114152,-1.39310245061395));
#52852=CARTESIAN_POINT('Ctrl Pts',(-27.9865862193559,1.82112625016851,0.252642976453954));
#52853=CARTESIAN_POINT('Ctrl Pts',(-27.8754398744784,0.775291433296788,
1.66710893100567));
#52854=CARTESIAN_POINT('Ctrl Pts',(-27.764293529601,-0.980275235800491,
1.55543873831543));
#52855=CARTESIAN_POINT('Ctrl Pts',(-27.6531471847236,-1.83845989126956,
0.019859410984222));
#52856=CARTESIAN_POINT('Ctrl Pts',(-27.5420008398462,-1.01364691392612,
-1.53389995281355));
#52857=CARTESIAN_POINT('Ctrl Pts',(-27.4308544949688,0.739097826986148,
-1.68346772023046));
#52858=CARTESIAN_POINT('Ctrl Pts',(-27.3197081500913,1.81524370282257,-0.291923713345362));
#52859=CARTESIAN_POINT('Ctrl Pts',(-27.2085618052139,1.22964495869491,1.36685859779542));
#52860=CARTESIAN_POINT('Ctrl Pts',(-27.0974154603365,-0.48161855815431,
1.77436544145867));
#52861=CARTESIAN_POINT('Ctrl Pts',(-26.9862691154591,-1.75198973384851,
0.557549214370556));
#52862=CARTESIAN_POINT('Ctrl Pts',(-26.8751227705816,-1.4185214322724,-1.16966922661718));
#52863=CARTESIAN_POINT('Ctrl Pts',(-26.7639764257042,0.213516505753145,
-1.82612700980389));
#52864=CARTESIAN_POINT('Ctrl Pts',(-26.6528300808268,1.65009313818133,-0.810877172722089));
#52865=CARTESIAN_POINT('Ctrl Pts',(-26.5416837359494,1.5761103965168,0.946681135265884));
#52866=CARTESIAN_POINT('Ctrl Pts',(-26.4305373910719,0.0592949571880597,
1.83761074823246));
#52867=CARTESIAN_POINT('Ctrl Pts',(-26.3193910461945,-1.51180138990354,
1.04632008076494));
#52868=CARTESIAN_POINT('Ctrl Pts',(-26.2082447013171,-1.69893600272116,
-0.702812644011505));
#52869=CARTESIAN_POINT('Ctrl Pts',(-26.0970983564397,-0.330798585473345,
-1.80856336626222));
#52870=CARTESIAN_POINT('Ctrl Pts',(-25.9859520115622,1.340164710296,-1.25868491021684));
#52871=CARTESIAN_POINT('Ctrl Pts',(-25.8748056666848,1.78428915735557,0.443442619595842));
#52872=CARTESIAN_POINT('Ctrl Pts',(-25.7636593218074,0.595005980146546,
1.7396255452028));
#52873=CARTESIAN_POINT('Ctrl Pts',(-25.65251297693,-1.13896879060324,1.44328765253607));
#52874=CARTESIAN_POINT('Ctrl Pts',(-25.5413666320525,-1.83028727511895,
-0.174291837069515));
#52875=CARTESIAN_POINT('Ctrl Pts',(-25.4302202871752,-0.846089671080599,
-1.63231780680796));
#52876=CARTESIAN_POINT('Ctrl Pts',(-25.3190739422977,0.912651293186798,
-1.59605663150652));
#52877=CARTESIAN_POINT('Ctrl Pts',(-25.2079275974203,1.83591580205738,-0.0987031999860136));
#52878=CARTESIAN_POINT('Ctrl Pts',(-25.0967812525428,1.07851165011462,1.48900697597377));
#52879=CARTESIAN_POINT('Ctrl Pts',(-24.9856349076655,-0.666203972560349,
1.7136223098677));
#52880=CARTESIAN_POINT('Ctrl Pts',(-24.874488562788,-1.80105059299849,0.369521197485718));
#52881=CARTESIAN_POINT('Ctrl Pts',(-24.7633422179106,-1.2871455197044,-1.31285397704253));
#52882=CARTESIAN_POINT('Ctrl Pts',(-24.6521958730331,0.405062575138557,
-1.79339160925706));
#52883=CARTESIAN_POINT('Ctrl Pts',(-24.5410495281557,1.72646064975028,-0.632188879050662));
#52884=CARTESIAN_POINT('Ctrl Pts',(-24.4299031832783,1.46738956291618,1.10774411511692));
#52885=CARTESIAN_POINT('Ctrl Pts',(-24.3187568384009,-0.134986946113292,
1.83360510424424));
#52886=CARTESIAN_POINT('Ctrl Pts',(-24.2076104935235,-1.61379115967188,
0.88091273511989));
#52887=CARTESIAN_POINT('Ctrl Pts',(-24.0964641486461,-1.61526824084304,
-0.878201380126073));
#52888=CARTESIAN_POINT('Ctrl Pts',(-23.9853178037686,-0.138066012129827,
-1.83337582896308));
#52889=CARTESIAN_POINT('Ctrl Pts',(-23.8741714588912,1.46552720872477,-1.11020680704943));
#52890=CARTESIAN_POINT('Ctrl Pts',(-23.7630251140138,1.7275198787737,0.629288663788884));
#52891=CARTESIAN_POINT('Ctrl Pts',(-23.6518787691364,0.408073727971786,
1.79270884040625));
#52892=CARTESIAN_POINT('Ctrl Pts',(-23.5407324242589,-1.28493896936505,
1.31501368773811));
#52893=CARTESIAN_POINT('Ctrl Pts',(-23.4295860793815,-1.8016686070705,-0.366496090331334));
#52894=CARTESIAN_POINT('Ctrl Pts',(-23.3184397345041,-0.669080796948889,
-1.71250110688599));
#52895=CARTESIAN_POINT('Ctrl Pts',(-23.2072933896267,1.07600957223555,-1.49081606993921));
#52896=CARTESIAN_POINT('Ctrl Pts',(-23.0961470447492,1.83607896999803,0.0956199239828239));
#52897=CARTESIAN_POINT('Ctrl Pts',(-22.9850006998718,0.91533033667428,1.59452172412145));
#52898=CARTESIAN_POINT('Ctrl Pts',(-22.8738543549944,-0.843347252550528,
1.633736381901));
#52899=CARTESIAN_POINT('Ctrl Pts',(-22.7627080101169,-1.82999199802708,
0.177365275881016));
#52900=CARTESIAN_POINT('Ctrl Pts',(-22.6515616652396,-1.14139096307257,
-1.44137289531467));
#52901=CARTESIAN_POINT('Ctrl Pts',(-22.5404153203621,0.592083708909288,
-1.74062231273063));
#52902=CARTESIAN_POINT('Ctrl Pts',(-22.4292689754847,1.78354194798782,-0.446438432148635));
#52903=CARTESIAN_POINT('Ctrl Pts',(-22.3181226306072,1.34227658728578,1.25643253585536));
#52904=CARTESIAN_POINT('Ctrl Pts',(-22.2069762857299,-0.327760916379816,
1.80911634109733));
#52905=CARTESIAN_POINT('Ctrl Pts',(-22.0958299408524,-1.69775334184427,
0.705664753397891));
#52906=CARTESIAN_POINT('Ctrl Pts',(-21.984683595975,-1.51355639095973,-1.04377976858935));
#52907=CARTESIAN_POINT('Ctrl Pts',(-21.8735372510976,0.056208890351046,
-1.83770773372074));
#52908=CARTESIAN_POINT('Ctrl Pts',(-21.7623909062202,1.57451836940432,-0.949326634167536));
#52909=CARTESIAN_POINT('Ctrl Pts',(-21.6512445613427,1.65145255424892,0.808104952958591));
#52910=CARTESIAN_POINT('Ctrl Pts',(-21.5400982164653,0.216582902754202,
1.82576586674362));
#52911=CARTESIAN_POINT('Ctrl Pts',(-21.4289518715879,-1.41655515338036,
1.17204976488333));
#52912=CARTESIAN_POINT('Ctrl Pts',(-21.3178055267105,-1.75292358101011,
-0.554606232448005));
#52913=CARTESIAN_POINT('Ctrl Pts',(-21.206659181833,-0.484597651685728,
-1.77355413503851));
#52914=CARTESIAN_POINT('Ctrl Pts',(-21.0955128369556,1.2273477973243,-1.36892166990471));
#52915=CARTESIAN_POINT('Ctrl Pts',(-20.9843664920782,1.81573138332858,0.288874882132692));
#52916=CARTESIAN_POINT('Ctrl Pts',(-20.8732201472008,0.741923909701551,
1.68222414265896));
#52917=CARTESIAN_POINT('Ctrl Pts',(-20.7620738023233,-1.01106953876495,
1.53560005916682));
#52918=CARTESIAN_POINT('Ctrl Pts',(-20.6509274574459,-1.83849064573244,
-0.0167719851482926));
#52919=CARTESIAN_POINT('Ctrl Pts',(-20.5397811125685,-0.982885979939318,
-1.55379030257311));
#52920=CARTESIAN_POINT('Ctrl Pts',(-20.4286347676911,0.772490702514734,
-1.66840860356802));
#52921=CARTESIAN_POINT('Ctrl Pts',(-20.3174884228136,1.82069938029707,-0.255700841839434));
#52922=CARTESIAN_POINT('Ctrl Pts',(-20.2063420779362,1.20216910098862,1.3910854059186));
#52923=CARTESIAN_POINT('Ctrl Pts',(-20.0951957330588,-0.516873484366524,
1.76441802164065));
#52924=CARTESIAN_POINT('Ctrl Pts',(-19.9840493881814,-1.7627499987032,0.52253382283197));
#52925=CARTESIAN_POINT('Ctrl Pts',(-19.872903043304,-1.39493667151811,-1.1976981407623));
#52926=CARTESIAN_POINT('Ctrl Pts',(-19.7617566984265,0.249855885875982,
-1.82151068902289));
#52927=CARTESIAN_POINT('Ctrl Pts',(-19.6506103535491,1.66592065703884,-0.777841576661194));
#52928=CARTESIAN_POINT('Ctrl Pts',(-19.5394640086717,1.55693692840167,0.977893938477322));
#52929=CARTESIAN_POINT('Ctrl Pts',(-19.4283176637942,0.0226726397870904,
1.83842734567798));
#52930=CARTESIAN_POINT('Ctrl Pts',(-19.3171713189168,-1.53234706424761,
1.01599292744745));
#52931=CARTESIAN_POINT('Ctrl Pts',(-19.2060249740394,-1.68459672540546,
-0.736520893583273));
#52932=CARTESIAN_POINT('Ctrl Pts',(-19.094878629162,-0.29470108811063,-1.81479487066663));
#52933=CARTESIAN_POINT('Ctrl Pts',(-18.9837322842846,1.36497537602827,-1.23173510819818));
#52934=CARTESIAN_POINT('Ctrl Pts',(-18.8725859394071,1.77510034401367,0.478902832121552));
#52935=CARTESIAN_POINT('Ctrl Pts',(-18.7614395945297,0.560229484500028,
1.75113451186034));
#52936=CARTESIAN_POINT('Ctrl Pts',(-18.6502932496523,-1.1674972131777,1.42030961806002));
#52937=CARTESIAN_POINT('Ctrl Pts',(-18.5391469047748,-1.82645159810784,
-0.210721887094827));
#52938=CARTESIAN_POINT('Ctrl Pts',(-18.4280005598975,-0.813401222257357,
-1.64885038907772));
#52939=CARTESIAN_POINT('Ctrl Pts',(-18.31685421502,0.94426823764005,-1.57755717782769));
#52940=CARTESIAN_POINT('Ctrl Pts',(-18.2057078701426,1.83751786269281,-0.0621068290635167));
#52941=CARTESIAN_POINT('Ctrl Pts',(-18.0945615252652,1.04863223837752,1.51019852422351));
#52942=CARTESIAN_POINT('Ctrl Pts',(-17.9834151803877,-0.700212082183364,
1.70000946876656));
#52943=CARTESIAN_POINT('Ctrl Pts',(-17.8722688355103,-1.80805505555301,
0.333565690712785));
#52944=CARTESIAN_POINT('Ctrl Pts',(-17.7611224906329,-1.26073417800543,
-1.33823708151452));
#52945=CARTESIAN_POINT('Ctrl Pts',(-17.6499761457555,0.440711752671261,
-1.78496563131869));
#52946=CARTESIAN_POINT('Ctrl Pts',(-17.5388298008781,1.73871302083308,-0.59766728630315));
#52947=CARTESIAN_POINT('Ctrl Pts',(-17.4276834560006,1.44502883098667,1.1367589153153));
#52948=CARTESIAN_POINT('Ctrl Pts',(-17.3165371111232,-0.171490898207203,
1.83055183640442));
#52949=CARTESIAN_POINT('Ctrl Pts',(-17.2053907662458,-1.63102119580044,
0.848586479258995));
#52950=CARTESIAN_POINT('Ctrl Pts',(-17.0942444213684,-1.5974513164508,-0.91020791333691));
#52951=CARTESIAN_POINT('Ctrl Pts',(-16.9830980764909,-0.101512432092709,
-1.83576261538962));
#52952=CARTESIAN_POINT('Ctrl Pts',(-16.8719517316135,1.48735487692949,-1.08078888965679));
#52953=CARTESIAN_POINT('Ctrl Pts',(-16.7608053867361,1.71463973954429,0.663580980368641));
#52954=CARTESIAN_POINT('Ctrl Pts',(-16.6496590418587,0.372276761224383,
1.80048303712748));
#52955=CARTESIAN_POINT('Ctrl Pts',(-16.5385126969812,-1.31088282935724,
1.28915296285113));
#52956=CARTESIAN_POINT('Ctrl Pts',(-16.4273663521038,-1.79400934280639,
-0.402317824431001));
#52957=CARTESIAN_POINT('Ctrl Pts',(-16.3162200072264,-0.634829996541143,
-1.72549124292854));
#52958=CARTESIAN_POINT('Ctrl Pts',(-16.205073662349,1.10549739525827,-1.46908293265175));
#52959=CARTESIAN_POINT('Ctrl Pts',(-16.0939273174715,1.83380951667369,0.132180976273241));
#52960=CARTESIAN_POINT('Ctrl Pts',(-15.9827809725941,0.883381152756941,
1.61244128354657));
#52961=CARTESIAN_POINT('Ctrl Pts',(-15.8716346277167,-0.875728642698206,
1.61661018748783));
#52962=CARTESIAN_POINT('Ctrl Pts',(-15.7604882828393,-1.83316241166559,
0.140871311443935));
#52963=CARTESIAN_POINT('Ctrl Pts',(-15.6493419379619,-1.11244808036887,
-1.46382663673507));
#52964=CARTESIAN_POINT('Ctrl Pts',(-15.5381955930844,0.626644448535124,
-1.72848080378452));
#52965=CARTESIAN_POINT('Ctrl Pts',(-15.427049248207,1.79208230060405,-0.410816481890913));
#52966=CARTESIAN_POINT('Ctrl Pts',(-15.3159029033296,1.31697838226697,1.28292521004654));
#52967=CARTESIAN_POINT('Ctrl Pts',(-15.2047565584522,-0.363738719182501,
1.80222731587859));
#52968=CARTESIAN_POINT('Ctrl Pts',(-15.0936102135747,-1.71147526380616,
0.671700510131698));
#52969=CARTESIAN_POINT('Ctrl Pts',(-14.9824638686973,-1.49246085154338,
-1.0737270419161));
#52970=CARTESIAN_POINT('Ctrl Pts',(-14.8713175238199,0.0928102146840508,
-1.83622313948545));
#52971=CARTESIAN_POINT('Ctrl Pts',(-14.7601711789425,1.59311920419314,-0.917769227618005));
#52972=CARTESIAN_POINT('Ctrl Pts',(-14.649024834065,1.63502497258126,0.840846295684967));
#52973=CARTESIAN_POINT('Ctrl Pts',(-14.5378784891876,0.180165351192192,
1.82971844833059));
#52974=CARTESIAN_POINT('Ctrl Pts',(-14.4267321443102,-1.43962463311105,
1.14359523856626));
#52975=CARTESIAN_POINT('Ctrl Pts',(-14.3155857994328,-1.74152629078552,
-0.589419487660784));
#52976=CARTESIAN_POINT('Ctrl Pts',(-14.2044394545554,-0.449167113826005,
-1.78285671263529));
#52977=CARTESIAN_POINT('Ctrl Pts',(-14.0932931096779,1.25437709178756,-1.34419762889618));
#52978=CARTESIAN_POINT('Ctrl Pts',(-13.9821467648005,1.80961576800425,0.324992193939892));
#52979=CARTESIAN_POINT('Ctrl Pts',(-13.8710004199231,0.708261856483432,
1.69667153467668));
#52980=CARTESIAN_POINT('Ctrl Pts',(-13.7598540750457,-1.04146247840172,
1.51515182737997));
#52981=CARTESIAN_POINT('Ctrl Pts',(-13.6487077301683,-1.83779159390846,
-0.0533967348337232));
#52982=CARTESIAN_POINT('Ctrl Pts',(-13.5375613852908,-0.951734875856344,
-1.57306385121844));
#52983=CARTESIAN_POINT('Ctrl Pts',(-13.4264150404134,0.805576927784317,
-1.65268719585804));
#52984=CARTESIAN_POINT('Ctrl Pts',(-13.315268695536,1.82543231055633,-0.219376465256566));
#52985=CARTESIAN_POINT('Ctrl Pts',(-13.2041223506585,1.1742160279774,1.41476000564494));
#52986=CARTESIAN_POINT('Ctrl Pts',(-13.0929760057811,-0.55192323148034,
1.75377019603021));
#52987=CARTESIAN_POINT('Ctrl Pts',(-12.9818296609037,-1.77281051953266,
0.487311005176181));
#52988=CARTESIAN_POINT('Ctrl Pts',(-12.8706833160263,-1.37079817438837,
-1.22525161457759));
#52989=CARTESIAN_POINT('Ctrl Pts',(-12.7595369711488,0.286096082776584,
-1.81617129846043));
#52990=CARTESIAN_POINT('Ctrl Pts',(-12.6483906262714,1.6810868693329,-0.74449720730706));
#52991=CARTESIAN_POINT('Ctrl Pts',(-12.537244281394,1.53714541606292,1.00871855530086));
#52992=CARTESIAN_POINT('Ctrl Pts',(-12.4260979365166,-0.0139586777784811,
1.83851415802169));
#52993=CARTESIAN_POINT('Ctrl Pts',(-12.3149515916392,-1.55228445560866,
0.985262463918737));
#52994=CARTESIAN_POINT('Ctrl Pts',(-12.2038052467617,-1.66958872783078,
-0.769936772619606));
#52995=CARTESIAN_POINT('Ctrl Pts',(-12.0926589018843,-0.258486605724834,
-1.82030597114671));
#52996=CARTESIAN_POINT('Ctrl Pts',(-11.9815125570069,1.38924419891378,-1.20429635460542));
#52997=CARTESIAN_POINT('Ctrl Pts',(-11.8703662121295,1.76520688394983,0.514172938599101));
#52998=CARTESIAN_POINT('Ctrl Pts',(-11.759219867252,0.525230599245605,1.76194834531198));
#52999=CARTESIAN_POINT('Ctrl Pts',(-11.6480735223746,-1.19556218415814,
1.39676777516613));
#53000=CARTESIAN_POINT('Ctrl Pts',(-11.5369271774972,-1.82189088989749,
-0.247068288616763));
#53001=CARTESIAN_POINT('Ctrl Pts',(-11.4257808326198,-0.780389884361033,
-1.66472844101327));
#53002=CARTESIAN_POINT('Ctrl Pts',(-11.3146344877423,0.975510343836714,
-1.55843149448383));
#53003=CARTESIAN_POINT('Ctrl Pts',(-11.2034881428649,1.83839049924661,-0.0254858041131052));
#53004=CARTESIAN_POINT('Ctrl Pts',(-11.0923417979875,1.01833655988029,1.53079058160895));
#53005=CARTESIAN_POINT('Ctrl Pts',(-10.9811954531101,-0.733942234478493,
1.68572178913967));
#53006=CARTESIAN_POINT('Ctrl Pts',(-10.8700491082326,-1.81434178962977,
0.297477771160369));
#53007=CARTESIAN_POINT('Ctrl Pts',(-10.7589027633552,-1.23382237321512,
-1.3630889572164));
#53008=CARTESIAN_POINT('Ctrl Pts',(-10.6477564184778,0.476185984549256,
-1.77583109051801));
#53009=CARTESIAN_POINT('Ctrl Pts',(-10.5366100736004,1.7502751895651,-0.562908442576898));
#53010=CARTESIAN_POINT('Ctrl Pts',(-10.4254637287229,1.4220944780604,1.16532246584438));
#53011=CARTESIAN_POINT('Ctrl Pts',(-10.3143173838456,-0.207926774994991,
1.82677190972811));
#53012=CARTESIAN_POINT('Ctrl Pts',(-10.2031710389681,-1.64760377910037,
0.815923367128113));
#53013=CARTESIAN_POINT('Ctrl Pts',(-10.0920246940907,-1.57900026518387,
-0.941853128932933));
#53014=CARTESIAN_POINT('Ctrl Pts',(-9.98087834921326,-0.0649185555153559,
-1.83742067450035));
#53015=CARTESIAN_POINT('Ctrl Pts',(-9.86973200433583,1.50859212232134,-1.05094194054737));
#53016=CARTESIAN_POINT('Ctrl Pts',(-9.75858565945843,1.70107895413302,0.697609880762318));
#53017=CARTESIAN_POINT('Ctrl Pts',(-9.64743931458098,0.33633201488792,1.80754251117172));
#53018=CARTESIAN_POINT('Ctrl Pts',(-9.53629296970358,-1.33630631916782,
1.26278049370572));
#53019=CARTESIAN_POINT('Ctrl Pts',(-9.42514662482614,-1.78563792567352,
-0.437979853792231));
#53020=CARTESIAN_POINT('Ctrl Pts',(-9.31400027994872,-0.600327192984703,
-1.73779642515878));
#53021=CARTESIAN_POINT('Ctrl Pts',(-9.20285393507129,1.13454637823559,-1.44676662581219));
#53022=CARTESIAN_POINT('Ctrl Pts',(-9.09170759019388,1.83081211133877,0.168689557788168));
#53023=CARTESIAN_POINT('Ctrl Pts',(-8.98056124531644,0.851081300419372,
1.62972076565527));
#53024=CARTESIAN_POINT('Ctrl Pts',(-8.86941490043904,-0.907762402178502,
1.59884226086334));
#53025=CARTESIAN_POINT('Ctrl Pts',(-8.7582685555616,-1.83560513016937,0.104321426501776));
#53026=CARTESIAN_POINT('Ctrl Pts',(-8.64712221068418,-1.08306359846452,
-1.48569929515115));
#53027=CARTESIAN_POINT('Ctrl Pts',(-8.53597586580675,0.660956434360724,
-1.71565315428517));
#53028=CARTESIAN_POINT('Ctrl Pts',(-8.42482952092933,1.79991126531332,-0.375031453253858));
#53029=CARTESIAN_POINT('Ctrl Pts',(-8.31368317605192,1.29115738736595,1.30890861215818));
#53030=CARTESIAN_POINT('Ctrl Pts',(-8.20253683117448,-0.399572131671196,
1.79462287557114));
#53031=CARTESIAN_POINT('Ctrl Pts',(-8.09139048629707,-1.7245177957616,0.637469627537685));
#53032=CARTESIAN_POINT('Ctrl Pts',(-7.98024414141963,-1.47077286243819,
-1.10324808680863));
#53033=CARTESIAN_POINT('Ctrl Pts',(-7.86909779654222,0.12937469692319,-1.83400963512396));
#53034=CARTESIAN_POINT('Ctrl Pts',(-7.75795145166479,1.61108763178959,-0.885847501902045));
#53035=CARTESIAN_POINT('Ctrl Pts',(-7.64680510678736,1.61794834873923,0.873253854697203));
#53036=CARTESIAN_POINT('Ctrl Pts',(-7.53565876190995,0.143676280899092,
1.83294470190416));
#53037=CARTESIAN_POINT('Ctrl Pts',(-7.42451241703252,-1.46212263710416,
1.11468674882187));
#53038=CARTESIAN_POINT('Ctrl Pts',(-7.3133660721551,-1.72943768144993,-0.623998765954385));
#53039=CARTESIAN_POINT('Ctrl Pts',(-7.20221972727767,-0.413558273857659,
-1.79145156452956));
#53040=CARTESIAN_POINT('Ctrl Pts',(-7.09107338240025,1.28090844667878,-1.31893999300895));
#53041=CARTESIAN_POINT('Ctrl Pts',(-6.97992703752282,1.80278180465922,0.360980496316825));
#53042=CARTESIAN_POINT('Ctrl Pts',(-6.8687806926454,0.674318650485929,1.71044541320042));
#53043=CARTESIAN_POINT('Ctrl Pts',(-6.75763434776798,-1.07144199739794,
1.49410213845754));
#53044=CARTESIAN_POINT('Ctrl Pts',(-6.64648800289056,-1.83636300934206,
-0.0900002880644057));
#53045=CARTESIAN_POINT('Ctrl Pts',(-6.53534165801313,-0.920205969547918,
-1.59171295387702));
#53046=CARTESIAN_POINT('Ctrl Pts',(-6.42419531313571,0.838343369925463,
-1.63630973474875));
#53047=CARTESIAN_POINT('Ctrl Pts',(-6.31304896825829,1.82944061423442,-0.182965004634956));
#53048=CARTESIAN_POINT('Ctrl Pts',(-6.20190262338086,1.14579683626047,1.43787299993672));
#53049=CARTESIAN_POINT('Ctrl Pts',(-6.09075627850344,-0.586753886249875,
1.74242619094817));
#53050=CARTESIAN_POINT('Ctrl Pts',(-5.97960993362602,-1.78216730261277,
0.451894743750581));
#53051=CARTESIAN_POINT('Ctrl Pts',(-5.86846358874859,-1.34611552298411,
-1.25231871051771));
#53052=CARTESIAN_POINT('Ctrl Pts',(-5.75731724387117,0.322222710510533,
-1.81011095758319));
#53053=CARTESIAN_POINT('Ctrl Pts',(-5.64617089899375,1.69558575464707,-0.710857301129708));
#53054=CARTESIAN_POINT('Ctrl Pts',(-5.53502455411632,1.51674371597785,1.03914274956487));
#53055=CARTESIAN_POINT('Ctrl Pts',(-5.4238782092389,-0.0505844542846405,
1.83787115079273));
#53056=CARTESIAN_POINT('Ctrl Pts',(-5.31273186436147,-1.57160564960563,
0.954140888998658));
#53057=CARTESIAN_POINT('Ctrl Pts',(-5.20158551948405,-1.65391796759717,
-0.803047016301529));
#53058=CARTESIAN_POINT('Ctrl Pts',(-5.09043917460663,-0.22216951407526,
-1.82509448000564));
#53059=CARTESIAN_POINT('Ctrl Pts',(-4.9792928297292,1.4129615451609,-1.17637954157153));
#53060=CARTESIAN_POINT('Ctrl Pts',(-4.86814648485178,1.75461270448817,0.549238938150095));
#53061=CARTESIAN_POINT('Ctrl Pts',(-4.75700013997435,0.490023217597568,
1.7720627528806));
#53062=CARTESIAN_POINT('Ctrl Pts',(-4.64585379509693,-1.22315256282799,
1.37267146906276));
#53063=CARTESIAN_POINT('Ctrl Pts',(-4.53470745021951,-1.81660696091404,
-0.28331661350876));
#53064=CARTESIAN_POINT('Ctrl Pts',(-4.42356110534208,-0.747068761626052,
-1.67994565963717));
#53065=CARTESIAN_POINT('Ctrl Pts',(-4.31241476046467,1.00636520985961,-1.53868717363749));
#53066=CARTESIAN_POINT('Ctrl Pts',(-4.20126841558724,1.83853336531533,0.0111453377239352));
#53067=CARTESIAN_POINT('Ctrl Pts',(-4.09012207070981,0.987636640845155,
1.55077497387288));
#53068=CARTESIAN_POINT('Ctrl Pts',(-3.9789757258324,-0.767381039870437,
1.6707649426488));
#53069=CARTESIAN_POINT('Ctrl Pts',(-3.86782938095496,-1.81990829963504,
0.26127176434536));
#53070=CARTESIAN_POINT('Ctrl Pts',(-3.75668303607755,-1.20642078829025,
-1.38739973890271));
#53071=CARTESIAN_POINT('Ctrl Pts',(-3.64553669120012,0.511471188869394,
-1.7659916129257));
#53072=CARTESIAN_POINT('Ctrl Pts',(-3.5343903463227,1.76114256619831,-0.527926145782834));
#53073=CARTESIAN_POINT('Ctrl Pts',(-3.42324400144528,1.3985956082158,1.19342342803983));
#53074=CARTESIAN_POINT('Ctrl Pts',(-3.31209765656785,-0.244280112870538,
1.82226682475983));
#53075=CARTESIAN_POINT('Ctrl Pts',(-3.20095131169043,-1.66353232684867,
0.782936364617715));
#53076=CARTESIAN_POINT('Ctrl Pts',(-3.089804966813,-1.55992241154186,-0.973124464765563));
#53077=CARTESIAN_POINT('Ctrl Pts',(-2.97865862193558,-0.0282989084957232,
-1.83834934851334));
#53078=CARTESIAN_POINT('Ctrl Pts',(-2.86751227705816,1.52923051402139,-1.02067780704635));
#53079=CARTESIAN_POINT('Ctrl Pts',(-2.75636593218073,1.6868429066166,0.731361855340862));
#53080=CARTESIAN_POINT('Ctrl Pts',(-2.64521958730331,0.300253755811285,
1.81388446297849));
#53081=CARTESIAN_POINT('Ctrl Pts',(-2.53407324242589,-1.36119934315438,
1.23590674387245));
#53082=CARTESIAN_POINT('Ctrl Pts',(-2.42292689754847,-1.77655768544653,
-0.473468011899886));
#53083=CARTESIAN_POINT('Ctrl Pts',(-2.31178055267104,-0.565586069932105,
-1.74941178802327));
#53084=CARTESIAN_POINT('Ctrl Pts',(-2.20063420779361,1.16314496579956,-1.42387597174662));
#53085=CARTESIAN_POINT('Ctrl Pts',(-2.08948786291619,1.82708798956902,0.205131106799974));
#53086=CARTESIAN_POINT('Ctrl Pts',(-1.97834151803877,0.818443514495715,
1.64635344282621));
#53087=CARTESIAN_POINT('Ctrl Pts',(-1.86719517316135,-0.939435649392642,
1.58043940475681));
#53088=CARTESIAN_POINT('Ctrl Pts',(-1.75604882828392,-1.83731949853668,
0.067730606360174));
#53089=CARTESIAN_POINT('Ctrl Pts',(-1.6449024834065,-1.05324858333434,-1.50698309414738));
#53090=CARTESIAN_POINT('Ctrl Pts',(-1.53375613852907,0.695004907338835,
-1.70214273260888));
#53091=CARTESIAN_POINT('Ctrl Pts',(-1.42260979365165,1.80702789992282,-0.339100830268501));
#53092=CARTESIAN_POINT('Ctrl Pts',(-1.31146344877422,1.26481973322455,1.33437866444013));
#53093=CARTESIAN_POINT('Ctrl Pts',(-1.2003171038968,-0.43523909383229,1.78629417578513));
#53094=CARTESIAN_POINT('Ctrl Pts',(-1.08917075901938,-1.73689066467127,
0.603008259306024));
#53095=CARTESIAN_POINT('Ctrl Pts',(-0.978024414141956,-1.44847268249357,
-1.13237410758484));
#53096=CARTESIAN_POINT('Ctrl Pts',(-0.866878069264529,0.165833894051307,
-1.83098644971143));
#53097=CARTESIAN_POINT('Ctrl Pts',(-0.755731724387107,1.62851911260145,
-0.853729469588644));
#53098=CARTESIAN_POINT('Ctrl Pts',(-0.644585379509683,1.60003419765428,
0.9056105153729));
#53099=CARTESIAN_POINT('Ctrl Pts',(-0.533439034632261,0.107502597833407,
1.83487847835014));
#53100=CARTESIAN_POINT('Ctrl Pts',(-0.422292689754837,-1.48475723354389,
1.08643005973131));
#53101=CARTESIAN_POINT('Ctrl Pts',(-0.311146344877411,-1.71522461751901,
-0.660581065959966));
#53102=CARTESIAN_POINT('Ctrl Pts',(-0.237048781625798,-0.82586340403187,
-1.41601857102626));
#53103=CARTESIAN_POINT('Ctrl Pts',(-0.199999999999991,-0.319621170202164,
-1.52230829911638));
#53104=CARTESIAN_POINT('Ctrl Pts',(-29.7993827215147,-0.74439243930905,
1.51537102412048));
#53105=CARTESIAN_POINT('Ctrl Pts',(-29.7623339398889,-1.24832768867796,
1.26782399863261));
#53106=CARTESIAN_POINT('Ctrl Pts',(-29.6882363766373,-1.98112742558818,
0.234798322871887));
#53107=CARTESIAN_POINT('Ctrl Pts',(-29.5770900317599,-1.27024443564024,
-1.54081120066757));
#53108=CARTESIAN_POINT('Ctrl Pts',(-29.4659436868824,0.605118257442928,
-1.90099874320803));
#53109=CARTESIAN_POINT('Ctrl Pts',(-29.354797342005,1.92568495081712,-0.523397430499743));
#53110=CARTESIAN_POINT('Ctrl Pts',(-29.2436509971276,1.48384799292067,1.33462123580558));
#53111=CARTESIAN_POINT('Ctrl Pts',(-29.1325046522502,-0.316593801218701,
1.97020497840553));
#53112=CARTESIAN_POINT('Ctrl Pts',(-29.0213583073727,-1.82709100852228,
0.802538989390837));
#53113=CARTESIAN_POINT('Ctrl Pts',(-28.9102119624953,-1.66506241652075,
-1.09998764710766));
#53114=CARTESIAN_POINT('Ctrl Pts',(-28.7990656176179,0.0212628134219854,
-1.9954454510636));
#53115=CARTESIAN_POINT('Ctrl Pts',(-28.6879192727405,1.68810546588451,-1.06424615970824));
#53116=CARTESIAN_POINT('Ctrl Pts',(-28.5767729278631,1.80960012558748,0.84123233761007));
#53117=CARTESIAN_POINT('Ctrl Pts',(-28.4656265829856,0.274511605380939,
1.97659991436632));
#53118=CARTESIAN_POINT('Ctrl Pts',(-28.3544802381082,-1.51187292244025,
1.30251856761311));
#53119=CARTESIAN_POINT('Ctrl Pts',(-28.2433338932308,-1.91423158988198,
-0.563942797482219));
#53120=CARTESIAN_POINT('Ctrl Pts',(-28.1321875483534,-0.564227567634542,
-1.91414695711486));
#53121=CARTESIAN_POINT('Ctrl Pts',(-28.0210412034759,1.3022919182218,-1.51206769792338));
#53122=CARTESIAN_POINT('Ctrl Pts',(-27.9098948585985,1.9766429780571,0.274217652574654));
#53123=CARTESIAN_POINT('Ctrl Pts',(-27.798748513721,0.841498148429855,1.8094732102312));
#53124=CARTESIAN_POINT('Ctrl Pts',(-27.6876021688437,-1.06398672866812,
1.68826684015161));
#53125=CARTESIAN_POINT('Ctrl Pts',(-27.5764558239662,-1.99545684116154,
0.0215553233975659));
#53126=CARTESIAN_POINT('Ctrl Pts',(-27.4653094790888,-1.10020821151516,
-1.66488873052626));
#53127=CARTESIAN_POINT('Ctrl Pts',(-27.3541631342114,0.802213756280972,
-1.82722897309913));
#53128=CARTESIAN_POINT('Ctrl Pts',(-27.243016789334,1.97025808524513,-0.316852803620255));
#53129=CARTESIAN_POINT('Ctrl Pts',(-27.1318704444566,1.3346516052265,1.48358272749042));
#53130=CARTESIAN_POINT('Ctrl Pts',(-27.0207240995791,-0.522746811754401,
1.92588898767558));
#53131=CARTESIAN_POINT('Ctrl Pts',(-26.9095777547017,-1.90160248621939,
0.605161635226943));
#53132=CARTESIAN_POINT('Ctrl Pts',(-26.7984314098243,-1.53965735657548,
-1.26955419111032));
#53133=CARTESIAN_POINT('Ctrl Pts',(-26.6872850649469,0.231749941420772,
-1.98207078209722));
#53134=CARTESIAN_POINT('Ctrl Pts',(-26.5761387200694,1.79100433834535,-0.880122764349528));
#53135=CARTESIAN_POINT('Ctrl Pts',(-26.464992375192,1.7107037733542,1.02752382944862));
#53136=CARTESIAN_POINT('Ctrl Pts',(-26.3538460303146,0.0643585038373884,
1.99453518478462));
#53137=CARTESIAN_POINT('Ctrl Pts',(-26.2426996854372,-1.64090304079323,
1.13567153307063));
#53138=CARTESIAN_POINT('Ctrl Pts',(-26.1315533405598,-1.84401818360282,
-0.76282996719567));
#53139=CARTESIAN_POINT('Ctrl Pts',(-26.0204069956823,-0.359047430712987,
-1.96300727528516));
#53140=CARTESIAN_POINT('Ctrl Pts',(-25.9092606508049,1.45460929125672,-1.36617144974778));
#53141=CARTESIAN_POINT('Ctrl Pts',(-25.7981143059275,1.93666014829227,0.481310804297285));
#53142=CARTESIAN_POINT('Ctrl Pts',(-25.68696796105,0.645817055489537,1.88818244647001));
#53143=CARTESIAN_POINT('Ctrl Pts',(-25.5758216161726,-1.23623206351777,
1.56653851068145));
#53144=CARTESIAN_POINT('Ctrl Pts',(-25.4646752712952,-1.9865863170422,-0.189175646578258));
#53145=CARTESIAN_POINT('Ctrl Pts',(-25.3535289264178,-0.91834226594298,
-1.77171106642719));
#53146=CARTESIAN_POINT('Ctrl Pts',(-25.2423825815403,0.990587978140239,
-1.73235333517204));
#53147=CARTESIAN_POINT('Ctrl Pts',(-25.1312362366629,1.99269549714361,-0.107132049272218));
#53148=CARTESIAN_POINT('Ctrl Pts',(-25.0200898917855,1.17061213068258,1.61616207721148));
#53149=CARTESIAN_POINT('Ctrl Pts',(-24.9089435469081,-0.723095065041999,
1.85995864126857));
#53150=CARTESIAN_POINT('Ctrl Pts',(-24.7977972020306,-1.95485294193452,
0.401076795299436));
#53151=CARTESIAN_POINT('Ctrl Pts',(-24.6866508571532,-1.39706247879622,
-1.42496633316633));
#53152=CARTESIAN_POINT('Ctrl Pts',(-24.5755045122758,0.439653261132996,
-1.94653991232978));
#53153=CARTESIAN_POINT('Ctrl Pts',(-24.4643581673984,1.87389332282981,-0.686175221770339));
#53154=CARTESIAN_POINT('Ctrl Pts',(-24.353211822521,1.59269862555882,1.20234092854762));
#53155=CARTESIAN_POINT('Ctrl Pts',(-24.2420654776435,-0.146514278809422,
1.9901874751949));
#53156=CARTESIAN_POINT('Ctrl Pts',(-24.1309191327661,-1.75160231945531,
0.956139077120314));
#53157=CARTESIAN_POINT('Ctrl Pts',(-24.0197727878887,-1.75320553731272,
-0.95319618350774));
#53158=CARTESIAN_POINT('Ctrl Pts',(-23.9086264430113,-0.149856284460993,
-1.98993862074318));
#53159=CARTESIAN_POINT('Ctrl Pts',(-23.7974800981338,1.59067723394218,-1.20501392429124));
#53160=CARTESIAN_POINT('Ctrl Pts',(-23.6863337532564,1.87504300567635,0.683027339995933));
#53161=CARTESIAN_POINT('Ctrl Pts',(-23.575187408379,0.442921554093378,1.94579883781372));
#53162=CARTESIAN_POINT('Ctrl Pts',(-23.4640410635016,-1.39466749808941,
1.4273104743155));
#53163=CARTESIAN_POINT('Ctrl Pts',(-23.3528947186241,-1.95552373187871,
-0.397793356375988));
#53164=CARTESIAN_POINT('Ctrl Pts',(-23.2417483737467,-0.726217558458331,
-1.85874169214136));
#53165=CARTESIAN_POINT('Ctrl Pts',(-23.1306020288693,1.16789638559377,-1.61812566039685));
#53166=CARTESIAN_POINT('Ctrl Pts',(-23.0194556839919,1.99287259895853,0.103785474118366));
#53167=CARTESIAN_POINT('Ctrl Pts',(-22.9083093391144,0.993495800976093,
1.73068735297875));
#53168=CARTESIAN_POINT('Ctrl Pts',(-22.797162994237,-0.915365656095304,
1.77325078202687));
#53169=CARTESIAN_POINT('Ctrl Pts',(-22.6860166493596,-1.98626582449528,
0.192511544484518));
#53170=CARTESIAN_POINT('Ctrl Pts',(-22.5748703044822,-1.2388610796019,-1.56446024103054));
#53171=CARTESIAN_POINT('Ctrl Pts',(-22.4637239596048,0.642645234249625,
-1.8892643338649));
#53172=CARTESIAN_POINT('Ctrl Pts',(-22.3525776147273,1.93584913030288,-0.484562446980071));
#53173=CARTESIAN_POINT('Ctrl Pts',(-22.2414312698499,1.45690151389741,1.36372673183492));
#53174=CARTESIAN_POINT('Ctrl Pts',(-22.1302849249725,-0.355750357112206,
1.96360747190783));
#53175=CARTESIAN_POINT('Ctrl Pts',(-22.0191385800951,-1.84273452832774,
0.765925635049822));
#53176=CARTESIAN_POINT('Ctrl Pts',(-21.9079922352176,-1.64280791175631,
-1.13291428863289));
#53177=CARTESIAN_POINT('Ctrl Pts',(-21.7968458903402,0.0610088995239246,
-1.99464045243663));
#53178=CARTESIAN_POINT('Ctrl Pts',(-21.6856995454628,1.70897579364258,-1.03039524312831));
#53179=CARTESIAN_POINT('Ctrl Pts',(-21.5745532005853,1.79247984298095,0.877113808365062));
#53180=CARTESIAN_POINT('Ctrl Pts',(-21.463406855708,0.235078196174796,1.98167879889778));
#53181=CARTESIAN_POINT('Ctrl Pts',(-21.3522605108305,-1.53752316551414,
1.27213801760072));
#53182=CARTESIAN_POINT('Ctrl Pts',(-21.2411141659531,-1.90261608010631,
-0.601967334693983));
#53183=CARTESIAN_POINT('Ctrl Pts',(-21.1299678210757,-0.525980307679819,
-1.92500839900785));
#53184=CARTESIAN_POINT('Ctrl Pts',(-21.0188214761983,1.33215827567724,-1.48582197751358));
#53185=CARTESIAN_POINT('Ctrl Pts',(-20.9076751313208,1.97078741167024,0.313543614701046));
#53186=CARTESIAN_POINT('Ctrl Pts',(-20.7965287864434,0.80528117489297,1.82587919909306));
#53187=CARTESIAN_POINT('Ctrl Pts',(-20.685382441566,-1.09741073906456,1.66673401900348));
#53188=CARTESIAN_POINT('Ctrl Pts',(-20.5742360966886,-1.99549022192967,
-0.0182042440322412));
#53189=CARTESIAN_POINT('Ctrl Pts',(-20.4630897518111,-1.06682041967049,
-1.68647763474402));
#53190=CARTESIAN_POINT('Ctrl Pts',(-20.3519434069337,0.838458246702548,
-1.81088386951074));
#53191=CARTESIAN_POINT('Ctrl Pts',(-20.2407970620563,1.97617965524583,-0.277536647148052));
#53192=CARTESIAN_POINT('Ctrl Pts',(-20.1296507171789,1.30482942173087,1.50987840586691));
#53193=CARTESIAN_POINT('Ctrl Pts',(-20.0185043723015,-0.561012364366608,
1.91509209891992));
#53194=CARTESIAN_POINT('Ctrl Pts',(-19.907358027424,-1.91328163365087,0.567156072569076));
#53195=CARTESIAN_POINT('Ctrl Pts',(-19.7962116825466,-1.51405855378528,
-1.29997665980099));
#53196=CARTESIAN_POINT('Ctrl Pts',(-19.6850653376692,0.271192555868894,
-1.97706024641613));
#53197=CARTESIAN_POINT('Ctrl Pts',(-19.5739189927918,1.80818346253121,-0.844266063599836));
#53198=CARTESIAN_POINT('Ctrl Pts',(-19.4627726479143,1.68989296953911,1.06140207830021));
#53199=CARTESIAN_POINT('Ctrl Pts',(-19.3516263030369,0.0246087904256447,
1.99542151630965));
#53200=CARTESIAN_POINT('Ctrl Pts',(-19.2404799581595,-1.66320323163278,
1.10275456498897));
#53201=CARTESIAN_POINT('Ctrl Pts',(-19.129333613282,-1.82845439069506,-0.79941676331289));
#53202=CARTESIAN_POINT('Ctrl Pts',(-19.0181872684046,-0.319867354822673,
-1.96977092466014));
#53203=CARTESIAN_POINT('Ctrl Pts',(-18.9070409235272,1.48153868629239,-1.33692024494236));
#53204=CARTESIAN_POINT('Ctrl Pts',(-18.7958945786498,1.92668664790082,0.519799173833923));
#53205=CARTESIAN_POINT('Ctrl Pts',(-18.6847482337724,0.60807078945512,1.90067423177386));
#53206=CARTESIAN_POINT('Ctrl Pts',(-18.5736018888949,-1.26719669661316,
1.54159824611032));
#53207=CARTESIAN_POINT('Ctrl Pts',(-18.4624555440175,-1.98242308891378,
-0.228716673767415));
#53208=CARTESIAN_POINT('Ctrl Pts',(-18.3513091991401,-0.882862357384166,
-1.78965546355487));
#53209=CARTESIAN_POINT('Ctrl Pts',(-18.2401628542626,1.02490488024154,-1.71227410386737));
#53210=CARTESIAN_POINT('Ctrl Pts',(-18.1290165093853,1.99443436720007,-0.0674104980620086));
#53211=CARTESIAN_POINT('Ctrl Pts',(-18.0178701645078,1.13818113947967,1.63916329694466));
#53212=CARTESIAN_POINT('Ctrl Pts',(-17.9067238196304,-0.760007328031514,
1.84518331925479));
#53213=CARTESIAN_POINT('Ctrl Pts',(-17.7955774747529,-1.9624555569219,0.362050835414104));
#53214=CARTESIAN_POINT('Ctrl Pts',(-17.6844311298756,-1.36839571661786,
-1.45251705086709));
#53215=CARTESIAN_POINT('Ctrl Pts',(-17.5732847849981,0.478346732514791,
-1.93739439036303));
#53216=CARTESIAN_POINT('Ctrl Pts',(-17.4621384401207,1.88719199625409,-0.64870562629918));
#53217=CARTESIAN_POINT('Ctrl Pts',(-17.3509920952433,1.56842837864508,1.23383347392527));
#53218=CARTESIAN_POINT('Ctrl Pts',(-17.2398457503659,-0.186135519001358,
1.98687347077861));
#53219=CARTESIAN_POINT('Ctrl Pts',(-17.1286994054884,-1.77030373014666,
0.92105229132037));
#53220=CARTESIAN_POINT('Ctrl Pts',(-17.017553060611,-1.73386712050211,-0.987935943651935));
#53221=CARTESIAN_POINT('Ctrl Pts',(-16.9064067157336,-0.110181178302628,
-1.99252922896141));
#53222=CARTESIAN_POINT('Ctrl Pts',(-16.7952603708562,1.61436889567086,-1.1730838371609));
#53223=CARTESIAN_POINT('Ctrl Pts',(-16.6841140259787,1.8610629552752,0.720248080053035));
#53224=CARTESIAN_POINT('Ctrl Pts',(-16.5729676811013,0.40406767290285,1.95423691911513));
#53225=CARTESIAN_POINT('Ctrl Pts',(-16.4618213362239,-1.42282685753662,
1.3992413493712));
#53226=CARTESIAN_POINT('Ctrl Pts',(-16.3506749913465,-1.94721039779585,
-0.43667411994929));
#53227=CARTESIAN_POINT('Ctrl Pts',(-16.239528646469,-0.689041879884402,
-1.87284113263327));
#53228=CARTESIAN_POINT('Ctrl Pts',(-16.1283823015916,1.19990234800887,-1.59453660213884));
#53229=CARTESIAN_POINT('Ctrl Pts',(-16.0172359567142,1.99040934360917,0.143468690629876));
#53230=CARTESIAN_POINT('Ctrl Pts',(-15.9060896118368,0.958818287520326,
1.75013716943395));
#53231=CARTESIAN_POINT('Ctrl Pts',(-15.7949432669594,-0.950512284424457,
1.75466208070839));
#53232=CARTESIAN_POINT('Ctrl Pts',(-15.6837969220819,-1.98970697848199,
0.152901144854428));
#53233=CARTESIAN_POINT('Ctrl Pts',(-15.5726505772045,-1.20744659317862,
-1.588831440065));
#53234=CARTESIAN_POINT('Ctrl Pts',(-15.4615042323271,0.680157319582284,
-1.87608598975003));
#53235=CARTESIAN_POINT('Ctrl Pts',(-15.3503578874496,1.94511879407684,-0.445898527971097));
#53236=CARTESIAN_POINT('Ctrl Pts',(-15.2392115425722,1.42944294571563,1.39248177196742));
#53237=CARTESIAN_POINT('Ctrl Pts',(-15.1280651976948,-0.394800517016975,
1.95613015213222));
#53238=CARTESIAN_POINT('Ctrl Pts',(-15.0169188528174,-1.85762824626129,
0.729060984424456));
#53239=CARTESIAN_POINT('Ctrl Pts',(-14.9057725079399,-1.61991089961792,
-1.16541893652745));
#53240=CARTESIAN_POINT('Ctrl Pts',(-14.7946261630626,0.100735827145627,
-1.99302907993009));
#53241=CARTESIAN_POINT('Ctrl Pts',(-14.6834798181851,1.72916506358908,-0.99614296322402));
#53242=CARTESIAN_POINT('Ctrl Pts',(-14.5723334733077,1.77464941307702,0.912651127749848));
#53243=CARTESIAN_POINT('Ctrl Pts',(-14.4611871284303,0.195550734766548,
1.98596891477434));
#53244=CARTESIAN_POINT('Ctrl Pts',(-14.3500407835529,-1.56256268439037,
1.24125359120065));
#53245=CARTESIAN_POINT('Ctrl Pts',(-14.2388944386754,-1.89024550794569,
-0.639753499411164));
#53246=CARTESIAN_POINT('Ctrl Pts',(-14.127748093798,-0.487524146904184,
-1.93510537865592));
#53247=CARTESIAN_POINT('Ctrl Pts',(-14.0166017489206,1.36149576125667,-1.4589866045985));
#53248=CARTESIAN_POINT('Ctrl Pts',(-13.9054554040432,1.96414954782845,0.352745197108303));
#53249=CARTESIAN_POINT('Ctrl Pts',(-13.7943090591657,0.768744520108917,
1.84156033925587));
#53250=CARTESIAN_POINT('Ctrl Pts',(-13.6831627142883,-1.13039911134791,
1.64453959191672));
#53251=CARTESIAN_POINT('Ctrl Pts',(-13.5720163694109,-1.99473147394114,
-0.0579565974355843));
#53252=CARTESIAN_POINT('Ctrl Pts',(-13.4608700245335,-1.0330091388004,-1.70739706555697));
#53253=CARTESIAN_POINT('Ctrl Pts',(-13.349723679656,0.874369900188122,-1.7938199179301));
#53254=CARTESIAN_POINT('Ctrl Pts',(-13.2385773347786,1.98131675837734,-0.238110317480801));
#53255=CARTESIAN_POINT('Ctrl Pts',(-13.1274309899012,1.27448927069651,1.53557471950966));
#53256=CARTESIAN_POINT('Ctrl Pts',(-13.0162846450238,-0.599055216425213,
1.90353499258393));
#53257=CARTESIAN_POINT('Ctrl Pts',(-12.9051383001463,-1.92420128178143,
0.528925370452593));
#53258=CARTESIAN_POINT('Ctrl Pts',(-12.7939919552689,-1.48785872779961,
-1.32988308750365));
#53259=CARTESIAN_POINT('Ctrl Pts',(-12.6828456103915,0.310527517253561,
-1.97126489375378));
#53260=CARTESIAN_POINT('Ctrl Pts',(-12.5716992655141,1.82464480727981,-0.808074221581474));
#53261=CARTESIAN_POINT('Ctrl Pts',(-12.4605529206366,1.66841134305336,1.09485899123521));
#53262=CARTESIAN_POINT('Ctrl Pts',(-12.3494065757592,-0.0151506917279239,
1.99551574207219));
#53263=CARTESIAN_POINT('Ctrl Pts',(-12.2382602308818,-1.68484319461224,
1.0693998456548));
#53264=CARTESIAN_POINT('Ctrl Pts',(-12.1271138860044,-1.81216477155529,
-0.835686221647619));
#53265=CARTESIAN_POINT('Ctrl Pts',(-12.0159675411269,-0.280560303867124,
-1.97575265056427));
#53266=CARTESIAN_POINT('Ctrl Pts',(-11.9048211962496,1.50787996731995,-1.30713833409968));
#53267=CARTESIAN_POINT('Ctrl Pts',(-11.7936748513721,1.91594832684148,0.55808120304399));
#53268=CARTESIAN_POINT('Ctrl Pts',(-11.6825285064947,0.570083142650521,
1.91241152234122));
#53269=CARTESIAN_POINT('Ctrl Pts',(-11.5713821616172,-1.29765830124531,
1.51604602619013));
#53270=CARTESIAN_POINT('Ctrl Pts',(-11.4602358167399,-1.97747291488927,
-0.26816690921338));
#53271=CARTESIAN_POINT('Ctrl Pts',(-11.3490894718624,-0.847031986347007,
-1.8068894361368));
#53272=CARTESIAN_POINT('Ctrl Pts',(-11.237943126985,1.05881493443335,-1.69151516544742));
#53273=CARTESIAN_POINT('Ctrl Pts',(-11.1267967821076,1.99538152334385,-0.0276621874708096));
#53274=CARTESIAN_POINT('Ctrl Pts',(-11.0156504372301,1.10529833403908,1.66151383174746));
#53275=CARTESIAN_POINT('Ctrl Pts',(-10.9045040923527,-0.79661789727502,
1.82967553026728));
#53276=CARTESIAN_POINT('Ctrl Pts',(-10.7933577474753,-1.96927915235719,
0.322881155239884));
#53277=CARTESIAN_POINT('Ctrl Pts',(-10.6822114025979,-1.33918575384856,
-1.4794911750351));
#53278=CARTESIAN_POINT('Ctrl Pts',(-10.5710650577204,0.516850318599018,
-1.92747979716568));
#53279=CARTESIAN_POINT('Ctrl Pts',(-10.459918712843,1.89974152687182,-0.610978519586766));
#53280=CARTESIAN_POINT('Ctrl Pts',(-10.3487723679656,1.54353552584929,1.26483623475882));
#53281=CARTESIAN_POINT('Ctrl Pts',(-10.2376260230882,-0.225682870534658,
1.9827707538354));
#53282=CARTESIAN_POINT('Ctrl Pts',(-10.1264796782107,-1.78830239818783,
0.885599883103732));
#53283=CARTESIAN_POINT('Ctrl Pts',(-10.0153333333333,-1.7138404249772,-1.02228353113588));
#53284=CARTESIAN_POINT('Ctrl Pts',(-9.9041869884559,-0.07046233444443,-1.99432887953376));
#53285=CARTESIAN_POINT('Ctrl Pts',(-9.79304064357848,1.63741971489506,-1.1406880807612));
#53286=CARTESIAN_POINT('Ctrl Pts',(-9.68189429870107,1.84634413429414,0.757182909259928));
#53287=CARTESIAN_POINT('Ctrl Pts',(-9.57074795382363,0.365053392351222,
1.96189924334829));
#53288=CARTESIAN_POINT('Ctrl Pts',(-9.45960160894621,-1.4504214093186,1.37061677930337));
#53289=CARTESIAN_POINT('Ctrl Pts',(-9.3484552640688,-1.93812409590406,-0.475381540653165));
#53290=CARTESIAN_POINT('Ctrl Pts',(-9.23730891919136,-0.651592678124332,
-1.88619712706082));
#53291=CARTESIAN_POINT('Ctrl Pts',(-9.12616257431395,1.23143199523488,-1.5703145740359));
#53292=CARTESIAN_POINT('Ctrl Pts',(-9.01501622943651,1.98715597212704,0.183094955576432));
#53293=CARTESIAN_POINT('Ctrl Pts',(-8.9038698845591,0.923760159996531,1.76889224858976));
#53294=CARTESIAN_POINT('Ctrl Pts',(-8.79272353968166,-0.985281595850083,
1.73537684587435));
#53295=CARTESIAN_POINT('Ctrl Pts',(-8.68157719480427,-1.99235829514795,
0.113230049337008));
#53296=CARTESIAN_POINT('Ctrl Pts',(-8.57043084992681,-1.17555279679042,
-1.61257193398495));
#53297=CARTESIAN_POINT('Ctrl Pts',(-8.45928450504942,0.717399408558318,
-1.86216291148704));
#53298=CARTESIAN_POINT('Ctrl Pts',(-8.34813816017196,1.9536163203283,-0.407057604356679));
#53299=CARTESIAN_POINT('Ctrl Pts',(-8.23699181529457,1.40141694353548,1.42068405026924));
#53300=CARTESIAN_POINT('Ctrl Pts',(-8.12584547041712,-0.433693956265927,
1.94787632374751));
#53301=CARTESIAN_POINT('Ctrl Pts',(-8.01469912553972,-1.8717845570626,0.691906924564031));
#53302=CARTESIAN_POINT('Ctrl Pts',(-7.90355278066229,-1.59637084501215,
-1.19746095782407));
#53303=CARTESIAN_POINT('Ctrl Pts',(-7.79240643578486,0.140422766509441,
-1.99062655135601));
#53304=CARTESIAN_POINT('Ctrl Pts',(-7.68126009090745,1.74866792135743,-0.961495252787647));
#53305=CARTESIAN_POINT('Ctrl Pts',(-7.57011374603,1.75611451545356,0.947826159657482));
#53306=CARTESIAN_POINT('Ctrl Pts',(-7.4589674011526,0.155945647220306,1.98947067719803));
#53307=CARTESIAN_POINT('Ctrl Pts',(-7.34782105627516,-1.58698192584009,
1.20987643475463));
#53308=CARTESIAN_POINT('Ctrl Pts',(-7.23667471139775,-1.87712458085155,
-0.677285706537936));
#53309=CARTESIAN_POINT('Ctrl Pts',(-7.12552836652031,-0.448874457749643,
-1.9444341957232));
#53310=CARTESIAN_POINT('Ctrl Pts',(-7.0143820216429,1.39029278526267,-1.43157206998609));
#53311=CARTESIAN_POINT('Ctrl Pts',(-6.90323567676547,1.95673199198518,0.391806753207983));
#53312=CARTESIAN_POINT('Ctrl Pts',(-6.79208933188805,0.731902703248883,
1.85651045062901));
#53313=CARTESIAN_POINT('Ctrl Pts',(-6.68094298701063,-1.16293875856013,
1.62169234571676));
#53314=CARTESIAN_POINT('Ctrl Pts',(-6.5697966421332,-1.99318089409997,-0.0976859442937018));
#53315=CARTESIAN_POINT('Ctrl Pts',(-6.45865029725579,-0.998787792941156,
-1.72763872525175));
#53316=CARTESIAN_POINT('Ctrl Pts',(-6.34750395237835,0.909934462374966,
-1.77604388867507));
#53317=CARTESIAN_POINT('Ctrl Pts',(-6.23635760750093,1.98566735478354,-0.198589467154337));
#53318=CARTESIAN_POINT('Ctrl Pts',(-6.12521126262351,1.2436431963268,1.5606614689124));
#53319=CARTESIAN_POINT('Ctrl Pts',(-6.01406491774608,-0.63686026655008,
1.89122225589894));
#53320=CARTESIAN_POINT('Ctrl Pts',(-5.90291857286866,-1.93435709583923,
0.490484705260119));
#53321=CARTESIAN_POINT('Ctrl Pts',(-5.79177222799124,-1.4610682789916,-1.35926160265134));
#53322=CARTESIAN_POINT('Ctrl Pts',(-5.6806258831138,0.349739211129583,-1.96468702457062));
#53323=CARTESIAN_POINT('Ctrl Pts',(-5.5694795382364,1.84038183805583,-0.77156160510482));
#53324=CARTESIAN_POINT('Ctrl Pts',(-5.45833319335896,1.64626742128525,1.12788128716304));
#53325=CARTESIAN_POINT('Ctrl Pts',(-5.34718684848155,-0.0549041596382843,
1.99481782465771));
#53326=CARTESIAN_POINT('Ctrl Pts',(-5.23604050360411,-1.70581433949485,
1.03562061561725));
#53327=CARTESIAN_POINT('Ctrl Pts',(-5.12489415872671,-1.7951557925382,-0.871623944619641));
#53328=CARTESIAN_POINT('Ctrl Pts',(-5.01374781384927,-0.241141881236654,
-1.98095007848036));
#53329=CARTESIAN_POINT('Ctrl Pts',(-4.90260146897185,1.53362267786139,-1.2768375394963));
#53330=CARTESIAN_POINT('Ctrl Pts',(-4.79145512409443,1.90444944781581,0.596141695431386));
#53331=CARTESIAN_POINT('Ctrl Pts',(-4.680308779217,0.53186919471367,1.92338965891789));
#53332=CARTESIAN_POINT('Ctrl Pts',(-4.56916243433959,-1.32760478532606,
1.48989199417179));
#53333=CARTESIAN_POINT('Ctrl Pts',(-4.45801608946215,-1.97173775999777,
-0.307510692686641));
#53334=CARTESIAN_POINT('Ctrl Pts',(-4.34686974458474,-0.810865376113923,
-1.82340614294705));
#53335=CARTESIAN_POINT('Ctrl Pts',(-4.2357233997073,1.09230467972553,-1.67008476041437));
#53336=CARTESIAN_POINT('Ctrl Pts',(-4.12457705482989,1.99553658959009,0.0120971039477285));
#53337=CARTESIAN_POINT('Ctrl Pts',(-4.01343070995246,1.07197676757322,1.68320480931454));
#53338=CARTESIAN_POINT('Ctrl Pts',(-3.90228436507504,-0.832912239782294,
1.81344143030452));
#53339=CARTESIAN_POINT('Ctrl Pts',(-3.79113802019761,-1.97532101953316,
0.283583303634182));
#53340=CARTESIAN_POINT('Ctrl Pts',(-3.67999167532019,-1.30944418572589,
-1.50587799797332));
#53341=CARTESIAN_POINT('Ctrl Pts',(-3.56884533044276,0.555148734945638,
-1.91680006845999));
#53342=CARTESIAN_POINT('Ctrl Pts',(-3.45769898556535,1.91153693298929,-0.573008877829148));
#53343=CARTESIAN_POINT('Ctrl Pts',(-3.34655264068792,1.51802994870092,1.29533690410844));
#53344=CARTESIAN_POINT('Ctrl Pts',(-3.2354062958105,-0.265140634670444,
1.97788095305015));
#53345=CARTESIAN_POINT('Ctrl Pts',(-3.12425995093307,-1.80559117871824,
0.84979592559486));
#53346=CARTESIAN_POINT('Ctrl Pts',(-3.01311360605565,-1.69313340071988,
-1.05622531105494));
#53347=CARTESIAN_POINT('Ctrl Pts',(-2.90196726117823,-0.0307155194536576,
-1.99533685850639));
#53348=CARTESIAN_POINT('Ctrl Pts',(-2.7908209163008,1.65982054077328,-1.10783951413039));
#53349=CARTESIAN_POINT('Ctrl Pts',(-2.67967457142338,1.83089238658801,0.793817164320537));
#53350=CARTESIAN_POINT('Ctrl Pts',(-2.56852822654595,0.325894197617876,
1.96878277188174));
#53351=CARTESIAN_POINT('Ctrl Pts',(-2.45738188166853,-1.47744019566639,
1.34144812122869));
#53352=CARTESIAN_POINT('Ctrl Pts',(-2.34623553679111,-1.92826844032713,
-0.513900242210063));
#53353=CARTESIAN_POINT('Ctrl Pts',(-2.23508919191368,-0.613884805358574,
-1.89880439437223));
#53354=CARTESIAN_POINT('Ctrl Pts',(-2.12394284703626,1.2624727851227,-1.54546915180465));
#53355=CARTESIAN_POINT('Ctrl Pts',(-2.01279650215884,1.98311382560099,0.222648463718466));
#53356=CARTESIAN_POINT('Ctrl Pts',(-1.90165015728141,0.888335240741561,
1.78694528831349));
#53357=CARTESIAN_POINT('Ctrl Pts',(-1.790503812404,-1.01965960873761,1.71540246117927));
#53358=CARTESIAN_POINT('Ctrl Pts',(-1.67935746752656,-1.9942190635569,0.0735145229216604));
#53359=CARTESIAN_POINT('Ctrl Pts',(-1.56821112264915,-1.14319170140108,
-1.6356732823008));
#53360=CARTESIAN_POINT('Ctrl Pts',(-1.45706477777171,0.754355481768247,
-1.84749875509779));
#53361=CARTESIAN_POINT('Ctrl Pts',(-1.3459184328943,1.96134068640505,-0.368058653232534));
#53362=CARTESIAN_POINT('Ctrl Pts',(-1.23477208801687,1.3728301615305,1.44832914076707));
#53363=CARTESIAN_POINT('Ctrl Pts',(-1.12362574313945,-0.472406731010585,
1.93883638708916));
#53364=CARTESIAN_POINT('Ctrl Pts',(-1.01247939826202,-1.88521401833496,
0.654502696535881));
#53365=CARTESIAN_POINT('Ctrl Pts',(-0.901333053384601,-1.57216632097497,
-1.22907422156167));
#53366=CARTESIAN_POINT('Ctrl Pts',(-0.790186708507175,0.179995429844686,
-1.98734519828315));
#53367=CARTESIAN_POINT('Ctrl Pts',(-0.679040363629751,1.76758797928351,
-0.926634471973894));
#53368=CARTESIAN_POINT('Ctrl Pts',(-0.567894018752328,1.73667056918864,
0.982945946718963));
#53369=CARTESIAN_POINT('Ctrl Pts',(-0.456747673874906,0.116682879679813,
1.99156959023754));
#53370=CARTESIAN_POINT('Ctrl Pts',(-0.345601328997482,-1.61154942417229,
1.17920674007046));
#53371=CARTESIAN_POINT('Ctrl Pts',(-0.234454984120056,-1.86169777943505,
-0.71699198523252));
#53372=CARTESIAN_POINT('Ctrl Pts',(-0.160357420868444,-0.896388758474477,
-1.53694076122322));
#53373=CARTESIAN_POINT('Ctrl Pts',(-0.123308639242636,-0.346915509926856,
-1.652307197048));
#53374=CARTESIAN_POINT('Ctrl Pts',(-29.7226913607574,-0.802959149489686,
1.63459616787406));
#53375=CARTESIAN_POINT('Ctrl Pts',(-29.6856425791315,-1.34654261146935,
1.36757283643219));
#53376=CARTESIAN_POINT('Ctrl Pts',(-29.6115450158799,-2.13699697723614,
0.253271596645648));
#53377=CARTESIAN_POINT('Ctrl Pts',(-29.5003986710025,-1.37018370663775,
-1.66203790618904));
#53378=CARTESIAN_POINT('Ctrl Pts',(-29.3892523261251,0.652727265457014,
-2.05056399477137));
#53379=CARTESIAN_POINT('Ctrl Pts',(-29.2781059812477,2.07719244398607,-0.56457687295854));
#53380=CARTESIAN_POINT('Ctrl Pts',(-29.1669596363702,1.60059299295594,1.43962549295637));
#53381=CARTESIAN_POINT('Ctrl Pts',(-29.0558132914928,-0.341502513910902,
2.12521518253081));
#53382=CARTESIAN_POINT('Ctrl Pts',(-28.9446669466154,-1.9708414067249,0.865680507114811));
#53383=CARTESIAN_POINT('Ctrl Pts',(-28.8335206017379,-1.7960648593605,-1.18653159130759));
#53384=CARTESIAN_POINT('Ctrl Pts',(-28.7223742568606,0.0229357119706541,
-2.15244150481461));
#53385=CARTESIAN_POINT('Ctrl Pts',(-28.6112279119831,1.82092087124584,-1.14797806388266));
#53386=CARTESIAN_POINT('Ctrl Pts',(-28.5000815671057,1.95197439015737,0.907418139493177));
#53387=CARTESIAN_POINT('Ctrl Pts',(-28.3889352222283,0.296109408884188,
2.13211325412446));
#53388=CARTESIAN_POINT('Ctrl Pts',(-28.2777888773509,-1.63082284536082,
1.40499707683198));
#53389=CARTESIAN_POINT('Ctrl Pts',(-28.1666425324734,-2.06483796472262,
-0.608312235744213));
#53390=CARTESIAN_POINT('Ctrl Pts',(-28.055496187596,-0.60861941081362,-2.0647466732867));
#53391=CARTESIAN_POINT('Ctrl Pts',(-27.9443498427186,1.40475259530209,-1.6310329452328));
#53392=CARTESIAN_POINT('Ctrl Pts',(-27.8332034978412,2.13215970594569,0.295792328695355));
#53393=CARTESIAN_POINT('Ctrl Pts',(-27.7220571529637,0.907704863562922,
1.95183748945672));
#53394=CARTESIAN_POINT('Ctrl Pts',(-27.6109108080863,-1.14769822153575,
1.82109494198778));
#53395=CARTESIAN_POINT('Ctrl Pts',(-27.4997644632089,-2.15245379105352,
0.0232512358109067));
#53396=CARTESIAN_POINT('Ctrl Pts',(-27.3886181183314,-1.1867695091042,-1.79587750823898));
#53397=CARTESIAN_POINT('Ctrl Pts',(-27.2774717734541,0.865329685575796,
-1.97099022596782));
#53398=CARTESIAN_POINT('Ctrl Pts',(-27.1663254285766,2.12527246766768,-0.341781893895144));
#53399=CARTESIAN_POINT('Ctrl Pts',(-27.0551790836992,1.43965825175809,1.60030685718542));
#53400=CARTESIAN_POINT('Ctrl Pts',(-26.9440327388218,-0.563875065354492,
2.07741253389249));
#53401=CARTESIAN_POINT('Ctrl Pts',(-26.8328863939443,-2.05121523859028,
0.652774056083331));
#53402=CARTESIAN_POINT('Ctrl Pts',(-26.721740049067,-1.66079328087856,-1.36943915560345));
#53403=CARTESIAN_POINT('Ctrl Pts',(-26.6105937041895,0.249983377088396,
-2.13801455439055));
#53404=CARTESIAN_POINT('Ctrl Pts',(-26.4994473593121,1.93191553850937,-0.949368355976965));
#53405=CARTESIAN_POINT('Ctrl Pts',(-26.3883010144347,1.84529715019161,1.10836652363136));
#53406=CARTESIAN_POINT('Ctrl Pts',(-26.2771546695572,0.0694220504867175,
2.15145962133678));
#53407=CARTESIAN_POINT('Ctrl Pts',(-26.1660083246798,-1.77000469168292,
1.22502298537633));
#53408=CARTESIAN_POINT('Ctrl Pts',(-26.0548619798024,-1.98910036448447,
-0.822847290379835));
#53409=CARTESIAN_POINT('Ctrl Pts',(-25.943715634925,-0.387296275952628,
-2.1174511843081));
#53410=CARTESIAN_POINT('Ctrl Pts',(-25.8325692900475,1.56905387221744,-1.47365798927873));
#53411=CARTESIAN_POINT('Ctrl Pts',(-25.7214229451701,2.08903113922897,0.519178988998727));
#53412=CARTESIAN_POINT('Ctrl Pts',(-25.6102766002927,0.696628130832529,
2.03673934773722));
#53413=CARTESIAN_POINT('Ctrl Pts',(-25.4991302554153,-1.3334953364323,1.68978936882682));
#53414=CARTESIAN_POINT('Ctrl Pts',(-25.3879839105379,-2.14288535896546,
-0.204059456087));
#53415=CARTESIAN_POINT('Ctrl Pts',(-25.2768375656604,-0.990594860805363,
-1.91110432604642));
#53416=CARTESIAN_POINT('Ctrl Pts',(-25.165691220783,1.06852466309368,-1.86865003883757));
#53417=CARTESIAN_POINT('Ctrl Pts',(-25.0545448759056,2.14947519222985,-0.115560898558425));
#53418=CARTESIAN_POINT('Ctrl Pts',(-24.9433985310282,1.26271261125054,1.74331717844919));
#53419=CARTESIAN_POINT('Ctrl Pts',(-24.8322521861507,-0.779986157523649,
2.00629497266944));
#53420=CARTESIAN_POINT('Ctrl Pts',(-24.7211058412733,-2.10865529087055,
0.432632393113157));
#53421=CARTESIAN_POINT('Ctrl Pts',(-24.6099594963959,-1.50697943788803,
-1.53707868929012));
#53422=CARTESIAN_POINT('Ctrl Pts',(-24.4988131515184,0.474243947127435,
-2.09968821540251));
#53423=CARTESIAN_POINT('Ctrl Pts',(-24.3876668066411,2.02132599590933,-0.740161564490013));
#53424=CARTESIAN_POINT('Ctrl Pts',(-24.2765204617636,1.71800768820146,1.29693774197832));
#53425=CARTESIAN_POINT('Ctrl Pts',(-24.1653741168862,-0.158041611505553,
2.14676984614558));
#53426=CARTESIAN_POINT('Ctrl Pts',(-24.0542277720087,-1.88941347923875,
1.03136541912073));
#53427=CARTESIAN_POINT('Ctrl Pts',(-23.9430814271314,-1.89114283378241,
-1.0281909868894));
#53428=CARTESIAN_POINT('Ctrl Pts',(-23.8319350822539,-0.161646556792161,
-2.14650141252327));
#53429=CARTESIAN_POINT('Ctrl Pts',(-23.7207887373765,1.71582725915959,-1.29982104153306));
#53430=CARTESIAN_POINT('Ctrl Pts',(-23.6096423924991,2.02256613257899,0.73676601620298));
#53431=CARTESIAN_POINT('Ctrl Pts',(-23.4984960476216,0.477769380214973,
2.09888883522119));
#53432=CARTESIAN_POINT('Ctrl Pts',(-23.3873497027443,-1.50439602681377,
1.53960726089289));
#53433=CARTESIAN_POINT('Ctrl Pts',(-23.2762033578667,-2.10937885668692,
-0.42909062242064));
#53434=CARTESIAN_POINT('Ctrl Pts',(-23.1650570129894,-0.783354319967773,
-2.00498227739674));
#53435=CARTESIAN_POINT('Ctrl Pts',(-23.0539106681119,1.259783198952,-1.74543525085448));
#53436=CARTESIAN_POINT('Ctrl Pts',(-22.9427643232346,2.14966622791904,0.111951024253906));
#53437=CARTESIAN_POINT('Ctrl Pts',(-22.8316179783571,1.0716612652779,1.86685298183605));
#53438=CARTESIAN_POINT('Ctrl Pts',(-22.7204716334797,-0.987384059640079,
1.91276518215275));
#53439=CARTESIAN_POINT('Ctrl Pts',(-22.6093252886022,-2.14253965096347,
0.207657813088019));
#53440=CARTESIAN_POINT('Ctrl Pts',(-22.4981789437248,-1.33633119613124,
-1.68754758674641));
#53441=CARTESIAN_POINT('Ctrl Pts',(-22.3870325988474,0.693206759589962,
-2.03790635499916));
#53442=CARTESIAN_POINT('Ctrl Pts',(-22.27588625397,2.08815631261794,-0.522686461811507));
#53443=CARTESIAN_POINT('Ctrl Pts',(-22.1647399090925,1.57152644050903,1.47102092781448));
#53444=CARTESIAN_POINT('Ctrl Pts',(-22.0535935642152,-0.383739797844597,
2.11809860271834));
#53445=CARTESIAN_POINT('Ctrl Pts',(-21.9424472193377,-1.9877157148112,0.826186516701757));
#53446=CARTESIAN_POINT('Ctrl Pts',(-21.8313008744603,-1.77205943255289,
-1.22204880867642));
#53447=CARTESIAN_POINT('Ctrl Pts',(-21.7201545295828,0.0658089086968051,
-2.15157317115252));
#53448=CARTESIAN_POINT('Ctrl Pts',(-21.6090081847055,1.84343321788083,-1.11146385208909));
#53449=CARTESIAN_POINT('Ctrl Pts',(-21.497861839828,1.93350713171299,0.946122663771537));
#53450=CARTESIAN_POINT('Ctrl Pts',(-21.3867154949506,0.253573489595389,
2.13759173105193));
#53451=CARTESIAN_POINT('Ctrl Pts',(-21.2755691500732,-1.65849117764792,
1.37222627031812));
#53452=CARTESIAN_POINT('Ctrl Pts',(-21.1644228051957,-2.05230857920252,
-0.649328436939962));
#53453=CARTESIAN_POINT('Ctrl Pts',(-21.0532764603183,-0.567362963673909,
-2.07646266297719));
#53454=CARTESIAN_POINT('Ctrl Pts',(-20.9421301154409,1.43696875403018,-1.60272228512245));
#53455=CARTESIAN_POINT('Ctrl Pts',(-20.8309837705635,2.12584344001191,0.3382123472694));
#53456=CARTESIAN_POINT('Ctrl Pts',(-20.7198374256861,0.868638440084387,
1.96953425552716));
#53457=CARTESIAN_POINT('Ctrl Pts',(-20.6086910808086,-1.18375193936417,
1.79786797884015));
#53458=CARTESIAN_POINT('Ctrl Pts',(-20.4975447359312,-2.1524897981269,-0.0196365029161898));
#53459=CARTESIAN_POINT('Ctrl Pts',(-20.3863983910538,-1.15075485940167,
-1.81916496691493));
#53460=CARTESIAN_POINT('Ctrl Pts',(-20.2752520461764,0.904425790890365,
-1.95335913545346));
#53461=CARTESIAN_POINT('Ctrl Pts',(-20.1641057012989,2.1316599301946,-0.299372452456672));
#53462=CARTESIAN_POINT('Ctrl Pts',(-20.0529593564215,1.40748974247311,1.62867140581522));
#53463=CARTESIAN_POINT('Ctrl Pts',(-19.9418130115441,-0.605151244366693,
2.06576617619918));
#53464=CARTESIAN_POINT('Ctrl Pts',(-19.8306666666667,-2.06381326859854,
0.611778322306184));
#53465=CARTESIAN_POINT('Ctrl Pts',(-19.7195203217892,-1.63318043605245,
-1.40225517883968));
#53466=CARTESIAN_POINT('Ctrl Pts',(-19.6083739769118,0.292529225861806,
-2.13260980380937));
#53467=CARTESIAN_POINT('Ctrl Pts',(-19.4972276320344,1.95044626802358,-0.91069055053848));
#53468=CARTESIAN_POINT('Ctrl Pts',(-19.386081287157,1.82284901067655,1.1449102181231));
#53469=CARTESIAN_POINT('Ctrl Pts',(-19.2749349422795,0.0265449410641972,
2.15241568694131));
#53470=CARTESIAN_POINT('Ctrl Pts',(-19.1637885974022,-1.79405939901794,
1.1895162025305));
#53471=CARTESIAN_POINT('Ctrl Pts',(-19.0526422525247,-1.97231205598467,
-0.862312633042507));
#53472=CARTESIAN_POINT('Ctrl Pts',(-18.9414959076473,-0.345033621534715,
-2.12474697865364));
#53473=CARTESIAN_POINT('Ctrl Pts',(-18.8303495627699,1.5981019965565,-1.44210538168655));
#53474=CARTESIAN_POINT('Ctrl Pts',(-18.7192032178924,2.07827295178796,0.560695515546295));
#53475=CARTESIAN_POINT('Ctrl Pts',(-18.608056873015,0.655912094410212,2.05021395168738));
#53476=CARTESIAN_POINT('Ctrl Pts',(-18.4969105281376,-1.36689618004863,
1.66288687416061));
#53477=CARTESIAN_POINT('Ctrl Pts',(-18.3857641832601,-2.13839457971973,
-0.246711460440006));
#53478=CARTESIAN_POINT('Ctrl Pts',(-18.2746178383827,-0.952323492510973,
-1.93046053803202));
#53479=CARTESIAN_POINT('Ctrl Pts',(-18.1634714935053,1.10554152284303,-1.84699102990705));
#53480=CARTESIAN_POINT('Ctrl Pts',(-18.0523251486279,2.15135087170732,-0.0727141670605007));
#53481=CARTESIAN_POINT('Ctrl Pts',(-17.9411788037505,1.22773004058181,1.76812806966582));
#53482=CARTESIAN_POINT('Ctrl Pts',(-17.830032458873,-0.819802573879665,
1.99035716974302));
#53483=CARTESIAN_POINT('Ctrl Pts',(-17.7188861139956,-2.11685605829079,
0.390535980115425));
#53484=CARTESIAN_POINT('Ctrl Pts',(-17.6077397691182,-1.47605725523029,
-1.56679702021966));
#53485=CARTESIAN_POINT('Ctrl Pts',(-17.4965934242408,0.515981712358321,
-2.08982314940737));
#53486=CARTESIAN_POINT('Ctrl Pts',(-17.3854470793633,2.03567097167509,-0.699743966295212));
#53487=CARTESIAN_POINT('Ctrl Pts',(-17.2743007344859,1.69182792630349,1.33090803253524));
#53488=CARTESIAN_POINT('Ctrl Pts',(-17.1631543896085,-0.200780139795509,
2.14319510515279));
#53489=CARTESIAN_POINT('Ctrl Pts',(-17.0520080447311,-1.90958626449289,
0.993518103381745));
#53490=CARTESIAN_POINT('Ctrl Pts',(-16.9408616998537,-1.87028292455343,
-1.06566397396696));
#53491=CARTESIAN_POINT('Ctrl Pts',(-16.8297153549762,-0.118849924512552,
-2.14929584253321));
#53492=CARTESIAN_POINT('Ctrl Pts',(-16.7185690100988,1.74138291441223,-1.26537878466501));
#53493=CARTESIAN_POINT('Ctrl Pts',(-16.6074226652214,2.0074861710061,0.776915179737431));
#53494=CARTESIAN_POINT('Ctrl Pts',(-16.496276320344,0.435858584581321,2.10799080110278));
#53495=CARTESIAN_POINT('Ctrl Pts',(-16.3851299754665,-1.53477088571601,
1.50932973589128));
#53496=CARTESIAN_POINT('Ctrl Pts',(-16.2739836305891,-2.1004114527853,-0.471030415467579));
#53497=CARTESIAN_POINT('Ctrl Pts',(-16.1628372857117,-0.743253763227663,
-2.020191022338));
#53498=CARTESIAN_POINT('Ctrl Pts',(-16.0516909408343,1.29430730075948,-1.71999027162594));
#53499=CARTESIAN_POINT('Ctrl Pts',(-15.9405445959568,2.14700917054466,0.15475640498651));
#53500=CARTESIAN_POINT('Ctrl Pts',(-15.8293982510794,1.03425542228371,1.88783305532134));
#53501=CARTESIAN_POINT('Ctrl Pts',(-15.718251906202,-1.02529592615071,1.89271397392895));
#53502=CARTESIAN_POINT('Ctrl Pts',(-15.6071055613246,-2.1462515452984,0.16493097826492));
#53503=CARTESIAN_POINT('Ctrl Pts',(-15.4959592164472,-1.30244510598838,
-1.71383624339494));
#53504=CARTESIAN_POINT('Ctrl Pts',(-15.3848128715697,0.733670190629446,
-2.02369117571553));
#53505=CARTESIAN_POINT('Ctrl Pts',(-15.2736665266923,2.09815528754964,-0.480980574051286));
#53506=CARTESIAN_POINT('Ctrl Pts',(-15.1625201818149,1.54190750916428,1.5020383338883));
#53507=CARTESIAN_POINT('Ctrl Pts',(-15.0513738369374,-0.425862314851449,
2.11003298838585));
#53508=CARTESIAN_POINT('Ctrl Pts',(-14.94022749206,-2.00378122871642,0.786421458717215));
#53509=CARTESIAN_POINT('Ctrl Pts',(-14.8290811471826,-1.74736094769246,
-1.2571108311388));
#53510=CARTESIAN_POINT('Ctrl Pts',(-14.7179348023052,0.108661439607204,
-2.14983502037473));
#53511=CARTESIAN_POINT('Ctrl Pts',(-14.6067884574278,1.86521092298501,-1.07451669883004));
#53512=CARTESIAN_POINT('Ctrl Pts',(-14.4956421125503,1.91427385357279,0.984455959814731));
#53513=CARTESIAN_POINT('Ctrl Pts',(-14.3844957676729,0.210936118340905,
2.14221938121809));
#53514=CARTESIAN_POINT('Ctrl Pts',(-14.2733494227955,-1.68550073566969,
1.33891194383504));
#53515=CARTESIAN_POINT('Ctrl Pts',(-14.1622030779181,-2.03896472510586,
-0.690087511161547));
#53516=CARTESIAN_POINT('Ctrl Pts',(-14.0510567330406,-0.525881179982363,
-2.08735404467654));
#53517=CARTESIAN_POINT('Ctrl Pts',(-13.9399103881632,1.46861443072578,-1.57377558030083));
#53518=CARTESIAN_POINT('Ctrl Pts',(-13.8287640432858,2.11868332765266,0.380498200276715));
#53519=CARTESIAN_POINT('Ctrl Pts',(-13.7176176984084,0.829227183734402,
1.98644914383506));
#53520=CARTESIAN_POINT('Ctrl Pts',(-13.606471353531,-1.2193357442941,1.77392735645346));
#53521=CARTESIAN_POINT('Ctrl Pts',(-13.4953250086535,-2.15167135397382,
-0.0625164600374452));
#53522=CARTESIAN_POINT('Ctrl Pts',(-13.3841786637761,-1.11428340174446,
-1.8417302798955));
#53523=CARTESIAN_POINT('Ctrl Pts',(-13.2730323188987,0.943162872591929,
-1.93495264000216));
#53524=CARTESIAN_POINT('Ctrl Pts',(-13.1618859740213,2.13720120619835,-0.256844169705039));
#53525=CARTESIAN_POINT('Ctrl Pts',(-13.0507396291438,1.37476251341562,1.65638943337438));
#53526=CARTESIAN_POINT('Ctrl Pts',(-12.9395932842664,-0.646187201370086,
2.05329978913764));
#53527=CARTESIAN_POINT('Ctrl Pts',(-12.828446939389,-2.07559204403019,0.570539735729004));
#53528=CARTESIAN_POINT('Ctrl Pts',(-12.7173005945115,-1.60491928121084,
-1.4345145604297));
#53529=CARTESIAN_POINT('Ctrl Pts',(-12.6061542496342,0.334958951730538,
-2.12635848904713));
#53530=CARTESIAN_POINT('Ctrl Pts',(-12.4950079047567,1.96820274522673,-0.871651235855885));
#53531=CARTESIAN_POINT('Ctrl Pts',(-12.3838615598793,1.7996772700438,1.18099942716957));
#53532=CARTESIAN_POINT('Ctrl Pts',(-12.2727152150019,-0.0163427056773679,
2.15251732612268));
#53533=CARTESIAN_POINT('Ctrl Pts',(-12.1615688701244,-1.81740193361583,
1.15353722739085));
#53534=CARTESIAN_POINT('Ctrl Pts',(-12.050422525247,-1.9547408152798,-0.901435670675633));
#53535=CARTESIAN_POINT('Ctrl Pts',(-11.9392761803696,-0.302634002009415,
-2.13119932998182));
#53536=CARTESIAN_POINT('Ctrl Pts',(-11.8281298354922,1.62651573572611,-1.40998031359395));
#53537=CARTESIAN_POINT('Ctrl Pts',(-11.7169834906148,2.06668976973314,0.60198946748888));
#53538=CARTESIAN_POINT('Ctrl Pts',(-11.6058371457373,0.614935686055437,
2.06287469937045));
#53539=CARTESIAN_POINT('Ctrl Pts',(-11.4946908008599,-1.39975441833248,
1.63532427721413));
#53540=CARTESIAN_POINT('Ctrl Pts',(-11.3835444559825,-2.13305493988104,
-0.289265529810001));
#53541=CARTESIAN_POINT('Ctrl Pts',(-11.2723981111051,-0.913674088332984,
-1.94905043126032));
#53542=CARTESIAN_POINT('Ctrl Pts',(-11.1612517662276,1.14211952503,-1.82459883641102));
#53543=CARTESIAN_POINT('Ctrl Pts',(-11.0501054213502,2.15237254744109,-0.0298385708285128));
#53544=CARTESIAN_POINT('Ctrl Pts',(-10.9389590764728,1.19226010819787,1.79223708188598));
#53545=CARTESIAN_POINT('Ctrl Pts',(-10.8278127315954,-0.859293560071549,
1.9736292713949));
#53546=CARTESIAN_POINT('Ctrl Pts',(-10.7166663867179,-2.12421651508461,
0.348284539319401));
#53547=CARTESIAN_POINT('Ctrl Pts',(-10.6055200418405,-1.44454913448201,
-1.5958933928538));
#53548=CARTESIAN_POINT('Ctrl Pts',(-10.4943736969631,0.557514652648782,
-2.07912850381334));
#53549=CARTESIAN_POINT('Ctrl Pts',(-10.3832273520857,2.04920786417854,-0.659048596596637));
#53550=CARTESIAN_POINT('Ctrl Pts',(-10.2720810072083,1.66497657363818,1.36435000367326));
#53551=CARTESIAN_POINT('Ctrl Pts',(-10.1609346623308,-0.243438966074324,
2.13876959794267));
#53552=CARTESIAN_POINT('Ctrl Pts',(-10.0497883174534,-1.9290010172753,0.955276399079356));
#53553=CARTESIAN_POINT('Ctrl Pts',(-9.93864197257598,-1.84868058477054,
-1.10271393333884));
#53554=CARTESIAN_POINT('Ctrl Pts',(-9.82749562769855,-0.0760061133735042,
-2.15123708456717));
#53555=CARTESIAN_POINT('Ctrl Pts',(-9.71634928282113,1.76624730746878,-1.23043422097504));
#53556=CARTESIAN_POINT('Ctrl Pts',(-9.60520293794371,1.99160931445526,0.816755937757542));
#53557=CARTESIAN_POINT('Ctrl Pts',(-9.49405659306628,0.393774769814524,
2.11625597552487));
#53558=CARTESIAN_POINT('Ctrl Pts',(-9.38291024818886,-1.56453649946938,
1.47845306490103));
#53559=CARTESIAN_POINT('Ctrl Pts',(-9.27176390331143,-2.0906102661346,-0.512783227514099));
#53560=CARTESIAN_POINT('Ctrl Pts',(-9.16061755843402,-0.70285816326396,
-2.03459782896287));
#53561=CARTESIAN_POINT('Ctrl Pts',(-9.04947121355658,1.32831761223416,-1.69386252225961));
#53562=CARTESIAN_POINT('Ctrl Pts',(-8.93832486867917,2.14349983291531,0.197500353364697));
#53563=CARTESIAN_POINT('Ctrl Pts',(-8.82717852380173,0.996439019573689,
1.90806373152424));
#53564=CARTESIAN_POINT('Ctrl Pts',(-8.71603217892433,-1.06280078952167,
1.87191143088536));
#53565=CARTESIAN_POINT('Ctrl Pts',(-8.60488583404689,-2.14911146012652,
0.122138672172239));
#53566=CARTESIAN_POINT('Ctrl Pts',(-8.49373948916947,-1.26804199511632,
-1.73944457281875));
#53567=CARTESIAN_POINT('Ctrl Pts',(-8.38259314429205,0.773842382755913,
-2.0086726686889));
#53568=CARTESIAN_POINT('Ctrl Pts',(-8.27144679941462,2.10732137534329,-0.439083755459502));
#53569=CARTESIAN_POINT('Ctrl Pts',(-8.16030045453719,1.511676499705,1.53245948838031));
#53570=CARTESIAN_POINT('Ctrl Pts',(-8.04915410965979,-0.46781578086066,
2.10112977192388));
#53571=CARTESIAN_POINT('Ctrl Pts',(-7.93800776478234,-2.0190513183636,0.746344221590376));
#53572=CARTESIAN_POINT('Ctrl Pts',(-7.82686141990494,-1.72196882758612,
-1.2916738288395));
#53573=CARTESIAN_POINT('Ctrl Pts',(-7.71571507502751,0.151470836095693,
-2.14724346758807));
#53574=CARTESIAN_POINT('Ctrl Pts',(-7.60456873015009,1.88624821092527,-1.03714300367325));
#53575=CARTESIAN_POINT('Ctrl Pts',(-7.49342238527265,1.89428068216789,1.02239846461776));
#53576=CARTESIAN_POINT('Ctrl Pts',(-7.38227604039525,0.168215013541517,
2.1459966524919));
#53577=CARTESIAN_POINT('Ctrl Pts',(-7.2711296955178,-1.71184121457602,1.30506612068739));
#53578=CARTESIAN_POINT('Ctrl Pts',(-7.15998335064039,-2.02481148025317,
-0.730572647121488));
#53579=CARTESIAN_POINT('Ctrl Pts',(-7.04883700576296,-0.484190641641625,
-2.09741682691683));
#53580=CARTESIAN_POINT('Ctrl Pts',(-6.93769066088555,1.49967712384657,-1.54420414696323));
#53581=CARTESIAN_POINT('Ctrl Pts',(-6.82654431600811,2.11068217931116,0.422633010099142));
#53582=CARTESIAN_POINT('Ctrl Pts',(-6.7153979711307,0.789486756011834,2.0025754880576));
#53583=CARTESIAN_POINT('Ctrl Pts',(-6.60425162625327,-1.25443551972232,
1.74928255297597));
#53584=CARTESIAN_POINT('Ctrl Pts',(-6.49310528137585,-2.14999877885788,
-0.105371600522998));
#53585=CARTESIAN_POINT('Ctrl Pts',(-6.38195893649842,-1.07736961633439,
-1.86356449662648));
#53586=CARTESIAN_POINT('Ctrl Pts',(-6.270812591621,0.98152555482447,-1.9157780426014));
#53587=CARTESIAN_POINT('Ctrl Pts',(-6.15966624674358,2.14189409533265,-0.214213929673716));
#53588=CARTESIAN_POINT('Ctrl Pts',(-6.04851990186615,1.34148955639313,1.68344993788808));
#53589=CARTESIAN_POINT('Ctrl Pts',(-5.93737355698873,-0.686966646850282,
2.0400183208497));
#53590=CARTESIAN_POINT('Ctrl Pts',(-5.82622721211131,-2.08654688906569,
0.529074666769661));
#53591=CARTESIAN_POINT('Ctrl Pts',(-5.71508086723388,-1.57602103499908,
-1.46620449478496));
#53592=CARTESIAN_POINT('Ctrl Pts',(-5.60393452235647,0.37725571174863,-2.11926309155805));
#53593=CARTESIAN_POINT('Ctrl Pts',(-5.49278817747903,1.9851779214646,-0.832265909079935));
#53594=CARTESIAN_POINT('Ctrl Pts',(-5.38164183260162,1.77579112659265,1.21661982476122));
#53595=CARTESIAN_POINT('Ctrl Pts',(-5.27049548772418,-0.0592238649919277,
2.15176449852268));
#53596=CARTESIAN_POINT('Ctrl Pts',(-5.15934914284677,-1.84002302938406,
1.11710034223584));
#53597=CARTESIAN_POINT('Ctrl Pts',(-5.04820279796934,-1.93639361747923,
-0.940200872937754));
#53598=CARTESIAN_POINT('Ctrl Pts',(-4.93705645309191,-0.260114248398049,
-2.13680567695508));
#53599=CARTESIAN_POINT('Ctrl Pts',(-4.8259101082145,1.65428381056188,-1.37729553742109));
#53600=CARTESIAN_POINT('Ctrl Pts',(-4.71476376333707,2.05428619114345,0.643044452712678));
#53601=CARTESIAN_POINT('Ctrl Pts',(-4.60361741845965,0.573715171829774,
2.07471656495518));
#53602=CARTESIAN_POINT('Ctrl Pts',(-4.49247107358222,-1.43205700782412,
1.60711251928082));
#53603=CARTESIAN_POINT('Ctrl Pts',(-4.3813247287048,-2.12686855908149,-0.331704771864523));
#53604=CARTESIAN_POINT('Ctrl Pts',(-4.27017838382738,-0.874661990601799,
-1.96686662625693));
#53605=CARTESIAN_POINT('Ctrl Pts',(-4.15903203894995,1.17824414959146,-1.80148234719126));
#53606=CARTESIAN_POINT('Ctrl Pts',(-4.04788569407253,2.15253981386485,0.0130488701715242));
#53607=CARTESIAN_POINT('Ctrl Pts',(-3.9367393491951,1.15631689430128,1.8156346447562));
#53608=CARTESIAN_POINT('Ctrl Pts',(-3.82559300431768,-0.89844343969415,
1.95611791796024));
#53609=CARTESIAN_POINT('Ctrl Pts',(-3.71444665944026,-2.13073373943129,
0.305894842923001));
#53610=CARTESIAN_POINT('Ctrl Pts',(-3.60330031456283,-1.41246758316153,
-1.62435625704392));
#53611=CARTESIAN_POINT('Ctrl Pts',(-3.49215396968542,0.59882628102188,-2.06760852399429));
#53612=CARTESIAN_POINT('Ctrl Pts',(-3.38100762480798,2.06193129978027,-0.618091609875463));
#53613=CARTESIAN_POINT('Ctrl Pts',(-3.26986127993057,1.63746428918603,1.39725038017704));
#53614=CARTESIAN_POINT('Ctrl Pts',(-3.15871493505314,-0.286001156470349,
2.13349508134046));
#53615=CARTESIAN_POINT('Ctrl Pts',(-3.04756859017572,-1.94765003058781,
0.916655486572005));
#53616=CARTESIAN_POINT('Ctrl Pts',(-2.93642224529829,-1.8263443898979,-1.13932615734432));
#53617=CARTESIAN_POINT('Ctrl Pts',(-2.82527590042087,-0.0331321304115914,
-2.15232436849944));
#53618=CARTESIAN_POINT('Ctrl Pts',(-2.71412955554345,1.79041056752518,-1.19500122121443));
#53619=CARTESIAN_POINT('Ctrl Pts',(-2.60298321066602,1.97494186655942,0.856272473300212));
#53620=CARTESIAN_POINT('Ctrl Pts',(-2.4918368657886,0.351534639424466,2.12368108078498));
#53621=CARTESIAN_POINT('Ctrl Pts',(-2.38069052091118,-1.59368104817839,
1.44698949858494));
#53622=CARTESIAN_POINT('Ctrl Pts',(-2.26954417603376,-2.07997919520774,
-0.55433247252024));
#53623=CARTESIAN_POINT('Ctrl Pts',(-2.15839783115633,-0.662183540785041,
-2.04819700072118));
#53624=CARTESIAN_POINT('Ctrl Pts',(-2.0472514862789,1.36180060444583,-1.66706233186268));
#53625=CARTESIAN_POINT('Ctrl Pts',(-1.93610514140148,2.13913966163297,0.240165820636954));
#53626=CARTESIAN_POINT('Ctrl Pts',(-1.82495879652405,0.958226966987404,
1.92753713380078));
#53627=CARTESIAN_POINT('Ctrl Pts',(-1.71381245164664,-1.09988356808257,
1.85036551760173));
#53628=CARTESIAN_POINT('Ctrl Pts',(-1.60266610676921,-2.15111862857713,
0.0792984394831497));
#53629=CARTESIAN_POINT('Ctrl Pts',(-1.49151976189179,-1.23313481946782,
-1.76436347045422));
#53630=CARTESIAN_POINT('Ctrl Pts',(-1.38037341701436,0.813706056197659,
-1.9928547775867));
#53631=CARTESIAN_POINT('Ctrl Pts',(-1.26922707213695,2.11565347288727,-0.397016476196565));
#53632=CARTESIAN_POINT('Ctrl Pts',(-1.15808072725951,1.48084058983645,1.562279617094));
#53633=CARTESIAN_POINT('Ctrl Pts',(-1.04693438238209,-0.509574368188878,
2.0913785983932));
#53634=CARTESIAN_POINT('Ctrl Pts',(-0.935788037504666,-2.03353737199865,
0.705997133765736));
#53635=CARTESIAN_POINT('Ctrl Pts',(-0.824641692627246,-1.69585995945638,
-1.32577433553849));
#53636=CARTESIAN_POINT('Ctrl Pts',(-0.71349534774982,0.194156965638061,
-2.14370394685488));
#53637=CARTESIAN_POINT('Ctrl Pts',(-0.602349002872396,1.90665684596558,
-0.999539474359144));
#53638=CARTESIAN_POINT('Ctrl Pts',(-0.491202657994974,1.87330694072299,
1.06028137806503));
#53639=CARTESIAN_POINT('Ctrl Pts',(-0.38005631311755,0.125863161526222,
2.14826070212494));
#53640=CARTESIAN_POINT('Ctrl Pts',(-0.268909968240128,-1.7383416148007,
1.27198342040961));
#53641=CARTESIAN_POINT('Ctrl Pts',(-0.157763623362701,-2.00817094135109,
-0.773402904505074));
#53642=CARTESIAN_POINT('Ctrl Pts',(-0.0836660601110885,-0.966914112917088,
-1.65786295142018));
#53643=CARTESIAN_POINT('Ctrl Pts',(-0.0466172784852814,-0.374209849651548,
-1.78230609497963));
#53644=CARTESIAN_POINT('Ctrl Pts',(-29.646,-0.861525859670322,1.75382131162764));
#53645=CARTESIAN_POINT('Ctrl Pts',(-29.6089512183742,-1.44475753426074,
1.46732167423177));
#53646=CARTESIAN_POINT('Ctrl Pts',(-29.5348536551226,-2.29286652888411,
0.271744870419408));
#53647=CARTESIAN_POINT('Ctrl Pts',(-29.4237073102451,-1.47012297763525,
-1.78326461171051));
#53648=CARTESIAN_POINT('Ctrl Pts',(-29.3125609653677,0.700336273471097,
-2.2001292463347));
#53649=CARTESIAN_POINT('Ctrl Pts',(-29.2014146204903,2.22869993715502,-0.605756315417338));
#53650=CARTESIAN_POINT('Ctrl Pts',(-29.0902682756129,1.71733799299121,1.54462975010717));
#53651=CARTESIAN_POINT('Ctrl Pts',(-28.9791219307354,-0.366411226603099,
2.2802253866561));
#53652=CARTESIAN_POINT('Ctrl Pts',(-28.8679755858581,-2.11459180492753,
0.928822024838786));
#53653=CARTESIAN_POINT('Ctrl Pts',(-28.7568292409806,-1.92706730220025,
-1.27307553550754));
#53654=CARTESIAN_POINT('Ctrl Pts',(-28.6456828961032,0.0246086105193235,
-2.30943755856561));
#53655=CARTESIAN_POINT('Ctrl Pts',(-28.5345365512257,1.95373627660718,-1.23170996805708));
#53656=CARTESIAN_POINT('Ctrl Pts',(-28.4233902063484,2.09434865472725,0.973603941376282));
#53657=CARTESIAN_POINT('Ctrl Pts',(-28.3122438614709,0.317707212387436,
2.28762659388261));
#53658=CARTESIAN_POINT('Ctrl Pts',(-28.2010975165935,-1.74977276828138,
1.50747558605084));
#53659=CARTESIAN_POINT('Ctrl Pts',(-28.0899511717161,-2.21544433956327,
-0.652681674006207));
#53660=CARTESIAN_POINT('Ctrl Pts',(-27.9788048268387,-0.653011253992698,
-2.21534638945854));
#53661=CARTESIAN_POINT('Ctrl Pts',(-27.8676584819612,1.50721327238238,-1.74999819254223));
#53662=CARTESIAN_POINT('Ctrl Pts',(-27.7565121370838,2.28767643383428,0.317367004816054));
#53663=CARTESIAN_POINT('Ctrl Pts',(-27.6453657922064,0.973911578695988,
2.09420176868224));
#53664=CARTESIAN_POINT('Ctrl Pts',(-27.534219447329,-1.23140971440338,1.95392304382396));
#53665=CARTESIAN_POINT('Ctrl Pts',(-27.4230731024515,-2.3094507409455,0.0249471482242496));
#53666=CARTESIAN_POINT('Ctrl Pts',(-27.3119267575742,-1.27333080669325,
-1.92686628595169));
#53667=CARTESIAN_POINT('Ctrl Pts',(-27.2007804126966,0.928445614870621,
-2.1147514788365));
#53668=CARTESIAN_POINT('Ctrl Pts',(-27.0896340678193,2.28028685009023,-0.366710984170037));
#53669=CARTESIAN_POINT('Ctrl Pts',(-26.9784877229418,1.54466489828968,1.71703098688042));
#53670=CARTESIAN_POINT('Ctrl Pts',(-26.8673413780645,-0.605003318954584,
2.22893608010939));
#53671=CARTESIAN_POINT('Ctrl Pts',(-26.756195033187,-2.20082799096117,0.70038647693972));
#53672=CARTESIAN_POINT('Ctrl Pts',(-26.6450486883096,-1.78192920518164,
-1.46932412009659));
#53673=CARTESIAN_POINT('Ctrl Pts',(-26.5339023434321,0.268216812756021,
-2.29395832668387));
#53674=CARTESIAN_POINT('Ctrl Pts',(-26.4227559985547,2.07282673867339,-1.01861394760441));
#53675=CARTESIAN_POINT('Ctrl Pts',(-26.3116096536773,1.97989052702902,1.18920921781411));
#53676=CARTESIAN_POINT('Ctrl Pts',(-26.2004633087999,0.0744855971360473,
2.30838405788893));
#53677=CARTESIAN_POINT('Ctrl Pts',(-26.0893169639225,-1.89910634257262,
1.31437443768203));
#53678=CARTESIAN_POINT('Ctrl Pts',(-25.978170619045,-2.13418254536613,-0.882864613564002));
#53679=CARTESIAN_POINT('Ctrl Pts',(-25.8670242741676,-0.41554512119227,
-2.27189509333105));
#53680=CARTESIAN_POINT('Ctrl Pts',(-25.7558779292902,1.68349845317816,-1.58114452880967));
#53681=CARTESIAN_POINT('Ctrl Pts',(-25.6447315844128,2.24140213016567,0.557047173700168));
#53682=CARTESIAN_POINT('Ctrl Pts',(-25.5335852395353,0.747439206175521,
2.18529624900443));
#53683=CARTESIAN_POINT('Ctrl Pts',(-25.4224388946579,-1.43075860934684,
1.8130402269722));
#53684=CARTESIAN_POINT('Ctrl Pts',(-25.3112925497805,-2.29918440088871,
-0.218943265595743));
#53685=CARTESIAN_POINT('Ctrl Pts',(-25.2001462049031,-1.06284745566775,
-2.05049758566565));
#53686=CARTESIAN_POINT('Ctrl Pts',(-25.0889998600256,1.14646134804713,-2.00494674250309));
#53687=CARTESIAN_POINT('Ctrl Pts',(-24.9778535151482,2.30625488731607,-0.12398974784463));
#53688=CARTESIAN_POINT('Ctrl Pts',(-24.8667071702708,1.3548130918185,1.87047227968689));
#53689=CARTESIAN_POINT('Ctrl Pts',(-24.7555608253934,-0.8368772500053,2.15263130407031));
#53690=CARTESIAN_POINT('Ctrl Pts',(-24.6444144805159,-2.26245763980657,
0.464187990926873));
#53691=CARTESIAN_POINT('Ctrl Pts',(-24.5332681356385,-1.61689639697985,
-1.64919104541392));
#53692=CARTESIAN_POINT('Ctrl Pts',(-24.4221217907611,0.508834633121875,
-2.25283651847523));
#53693=CARTESIAN_POINT('Ctrl Pts',(-24.3109754458837,2.16875866898886,-0.794147907209686));
#53694=CARTESIAN_POINT('Ctrl Pts',(-24.1998291010062,1.84331675084411,1.39153455540902));
#53695=CARTESIAN_POINT('Ctrl Pts',(-24.0886827561289,-0.169568944201683,
2.30335221709625));
#53696=CARTESIAN_POINT('Ctrl Pts',(-23.9775364112514,-2.02722463902219,
1.10659176112116));
#53697=CARTESIAN_POINT('Ctrl Pts',(-23.866390066374,-2.02908013025209,-1.10318579027107));
#53698=CARTESIAN_POINT('Ctrl Pts',(-23.7552437214965,-0.173436829123328,
-2.30306420430337));
#53699=CARTESIAN_POINT('Ctrl Pts',(-23.6440973766192,1.84097728437699,-1.39462815877487));
#53700=CARTESIAN_POINT('Ctrl Pts',(-23.5329510317417,2.17008925948164,0.790504692410032));
#53701=CARTESIAN_POINT('Ctrl Pts',(-23.4218046868643,0.512617206336567,
2.25197883262866));
#53702=CARTESIAN_POINT('Ctrl Pts',(-23.3106583419869,-1.61412455553813,
1.65190404747029));
#53703=CARTESIAN_POINT('Ctrl Pts',(-23.1995119971095,-2.26323398149513,
-0.460387888465295));
#53704=CARTESIAN_POINT('Ctrl Pts',(-23.088365652232,-0.840491081477214,
-2.15122286265211));
#53705=CARTESIAN_POINT('Ctrl Pts',(-22.9772193073546,1.35167001231022,-1.87274484131212));
#53706=CARTESIAN_POINT('Ctrl Pts',(-22.8660729624772,2.30645985687955,0.120116574389448));
#53707=CARTESIAN_POINT('Ctrl Pts',(-22.7549266175997,1.14982672957971,2.00301861069334));
#53708=CARTESIAN_POINT('Ctrl Pts',(-22.6437802727223,-1.05940246318485,
2.05227958227862));
#53709=CARTESIAN_POINT('Ctrl Pts',(-22.5326339278449,-2.29881347743167,
0.222804081691522));
#53710=CARTESIAN_POINT('Ctrl Pts',(-22.4214875829675,-1.43380131266057,
-1.81063493246228));
#53711=CARTESIAN_POINT('Ctrl Pts',(-22.3103412380901,0.743768284930297,
-2.18654837613342));
#53712=CARTESIAN_POINT('Ctrl Pts',(-22.1991948932126,2.240463494933,-0.560810476642942));
#53713=CARTESIAN_POINT('Ctrl Pts',(-22.0880485483352,1.68615136712066,1.57831512379404));
#53714=CARTESIAN_POINT('Ctrl Pts',(-21.9769022034578,-0.411729238576987,
2.27258973352884));
#53715=CARTESIAN_POINT('Ctrl Pts',(-21.8657558585804,-2.13269690129466,
0.886447398353686));
#53716=CARTESIAN_POINT('Ctrl Pts',(-21.7546095137029,-1.90131095334948,
-1.31118332871995));
#53717=CARTESIAN_POINT('Ctrl Pts',(-21.6434631688255,0.070608917869684,
-2.30850588986841));
#53718=CARTESIAN_POINT('Ctrl Pts',(-21.5323168239481,1.97789064211908,-1.19253246104986));
#53719=CARTESIAN_POINT('Ctrl Pts',(-21.4211704790707,2.07453442044502,1.01513151917801));
#53720=CARTESIAN_POINT('Ctrl Pts',(-21.3100241341932,0.272068783015987,
2.29350466320609));
#53721=CARTESIAN_POINT('Ctrl Pts',(-21.1988777893159,-1.77945918978171,
1.47231452303552));
#53722=CARTESIAN_POINT('Ctrl Pts',(-21.0877314444384,-2.20200107829871,
-0.69668953918594));
#53723=CARTESIAN_POINT('Ctrl Pts',(-20.976585099561,-0.608745619668004,
-2.22791692694654));
#53724=CARTESIAN_POINT('Ctrl Pts',(-20.8654387546836,1.54177923238312,-1.71962259273132));
#53725=CARTESIAN_POINT('Ctrl Pts',(-20.7542924098061,2.28089946835357,0.362881079837752));
#53726=CARTESIAN_POINT('Ctrl Pts',(-20.6431460649287,0.931995705275805,
2.11318931196126));
#53727=CARTESIAN_POINT('Ctrl Pts',(-20.5319997200513,-1.27009313966377,
1.92900193867681));
#53728=CARTESIAN_POINT('Ctrl Pts',(-20.4208533751739,-2.30948937432413,
-0.0210687618001371));
#53729=CARTESIAN_POINT('Ctrl Pts',(-20.3097070302964,-1.23468929913284,
-1.95185229908585));
#53730=CARTESIAN_POINT('Ctrl Pts',(-20.198560685419,0.970393335078177,-2.09583440139618));
#53731=CARTESIAN_POINT('Ctrl Pts',(-20.0874143405416,2.28714020514337,-0.32120825776529));
#53732=CARTESIAN_POINT('Ctrl Pts',(-19.9762679956642,1.51015006321536,1.74746440576353));
#53733=CARTESIAN_POINT('Ctrl Pts',(-19.8651216507867,-0.649290124366777,
2.21644025347845));
#53734=CARTESIAN_POINT('Ctrl Pts',(-19.7539753059093,-2.21434490354622,
0.65640057204329));
#53735=CARTESIAN_POINT('Ctrl Pts',(-19.6428289610319,-1.75230231831962,
-1.50453369787837));
#53736=CARTESIAN_POINT('Ctrl Pts',(-19.5316826161545,0.313865895854717,
-2.28815936120261));
#53737=CARTESIAN_POINT('Ctrl Pts',(-19.420536271277,2.09270907351595,-0.97711503747712));
#53738=CARTESIAN_POINT('Ctrl Pts',(-19.3093899263996,1.95580505181399,1.22841835794599));
#53739=CARTESIAN_POINT('Ctrl Pts',(-19.1982435815222,0.028481091702752,
2.30940985757298));
#53740=CARTESIAN_POINT('Ctrl Pts',(-19.0870972366448,-1.9249155664031,1.27627784007202));
#53741=CARTESIAN_POINT('Ctrl Pts',(-18.9759508917673,-2.11616972127427,
-0.925208502772121));
#53742=CARTESIAN_POINT('Ctrl Pts',(-18.8648045468899,-0.370199888246757,
-2.27972303264715));
#53743=CARTESIAN_POINT('Ctrl Pts',(-18.7536582020125,1.71466530682062,-1.54729051843073));
#53744=CARTESIAN_POINT('Ctrl Pts',(-18.6425118571351,2.22985925567511,0.601591857258662));
#53745=CARTESIAN_POINT('Ctrl Pts',(-18.5313655122576,0.7037533993653,2.1997536716009));
#53746=CARTESIAN_POINT('Ctrl Pts',(-18.4202191673802,-1.46659566348409,
1.78417550221091));
#53747=CARTESIAN_POINT('Ctrl Pts',(-18.3090728225028,-2.29436607052567,
-0.264706247112593));
#53748=CARTESIAN_POINT('Ctrl Pts',(-18.1979264776254,-1.02178462763778,
-2.07126561250917));
#53749=CARTESIAN_POINT('Ctrl Pts',(-18.086780132748,1.18617816544452,-1.98170795594672));
#53750=CARTESIAN_POINT('Ctrl Pts',(-17.9756337878705,2.30826737621457,-0.0780178360589921));
#53751=CARTESIAN_POINT('Ctrl Pts',(-17.8644874429931,1.31727894168396,1.89709284238697));
#53752=CARTESIAN_POINT('Ctrl Pts',(-17.7533410981157,-0.879597819727813,
2.13553102023126));
#53753=CARTESIAN_POINT('Ctrl Pts',(-17.6421947532383,-2.27125655965968,
0.419021124816741));
#53754=CARTESIAN_POINT('Ctrl Pts',(-17.5310484083608,-1.58371879384272,
-1.68107698957223));
#53755=CARTESIAN_POINT('Ctrl Pts',(-17.4199020634834,0.553616692201852,
-2.24225190845172));
#53756=CARTESIAN_POINT('Ctrl Pts',(-17.308755718606,2.18414994709609,-0.75078230629124));
#53757=CARTESIAN_POINT('Ctrl Pts',(-17.1976093737286,1.8152274739619,1.42798259114521));
#53758=CARTESIAN_POINT('Ctrl Pts',(-17.0864630288511,-0.215424760589663,
2.29951673952697));
#53759=CARTESIAN_POINT('Ctrl Pts',(-16.9753166839737,-2.0488687988391,1.06598391544312));
#53760=CARTESIAN_POINT('Ctrl Pts',(-16.8641703390963,-2.00669872860475,
-1.14339200428198));
#53761=CARTESIAN_POINT('Ctrl Pts',(-16.7530239942189,-0.127518670722472,
-2.306062456105));
#53762=CARTESIAN_POINT('Ctrl Pts',(-16.6418776493414,1.8683969331536,-1.35767373216913));
#53763=CARTESIAN_POINT('Ctrl Pts',(-16.530731304464,2.15390938673701,0.833582279421827));
#53764=CARTESIAN_POINT('Ctrl Pts',(-16.4195849595866,0.467649496259791,
2.26174468309042));
#53765=CARTESIAN_POINT('Ctrl Pts',(-16.3084386147092,-1.6467149138954,1.61941812241135));
#53766=CARTESIAN_POINT('Ctrl Pts',(-16.1972922698318,-2.25361250777475,
-0.505386710985868));
#53767=CARTESIAN_POINT('Ctrl Pts',(-16.0861459249543,-0.797465646570921,
-2.16754091204274));
#53768=CARTESIAN_POINT('Ctrl Pts',(-15.9749995800769,1.38871225351008,-1.84544394111303));
#53769=CARTESIAN_POINT('Ctrl Pts',(-15.8638532351995,2.30360899748014,0.166044119343147));
#53770=CARTESIAN_POINT('Ctrl Pts',(-15.7527068903221,1.1096925570471,2.02552894120872));
#53771=CARTESIAN_POINT('Ctrl Pts',(-15.6415605454446,-1.10007956787695,
2.03076586714951));
#53772=CARTESIAN_POINT('Ctrl Pts',(-15.5304142005672,-2.30279611211481,
0.17696081167541));
#53773=CARTESIAN_POINT('Ctrl Pts',(-15.4192678556898,-1.39744361879813,
-1.83884104672487));
#53774=CARTESIAN_POINT('Ctrl Pts',(-15.3081215108124,0.787183061676606,
-2.17129636168103));
#53775=CARTESIAN_POINT('Ctrl Pts',(-15.1969751659349,2.25119178102243,-0.516062620131469));
#53776=CARTESIAN_POINT('Ctrl Pts',(-15.0858288210575,1.65437207261294,1.61159489580918));
#53777=CARTESIAN_POINT('Ctrl Pts',(-14.9746824761801,-0.45692411268592,
2.26393582463948));
#53778=CARTESIAN_POINT('Ctrl Pts',(-14.8635361313027,-2.14993421117156,
0.843781933009972));
#53779=CARTESIAN_POINT('Ctrl Pts',(-14.7523897864253,-1.87481099576699,
-1.34880272575014));
#53780=CARTESIAN_POINT('Ctrl Pts',(-14.6412434415478,0.116587052068778,
-2.30664096081938));
#53781=CARTESIAN_POINT('Ctrl Pts',(-14.5300970966704,2.00125678238095,-1.15289043443605));
#53782=CARTESIAN_POINT('Ctrl Pts',(-14.418950751793,2.05389829406855,1.05626079187961));
#53783=CARTESIAN_POINT('Ctrl Pts',(-14.3078044069156,0.226321501915263,
2.29846984766184));
#53784=CARTESIAN_POINT('Ctrl Pts',(-14.1966580620381,-1.80843878694902,
1.43657029646943));
#53785=CARTESIAN_POINT('Ctrl Pts',(-14.0855117171607,-2.18768394226603,
-0.740421522911927));
#53786=CARTESIAN_POINT('Ctrl Pts',(-13.9743653722833,-0.564238213060542,
-2.23960271069716));
#53787=CARTESIAN_POINT('Ctrl Pts',(-13.8632190274059,1.57573310019489,-1.68856455600315));
#53788=CARTESIAN_POINT('Ctrl Pts',(-13.7520726825284,2.27321710747686,0.408251203445124));
#53789=CARTESIAN_POINT('Ctrl Pts',(-13.640926337651,0.889709847359887,2.13133794841426));
#53790=CARTESIAN_POINT('Ctrl Pts',(-13.5297799927736,-1.30827237724028,
1.90331512099021));
#53791=CARTESIAN_POINT('Ctrl Pts',(-13.4186336478962,-2.3086112340065,-0.067076322639307));
#53792=CARTESIAN_POINT('Ctrl Pts',(-13.3074873030187,-1.19555766468852,
-1.97606349423402));
#53793=CARTESIAN_POINT('Ctrl Pts',(-13.1963409581413,1.01195584499574,-2.07608536207423));
#53794=CARTESIAN_POINT('Ctrl Pts',(-13.0851946132639,2.29308565401936,-0.275578021929272));
#53795=CARTESIAN_POINT('Ctrl Pts',(-12.9740482683865,1.47503575613473,1.7772041472391));
#53796=CARTESIAN_POINT('Ctrl Pts',(-12.862901923509,-0.693319186314957,
2.20306458569137));
#53797=CARTESIAN_POINT('Ctrl Pts',(-12.7517555786316,-2.22698280627896,
0.612154101005415));
#53798=CARTESIAN_POINT('Ctrl Pts',(-12.6406092337542,-1.72197983462208,
-1.53914603335576));
#53799=CARTESIAN_POINT('Ctrl Pts',(-12.5294628888768,0.359390386207514,
-2.28145208434048));
#53800=CARTESIAN_POINT('Ctrl Pts',(-12.4183165439994,2.11176068317365,-0.935228250130298));
#53801=CARTESIAN_POINT('Ctrl Pts',(-12.3071701991219,1.93094319703423,1.26713986310393));
#53802=CARTESIAN_POINT('Ctrl Pts',(-12.1960238542445,-0.0175347196268082,
2.30951891017318));
#53803=CARTESIAN_POINT('Ctrl Pts',(-12.0848775093671,-1.94996067261942,
1.23767460912692));
#53804=CARTESIAN_POINT('Ctrl Pts',(-11.9737311644897,-2.0973168590043,-0.967185119703648));
#53805=CARTESIAN_POINT('Ctrl Pts',(-11.8625848196123,-0.324707700151707,
-2.28664600939937));
#53806=CARTESIAN_POINT('Ctrl Pts',(-11.7514384747348,1.74515150413228,-1.51282229308821));
#53807=CARTESIAN_POINT('Ctrl Pts',(-11.6402921298574,2.21743121262479,0.645897731933769));
#53808=CARTESIAN_POINT('Ctrl Pts',(-11.52914578498,0.659788229460352,2.21333787639969));
#53809=CARTESIAN_POINT('Ctrl Pts',(-11.4179994401025,-1.50185053541965,
1.75460252823812));
#53810=CARTESIAN_POINT('Ctrl Pts',(-11.3068530952251,-2.28863696487281,
-0.31036415040662));
#53811=CARTESIAN_POINT('Ctrl Pts',(-11.1957067503477,-0.980316190318959,
-2.09121142638385));
#53812=CARTESIAN_POINT('Ctrl Pts',(-11.0845604054703,1.22542411562664,-1.95768250737462));
#53813=CARTESIAN_POINT('Ctrl Pts',(-10.9734140605928,2.30936357153834,-0.0320149541862179));
#53814=CARTESIAN_POINT('Ctrl Pts',(-10.8622677157154,1.27922188235666,1.92296033202449));
#53815=CARTESIAN_POINT('Ctrl Pts',(-10.751121370838,-0.921969222868076,
2.11758301252251));
#53816=CARTESIAN_POINT('Ctrl Pts',(-10.6399750259606,-2.27915387781204,
0.37368792339892));
#53817=CARTESIAN_POINT('Ctrl Pts',(-10.5288286810831,-1.54991251511545,
-1.71229561067251));
#53818=CARTESIAN_POINT('Ctrl Pts',(-10.4176823362058,0.598178986698543,
-2.23077721046101));
#53819=CARTESIAN_POINT('Ctrl Pts',(-10.3065359913283,2.19867420148525,-0.707118673606509));
#53820=CARTESIAN_POINT('Ctrl Pts',(-10.1953896464509,1.78641762142706,1.4638637725877));
#53821=CARTESIAN_POINT('Ctrl Pts',(-10.0842433015735,-0.261195061613987,
2.29476844204995));
#53822=CARTESIAN_POINT('Ctrl Pts',(-9.97309695669604,-2.06969963636276,
1.02495291505498));
#53823=CARTESIAN_POINT('Ctrl Pts',(-9.86195061181862,-1.98352074456387,
-1.18314433554179));
#53824=CARTESIAN_POINT('Ctrl Pts',(-9.7508042669412,-0.0815498923025786,
-2.30814528960058));
#53825=CARTESIAN_POINT('Ctrl Pts',(-9.63965792206376,1.8950749000425,-1.32018036118887));
#53826=CARTESIAN_POINT('Ctrl Pts',(-9.52851157718637,2.13687449461638,0.876328966255154));
#53827=CARTESIAN_POINT('Ctrl Pts',(-9.41736523230891,0.422496147277826,
2.27061270770145));
#53828=CARTESIAN_POINT('Ctrl Pts',(-9.30621888743152,-1.67865158962016,
1.58628935049869));
#53829=CARTESIAN_POINT('Ctrl Pts',(-9.19507254255407,-2.24309643636514,
-0.55018491437503));
#53830=CARTESIAN_POINT('Ctrl Pts',(-9.08392619767667,-0.754123648403588,
-2.18299853086491));
#53831=CARTESIAN_POINT('Ctrl Pts',(-8.97277985279923,1.42520322923344,-1.81741047048332));
#53832=CARTESIAN_POINT('Ctrl Pts',(-8.86163350792181,2.29984369370358,0.211905751152958));
#53833=CARTESIAN_POINT('Ctrl Pts',(-8.75048716304439,1.06911787915085,2.04723521445874));
#53834=CARTESIAN_POINT('Ctrl Pts',(-8.63934081816696,-1.14031998319325,
2.00844601589637));
#53835=CARTESIAN_POINT('Ctrl Pts',(-8.52819447328954,-2.3058646251051,0.131047295007472));
#53836=CARTESIAN_POINT('Ctrl Pts',(-8.41704812841211,-1.36053119344223,
-1.86631721165256));
#53837=CARTESIAN_POINT('Ctrl Pts',(-8.3059017835347,0.830285356953508,-2.15518242589077));
#53838=CARTESIAN_POINT('Ctrl Pts',(-8.19475543865726,2.26102643035827,-0.471109906562324));
#53839=CARTESIAN_POINT('Ctrl Pts',(-8.08360909377985,1.62193605587453,1.64423492649137));
#53840=CARTESIAN_POINT('Ctrl Pts',(-7.97246274890242,-0.50193760545539,
2.25438322010025));
#53841=CARTESIAN_POINT('Ctrl Pts',(-7.861316404025,-2.1663180796646,0.800781518616722));
#53842=CARTESIAN_POINT('Ctrl Pts',(-7.75017005914758,-1.84756681016008,
-1.38588669985493));
#53843=CARTESIAN_POINT('Ctrl Pts',(-7.63902371427016,0.162518905681942,
-2.30386038382012));
#53844=CARTESIAN_POINT('Ctrl Pts',(-7.52787736939272,2.02382850049311,-1.11279075455885));
#53845=CARTESIAN_POINT('Ctrl Pts',(-7.41673102451531,2.03244684888222,1.09697076957804));
#53846=CARTESIAN_POINT('Ctrl Pts',(-7.30558467963787,0.18048437986273,2.30252262778576));
#53847=CARTESIAN_POINT('Ctrl Pts',(-7.19443833476047,-1.83670050331195,
1.40025580662016));
#53848=CARTESIAN_POINT('Ctrl Pts',(-7.08329198988302,-2.1724983796548,-0.783859587705042));
#53849=CARTESIAN_POINT('Ctrl Pts',(-6.97214564500562,-0.519506825533608,
-2.25039945811047));
#53850=CARTESIAN_POINT('Ctrl Pts',(-6.86099930012817,1.60906146243046,-1.65683622394037));
#53851=CARTESIAN_POINT('Ctrl Pts',(-6.74985295525077,2.26463236663712,0.453459266990303));
#53852=CARTESIAN_POINT('Ctrl Pts',(-6.63870661037333,0.847070808774789,
2.14864052548618));
#53853=CARTESIAN_POINT('Ctrl Pts',(-6.52756026549592,-1.34593228088452,
1.87687276023519));
#53854=CARTESIAN_POINT('Ctrl Pts',(-6.41641392061849,-2.30681666361579,
-0.113057256752296));
#53855=CARTESIAN_POINT('Ctrl Pts',(-6.30526757574106,-1.15595143972763,
-1.9994902680012));
#53856=CARTESIAN_POINT('Ctrl Pts',(-6.19412123086365,1.05311664727397,-2.05551219652773));
#53857=CARTESIAN_POINT('Ctrl Pts',(-6.08297488598622,2.29812083588177,-0.229838392193094));
#53858=CARTESIAN_POINT('Ctrl Pts',(-5.97182854110879,1.43933591645946,1.80623840686375));
#53859=CARTESIAN_POINT('Ctrl Pts',(-5.86068219623138,-0.737073027150487,
2.18881438580046));
#53860=CARTESIAN_POINT('Ctrl Pts',(-5.74953585135395,-2.23873668229215,
0.5676646282792));
#53861=CARTESIAN_POINT('Ctrl Pts',(-5.63838950647653,-1.69097379100657,
-1.57314738691859));
#53862=CARTESIAN_POINT('Ctrl Pts',(-5.5272431615991,0.404772212367679,-2.27383915854548));
#53863=CARTESIAN_POINT('Ctrl Pts',(-5.41609681672169,2.12997400487336,-0.892970213055048));
#53864=CARTESIAN_POINT('Ctrl Pts',(-5.30495047184425,1.90531483190004,1.3053583623594));
#53865=CARTESIAN_POINT('Ctrl Pts',(-5.19380412696684,-0.0635435703455707,
2.30871117238765));
#53866=CARTESIAN_POINT('Ctrl Pts',(-5.0826577820894,-1.97423171927328,1.19858006885444));
#53867=CARTESIAN_POINT('Ctrl Pts',(-4.97151143721199,-2.07763144242026,
-1.00877780125587));
#53868=CARTESIAN_POINT('Ctrl Pts',(-4.86036509233456,-0.279086615559442,
-2.2926612754298));
#53869=CARTESIAN_POINT('Ctrl Pts',(-4.74921874745714,1.77494494326237,-1.47775353534586));
#53870=CARTESIAN_POINT('Ctrl Pts',(-4.63807240257972,2.20412293447108,0.689947209993967));
#53871=CARTESIAN_POINT('Ctrl Pts',(-4.52692605770229,0.615561148945878,
2.22604347099247));
#53872=CARTESIAN_POINT('Ctrl Pts',(-4.41577971282487,-1.53650923032218,
1.72433304438984));
#53873=CARTESIAN_POINT('Ctrl Pts',(-4.30463336794745,-2.28199935816521,
-0.355898851042403));
#53874=CARTESIAN_POINT('Ctrl Pts',(-4.19348702307002,-0.938458605089674,
-2.11032710956682));
#53875=CARTESIAN_POINT('Ctrl Pts',(-4.0823406781926,1.26418361945739,-1.93287993396815));
#53876=CARTESIAN_POINT('Ctrl Pts',(-3.97119433331517,2.3095430381396,0.0140006363953164));
#53877=CARTESIAN_POINT('Ctrl Pts',(-3.86004798843775,1.24065702102934,1.94806448019787));
#53878=CARTESIAN_POINT('Ctrl Pts',(-3.74890164356033,-0.96397463960601,
2.09879440561595));
#53879=CARTESIAN_POINT('Ctrl Pts',(-3.63775529868291,-2.28614645932942,
0.328206382211824));
#53880=CARTESIAN_POINT('Ctrl Pts',(-3.52660895380548,-1.51549098059717,
-1.74283451611452));
#53881=CARTESIAN_POINT('Ctrl Pts',(-3.41546260892806,0.642503827098123,
-2.21841697952858));
#53882=CARTESIAN_POINT('Ctrl Pts',(-3.30431626405063,2.21232566657125,-0.663174341921778));
#53883=CARTESIAN_POINT('Ctrl Pts',(-3.19316991917321,1.75689862967114,1.49916385624564));
#53884=CARTESIAN_POINT('Ctrl Pts',(-3.08202357429578,-0.306861678270252,
2.28910920963077));
#53885=CARTESIAN_POINT('Ctrl Pts',(-2.97087722941836,-2.08970888245738,
0.98351504754915));
#53886=CARTESIAN_POINT('Ctrl Pts',(-2.85973088454094,-1.95955537907592,
-1.22242700363369));
#53887=CARTESIAN_POINT('Ctrl Pts',(-2.74858453966352,-0.0355487413695248,
-2.30931187849249));
#53888=CARTESIAN_POINT('Ctrl Pts',(-2.63743819478609,1.92100059427707,-1.28216292829847));
#53889=CARTESIAN_POINT('Ctrl Pts',(-2.52629184990867,2.11899134653083,0.918727782279886));
#53890=CARTESIAN_POINT('Ctrl Pts',(-2.41514550503124,0.377175081231055,
2.27857938968823));
#53891=CARTESIAN_POINT('Ctrl Pts',(-2.30399916015382,-1.70992190069039,
1.55253087594118));
#53892=CARTESIAN_POINT('Ctrl Pts',(-2.1928528152764,-2.23168995008835,-0.594764702830417));
#53893=CARTESIAN_POINT('Ctrl Pts',(-2.08170647039897,-0.710482276211509,
-2.19758960707013));
#53894=CARTESIAN_POINT('Ctrl Pts',(-1.97056012552155,1.46112842376896,-1.78865551192071));
#53895=CARTESIAN_POINT('Ctrl Pts',(-1.85941378064413,2.29516549766495,0.257683177555444));
#53896=CARTESIAN_POINT('Ctrl Pts',(-1.7482674357667,1.02811869323325,2.06812897928806));
#53897=CARTESIAN_POINT('Ctrl Pts',(-1.63712109088928,-1.18010752742753,
1.98532857402419));
#53898=CARTESIAN_POINT('Ctrl Pts',(-1.52597474601185,-2.30801819359736,
0.0850823560446368));
#53899=CARTESIAN_POINT('Ctrl Pts',(-1.41482840113444,-1.32307793753456,
-1.89305365860764));
#53900=CARTESIAN_POINT('Ctrl Pts',(-1.303682056257,0.873056630627069,-2.13821080007561));
#53901=CARTESIAN_POINT('Ctrl Pts',(-1.19253571137959,2.2699662593695,-0.425974299160599));
#53902=CARTESIAN_POINT('Ctrl Pts',(-1.08138936650216,1.58885101814241,1.67623009342094));
#53903=CARTESIAN_POINT('Ctrl Pts',(-0.970243021624737,-0.546742005367173,
2.24392080969723));
#53904=CARTESIAN_POINT('Ctrl Pts',(-0.859096676747312,-2.18186072566234,
0.757491570995594));
#53905=CARTESIAN_POINT('Ctrl Pts',(-0.74795033186989,-1.81955359793778,
-1.42247444951531));
#53906=CARTESIAN_POINT('Ctrl Pts',(-0.636803986992465,0.208318501431441,
-2.30006269542661));
#53907=CARTESIAN_POINT('Ctrl Pts',(-0.525657642115041,2.04572571264764,
-1.07244447674439));
#53908=CARTESIAN_POINT('Ctrl Pts',(-0.414511297237619,2.00994331225735,
1.13761680941109));
#53909=CARTESIAN_POINT('Ctrl Pts',(-0.303364952360196,0.13504344337263,
2.30495181401234));
#53910=CARTESIAN_POINT('Ctrl Pts',(-0.192218607482772,-1.8651338054291,
1.36476010074876));
#53911=CARTESIAN_POINT('Ctrl Pts',(-0.0810722626053462,-2.15464410326713,
-0.829813823777627));
#53912=CARTESIAN_POINT('Ctrl Pts',(-0.00697469935373359,-1.03743946735969,
-1.77878514161715));
#53913=CARTESIAN_POINT('Ctrl Pts',(0.0300740822720735,-0.401504189376239,
-1.91230499291126));
#53914=CARTESIAN_POINT('Ctrl Pts',(-0.821869692124218,-1.95215209727744,
0.00149476428280041));
#53915=CARTESIAN_POINT('Ctrl Pts',(-0.797229905372775,-1.94905050159948,
-0.431580103628319));
#53916=CARTESIAN_POINT('Ctrl Pts',(-0.772590118621332,-1.80689620255586,
-0.8665002741731));
#53917=CARTESIAN_POINT('Ctrl Pts',(-0.747950331869889,-1.54195943599701,
-1.20541148708205));
#53918=CARTESIAN_POINT('Ctrl Pts',(-0.710901550244083,-1.14359623148139,
-1.71500386481906));
#53919=CARTESIAN_POINT('Ctrl Pts',(-0.673852768618274,-0.467638865024983,
-2.00753328012283));
#53920=CARTESIAN_POINT('Ctrl Pts',(-0.636803986992467,0.176574353405899,
-1.94919495132769));
#53921=CARTESIAN_POINT('Ctrl Pts',(-0.599755205366656,0.820787571836855,
-1.89085662253254));
#53922=CARTESIAN_POINT('Ctrl Pts',(-0.562706423740843,1.43325664224232,
-1.4816505496384));
#53923=CARTESIAN_POINT('Ctrl Pts',(-0.525657642115033,1.73352744404662,
-0.908703965498717));
#53924=CARTESIAN_POINT('Ctrl Pts',(-0.488608860489229,2.03379824585086,
-0.335757381359131));
#53925=CARTESIAN_POINT('Ctrl Pts',(-0.451560078863429,2.02187077905411,
0.400929714025867));
#53926=CARTESIAN_POINT('Ctrl Pts',(-0.414511297237625,1.703423734175,0.963829095818625));
#53927=CARTESIAN_POINT('Ctrl Pts',(-0.377462515611816,1.38497668929586,
1.52672847761145));
#53928=CARTESIAN_POINT('Ctrl Pts',(-0.340413733986006,0.760010066334254,
1.91584014581191));
#53929=CARTESIAN_POINT('Ctrl Pts',(-0.303364952360198,0.114163880053164,
1.95369736103487));
#53930=CARTESIAN_POINT('Ctrl Pts',(-0.268909968240138,-0.486466400236942,
1.98890418004745));
#53931=CARTESIAN_POINT('Ctrl Pts',(-0.234454984120076,-1.10515501358679,
1.72031777295108));
#53932=CARTESIAN_POINT('Ctrl Pts',(-0.200000000000016,-1.49578438409774,
1.26230645381953));
#53933=CARTESIAN_POINT('',(-29.646,-0.903606778650365,-1.26612599672272));
#53934=CARTESIAN_POINT('Ctrl Pts',(-29.646,-0.905547027071384,-1.26790990717737));
#53935=CARTESIAN_POINT('Ctrl Pts',(-29.646,-0.937793378787907,-1.25067033643914));
#53936=CARTESIAN_POINT('Ctrl Pts',(-29.646,-0.969330541631396,-1.23224815777297));
#53937=CARTESIAN_POINT('Ctrl Pts',(-29.646,-1.0000857755141,-1.212657994507));
#53938=CARTESIAN_POINT('Ctrl Pts',(-29.646,-1.05010530373861,-1.18079705245915));
#53939=CARTESIAN_POINT('Ctrl Pts',(-29.646,-1.09805783850725,-1.14584956138978));
#53940=CARTESIAN_POINT('Ctrl Pts',(-29.646,-1.14386498430002,-1.10813609735372));
#53941=CARTESIAN_POINT('Ctrl Pts',(-29.646,-1.17024530883727,-1.08641692224519));
#53942=CARTESIAN_POINT('Ctrl Pts',(-29.646,-1.19591382840587,-1.06377941838232));
#53943=CARTESIAN_POINT('Ctrl Pts',(-29.646,-1.22085272934429,-1.04027778754456));
#53944=CARTESIAN_POINT('Ctrl Pts',(-29.646,-1.23377538328808,-1.02809988751677));
#53945=CARTESIAN_POINT('Ctrl Pts',(-29.646,-1.24650526559313,-1.01568644027074));
#53946=CARTESIAN_POINT('Ctrl Pts',(-29.646,-1.25901907626856,-1.00306598282231));
#53947=CARTESIAN_POINT('Ctrl Pts',(-29.646,-1.30290144787354,-0.958809631344597));
#53948=CARTESIAN_POINT('Ctrl Pts',(-29.646,-1.34417543373733,-0.911969878856539));
#53949=CARTESIAN_POINT('Ctrl Pts',(-29.646,-1.38275268314532,-0.862895840586046));
#53950=CARTESIAN_POINT('Ctrl Pts',(-29.646,-1.41241940958756,-0.82515685993998));
#53951=CARTESIAN_POINT('Ctrl Pts',(-29.646,-1.44049103671116,-0.78609530729656));
#53952=CARTESIAN_POINT('Ctrl Pts',(-29.646,-1.46691729796725,-0.74585166902644));
#53953=CARTESIAN_POINT('Ctrl Pts',(-29.646,-1.47995477603729,-0.725997345090078));
#53954=CARTESIAN_POINT('Ctrl Pts',(-29.646,-1.49259162401709,-0.705855084298863));
#53955=CARTESIAN_POINT('Ctrl Pts',(-29.646,-1.50482081984275,-0.685440594208854));
#53956=CARTESIAN_POINT('Ctrl Pts',(-29.646,-1.51109469121476,-0.674967470155894));
#53957=CARTESIAN_POINT('Ctrl Pts',(-29.646,-1.51725645140333,-0.664430682827637));
#53958=CARTESIAN_POINT('Ctrl Pts',(-29.646,-1.52330452002809,-0.653834544117298));
#53959=CARTESIAN_POINT('Ctrl Pts',(-29.646,-1.55542245224318,-0.597564338543406));
#53960=CARTESIAN_POINT('Ctrl Pts',(-29.646,-1.58434610869271,-0.539607784254353));
#53961=CARTESIAN_POINT('Ctrl Pts',(-29.646,-1.60998192831617,-0.480318248615203));
#53962=CARTESIAN_POINT('Ctrl Pts',(-29.646,-1.63611509124052,-0.419878476557027));
#53963=CARTESIAN_POINT('Ctrl Pts',(-29.646,-1.65883236197299,-0.358052705230473));
#53964=CARTESIAN_POINT('Ctrl Pts',(-29.646,-1.67800021593047,-0.295174352807214));
#53965=CARTESIAN_POINT('Ctrl Pts',(-29.646,-1.69037848125595,-0.254568610961997));
#53966=CARTESIAN_POINT('Ctrl Pts',(-29.646,-1.70127578873751,-0.213523101715277));
#53967=CARTESIAN_POINT('Ctrl Pts',(-29.646,-1.71064650068833,-0.172121311687352));
#53968=CARTESIAN_POINT('Ctrl Pts',(-29.646,-1.71591839185181,-0.148828979989804));
#53969=CARTESIAN_POINT('Ctrl Pts',(-29.646,-1.72070695331894,-0.125423806591512));
#53970=CARTESIAN_POINT('Ctrl Pts',(-29.646,-1.72500283464754,-0.101920209121272));
#53971=CARTESIAN_POINT('Ctrl Pts',(-29.646,-1.7270982621959,-0.090455719798291));
#53972=CARTESIAN_POINT('Ctrl Pts',(-29.646,-1.7290767393725,-0.0789660350709723));
#53973=CARTESIAN_POINT('Ctrl Pts',(-29.646,-1.73093620036666,-0.0674584042143595));
#53974=CARTESIAN_POINT('Ctrl Pts',(-29.646,-1.74175324651588,-0.000515040285197679));
#53975=CARTESIAN_POINT('Ctrl Pts',(-29.646,-1.74850514784089,0.0667726732139331));
#53976=CARTESIAN_POINT('Ctrl Pts',(-29.646,-1.75107273016818,0.134046743031648));
#53977=CARTESIAN_POINT('Ctrl Pts',(-29.646,-1.7519840544883,0.15792465155534));
#53978=CARTESIAN_POINT('Ctrl Pts',(-29.646,-1.7523678650129,0.181801136382496));
#53979=CARTESIAN_POINT('Ctrl Pts',(-29.646,-1.75221749782202,0.205661030890043));
#53980=CARTESIAN_POINT('Ctrl Pts',(-29.646,-1.75180885673372,0.270503189618104));
#53981=CARTESIAN_POINT('Ctrl Pts',(-29.646,-1.74745894739069,0.335222160736237));
#53982=CARTESIAN_POINT('Ctrl Pts',(-29.646,-1.73938470553461,0.399582523654373));
#53983=CARTESIAN_POINT('Ctrl Pts',(-29.646,-1.73502774243432,0.43431219008673));
#53984=CARTESIAN_POINT('Ctrl Pts',(-29.646,-1.72958541924836,0.468937626840657));
#53985=CARTESIAN_POINT('Ctrl Pts',(-29.646,-1.72308572421693,0.503422468839529));
#53986=CARTESIAN_POINT('Ctrl Pts',(-29.646,-1.71847023632418,0.527910444038297));
#53987=CARTESIAN_POINT('Ctrl Pts',(-29.646,-1.71332147606747,0.552327531312746));
#53988=CARTESIAN_POINT('Ctrl Pts',(-29.646,-1.7076482220736,0.576660653491874));
#53989=CARTESIAN_POINT('Ctrl Pts',(-29.646,-1.70507942959174,0.587678447051176));
#53990=CARTESIAN_POINT('Ctrl Pts',(-29.646,-1.70240254021491,0.598681189081229));
#53991=CARTESIAN_POINT('Ctrl Pts',(-29.646,-1.69962009251516,0.609660631171463));
#53992=CARTESIAN_POINT('Ctrl Pts',(-29.646,-1.68299527966229,0.675261565915201));
#53993=CARTESIAN_POINT('Ctrl Pts',(-29.646,-1.66265693563362,0.739837446467255));
#53994=CARTESIAN_POINT('Ctrl Pts',(-29.646,-1.63886568474381,0.803133427680957));
#53995=CARTESIAN_POINT('Ctrl Pts',(-29.646,-1.61455213843445,0.867818961769251));
#53996=CARTESIAN_POINT('Ctrl Pts',(-29.646,-1.58663225844587,0.931168648803791));
#53997=CARTESIAN_POINT('Ctrl Pts',(-29.646,-1.55532888245165,0.992914874479613));
#53998=CARTESIAN_POINT('Ctrl Pts',(-29.646,-1.52373954286451,1.05522516623404));
#53999=CARTESIAN_POINT('Ctrl Pts',(-29.646,-1.48870429933303,1.11590354521734));
#54000=CARTESIAN_POINT('Ctrl Pts',(-29.646,-1.45040012878564,1.17466536929942));
#54001=CARTESIAN_POINT('Ctrl Pts',(-29.646,-1.43549335870293,1.19753361024327));
#54002=CARTESIAN_POINT('Ctrl Pts',(-29.646,-1.42009097480235,1.2201114031708));
#54003=CARTESIAN_POINT('Ctrl Pts',(-29.646,-1.40420146593038,1.24238107953945));
#54004=CARTESIAN_POINT('Ctrl Pts',(-29.646,-1.3981387582144,1.25087816650674));
#54005=CARTESIAN_POINT('Ctrl Pts',(-29.646,-1.39200638190649,1.25932854263738));
#54006=CARTESIAN_POINT('Ctrl Pts',(-29.646,-1.38581027364365,1.26772416536366));
#54007=CARTESIAN_POINT('Ctrl Pts',(-29.646,-1.34294092093917,1.32581141893628));
#54008=CARTESIAN_POINT('Ctrl Pts',(-29.646,-1.29695511274685,1.38137692796401));
#54009=CARTESIAN_POINT('Ctrl Pts',(-29.646,-1.24809388707593,1.43414001244329));
#54010=CARTESIAN_POINT('Ctrl Pts',(-29.646,-1.19912143132231,1.48702320938739));
#54011=CARTESIAN_POINT('Ctrl Pts',(-29.646,-1.14726001944392,1.53709221743024));
#54012=CARTESIAN_POINT('Ctrl Pts',(-29.646,-1.09270275532193,1.58404817835453));
#54013=CARTESIAN_POINT('Ctrl Pts',(-29.646,-1.03931253040024,1.62999970021889));
#54014=CARTESIAN_POINT('Ctrl Pts',(-29.646,-0.983339984605486,1.67297078948674));
#54015=CARTESIAN_POINT('Ctrl Pts',(-29.646,-0.924926350941029,1.71265217222693));
#54016=CARTESIAN_POINT('Ctrl Pts',(-29.646,-0.904101655375222,1.72679874492503));
#54017=CARTESIAN_POINT('Ctrl Pts',(-29.646,-0.882966376139423,1.74052687656736));
#54018=CARTESIAN_POINT('Ctrl Pts',(-29.646,-0.861525859670494,1.75382131162756));
#54019=CARTESIAN_POINT('Ctrl Pts',(-29.646,-0.90554702707136,-1.26790990717739));
#54020=CARTESIAN_POINT('Ctrl Pts',(-29.6115450158799,-0.514141345293391,
-1.54438147758941));
#54021=CARTESIAN_POINT('Ctrl Pts',(-29.5400412501341,0.585902364535579,
-1.72181409200425));
#54022=CARTESIAN_POINT('Ctrl Pts',(-29.4314887027624,1.77417745764817,-0.482217988040945));
#54023=CARTESIAN_POINT('Ctrl Pts',(-29.320342357885,1.36710299288539,1.22961697865478));
#54024=CARTESIAN_POINT('Ctrl Pts',(-29.2091960130075,-0.291685088526501,
1.81519477428025));
#54025=CARTESIAN_POINT('Ctrl Pts',(-29.1197298185113,-1.41188498103577,
0.949241954866662));
#54026=CARTESIAN_POINT('Ctrl Pts',(-29.0673124056409,-1.554112608544,0.216012872988254));
#54027=CARTESIAN_POINT('Ctrl Pts',(-29.0519437743963,-1.55324480116087,
0.00070803006655188));
#54028=CARTESIAN_POINT('Origin',(-29.646,-2.59090492670967E-16,0.));
#54029=CARTESIAN_POINT('',(-29.646,-1.954,-2.39295984553393E-16));
#54030=CARTESIAN_POINT('Origin',(-29.646,0.,0.));
#54031=CARTESIAN_POINT('Origin',(-29.646,0.,0.));
#54032=CARTESIAN_POINT('',(-29.646,0.903606778650208,-1.26612599672284));
#54033=CARTESIAN_POINT('Ctrl Pts',(-29.646,0.863566668009735,1.75642846275435));
#54034=CARTESIAN_POINT('Ctrl Pts',(-29.646,0.902259155469474,1.73266520248623));
#54035=CARTESIAN_POINT('Ctrl Pts',(-29.646,0.940006532226865,1.70749215717109));
#54036=CARTESIAN_POINT('Ctrl Pts',(-29.646,0.976720689600575,1.68090467162269));
#54037=CARTESIAN_POINT('Ctrl Pts',(-29.646,1.0349027939429,1.63877062936124));
#54038=CARTESIAN_POINT('Ctrl Pts',(-29.646,1.09049234196888,1.59308558101157));
#54039=CARTESIAN_POINT('Ctrl Pts',(-29.646,1.14332803524928,1.54419031207811));
#54040=CARTESIAN_POINT('Ctrl Pts',(-29.646,1.16845341136095,1.52093875719617));
#54041=CARTESIAN_POINT('Ctrl Pts',(-29.646,1.19295541948053,1.49696080557489));
#54042=CARTESIAN_POINT('Ctrl Pts',(-29.646,1.21681313452585,1.47229119208527));
#54043=CARTESIAN_POINT('Ctrl Pts',(-29.646,1.2292556555639,1.45942524141639));
#54044=CARTESIAN_POINT('Ctrl Pts',(-29.646,1.24152289307511,1.44637114719752));
#54045=CARTESIAN_POINT('Ctrl Pts',(-29.646,1.25361161098408,1.43313375371991));
#54046=CARTESIAN_POINT('Ctrl Pts',(-29.646,1.26358724145162,1.42221023423005));
#54047=CARTESIAN_POINT('Ctrl Pts',(-29.646,1.27343483093232,1.41116895221076));
#54048=CARTESIAN_POINT('Ctrl Pts',(-29.646,1.28315121238943,1.40001516631078));
#54049=CARTESIAN_POINT('Ctrl Pts',(-29.646,1.3300441200689,1.34618510058174));
#54050=CARTESIAN_POINT('Ctrl Pts',(-29.646,1.37389955022329,1.28972022694498));
#54051=CARTESIAN_POINT('Ctrl Pts',(-29.646,1.41455393311167,1.23095477641172));
#54052=CARTESIAN_POINT('Ctrl Pts',(-29.646,1.44358986833681,1.18898366053364));
#54053=CARTESIAN_POINT('Ctrl Pts',(-29.646,1.47099202754879,1.1458383448938));
#54054=CARTESIAN_POINT('Ctrl Pts',(-29.646,1.49668525991621,1.10163578501629));
#54055=CARTESIAN_POINT('Ctrl Pts',(-29.646,1.51149551265388,1.07615627064161));
#54056=CARTESIAN_POINT('Ctrl Pts',(-29.646,1.52573769742341,1.05032541750307));
#54057=CARTESIAN_POINT('Ctrl Pts',(-29.646,1.53939530583147,1.02416547210538));
#54058=CARTESIAN_POINT('Ctrl Pts',(-29.646,1.54521957948012,1.01300958916617));
#54059=CARTESIAN_POINT('Ctrl Pts',(-29.646,1.55093325590683,1.0018019983193));
#54060=CARTESIAN_POINT('Ctrl Pts',(-29.646,1.55653443638647,0.990546796296277));
#54061=CARTESIAN_POINT('Ctrl Pts',(-29.646,1.58755327688888,0.928216486169085));
#54062=CARTESIAN_POINT('Ctrl Pts',(-29.646,1.6151376920719,0.864404941366738));
#54063=CARTESIAN_POINT('Ctrl Pts',(-29.646,1.6391334354648,0.799420358132647));
#54064=CARTESIAN_POINT('Ctrl Pts',(-29.646,1.66253760074651,0.736037869752487));
#54065=CARTESIAN_POINT('Ctrl Pts',(-29.646,1.68252795024664,0.671538496957767));
#54066=CARTESIAN_POINT('Ctrl Pts',(-29.646,1.69891301949968,0.606203195144271));
#54067=CARTESIAN_POINT('Ctrl Pts',(-29.646,1.70967608762625,0.563285567294857));
#54068=CARTESIAN_POINT('Ctrl Pts',(-29.646,1.71888251024604,0.520007171308568));
#54069=CARTESIAN_POINT('Ctrl Pts',(-29.646,1.72646591175805,0.47644935798757));
#54070=CARTESIAN_POINT('Ctrl Pts',(-29.646,1.73282394033038,0.439929885663143));
#54071=CARTESIAN_POINT('Ctrl Pts',(-29.646,1.73804092762139,0.403213996643961));
#54072=CARTESIAN_POINT('Ctrl Pts',(-29.646,1.74207225008614,0.366351346889232));
#54073=CARTESIAN_POINT('Ctrl Pts',(-29.646,1.74334867076358,0.354679681130935));
#54074=CARTESIAN_POINT('Ctrl Pts',(-29.646,1.74450615115825,0.342992647905779));
#54075=CARTESIAN_POINT('Ctrl Pts',(-29.646,1.74554204935843,0.331307707853706));
#54076=CARTESIAN_POINT('Ctrl Pts',(-29.646,1.7512962238706,0.266400572951581));
#54077=CARTESIAN_POINT('Ctrl Pts',(-29.646,1.75331678834241,0.20144064594388));
#54078=CARTESIAN_POINT('Ctrl Pts',(-29.646,1.7514364731807,0.136688241949958));
#54079=CARTESIAN_POINT('Ctrl Pts',(-29.646,1.75089895462669,0.1181777181439));
#54080=CARTESIAN_POINT('Ctrl Pts',(-29.646,1.7500423376016,0.0996841942035913));
#54081=CARTESIAN_POINT('Ctrl Pts',(-29.646,1.74886193315568,0.0812138946393991));
#54082=CARTESIAN_POINT('Ctrl Pts',(-29.646,1.7444812283952,0.0126671100964298));
#54083=CARTESIAN_POINT('Ctrl Pts',(-29.646,1.73564516145986,-0.0555619386623527));
#54084=CARTESIAN_POINT('Ctrl Pts',(-29.646,1.72254696331046,-0.123135794734825));
#54085=CARTESIAN_POINT('Ctrl Pts',(-29.646,1.7107923019786,-0.183778318535385));
#54086=CARTESIAN_POINT('Ctrl Pts',(-29.646,1.69560382797953,-0.243893450349329));
#54087=CARTESIAN_POINT('Ctrl Pts',(-29.646,1.67708883824234,-0.303212355847263));
#54088=CARTESIAN_POINT('Ctrl Pts',(-29.646,1.67396734919769,-0.313213080464503));
#54089=CARTESIAN_POINT('Ctrl Pts',(-29.646,1.67075231970824,-0.32318750802379));
#54090=CARTESIAN_POINT('Ctrl Pts',(-29.646,1.66744711192406,-0.333126627485946));
#54091=CARTESIAN_POINT('Ctrl Pts',(-29.646,1.64699549224018,-0.394626873311822));
#54092=CARTESIAN_POINT('Ctrl Pts',(-29.646,1.62306700922488,-0.454867564271816));
#54093=CARTESIAN_POINT('Ctrl Pts',(-29.646,1.59584883350397,-0.513575166957551));
#54094=CARTESIAN_POINT('Ctrl Pts',(-29.646,1.56873097546522,-0.572066391782911));
#54095=CARTESIAN_POINT('Ctrl Pts',(-29.646,1.53834687411596,-0.629036647008692));
#54096=CARTESIAN_POINT('Ctrl Pts',(-29.646,1.50484185692085,-0.684183082745647));
#54097=CARTESIAN_POINT('Ctrl Pts',(-29.646,1.47201694913541,-0.738210115688802));
#54098=CARTESIAN_POINT('Ctrl Pts',(-29.646,1.43619579268168,-0.790487244163948));
#54099=CARTESIAN_POINT('Ctrl Pts',(-29.646,1.39748800398724,-0.840688000782997));
#54100=CARTESIAN_POINT('Ctrl Pts',(-29.646,1.39006351372884,-0.850316942168009));
#54101=CARTESIAN_POINT('Ctrl Pts',(-29.646,1.38253276005615,-0.859869351508118));
#54102=CARTESIAN_POINT('Ctrl Pts',(-29.646,1.37489643439059,-0.869342715932));
#54103=CARTESIAN_POINT('Ctrl Pts',(-29.646,1.36836089236766,-0.877450485820595));
#54104=CARTESIAN_POINT('Ctrl Pts',(-29.646,1.36175071282073,-0.885496939562918));
#54105=CARTESIAN_POINT('Ctrl Pts',(-29.646,1.35507157412216,-0.893474782751297));
#54106=CARTESIAN_POINT('Ctrl Pts',(-29.646,1.31523219178395,-0.941060610709032));
#54107=CARTESIAN_POINT('Ctrl Pts',(-29.646,1.27288888818335,-0.986274661689286));
#54108=CARTESIAN_POINT('Ctrl Pts',(-29.646,1.22818063142926,-1.02884993242326));
#54109=CARTESIAN_POINT('Ctrl Pts',(-29.646,1.18427440391157,-1.07066143793007));
#54110=CARTESIAN_POINT('Ctrl Pts',(-29.646,1.13808660486174,-1.10992852640867));
#54111=CARTESIAN_POINT('Ctrl Pts',(-29.646,1.08972540441639,-1.14635444573824));
#54112=CARTESIAN_POINT('Ctrl Pts',(-29.646,1.04290945083493,-1.18161647672157));
#54113=CARTESIAN_POINT('Ctrl Pts',(-29.646,0.994056159108196,-1.21421629893641));
#54114=CARTESIAN_POINT('Ctrl Pts',(-29.646,0.94325105145388,-1.24383738917956));
#54115=CARTESIAN_POINT('Ctrl Pts',(-29.646,0.930165355350817,-1.25146679108538));
#54116=CARTESIAN_POINT('Ctrl Pts',(-29.646,0.916950133464095,-1.2588983186305));
#54117=CARTESIAN_POINT('Ctrl Pts',(-29.646,0.903606778650087,-1.26612599672292));
#54118=CARTESIAN_POINT('Origin',(-29.646,0.,0.));
#54119=CARTESIAN_POINT('Origin',(-30.9400562256037,0.,0.));
#54120=CARTESIAN_POINT('Ctrl Pts',(-29.646,0.903606778650087,-1.26612599672292));
#54121=CARTESIAN_POINT('Ctrl Pts',(-29.6089512183742,1.32465582191086,-0.965632388172658));
#54122=CARTESIAN_POINT('Ctrl Pts',(-29.5348536551225,1.83614857151059,0.0831884196457774));
#54123=CARTESIAN_POINT('Ctrl Pts',(-29.4237073102452,0.924038956922092,
1.59090722470862));
#54124=CARTESIAN_POINT('Ctrl Pts',(-29.3125609653677,-0.83473688776688,
1.63754421834404));
#54125=CARTESIAN_POINT('Ctrl Pts',(-29.2346772704873,-1.53141980147719,
0.621433224781769));
#54126=CARTESIAN_POINT('Ctrl Pts',(-29.1938423572326,-1.55773945610431,
0.0536831291795148));
#54127=CARTESIAN_POINT('Ctrl Pts',(-29.1900562256037,-1.55737653422887,
0.00100621910560853));
#54128=CARTESIAN_POINT('Ctrl Pts',(-29.8760740822721,1.13509973994375,-1.59049193030949));
#54129=CARTESIAN_POINT('Ctrl Pts',(-29.8390253006463,1.6640163780225,-1.21301554901262));
#54130=CARTESIAN_POINT('Ctrl Pts',(-29.7649277373946,2.30654728944499,0.104500271287817));
#54131=CARTESIAN_POINT('Ctrl Pts',(-29.6537813925172,1.16076639140178,1.99847812091342));
#54132=CARTESIAN_POINT('Ctrl Pts',(-29.5426350476398,-1.04858622867039,
2.05706293966191));
#54133=CARTESIAN_POINT('Ctrl Pts',(-29.4314887027624,-2.29751693097514,
0.235499367719248));
#54134=CARTESIAN_POINT('Ctrl Pts',(-29.320342357885,-1.44347707856157,-1.80319291664826));
#54135=CARTESIAN_POINT('Ctrl Pts',(-29.2091960130075,0.732117470005603,
-2.19036286313464));
#54136=CARTESIAN_POINT('Ctrl Pts',(-29.0980496681301,2.23742980466302,-0.572814850018687));
#54137=CARTESIAN_POINT('Ctrl Pts',(-28.9869033232526,1.69455056349597,1.56933369051493));
#54138=CARTESIAN_POINT('Ctrl Pts',(-28.8757569783753,-0.399606399986678,
2.27473567517142));
#54139=CARTESIAN_POINT('Ctrl Pts',(-28.7646106334978,-2.12793746980263,
0.897818014163103));
#54140=CARTESIAN_POINT('Ctrl Pts',(-28.6534642886204,-1.90827750560971,
-1.30102961800398));
#54141=CARTESIAN_POINT('Ctrl Pts',(-28.542317943743,0.0582967826181247,
-2.30884711344785));
#54142=CARTESIAN_POINT('Ctrl Pts',(-28.4311715988656,1.97150238108163,-1.20306522421591));
#54143=CARTESIAN_POINT('Ctrl Pts',(-28.3200252539881,2.07991891070671,1.00405403493572));
#54144=CARTESIAN_POINT('Ctrl Pts',(-28.2088789091107,0.284296424689126,
2.29202073726512));
#54145=CARTESIAN_POINT('Ctrl Pts',(-28.0977325642333,-1.7715818298528,1.48178390263166));
#54146=CARTESIAN_POINT('Ctrl Pts',(-27.9865862193559,-2.20568535982826,
-0.684936177450616));
#54147=CARTESIAN_POINT('Ctrl Pts',(-27.8754398744784,-0.620618745970624,
-2.22463870679357));
#54148=CARTESIAN_POINT('Ctrl Pts',(-27.764293529601,1.53258634975486,-1.72782071366884));
#54149=CARTESIAN_POINT('Ctrl Pts',(-27.6531471847236,2.28280236854648,0.350711595825784));
#54150=CARTESIAN_POINT('Ctrl Pts',(-27.5420008398461,0.94325239047631,2.10818883105081));
#54151=CARTESIAN_POINT('Ctrl Pts',(-27.4308544949688,-1.25978747172194,
1.93574812290515));
#54152=CARTESIAN_POINT('Ctrl Pts',(-27.3197081500913,-2.30956893500566,
-0.00875164606705387));
#54153=CARTESIAN_POINT('Ctrl Pts',(-27.2085618052139,-1.24508125418542,
-1.94523981057524));
#54154=CARTESIAN_POINT('Ctrl Pts',(-27.0974154603365,0.959202184405071,
-2.1009798730201));
#54155=CARTESIAN_POINT('Ctrl Pts',(-26.986269115459,2.28539467337763,-0.333401322767505));
#54156=CARTESIAN_POINT('Ctrl Pts',(-26.8751227705816,1.51944807776828,1.73938575175027));
#54157=CARTESIAN_POINT('Ctrl Pts',(-26.7639764257042,-0.637460327196598,
2.21987152481952));
#54158=CARTESIAN_POINT('Ctrl Pts',(-26.6528300808268,-2.21081277979495,
0.668200649323706));
#54159=CARTESIAN_POINT('Ctrl Pts',(-26.5416837359493,-1.76030131128423,
-1.4951670637397));
#54160=CARTESIAN_POINT('Ctrl Pts',(-26.430537391072,0.301658375125117,-2.28980075112679));
#54161=CARTESIAN_POINT('Ctrl Pts',(-26.3193910461945,2.08746826383544,-0.988261859306003));
#54162=CARTESIAN_POINT('Ctrl Pts',(-26.2082447013171,1.9623285939949,1.21797033800769));
#54163=CARTESIAN_POINT('Ctrl Pts',(-26.0970983564397,0.0407970817586391,
2.30922516295313));
#54164=CARTESIAN_POINT('Ctrl Pts',(-25.9859520115622,-1.91808166431569,
1.2865255473956));
#54165=CARTESIAN_POINT('Ctrl Pts',(-25.8748056666848,-2.12107392666094,
-0.913909542966534));
#54166=CARTESIAN_POINT('Ctrl Pts',(-25.7636593218074,-0.382352700941006,
-2.27771632719524));
#54167=CARTESIAN_POINT('Ctrl Pts',(-25.65251297693,1.70638904376409,-1.55641308347398));
#54168=CARTESIAN_POINT('Ctrl Pts',(-25.5413666320525,2.23303595503733,0.589691172223087));
#54169=CARTESIAN_POINT('Ctrl Pts',(-25.4302202871751,0.715474987117585,
2.19596921606308));
#54170=CARTESIAN_POINT('Ctrl Pts',(-25.3190739422977,-1.45705958421952,
1.79197171381733));
#54171=CARTESIAN_POINT('Ctrl Pts',(-25.2079275974203,-2.29574519723769,
-0.252466323392859));
#54172=CARTESIAN_POINT('Ctrl Pts',(-25.0967812525429,-1.0328164541474,-2.06578687843878));
#54173=CARTESIAN_POINT('Ctrl Pts',(-24.9856349076654,1.17559260177244,-1.9880058575732));
#54174=CARTESIAN_POINT('Ctrl Pts',(-24.874488562788,2.30781851167389,-0.0903270295247155));
#54175=CARTESIAN_POINT('Ctrl Pts',(-24.7633422179106,1.3273776843161,1.89004067106162));
#54176=CARTESIAN_POINT('Ctrl Pts',(-24.6521958730331,-0.868196251320992,
2.14019170269385));
#54177=CARTESIAN_POINT('Ctrl Pts',(-24.5410495281557,-2.26898960421259,
0.431128091247411));
#54178=CARTESIAN_POINT('Ctrl Pts',(-24.4299031832783,-1.59266171045552,
-1.67260692666757));
#54179=CARTESIAN_POINT('Ctrl Pts',(-24.3187568384009,0.541650596878888,
-2.24517257376536));
#54180=CARTESIAN_POINT('Ctrl Pts',(-24.2076104935235,2.18011490167143,-0.762420009310885));
#54181=CARTESIAN_POINT('Ctrl Pts',(-24.096464148646,1.82281731580137,1.41828145595369));
#54182=CARTESIAN_POINT('Ctrl Pts',(-23.9853178037686,-0.203158067613754,
2.30063296826132));
#54183=CARTESIAN_POINT('Ctrl Pts',(-23.8741714588912,-2.04315466210664,
1.07689566894818));
#54184=CARTESIAN_POINT('Ctrl Pts',(-23.7630251140138,-2.01276809090682,
-1.13267376914748));
#54185=CARTESIAN_POINT('Ctrl Pts',(-23.6518787691364,-0.139815401979066,
-2.30534962824663));
#54186=CARTESIAN_POINT('Ctrl Pts',(-23.5407324242589,1.86112973853166,-1.3676188619058));
#54187=CARTESIAN_POINT('Ctrl Pts',(-23.4295860793815,2.15832440107783,0.822083350275042));
#54188=CARTESIAN_POINT('Ctrl Pts',(-23.3184397345041,0.479705043887776,
2.25921852107228));
#54189=CARTESIAN_POINT('Ctrl Pts',(-23.2072933896267,-1.63805494970446,
1.62817727438881));
#54190=CARTESIAN_POINT('Ctrl Pts',(-23.0961470447492,-2.25627579472933,
-0.493360713075091));
#54191=CARTESIAN_POINT('Ctrl Pts',(-22.9850006998718,-0.809014108309205,
-2.16325713396352));
#54192=CARTESIAN_POINT('Ctrl Pts',(-22.8738543549944,1.37885052758575,-1.85282391976786));
#54193=CARTESIAN_POINT('Ctrl Pts',(-22.762708010117,2.30446181446416,0.153756303168402));
#54194=CARTESIAN_POINT('Ctrl Pts',(-22.6515616652395,1.12047921513559,2.01958203189089));
#54195=CARTESIAN_POINT('Ctrl Pts',(-22.5404153203621,-1.08923359462026,
2.03660389654887));
#54196=CARTESIAN_POINT('Ctrl Pts',(-22.4292689754847,-2.30181964903589,
0.189239420839657));
#54197=CARTESIAN_POINT('Ctrl Pts',(-22.3181226306073,-1.4072305581405,-1.83136217371742));
#54198=CARTESIAN_POINT('Ctrl Pts',(-22.2069762857299,0.775592064464368,
-2.17546367577749));
#54199=CARTESIAN_POINT('Ctrl Pts',(-22.0958299408524,2.24840757516354,-0.528061200084454));
#54200=CARTESIAN_POINT('Ctrl Pts',(-21.984683595975,1.66294342833263,1.60274901630066));
#54201=CARTESIAN_POINT('Ctrl Pts',(-21.8735372510976,-0.444843747458639,
2.26634050738947));
#54202=CARTESIAN_POINT('Ctrl Pts',(-21.7623909062202,-2.14540367215556,
0.855235837993748));
#54203=CARTESIAN_POINT('Ctrl Pts',(-21.6512445613427,-1.88197771441436,
-1.33878494820309));
#54204=CARTESIAN_POINT('Ctrl Pts',(-21.5400982164654,0.104283768475023,
-2.30722997352238));
#54205=CARTESIAN_POINT('Ctrl Pts',(-21.4289518715878,1.99507983769398,-1.16354703227434));
#54206=CARTESIAN_POINT('Ctrl Pts',(-21.3178055267105,2.05950230346372,1.04529207263571));
#54207=CARTESIAN_POINT('Ctrl Pts',(-21.206659181833,0.238576337445077,2.29723019880436));
#54208=CARTESIAN_POINT('Ctrl Pts',(-21.0955128369556,-1.80075167789753,
1.4461945407298));
#54209=CARTESIAN_POINT('Ctrl Pts',(-20.9843664920782,-2.19160163800585,
-0.728743792685421));
#54210=CARTESIAN_POINT('Ctrl Pts',(-20.8732201472008,-0.576174302687003,
-2.23656174249909));
#54211=CARTESIAN_POINT('Ctrl Pts',(-20.7620738023233,1.56670537690975,-1.69694417028066));
#54212=CARTESIAN_POINT('Ctrl Pts',(-20.6509274574459,2.27536207920589,0.396122031196596));
#54213=CARTESIAN_POINT('Ctrl Pts',(-20.5397811125685,0.901063923638144,
2.12656273375728));
#54214=CARTESIAN_POINT('Ctrl Pts',(-20.4286347676911,-1.29810315900734,
1.91026528096561));
#54215=CARTESIAN_POINT('Ctrl Pts',(-20.3174884228136,-2.3089361713204,-0.0547632345256441));
#54216=CARTESIAN_POINT('Ctrl Pts',(-20.2063420779362,-1.20607929730647,
-1.96965935727377));
#54217=CARTESIAN_POINT('Ctrl Pts',(-20.0951957330588,1.00086942839655,-2.08145277207738));
#54218=CARTESIAN_POINT('Ctrl Pts',(-19.9840493881814,2.2915833899632,-0.287803443225016));
#54219=CARTESIAN_POINT('Ctrl Pts',(-19.872903043304,1.48449287550998,1.76931234033099));
#54220=CARTESIAN_POINT('Ctrl Pts',(-19.7617566984265,-0.681560098046438,
2.20673085985544));
#54221=CARTESIAN_POINT('Ctrl Pts',(-19.6506103535491,-2.22368647542462,
0.624022206416638));
#54222=CARTESIAN_POINT('Ctrl Pts',(-19.5394640086717,-1.73016385052689,
-1.52994062153321));
#54223=CARTESIAN_POINT('Ctrl Pts',(-19.4283176637943,0.347217989697661,
-2.28333635777074));
#54224=CARTESIAN_POINT('Ctrl Pts',(-19.3171713189168,2.10674299078965,-0.946477271700759));
#54225=CARTESIAN_POINT('Ctrl Pts',(-19.2060249740394,1.93767359934984,1.25682388482638));
#54226=CARTESIAN_POINT('Ctrl Pts',(-19.094878629162,-0.00521749440511517,
2.3095796225373));
#54227=CARTESIAN_POINT('Ctrl Pts',(-18.9837322842846,-1.94333229105276,
1.24805643367561));
#54228=CARTESIAN_POINT('Ctrl Pts',(-18.8725859394071,-2.10244519912854,
-0.955986108554305));
#54229=CARTESIAN_POINT('Ctrl Pts',(-18.7614395945297,-0.336898080152378,
-2.28488182159977));
#54230=CARTESIAN_POINT('Ctrl Pts',(-18.6502932496523,1.73705863177231,-1.5221079346987));
#54231=CARTESIAN_POINT('Ctrl Pts',(-18.5391469047749,2.22084437771726,0.634062698042624));
#54232=CARTESIAN_POINT('Ctrl Pts',(-18.4280005598974,0.671582888059023,
2.20978770010916));
#54233=CARTESIAN_POINT('Ctrl Pts',(-18.31685421502,-1.4924716720845,1.76258717886881));
#54234=CARTESIAN_POINT('Ctrl Pts',(-18.2057078701426,-2.29025967271958,
-0.298154132290432));
#54235=CARTESIAN_POINT('Ctrl Pts',(-18.0945615252652,-0.991454979533412,
-2.08595356579331));
#54236=CARTESIAN_POINT('Ctrl Pts',(-17.9834151803877,1.21496612549574,-1.96419005419163));
#54237=CARTESIAN_POINT('Ctrl Pts',(-17.8722688355103,2.3091600310083,-0.0443306471998567));
#54238=CARTESIAN_POINT('Ctrl Pts',(-17.7611224906329,1.28945912033737,1.91611075673255));
#54239=CARTESIAN_POINT('Ctrl Pts',(-17.6499761457555,-0.910662771798187,
2.12246992231887));
#54240=CARTESIAN_POINT('Ctrl Pts',(-17.5388298008781,-2.27712857828129,
0.385837651172181));
#54241=CARTESIAN_POINT('Ctrl Pts',(-17.4276834560006,-1.55902240500851,
-1.70400539781096));
#54242=CARTESIAN_POINT('Ctrl Pts',(-17.3165371111232,0.586273454560011,
-2.23393569548582));
#54243=CARTESIAN_POINT('Ctrl Pts',(-17.2053907662458,2.19487181381747,-0.718834456601151));
#54244=CARTESIAN_POINT('Ctrl Pts',(-17.0942444213684,1.79419923164516,1.45431577460032));
#54245=CARTESIAN_POINT('Ctrl Pts',(-16.983098076491,-0.24895304186277,2.29612883742065));
#54246=CARTESIAN_POINT('Ctrl Pts',(-16.8719517316135,-2.06420402762972,
1.03597634500247));
#54247=CARTESIAN_POINT('Ctrl Pts',(-16.7608053867361,-1.98980244061841,
-1.17254914711346));
#54248=CARTESIAN_POINT('Ctrl Pts',(-16.6496590418587,-0.0938583844972828,
-2.30767758986106));
#54249=CARTESIAN_POINT('Ctrl Pts',(-16.5385126969813,1.88800728371649,-1.33026830065251));
#54250=CARTESIAN_POINT('Ctrl Pts',(-16.4273663521038,2.14151772476039,0.864920279346345));
#54251=CARTESIAN_POINT('Ctrl Pts',(-16.3162200072264,0.434599630602511,
2.26832722863514));
#54252=CARTESIAN_POINT('Ctrl Pts',(-16.205073662349,-1.67016785203829,1.59521929561588));
#54253=CARTESIAN_POINT('Ctrl Pts',(-16.0939273174715,-2.24599878754927,
-0.538214363813031));
#54254=CARTESIAN_POINT('Ctrl Pts',(-15.9827809725941,-0.765755163307141,
-2.17894568196545));
#54255=CARTESIAN_POINT('Ctrl Pts',(-15.8716346277167,1.41549049130265,-1.82498545860486));
#54256=CARTESIAN_POINT('Ctrl Pts',(-15.7604882828393,2.30094115044168,0.199637364467602));
#54257=CARTESIAN_POINT('Ctrl Pts',(-15.6493419379619,1.08002087601742,2.04150438707684));
#54258=CARTESIAN_POINT('Ctrl Pts',(-15.5381955930844,-1.12959247317232,
2.01449896987808));
#54259=CARTESIAN_POINT('Ctrl Pts',(-15.427049248207,-2.30513298142682,0.143342921086773));
#54260=CARTESIAN_POINT('Ctrl Pts',(-15.3159029033296,-1.37046519115816,
-1.85903480734257));
#54261=CARTESIAN_POINT('Ctrl Pts',(-15.2047565584522,0.818779685343973,
-2.15957983921769));
#54262=CARTESIAN_POINT('Ctrl Pts',(-15.0936102135747,2.25848182370628,-0.483161574502515));
#54263=CARTESIAN_POINT('Ctrl Pts',(-14.9824638686973,1.63068194598152,1.63556156904512));
#54264=CARTESIAN_POINT('Ctrl Pts',(-14.8713175238199,-0.489907546220147,
2.25702810156277));
#54265=CARTESIAN_POINT('Ctrl Pts',(-14.7601711789425,-2.16201663496024,
0.81232341172874));
#54266=CARTESIAN_POINT('Ctrl Pts',(-14.649024834065,-1.85493168960417,-1.37601369251531));
#54267=CARTESIAN_POINT('Ctrl Pts',(-14.5378784891876,0.15022979889931,-2.30469439679324));
#54268=CARTESIAN_POINT('Ctrl Pts',(-14.4267321443102,2.01786509222139,-1.12356829996301));
#54269=CARTESIAN_POINT('Ctrl Pts',(-14.3155857994328,2.03826827476513,1.08611587557377));
#54270=CARTESIAN_POINT('Ctrl Pts',(-14.2044394545554,0.1927614804521,2.30152737692633));
#54271=CARTESIAN_POINT('Ctrl Pts',(-14.0932931096779,-1.82920666292977,
1.41003129021336));
#54272=CARTESIAN_POINT('Ctrl Pts',(-13.9821467648005,-2.17664795214331,
-0.772262227172698));
#54273=CARTESIAN_POINT('Ctrl Pts',(-13.8710004199231,-0.531501131002706,
-2.24759689509269));
#54274=CARTESIAN_POINT('Ctrl Pts',(-13.7598540750456,1.60020247725313,-1.66539403351891));
#54275=CARTESIAN_POINT('Ctrl Pts',(-13.6487077301682,2.26701856100407,0.441375236222479));
#54276=CARTESIAN_POINT('Ctrl Pts',(-13.5375613852908,0.858517767645496,
2.14409246482619));
#54277=CARTESIAN_POINT('Ctrl Pts',(-13.4264150404134,-1.33590354843874,
1.88402414112882));
#54278=CARTESIAN_POINT('Ctrl Pts',(-13.315268695536,-2.30738684894824,-0.100753086246275));
#54279=CARTESIAN_POINT('Ctrl Pts',(-13.2041223506585,-1.16659857303008,
-1.99329702364993));
#54280=CARTESIAN_POINT('Ctrl Pts',(-13.0929760057811,1.04213936552734,-2.06109941485259));
#54281=CARTESIAN_POINT('Ctrl Pts',(-12.9818296609037,2.29686243593069,-0.242091316444785));
#54282=CARTESIAN_POINT('Ctrl Pts',(-12.8706833160263,1.44894838651503,1.79853657963994));
#54283=CARTESIAN_POINT('Ctrl Pts',(-12.7595369711489,-0.725389315675418,
2.19271420750434));
#54284=CARTESIAN_POINT('Ctrl Pts',(-12.6483906262714,-2.23567745285949,
0.579596050593111));
#54285=CARTESIAN_POINT('Ctrl Pts',(-12.537244281394,-1.69933958110716,-1.56410685158336));
#54286=CARTESIAN_POINT('Ctrl Pts',(-12.4260979365166,0.3926397720497,-2.27596556751023));
#54287=CARTESIAN_POINT('Ctrl Pts',(-12.3149515916392,2.12518142161832,-0.904316968930544));
#54288=CARTESIAN_POINT('Ctrl Pts',(-12.2038052467617,1.9122494226383,1.29517852078659));
#54289=CARTESIAN_POINT('Ctrl Pts',(-12.0926589018843,-0.0512299994234969,
2.30901726763714));
#54290=CARTESIAN_POINT('Ctrl Pts',(-11.9815125570069,-1.96781148944065,
1.20909188944132));
#54291=CARTESIAN_POINT('Ctrl Pts',(-11.8703662121295,-2.08298188152774,
-0.997683184339907));
#54292=CARTESIAN_POINT('Ctrl Pts',(-11.759219867252,-0.291309723753528,
-2.29114030559764));
#54293=CARTESIAN_POINT('Ctrl Pts',(-11.6480735223746,1.76703867415875,-1.48719856748004));
#54294=CARTESIAN_POINT('Ctrl Pts',(-11.5369271774972,2.20777121039822,0.678182525301448));
#54295=CARTESIAN_POINT('Ctrl Pts',(-11.4257808326198,0.627424196364101,
2.22272898323306));
#54296=CARTESIAN_POINT('Ctrl Pts',(-11.3146344877423,-1.5272913059653,1.73250296444486));
#54297=CARTESIAN_POINT('Ctrl Pts',(-11.2034881428649,-2.28386500299402,
-0.343723585438356));
#54298=CARTESIAN_POINT('Ctrl Pts',(-11.0923417979875,-0.949699935336984,
-2.10529220962515));
#54299=CARTESIAN_POINT('Ctrl Pts',(-10.9811954531101,1.25385735428831,-1.9395945427291));
#54300=CARTESIAN_POINT('Ctrl Pts',(-10.8700491082326,2.30958490241829,0.00168333269087447));
#54301=CARTESIAN_POINT('Ctrl Pts',(-10.7589027633552,1.25102869056742,1.94142021995873));
#54302=CARTESIAN_POINT('Ctrl Pts',(-10.6477564184778,-0.952767794099242,
2.10390560282886));
#54303=CARTESIAN_POINT('Ctrl Pts',(-10.5366100736004,-2.28436361968318,
0.340394048354919));
#54304=CARTESIAN_POINT('Ctrl Pts',(-10.4254637287229,-1.52476422749005,
-1.7347274441981));
#54305=CARTESIAN_POINT('Ctrl Pts',(-10.3143173838455,0.630663584176363,
-2.2218120304565));
#54306=CARTESIAN_POINT('Ctrl Pts',(-10.2031710389681,2.20875744607579,-0.674963554195493));
#54307=CARTESIAN_POINT('Ctrl Pts',(-10.0920246940907,1.7648689192416,1.48977278568995));
#54308=CARTESIAN_POINT('Ctrl Pts',(-9.98087834921324,-0.294649191307109,
2.29071323153936));
#54309=CARTESIAN_POINT('Ctrl Pts',(-9.86973200433586,-2.08443398336217,
0.99464577820062));
#54310=CARTESIAN_POINT('Ctrl Pts',(-9.75858565945839,-1.96604691511444,
-1.21195906806146));
#54311=CARTESIAN_POINT('Ctrl Pts',(-9.647439314581,-0.047864108838437,-2.30908949202333));
#54312=CARTESIAN_POINT('Ctrl Pts',(-9.53629296970356,1.91413536245694,-1.29238967392936));
#54313=CARTESIAN_POINT('Ctrl Pts',(-9.42514662482614,2.12386094808125,0.907413868255737));
#54314=CARTESIAN_POINT('Ctrl Pts',(-9.31400027994872,0.389321697940529,
2.27653549732926));
#54315=CARTESIAN_POINT('Ctrl Pts',(-9.2028539350713,-1.70161776182311,1.56162807599489));
#54316=CARTESIAN_POINT('Ctrl Pts',(-9.09170759019387,-2.23483020503478,
-0.58285436410105));
#54317=CARTESIAN_POINT('Ctrl Pts',(-8.98056124531646,-0.722192242889091,
-2.19376927214288));
#54318=CARTESIAN_POINT('Ctrl Pts',(-8.86941490043901,1.45156855961018,-1.79642254824377));
#54319=CARTESIAN_POINT('Ctrl Pts',(-8.75826855556161,2.29650710107497,0.245439177393632));
#54320=CARTESIAN_POINT('Ctrl Pts',(-8.64712221068417,1.03913381005442,2.06261634335842));
#54321=CARTESIAN_POINT('Ctrl Pts',(-8.53597586580677,-1.16950294685762,
1.9915943644173));
#54322=CARTESIAN_POINT('Ctrl Pts',(-8.42482952092932,-2.30753126447749,
0.0973895196946199));
#54323=CARTESIAN_POINT('Ctrl Pts',(-8.31368317605192,-1.33315580208287,
-1.88596947548475));
#54324=CARTESIAN_POINT('Ctrl Pts',(-8.20253683117448,0.86164228210699,-2.14283873232982));
#54325=CARTESIAN_POINT('Ctrl Pts',(-8.09139048629707,2.26765954162825,-0.438070152315537));
#54326=CARTESIAN_POINT('Ctrl Pts',(-7.98024414141964,1.59777314547094,1.66772486660701));
#54327=CARTESIAN_POINT('Ctrl Pts',(-7.86909779654221,-0.534776870484712,
2.24681974218716));
#54328=CARTESIAN_POINT('Ctrl Pts',(-7.75795145166479,-2.17777136012248,
0.769088524240027));
#54329=CARTESIAN_POINT('Ctrl Pts',(-7.64680510678736,-1.82714932809128,
-1.4126962121925));
#54330=CARTESIAN_POINT('Ctrl Pts',(-7.53565876190995,0.196116193858117,
-2.30124394482506));
#54331=CARTESIAN_POINT('Ctrl Pts',(-7.42451241703251,2.0398493317374,-1.08314355415055));
#54332=CARTESIAN_POINT('Ctrl Pts',(-7.31336607215511,2.01622513177459,1.12650853218607));
#54333=CARTESIAN_POINT('Ctrl Pts',(-7.20221972727766,0.146870104548076,
2.30491093699463));
#54334=CARTESIAN_POINT('Ctrl Pts',(-7.09107338240025,-1.85693552310777,
1.37330831138092));
#54335=CARTESIAN_POINT('Ctrl Pts',(-6.97992703752283,-2.16083022056687,
-0.815474103189318));
#54336=CARTESIAN_POINT('Ctrl Pts',(-6.8687806926454,-0.486616973764323,
-2.25773983796448));
#54337=CARTESIAN_POINT('Ctrl Pts',(-6.75763434776797,1.63306435861655,-1.63318279923092));
#54338=CARTESIAN_POINT('Ctrl Pts',(-6.64648800289056,2.25777512342436,0.486453232216203));
#54339=CARTESIAN_POINT('Ctrl Pts',(-6.53534165801313,0.815630813042409,
2.16077107346039));
#54340=CARTESIAN_POINT('Ctrl Pts',(-6.42419531313571,-1.37317363542316,
1.85703511600243));
#54341=CARTESIAN_POINT('Ctrl Pts',(-6.31304896825829,-2.30492158253688,
-0.146702942857817));
#54342=CARTESIAN_POINT('Ctrl Pts',(-6.20190262338086,-1.12665475388528,
-2.01614342759515));
#54343=CARTESIAN_POINT('Ctrl Pts',(-6.09075627850344,1.08299561331934,-2.03992788024932));
#54344=CARTESIAN_POINT('Ctrl Pts',(-5.97960993362602,2.30122971564711,-0.196283088701521));
#54345=CARTESIAN_POINT('Ctrl Pts',(-5.86846358874859,1.41282872061015,1.82704686894083));
#54346=CARTESIAN_POINT('Ctrl Pts',(-5.75731724387116,-0.76893058158095,
2.17782713175243));
#54347=CARTESIAN_POINT('Ctrl Pts',(-5.64617089899375,-2.24678095213377,
0.534939817377955));
#54348=CARTESIAN_POINT('Ctrl Pts',(-5.53502455411632,-1.66784073908135,
-1.59765219123186));
#54349=CARTESIAN_POINT('Ctrl Pts',(-5.4238782092389,0.43790569147873,-2.26769130625355));
#54350=CARTESIAN_POINT('Ctrl Pts',(-5.31273186436147,2.14277623697082,-0.861797687024427));
#54351=CARTESIAN_POINT('Ctrl Pts',(-5.20158551948405,1.88606615628344,1.33301902057307));
#54352=CARTESIAN_POINT('Ctrl Pts',(-5.09043917460662,-0.0972221680979084,
2.30753832148412));
#54353=CARTESIAN_POINT('Ctrl Pts',(-4.97929282972921,-1.99150954217679,
1.16964738212262));
#54354=CARTESIAN_POINT('Ctrl Pts',(-4.86814648485178,-2.06269170004884,
-1.03898421818477));
#54355=CARTESIAN_POINT('Ctrl Pts',(-4.75700013997435,-0.245605728572608,
-2.2964892948106));
#54356=CARTESIAN_POINT('Ctrl Pts',(-4.64585379509694,1.796317269997,-1.45169883949742));
#54357=CARTESIAN_POINT('Ctrl Pts',(-4.5347074502195,2.19382164262593,0.722033140121231));
#54358=CARTESIAN_POINT('Ctrl Pts',(-4.42356110534209,0.58301644133906,2.23478792824183));
#54359=CARTESIAN_POINT('Ctrl Pts',(-4.31241476046466,-1.56150466380355,
1.70173101282442));
#54360=CARTESIAN_POINT('Ctrl Pts',(-4.20126841558724,-2.27656372649916,
-0.389156593512695));
#54361=CARTESIAN_POINT('Ctrl Pts',(-4.09012207070982,-0.907567896709133,
-2.12379513323403));
#54362=CARTESIAN_POINT('Ctrl Pts',(-3.97897572583239,1.29225084982594,-1.91422908666128));
#54363=CARTESIAN_POINT('Ctrl Pts',(-3.86782938095497,2.30909295724377,0.0476966443656992));
#54364=CARTESIAN_POINT('Ctrl Pts',(-3.75668303607755,1.21210165041682,1.96595901384947));
#54365=CARTESIAN_POINT('Ctrl Pts',(-3.64553669120012,-0.994494604154669,
2.08450611355572));
#54366=CARTESIAN_POINT('Ctrl Pts',(-3.5343903463227,-2.29069185636784,0.29481532214432));
#54367=CARTESIAN_POINT('Ctrl Pts',(-3.42324400144527,-1.48990077711358,
-1.76476087032143));
#54368=CARTESIAN_POINT('Ctrl Pts',(-3.31209765656785,0.674803364609756,
-2.20880639137193));
#54369=CARTESIAN_POINT('Ctrl Pts',(-3.20095131169043,2.22176628626919,-0.630824717035695));
#54370=CARTESIAN_POINT('Ctrl Pts',(-3.08980496681301,1.73483802181615,1.52463841391558));
#54371=CARTESIAN_POINT('Ctrl Pts',(-2.97865862193558,-0.34022837674139,
2.28438830085055));
#54372=CARTESIAN_POINT('Ctrl Pts',(-2.86751227705816,-2.10383649800309,
0.952920374344482));
#54373=CARTESIAN_POINT('Ctrl Pts',(-2.75636593218073,-1.94151094591982,
-1.25088788615355));
#54374=CARTESIAN_POINT('Ctrl Pts',(-2.64521958730332,-0.00185083012522597,
-2.30958477732822));
#54375=CARTESIAN_POINT('Ctrl Pts',(-2.53407324242588,1.93950359750643,-1.25399801226566));
#54376=CARTESIAN_POINT('Ctrl Pts',(-2.42292689754847,2.10536109037917,0.949547237585121));
#54377=CARTESIAN_POINT('Ctrl Pts',(-2.31178055267104,0.343889199955978,
2.28384008989064));
#54378=CARTESIAN_POINT('Ctrl Pts',(-2.20063420779362,-1.73239215746682,
1.52741690980612));
#54379=CARTESIAN_POINT('Ctrl Pts',(-2.08948786291619,-2.2227745514199,-0.627262917205774));
#54380=CARTESIAN_POINT('Ctrl Pts',(-1.97834151803877,-0.678342505305206,
-2.20772216536846));
#54381=CARTESIAN_POINT('Ctrl Pts',(-1.86719517316134,1.48707015493526,-1.76714625072322));
#54382=CARTESIAN_POINT('Ctrl Pts',(-1.75604882828392,2.2911619134242,0.291143034710522));
#54383=CARTESIAN_POINT('Ctrl Pts',(-1.6449024834065,0.997833321604641,2.0829105200713));
#54384=CARTESIAN_POINT('Ctrl Pts',(-1.53375613852908,-1.20894741079716,
1.96789727020159));
#54385=CARTESIAN_POINT('Ctrl Pts',(-1.42260979365165,-2.30901689786607,
0.0514010769203556));
#54386=CARTESIAN_POINT('Ctrl Pts',(-1.31146344877423,-1.29531082547211,
-1.91216236950752));
#54387=CARTESIAN_POINT('Ctrl Pts',(-1.2003171038968,0.904150711394524,-2.12523390663066));
#54388=CARTESIAN_POINT('Ctrl Pts',(-1.08917075901938,2.2759601575129,-0.392829741546613));
#54389=CARTESIAN_POINT('Ctrl Pts',(-0.978024414141959,1.56418620131702,
1.69927352442324));
#54390=CARTESIAN_POINT('Ctrl Pts',(-0.866878069264531,-0.57935041752618,
2.23562934222088));
#54391=CARTESIAN_POINT('Ctrl Pts',(-0.755731724387112,-2.19282043956138,
0.725719843207388));
#54392=CARTESIAN_POINT('Ctrl Pts',(-0.644585379509683,-1.79833929219668,
-1.44914450295862));
#54393=CARTESIAN_POINT('Ctrl Pts',(-0.533439034632267,0.241347848115584,
-2.29625613399237));
#54394=CARTESIAN_POINT('Ctrl Pts',(-0.422292689754837,2.06213591769256,
-1.04349838147448));
#54395=CARTESIAN_POINT('Ctrl Pts',(-0.311146344877418,1.99113983194757,
1.16894947486069));
#54396=CARTESIAN_POINT('Ctrl Pts',(-0.237048781625798,0.734562905288542,
1.92373973464384));
#54397=CARTESIAN_POINT('Ctrl Pts',(-0.199999999999991,0.0853826423429707,
1.9521336543348));
#54398=CARTESIAN_POINT('Ctrl Pts',(-29.7993827215147,1.05793541951253,-1.4823699524473));
#54399=CARTESIAN_POINT('Ctrl Pts',(-29.7623339398889,1.55089619265196,-1.1305544953993));
#54400=CARTESIAN_POINT('Ctrl Pts',(-29.6882363766373,2.14974771680019,0.0973963207404695));
#54401=CARTESIAN_POINT('Ctrl Pts',(-29.5770900317599,1.08185724657521,1.86262115551182));
#54402=CARTESIAN_POINT('Ctrl Pts',(-29.4659436868824,-0.977303115035886,
1.91722336588929));
#54403=CARTESIAN_POINT('Ctrl Pts',(-29.354797342005,-2.14133124400932,0.219490070886125));
#54404=CARTESIAN_POINT('Ctrl Pts',(-29.2436509971276,-1.34534920141955,
-1.68061148074165));
#54405=CARTESIAN_POINT('Ctrl Pts',(-29.1325046522502,0.682347969528367,
-2.04146153236715));
#54406=CARTESIAN_POINT('Ctrl Pts',(-29.0213583073728,2.08532885325423,-0.533874775345859));
#54407=CARTESIAN_POINT('Ctrl Pts',(-28.9102119624953,1.57935465773805,1.46265005426954));
#54408=CARTESIAN_POINT('Ctrl Pts',(-28.7990656176179,-0.372441072386024,
2.12009866279412));
#54409=CARTESIAN_POINT('Ctrl Pts',(-28.6879192727404,-1.98327983047877,
0.836784155643198));
#54410=CARTESIAN_POINT('Ctrl Pts',(-28.5767729278631,-1.77855239711682,
-1.21258534936276));
#54411=CARTESIAN_POINT('Ctrl Pts',(-28.4656265829856,0.0543337550040538,
-2.15189119828085));
#54412=CARTESIAN_POINT('Ctrl Pts',(-28.3544802381082,1.83747923218003,-1.12128059578709));
#54413=CARTESIAN_POINT('Ctrl Pts',(-28.2433338932307,1.93852558318769,0.93579822925128));
#54414=CARTESIAN_POINT('Ctrl Pts',(-28.1321875483534,0.264969893601056,
2.13620868271033));
#54415=CARTESIAN_POINT('Ctrl Pts',(-28.0210412034759,-1.6511493223133,1.38105191948624));
#54416=CARTESIAN_POINT('Ctrl Pts',(-27.9098948585985,-2.05574240249434,
-0.638374071221615));
#54417=CARTESIAN_POINT('Ctrl Pts',(-27.7987485137211,-0.578428952338934,
-2.07340729692367));
#54418=CARTESIAN_POINT('Ctrl Pts',(-27.6876021688437,1.42840080550757,-1.61036309606447));
#54419=CARTESIAN_POINT('Ctrl Pts',(-27.5764558239662,2.12761698064718,0.326870147354796));
#54420=CARTESIAN_POINT('Ctrl Pts',(-27.4653094790888,0.879129893443812,
1.96487370836676));
#54421=CARTESIAN_POINT('Ctrl Pts',(-27.3541631342114,-1.174146852909,1.80415555603761));
#54422=CARTESIAN_POINT('Ctrl Pts',(-27.243016789334,-2.15256395025648,-0.00815670731610067));
#54423=CARTESIAN_POINT('Ctrl Pts',(-27.1318704444565,-1.16044036715154,
-1.81300199677203));
#54424=CARTESIAN_POINT('Ctrl Pts',(-27.0207240995791,0.893995417007299,
-1.95815481682795));
#54425=CARTESIAN_POINT('Ctrl Pts',(-26.9095777547017,2.13003306004753,-0.310736630320814));
#54426=CARTESIAN_POINT('Ctrl Pts',(-26.7984314098243,1.4161556760299,1.62114194041067));
#54427=CARTESIAN_POINT('Ctrl Pts',(-26.6872850649468,-0.594125639310525,
2.06896418898866));
#54428=CARTESIAN_POINT('Ctrl Pts',(-26.5761387200694,-2.06052125936704,
0.622776227836984));
#54429=CARTESIAN_POINT('Ctrl Pts',(-26.464992375192,-1.64063565578329,-1.3935252904711));
#54430=CARTESIAN_POINT('Ctrl Pts',(-26.3538460303146,0.281151574973685,
-2.13413961169929));
#54431=CARTESIAN_POINT('Ctrl Pts',(-26.2426996854371,1.94556172969375,-0.921079609061524));
#54432=CARTESIAN_POINT('Ctrl Pts',(-26.1315533405598,1.82892908108006,1.13517245679029));
#54433=CARTESIAN_POINT('Ctrl Pts',(-26.0204069956823,0.03802368751086,2.15224354790078));
#54434=CARTESIAN_POINT('Ctrl Pts',(-25.9092606508049,-1.78769006704002,
1.19906726854251));
#54435=CARTESIAN_POINT('Ctrl Pts',(-25.7981143059274,-1.97688287245175,
-0.851781778914594));
#54436=CARTESIAN_POINT('Ctrl Pts',(-25.6869679610501,-0.356360283451301,
-2.12287668946283));
#54437=CARTESIAN_POINT('Ctrl Pts',(-25.5758216161726,1.59038835561325,-1.45060779282844));
#54438=CARTESIAN_POINT('Ctrl Pts',(-25.4646752712952,2.08123369845556,0.549603841596811));
#54439=CARTESIAN_POINT('Ctrl Pts',(-25.3535289264178,0.666836846147605,
2.04668676423755));
#54440=CARTESIAN_POINT('Ctrl Pts',(-25.2423825815403,-1.35800836546965,
1.67015309765288));
#54441=CARTESIAN_POINT('Ctrl Pts',(-25.1312362366629,-2.13967995310613,
-0.235303609323872));
#54442=CARTESIAN_POINT('Ctrl Pts',(-25.0200898917855,-0.962605373120884,
-1.92535424946266));
#54443=CARTESIAN_POINT('Ctrl Pts',(-24.9089435469081,1.09567556802856,-1.85286079884874));
#54444=CARTESIAN_POINT('Ctrl Pts',(-24.7977972020306,2.15093252107306,-0.084186578950635));
#54445=CARTESIAN_POINT('Ctrl Pts',(-24.6866508571532,1.23714226855362,1.76155530643892));
#54446=CARTESIAN_POINT('Ctrl Pts',(-24.5755045122758,-0.809176086504933,
1.99470101802593));
#54447=CARTESIAN_POINT('Ctrl Pts',(-24.4643581673984,-2.11474321095452,
0.401819912407123));
#54448=CARTESIAN_POINT('Ctrl Pts',(-24.3532118225209,-1.48439223048003,
-1.55890275398294));
#54449=CARTESIAN_POINT('Ctrl Pts',(-24.2420654776435,0.504829074726625,
-2.09254526727519));
#54450=CARTESIAN_POINT('Ctrl Pts',(-24.1309191327661,2.03191022949194,-0.710590535801833));
#54451=CARTESIAN_POINT('Ctrl Pts',(-24.0197727878887,1.69890180908922,1.32186638256614));
#54452=CARTESIAN_POINT('Ctrl Pts',(-23.9086264430113,-0.189347339202901,
2.14423545242165));
#54453=CARTESIAN_POINT('Ctrl Pts',(-23.7974800981338,-1.90426057598421,
1.00368807357534));
#54454=CARTESIAN_POINT('Ctrl Pts',(-23.6863337532564,-1.87593969032234,
-1.05567436672414));
#54455=CARTESIAN_POINT('Ctrl Pts',(-23.575187408379,-0.13031072137717,-2.14863147286343));
#54456=CARTESIAN_POINT('Ctrl Pts',(-23.4640410635016,1.73460974521793,-1.27464784237848));
#54457=CARTESIAN_POINT('Ctrl Pts',(-23.3528947186241,2.01160105173812,0.766197950226435));
#54458=CARTESIAN_POINT('Ctrl Pts',(-23.2417483737467,0.447094593531423,
2.10563636811299));
#54459=CARTESIAN_POINT('Ctrl Pts',(-23.1306020288693,-1.52669962772263,
1.51749343886447));
#54460=CARTESIAN_POINT('Ctrl Pts',(-23.0194556839919,-2.10289368892934,
-0.459821947438659));
#54461=CARTESIAN_POINT('Ctrl Pts',(-22.9083093391144,-0.75401715809411,
-2.01619845639877));
#54462=CARTESIAN_POINT('Ctrl Pts',(-22.797162994237,1.28511597704955,-1.72686855777071));
#54463=CARTESIAN_POINT('Ctrl Pts',(-22.6860166493596,2.1478040128497,0.143303917154594));
#54464=CARTESIAN_POINT('Ctrl Pts',(-22.5748703044822,1.04430880107363,1.88229041815689));
#54465=CARTESIAN_POINT('Ctrl Pts',(-22.4637239596048,-1.01518726445027,
1.89815513285481));
#54466=CARTESIAN_POINT('Ctrl Pts',(-22.3525776147273,-2.14534146238614,
0.176374884980863));
#54467=CARTESIAN_POINT('Ctrl Pts',(-22.2414312698499,-1.31156672712401,
-1.70686578575655));
#54468=CARTESIAN_POINT('Ctrl Pts',(-22.1302849249725,0.72286715185956,-2.02757519491819));
#54469=CARTESIAN_POINT('Ctrl Pts',(-22.0191385800951,2.09556035259399,-0.492163488000983));
#54470=CARTESIAN_POINT('Ctrl Pts',(-21.9079922352176,1.54989618230904,1.49379379913996));
#54471=CARTESIAN_POINT('Ctrl Pts',(-21.7968458903402,-0.414603175407699,
2.11227420029383));
#54472=CARTESIAN_POINT('Ctrl Pts',(-21.6856995454628,-1.99955867670109,
0.797096724817328));
#54473=CARTESIAN_POINT('Ctrl Pts',(-21.5745532005854,-1.75404047129018,
-1.24777406422847));
#54474=CARTESIAN_POINT('Ctrl Pts',(-21.4634068557079,0.0971945358346896,
-2.15038399186959));
#54475=CARTESIAN_POINT('Ctrl Pts',(-21.3522605108305,1.85945388830448,-1.08444885889306));
#54476=CARTESIAN_POINT('Ctrl Pts',(-21.2411141659531,1.91949690122385,0.974232896425261));
#54477=CARTESIAN_POINT('Ctrl Pts',(-21.1299678210757,0.222357867559114,
2.14106400395216));
#54478=CARTESIAN_POINT('Ctrl Pts',(-21.0188214761983,-1.67833619791759,
1.34788192993475));
#54479=CARTESIAN_POINT('Ctrl Pts',(-20.9076751313208,-2.04261609506057,
-0.679203635506052));
#54480=CARTESIAN_POINT('Ctrl Pts',(-20.7965287864434,-0.537005851711156,
-2.08451980213983));
#54481=CARTESIAN_POINT('Ctrl Pts',(-20.685382441566,1.46020041397922,-1.5815855466272));
#54482=CARTESIAN_POINT('Ctrl Pts',(-20.5742360966886,2.12068248374981,0.369193571723346));
#54483=CARTESIAN_POINT('Ctrl Pts',(-20.4630897518111,0.839809407505516,
1.98199854928058));
#54484=CARTESIAN_POINT('Ctrl Pts',(-20.3519434069337,-1.20985783166774,
1.78040504308355));
#54485=CARTESIAN_POINT('Ctrl Pts',(-20.2407970620563,-2.15197420198039,
-0.0510404182583582));
#54486=CARTESIAN_POINT('Ctrl Pts',(-20.1296507171789,-1.12408977155138,
-1.83576149752049));
#54487=CARTESIAN_POINT('Ctrl Pts',(-20.0185043723015,0.932830112938281,
-1.93995517233793));
#54488=CARTESIAN_POINT('Ctrl Pts',(-19.907358027424,2.13580106637051,-0.268238504275029));
#54489=CARTESIAN_POINT('Ctrl Pts',(-19.7962116825466,1.38357673581526,1.64903411316925));
#54490=CARTESIAN_POINT('Ctrl Pts',(-19.6850653376692,-0.635227498409481,
2.05671682920852));
#54491=CARTESIAN_POINT('Ctrl Pts',(-19.5739189927917,-2.07251979844461,
0.581601044823888));
#54492=CARTESIAN_POINT('Ctrl Pts',(-19.4627726479143,-1.61254694598326,
-1.42593493445009));
#54493=CARTESIAN_POINT('Ctrl Pts',(-19.3516263030369,0.323614037310276,
-2.12811466917101));
#54494=CARTESIAN_POINT('Ctrl Pts',(-19.2404799581594,1.9635261566324,-0.88213554656046));
#54495=CARTESIAN_POINT('Ctrl Pts',(-19.1293336132821,1.8059501381863,1.17138473127749));
#54496=CARTESIAN_POINT('Ctrl Pts',(-19.0181872684046,-0.00486280803173237,
2.15257391124745));
#54497=CARTESIAN_POINT('Ctrl Pts',(-18.9070409235272,-1.81122415083018,
1.16321329331064));
#54498=CARTESIAN_POINT('Ctrl Pts',(-18.7958945786497,-1.95952052975758,
-0.89099797067317));
#54499=CARTESIAN_POINT('Ctrl Pts',(-18.6847482337724,-0.313995677398985,
-2.12955507204201));
#54500=CARTESIAN_POINT('Ctrl Pts',(-18.5736018888949,1.61897301854108,-1.41863471532354));
#54501=CARTESIAN_POINT('Ctrl Pts',(-18.4624555440175,2.06987090714062,0.590958981705142));
#54502=CARTESIAN_POINT('Ctrl Pts',(-18.3513091991401,0.625928541267625,
2.05956586481513));
#54503=CARTESIAN_POINT('Ctrl Pts',(-18.2401628542627,-1.39101313211078,
1.64276612960593));
#54504=CARTESIAN_POINT('Ctrl Pts',(-18.1290165093852,-2.13456733570513,
-0.277885551308158));
#54505=CARTESIAN_POINT('Ctrl Pts',(-18.0178701645078,-0.924055660300427,
-1.94415000114493));
#54506=CARTESIAN_POINT('Ctrl Pts',(-17.9067238196304,1.13237247128039,-1.83066399881886));
#54507=CARTESIAN_POINT('Ctrl Pts',(-17.795577474753,2.15218284363935,-0.0413170404259255));
#54508=CARTESIAN_POINT('Ctrl Pts',(-17.6844311298755,1.20180141657515,1.78585314217129));
#54509=CARTESIAN_POINT('Ctrl Pts',(-17.5732847849981,-0.848755723937063,
1.97818396802956));
#54510=CARTESIAN_POINT('Ctrl Pts',(-17.4621384401207,-2.12232889584438,
0.359608326028584));
#54511=CARTESIAN_POINT('Ctrl Pts',(-17.3509920952433,-1.45303973213311,
-1.58816675041623));
#54512=CARTESIAN_POINT('Ctrl Pts',(-17.2398457503659,0.546418461103423,
-2.08207227435804));
#54513=CARTESIAN_POINT('Ctrl Pts',(-17.1286994054884,2.04566396362873,-0.66996793818504));
#54514=CARTESIAN_POINT('Ctrl Pts',(-17.017553060611,1.67222918834758,1.35545108060876));
#54515=CARTESIAN_POINT('Ctrl Pts',(-16.9064067157336,-0.232029161415369,
2.1400375133483));
#54516=CARTESIAN_POINT('Ctrl Pts',(-16.7952603708562,-1.92387900118643,
0.965550453927213));
#54517=CARTESIAN_POINT('Ctrl Pts',(-16.6841140259787,-1.85453524979851,
-1.09283900806108));
#54518=CARTESIAN_POINT('Ctrl Pts',(-16.5729676811013,-0.0874778716651755,
-2.15080117915488));
#54519=CARTESIAN_POINT('Ctrl Pts',(-16.4618213362239,1.75966014919564,-1.23983638018002));
#54520=CARTESIAN_POINT('Ctrl Pts',(-16.3506749913465,1.99593689683189,0.806122815798095));
#54521=CARTESIAN_POINT('Ctrl Pts',(-16.239528646469,0.405055455782525,2.11412586380894));
#54522=CARTESIAN_POINT('Ctrl Pts',(-16.1283823015916,-1.55662948816291,
1.48677595046018));
#54523=CARTESIAN_POINT('Ctrl Pts',(-16.0172359567142,-2.09331531487129,
-0.501626437511458));
#54524=CARTESIAN_POINT('Ctrl Pts',(-15.9060896118368,-0.713698965323934,
-2.03082049358889));
#54525=CARTESIAN_POINT('Ctrl Pts',(-15.7949432669594,1.31926514828246,-1.7009225610863));
#54526=CARTESIAN_POINT('Ctrl Pts',(-15.6837969220819,2.14452268431221,0.186065974201366));
#54527=CARTESIAN_POINT('Ctrl Pts',(-15.5726505772045,1.00660082840694,1.90272248700002));
#54528=CARTESIAN_POINT('Ctrl Pts',(-15.4615042323271,-1.05280253790118,
1.877552903775));
#54529=CARTESIAN_POINT('Ctrl Pts',(-15.3503578874497,-2.14842955374026,
0.133598438989754));
#54530=CARTESIAN_POINT('Ctrl Pts',(-15.2392115425722,-1.27730067756617,
-1.73265722789423));
#54531=CARTESIAN_POINT('Ctrl Pts',(-15.1280651976948,0.763118869136211,
-2.01277114492766));
#54532=CARTESIAN_POINT('Ctrl Pts',(-15.0169188528174,2.10494975158977,-0.450316148463807));
#54533=CARTESIAN_POINT('Ctrl Pts',(-14.90577250794,1.51982784235249,1.52437574760794));
#54534=CARTESIAN_POINT('Ctrl Pts',(-14.7946261630625,-0.456603527596969,
2.10359485378509));
#54535=CARTESIAN_POINT('Ctrl Pts',(-14.6834798181851,-2.01504228678013,
0.757101494367162));
#54536=CARTESIAN_POINT('Ctrl Pts',(-14.5723334733077,-1.72883304096769,
-1.28247199062728));
#54537=CARTESIAN_POINT('Ctrl Pts',(-14.4611871284303,0.140017145391684,
-2.14802078418285));
#54538=CARTESIAN_POINT('Ctrl Pts',(-14.3500407835528,1.88069019640931,-1.04718788926104));
#54539=CARTESIAN_POINT('Ctrl Pts',(-14.2388944386754,1.89970636628787,1.01228148860406));
#54540=CARTESIAN_POINT('Ctrl Pts',(-14.127748093798,0.179657514235822,2.14506905899641));
#54541=CARTESIAN_POINT('Ctrl Pts',(-14.0166017489206,-1.7048568070482,1.3141770648381));
#54542=CARTESIAN_POINT('Ctrl Pts',(-13.9054554040431,-2.02867896392615,
-0.719763677611344));
#54543=CARTESIAN_POINT('Ctrl Pts',(-13.7943090591657,-0.495369571687756,
-2.09480478272584));
#54544=CARTESIAN_POINT('Ctrl Pts',(-13.6831627142883,1.49142037435554,-1.55218019483637));
#54545=CARTESIAN_POINT('Ctrl Pts',(-13.5720163694109,2.11290615968028,0.411370454299073));
#54546=CARTESIAN_POINT('Ctrl Pts',(-13.4608700245335,0.800155548197115,
1.99833660552333));
#54547=CARTESIAN_POINT('Ctrl Pts',(-13.349723679656,-1.24508854262961,1.75594778148371));
#54548=CARTESIAN_POINT('Ctrl Pts',(-13.2385773347786,-2.15053020287081,
-0.0939038701307013));
#54549=CARTESIAN_POINT('Ctrl Pts',(-13.1274309899012,-1.08729295526273,
-1.85779227033627));
#54550=CARTESIAN_POINT('Ctrl Pts',(-13.0162846450238,0.971294511013014,
-1.92098544064266));
#54551=CARTESIAN_POINT('Ctrl Pts',(-12.9051383001463,2.14072124167643,-0.225633897542892));
#54552=CARTESIAN_POINT('Ctrl Pts',(-12.7939919552689,1.35044856870098,1.67627168250812));
#54553=CARTESIAN_POINT('Ctrl Pts',(-12.6828456103915,-0.676077196552766,
2.04365303184921));
#54554=CARTESIAN_POINT('Ctrl Pts',(-12.5716992655141,-2.08369562669698,
0.540194988470795));
#54555=CARTESIAN_POINT('Ctrl Pts',(-12.4605529206366,-1.583818116919,-1.45777853695418));
#54556=CARTESIAN_POINT('Ctrl Pts',(-12.3494065757592,0.365948037289866,
-2.12124494679158));
#54557=CARTESIAN_POINT('Ctrl Pts',(-12.2382602308818,1.98071113903302,-0.842841310090813));
#54558=CARTESIAN_POINT('Ctrl Pts',(-12.1271138860044,1.78225430238563,1.20713201097189));
#54559=CARTESIAN_POINT('Ctrl Pts',(-12.0159675411269,-0.0477473732258512,
2.15204978535236));
#54560=CARTESIAN_POINT('Ctrl Pts',(-11.9048211962495,-1.83403924813354,
1.12689756703564));
#54561=CARTESIAN_POINT('Ctrl Pts',(-11.7936748513721,-1.94138033260439,
-0.929860470426608));
#54562=CARTESIAN_POINT('Ctrl Pts',(-11.6825285064947,-0.271506427111522,
-2.13538810297384));
#54563=CARTESIAN_POINT('Ctrl Pts',(-11.5713821616172,1.64691501130435,-1.38609849427286));
#54564=CARTESIAN_POINT('Ctrl Pts',(-11.4602358167399,2.05768645650133,0.63207953377416));
#54565=CARTESIAN_POINT('Ctrl Pts',(-11.3490894718624,0.584771766775093,
2.07162739677478));
#54566=CARTESIAN_POINT('Ctrl Pts',(-11.237943126985,-1.42346571991491,1.61472704644229));
#54567=CARTESIAN_POINT('Ctrl Pts',(-11.1267967821076,-2.12860737698019,
-0.320357183391695));
#54568=CARTESIAN_POINT('Ctrl Pts',(-11.0156504372302,-0.885139132841,-1.96217399987834));
#54569=CARTESIAN_POINT('Ctrl Pts',(-10.9045040923527,1.16861986611292,-1.80774049542829));
#54570=CARTESIAN_POINT('Ctrl Pts',(-10.7933577474753,2.15257883220101,0.00156889937841303));
#54571=CARTESIAN_POINT('Ctrl Pts',(-10.6822114025979,1.16598349555022,1.80944206273359));
#54572=CARTESIAN_POINT('Ctrl Pts',(-10.5710650577204,-0.887998437915542,
1.96088165490543));
#54573=CARTESIAN_POINT('Ctrl Pts',(-10.459918712843,-2.12907209760132,0.317253988943611));
#54574=CARTESIAN_POINT('Ctrl Pts',(-10.3487723679656,-1.42111043276905,
-1.61680030559128));
#54575=CARTESIAN_POINT('Ctrl Pts',(-10.2376260230881,0.587790940318532,
-2.07077277864196));
#54576=CARTESIAN_POINT('Ctrl Pts',(-10.1264796782108,2.05860564766888,-0.629079389005017));
#54577=CARTESIAN_POINT('Ctrl Pts',(-10.0153333333333,1.64489275678552,1.38849771658423));
#54578=CARTESIAN_POINT('Ctrl Pts',(-9.90418698845591,-0.27461887695429,
2.1349900615004));
#54579=CARTESIAN_POINT('Ctrl Pts',(-9.79304064357848,-1.94273372024891,
0.927029547799284));
#54580=CARTESIAN_POINT('Ctrl Pts',(-9.68189429870106,-1.83239462994335,
-1.12956983424659));
#54581=CARTESIAN_POINT('Ctrl Pts',(-9.57074795382363,-0.0446102965948741,
-2.1521170999095));
#54582=CARTESIAN_POINT('Ctrl Pts',(-9.45960160894622,1.78401203561639,-1.20453275051405));
#54583=CARTESIAN_POINT('Ctrl Pts',(-9.34845526406878,1.97948043156636,0.845727681544679));
#54584=CARTESIAN_POINT('Ctrl Pts',(-9.23730891919137,0.362855526560633,
2.12177613266092));
#54585=CARTESIAN_POINT('Ctrl Pts',(-9.12616257431394,-1.5859414264279,1.45546826905465));
#54586=CARTESIAN_POINT('Ctrl Pts',(-9.01501622943652,-2.08290597495865,
-0.543231801137112));
#54587=CARTESIAN_POINT('Ctrl Pts',(-8.90386988455909,-0.673097461450849,
-2.0446363729704));
#54588=CARTESIAN_POINT('Ctrl Pts',(-8.79272353968167,1.35289062187478,-1.67430136341352));
#54589=CARTESIAN_POINT('Ctrl Pts',(-8.68157719480423,2.14039006255939,0.228754170196138));
#54590=CARTESIAN_POINT('Ctrl Pts',(-8.57043084992684,0.968493273837022,
1.92239924802773));
#54591=CARTESIAN_POINT('Ctrl Pts',(-8.45928450504939,-1.089999889143,1.8562053582385));
#54592=CARTESIAN_POINT('Ctrl Pts',(-8.34813816017197,-2.15066480100183,
0.0907689595448498));
#54593=CARTESIAN_POINT('Ctrl Pts',(-8.23699181529456,-1.24252758865235,
-1.75776087159856));
#54594=CARTESIAN_POINT('Ctrl Pts',(-8.12584547041711,0.803067657504474,
-1.99716810202731));
#54595=CARTESIAN_POINT('Ctrl Pts',(-8.01469912553972,2.11350356630602,-0.408290050695375));
#54596=CARTESIAN_POINT('Ctrl Pts',(-7.90355278066228,1.48915618906188,1.55435257739802));
#54597=CARTESIAN_POINT('Ctrl Pts',(-7.79240643578487,-0.498422625706736,
2.09408046083924));
#54598=CARTESIAN_POINT('Ctrl Pts',(-7.68126009090743,-2.02972600239322,
0.71680572367549));
#54599=CARTESIAN_POINT('Ctrl Pts',(-7.57011374603002,-1.7029393302673,-1.3166608248573));
#54600=CARTESIAN_POINT('Ctrl Pts',(-7.45896740115258,0.182784173514752,
-2.14480489466936));
#54601=CARTESIAN_POINT('Ctrl Pts',(-7.34782105627517,1.90117994267266,-1.00951122622003));
#54602=CARTESIAN_POINT('Ctrl Pts',(-7.23667471139775,1.87916172082065,1.04992824387551));
#54603=CARTESIAN_POINT('Ctrl Pts',(-7.12552836652031,0.136885843773243,
2.14822260393554));
#54604=CARTESIAN_POINT('Ctrl Pts',(-7.0143820216429,-1.73070065344576,1.27995052187477));
#54605=CARTESIAN_POINT('Ctrl Pts',(-6.90323567676547,-2.01393652508823,
-0.760038001155664));
#54606=CARTESIAN_POINT('Ctrl Pts',(-6.79208933188806,-0.453536648952868,
-2.10425820619564));
#54607=CARTESIAN_POINT('Ctrl Pts',(-6.68094298701061,1.52204829807255,-1.52215868706898));
#54608=CARTESIAN_POINT('Ctrl Pts',(-6.56979664213322,2.10429109294252,0.45338403858971));
#54609=CARTESIAN_POINT('Ctrl Pts',(-6.45865029725577,0.760184057839905,
2.01388139881452));
#54610=CARTESIAN_POINT('Ctrl Pts',(-6.34750395237836,-1.27982500121702,
1.73079347599445));
#54611=CARTESIAN_POINT('Ctrl Pts',(-6.23635760750093,-2.14823252579159,
-0.136730045769932));
#54612=CARTESIAN_POINT('Ctrl Pts',(-6.12521126262351,-1.05006452539279,
-1.87908557090855));
#54613=CARTESIAN_POINT('Ctrl Pts',(-6.01406491774608,1.00937334243772,-1.90125315144018));
#54614=CARTESIAN_POINT('Ctrl Pts',(-5.90291857286866,2.14479163279392,-0.182939722811514));
#54615=CARTESIAN_POINT('Ctrl Pts',(-5.79177222799124,1.31678432532478,1.7028438363115));
#54616=CARTESIAN_POINT('Ctrl Pts',(-5.6806258831138,-0.716658517991673,
2.02977798265601));
#54617=CARTESIAN_POINT('Ctrl Pts',(-5.5694795382364,-2.09404430774185,0.498574495435823));
#54618=CARTESIAN_POINT('Ctrl Pts',(-5.45833319335896,-1.55446057283712,
-1.48904345731747));
#54619=CARTESIAN_POINT('Ctrl Pts',(-5.34718684848155,0.408136769940926,
-2.1135331715654));
#54620=CARTESIAN_POINT('Ctrl Pts',(-5.23604050360411,1.99710985511599,-0.803212497962859));
#54621=CARTESIAN_POINT('Ctrl Pts',(-5.1248941587267,1.75785098001617,1.24240010557842));
#54622=CARTESIAN_POINT('Ctrl Pts',(-5.01374781384926,-0.0906129845449661,
2.15067137827167));
#54623=CARTESIAN_POINT('Ctrl Pts',(-4.90260146897186,-1.85612630223178,
1.09013450566824));
#54624=CARTESIAN_POINT('Ctrl Pts',(-4.79145512409441,-1.92246948195445,
-0.968353851254212));
#54625=CARTESIAN_POINT('Ctrl Pts',(-4.68030877921701,-0.228909399190852,
-2.14037346676862));
#54626=CARTESIAN_POINT('Ctrl Pts',(-4.56916243433958,1.67420324200416,-1.35301204530782));
#54627=CARTESIAN_POINT('Ctrl Pts',(-4.45801608946216,2.04468518329698,0.672949174522688));
#54628=CARTESIAN_POINT('Ctrl Pts',(-4.34686974458473,0.543382860330313,
2.082866572151));
#54629=CARTESIAN_POINT('Ctrl Pts',(-4.23572339970731,-1.4553532464501,1.58604697860226));
#54630=CARTESIAN_POINT('Ctrl Pts',(-4.12457705482988,-2.1218024428059,-0.362701645966607));
#54631=CARTESIAN_POINT('Ctrl Pts',(-4.01343070995247,-0.845871239111339,
-1.97941909082634));
#54632=CARTESIAN_POINT('Ctrl Pts',(-3.90228436507503,1.20440336370244,-1.78409938842956));
#54633=CARTESIAN_POINT('Ctrl Pts',(-3.79113802019762,2.15212032956352,0.0444542163922969));
#54634=CARTESIAN_POINT('Ctrl Pts',(-3.67999167532019,1.12970272382336,1.8323127042249));
#54635=CARTESIAN_POINT('Ctrl Pts',(-3.56884533044277,-0.926888650596847,
1.94280094701669));
#54636=CARTESIAN_POINT('Ctrl Pts',(-3.45769898556534,-2.13497013941755,
0.274773714182162));
#54637=CARTESIAN_POINT('Ctrl Pts',(-3.34655264068793,-1.3886170071239,-1.64479205305372));
#54638=CARTESIAN_POINT('Ctrl Pts',(-3.23540629581049,0.628930089141089,
-2.05865126565347));
#54639=CARTESIAN_POINT('Ctrl Pts',(-3.12425995093308,2.07073014415415,-0.587941119332112));
#54640=CARTESIAN_POINT('Ctrl Pts',(-3.01311360605564,1.61690336611955,1.42099317202789));
#54641=CARTESIAN_POINT('Ctrl Pts',(-2.90196726117823,-0.317099579721297,
2.12909510093774));
#54642=CARTESIAN_POINT('Ctrl Pts',(-2.7908209163008,-1.96081724784028,0.888140645723541));
#54643=CARTESIAN_POINT('Ctrl Pts',(-2.67967457142338,-1.80952662112472,
-1.16585226305009));
#54644=CARTESIAN_POINT('Ctrl Pts',(-2.56852822654596,-0.00172501030186185,
-2.15257871561459));
#54645=CARTESIAN_POINT('Ctrl Pts',(-2.45738188166853,1.80765573268103,-1.16875096213131));
#54646=CARTESIAN_POINT('Ctrl Pts',(-2.34623553679111,1.96223819810419,0.8849968155145));
#54647=CARTESIAN_POINT('Ctrl Pts',(-2.23508919191368,0.320511539399493,
2.12858415747483));
#54648=CARTESIAN_POINT('Ctrl Pts',(-2.12394284703626,-1.61462377214598,
1.42358278518015));
#54649=CARTESIAN_POINT('Ctrl Pts',(-2.01279650215883,-2.07166986722666,
-0.584621451407953));
#54650=CARTESIAN_POINT('Ctrl Pts',(-1.90165015728142,-0.632228638303536,
-2.05764074556303));
#54651=CARTESIAN_POINT('Ctrl Pts',(-1.79050381240399,1.38597881123994,-1.64701527479129));
#54652=CARTESIAN_POINT('Ctrl Pts',(-1.67935746752657,2.1354082418958,0.271351069624803));
#54653=CARTESIAN_POINT('Ctrl Pts',(-1.56821112264915,0.930000401328434,
1.94131382231481));
#54654=CARTESIAN_POINT('Ctrl Pts',(-1.45706477777172,-1.12676291008018,
1.83411919750027));
#54655=CARTESIAN_POINT('Ctrl Pts',(-1.3459184328943,-2.1520494407184,0.0479068208384009));
#54656=CARTESIAN_POINT('Ctrl Pts',(-1.23477208801687,-1.207255321557,-1.78217316714502));
#54657=CARTESIAN_POINT('Ctrl Pts',(-1.12362574313945,0.842686354777153,
-1.98076005610316));
#54658=CARTESIAN_POINT('Ctrl Pts',(-1.01247939826203,2.12123990456699,-0.36612509262031));
#54659=CARTESIAN_POINT('Ctrl Pts',(-0.901333053384604,1.45785249247625,
1.58375655078235));
#54660=CARTESIAN_POINT('Ctrl Pts',(-0.790186708507176,-0.539966053591598,
2.0836507866298));
#54661=CARTESIAN_POINT('Ctrl Pts',(-0.679040363629756,-2.04375204222851,
0.67638525475331));
#54662=CARTESIAN_POINT('Ctrl Pts',(-0.567894018752329,-1.67608780670706,
-1.35063135310715));
#54663=CARTESIAN_POINT('Ctrl Pts',(-0.456747673874911,0.224940970347859,
-2.14015615627215));
#54664=CARTESIAN_POINT('Ctrl Pts',(-0.345601328997483,1.92195148180026,
-0.9725611407687));
#54665=CARTESIAN_POINT('Ctrl Pts',(-0.234454984120063,1.85578172498221,
1.08948404228951));
#54666=CARTESIAN_POINT('Ctrl Pts',(-0.160357420868444,0.684627163603588,
1.79296350055041));
#54667=CARTESIAN_POINT('Ctrl Pts',(-0.123308639242636,0.0795783122553931,
1.81942719557457));
#54668=CARTESIAN_POINT('Ctrl Pts',(-29.7226913607573,0.98077109908131,-1.37424797458511));
#54669=CARTESIAN_POINT('Ctrl Pts',(-29.6856425791315,1.43777600728141,-1.04809344178598));
#54670=CARTESIAN_POINT('Ctrl Pts',(-29.6115450158799,1.99294814415539,0.0902923701931233));
#54671=CARTESIAN_POINT('Ctrl Pts',(-29.5003986710025,1.00294810174865,1.72676419011022));
#54672=CARTESIAN_POINT('Ctrl Pts',(-29.389252326125,-0.906020001401381,
1.77738379211666));
#54673=CARTESIAN_POINT('Ctrl Pts',(-29.2781059812477,-1.98514555704351,
0.203480774053002));
#54674=CARTESIAN_POINT('Ctrl Pts',(-29.1669596363702,-1.24722132427754,
-1.55803004483504));
#54675=CARTESIAN_POINT('Ctrl Pts',(-29.0558132914928,0.632578469051131,
-1.89256020159966));
#54676=CARTESIAN_POINT('Ctrl Pts',(-28.9446669466154,1.93322790184544,-0.494934700673032));
#54677=CARTESIAN_POINT('Ctrl Pts',(-28.8335206017379,1.46415875198014,1.35596641802415));
#54678=CARTESIAN_POINT('Ctrl Pts',(-28.7223742568606,-0.345275744785372,
1.96546165041682));
#54679=CARTESIAN_POINT('Ctrl Pts',(-28.6112279119831,-1.83862219115491,
0.775750297123293));
#54680=CARTESIAN_POINT('Ctrl Pts',(-28.5000815671057,-1.64882728862394,
-1.12414108072153));
#54681=CARTESIAN_POINT('Ctrl Pts',(-28.3889352222282,0.0503707273899882,
-1.99493528311385));
#54682=CARTESIAN_POINT('Ctrl Pts',(-28.2777888773509,1.70345608327842,-1.03949596735827));
#54683=CARTESIAN_POINT('Ctrl Pts',(-28.1666425324734,1.79713225566867,0.867542423566838));
#54684=CARTESIAN_POINT('Ctrl Pts',(-28.055496187596,0.245643362512984,1.98039662815554));
#54685=CARTESIAN_POINT('Ctrl Pts',(-27.9443498427186,-1.5307168147738,1.28031993634082));
#54686=CARTESIAN_POINT('Ctrl Pts',(-27.8332034978412,-1.90579944516041,
-0.591811964992614));
#54687=CARTESIAN_POINT('Ctrl Pts',(-27.7220571529637,-0.536239158707246,
-1.92217588705377));
#54688=CARTESIAN_POINT('Ctrl Pts',(-27.6109108080863,1.32421526126029,-1.4929054784601));
#54689=CARTESIAN_POINT('Ctrl Pts',(-27.4997644632089,1.97243159274787,0.30302869888381));
#54690=CARTESIAN_POINT('Ctrl Pts',(-27.3886181183314,0.815007396411317,
1.82155858568272));
#54691=CARTESIAN_POINT('Ctrl Pts',(-27.277471773454,-1.08850623409605,1.67256298917007));
#54692=CARTESIAN_POINT('Ctrl Pts',(-27.1663254285766,-1.99555896550728,
-0.00756176856515067));
#54693=CARTESIAN_POINT('Ctrl Pts',(-27.0551790836992,-1.07579948011766,
-1.68076418296882));
#54694=CARTESIAN_POINT('Ctrl Pts',(-26.9440327388218,0.828788649609528,
-1.8153297606358));
#54695=CARTESIAN_POINT('Ctrl Pts',(-26.8328863939443,1.97467144671743,-0.288071937874124));
#54696=CARTESIAN_POINT('Ctrl Pts',(-26.721740049067,1.31286327429152,1.50289812907108));
#54697=CARTESIAN_POINT('Ctrl Pts',(-26.6105937041895,-0.550790951424447,
1.9180568531578));
#54698=CARTESIAN_POINT('Ctrl Pts',(-26.4994473593121,-1.91022973893913,
0.577351806350263));
#54699=CARTESIAN_POINT('Ctrl Pts',(-26.3883010144347,-1.52097000028234,
-1.2918835172025));
#54700=CARTESIAN_POINT('Ctrl Pts',(-26.2771546695572,0.260644774822252,
-1.9784784722718));
#54701=CARTESIAN_POINT('Ctrl Pts',(-26.1660083246798,1.80365519555206,-0.853897358817045));
#54702=CARTESIAN_POINT('Ctrl Pts',(-26.0548619798023,1.69552956816522,1.0523745755729));
#54703=CARTESIAN_POINT('Ctrl Pts',(-25.943715634925,0.0352502932630832,
1.99526193284844));
#54704=CARTESIAN_POINT('Ctrl Pts',(-25.8325692900475,-1.65729846976434,
1.1116089896894));
#54705=CARTESIAN_POINT('Ctrl Pts',(-25.7214229451701,-1.83269181824256,
-0.789654014862648));
#54706=CARTESIAN_POINT('Ctrl Pts',(-25.6102766002927,-0.330367865961598,
-1.96803705173043));
#54707=CARTESIAN_POINT('Ctrl Pts',(-25.4991302554152,1.47438766746241,-1.3448025021829));
#54708=CARTESIAN_POINT('Ctrl Pts',(-25.3879839105379,1.9294314418738,0.509516510970531));
#54709=CARTESIAN_POINT('Ctrl Pts',(-25.2768375656604,0.618198705177624,
1.89740431241202));
#54710=CARTESIAN_POINT('Ctrl Pts',(-25.165691220783,-1.25895714671978,1.54833448148843));
#54711=CARTESIAN_POINT('Ctrl Pts',(-25.0545448759056,-1.98361470897458,
-0.218140895254885));
#54712=CARTESIAN_POINT('Ctrl Pts',(-24.9433985310281,-0.892394292094368,
-1.78492162048654));
#54713=CARTESIAN_POINT('Ctrl Pts',(-24.8322521861507,1.01575853428468,-1.71771574012429));
#54714=CARTESIAN_POINT('Ctrl Pts',(-24.7211058412733,1.99404653047223,-0.0780461283765578));
#54715=CARTESIAN_POINT('Ctrl Pts',(-24.6099594963959,1.14690685279113,1.63306994181622));
#54716=CARTESIAN_POINT('Ctrl Pts',(-24.4988131515184,-0.750155921688874,
1.84921033335801));
#54717=CARTESIAN_POINT('Ctrl Pts',(-24.387666806641,-1.96049681769646,0.372511733566841));
#54718=CARTESIAN_POINT('Ctrl Pts',(-24.2765204617636,-1.37612275050455,
-1.44519858129832));
#54719=CARTESIAN_POINT('Ctrl Pts',(-24.1653741168862,0.468007552574359,
-1.93991796078501));
#54720=CARTESIAN_POINT('Ctrl Pts',(-24.0542277720088,1.88370555731245,-0.658761062292782));
#54721=CARTESIAN_POINT('Ctrl Pts',(-23.9430814271313,1.57498630237707,1.22545130917859));
#54722=CARTESIAN_POINT('Ctrl Pts',(-23.8319350822539,-0.175536610792046,
1.98783793658199));
#54723=CARTESIAN_POINT('Ctrl Pts',(-23.7207887373765,-1.76536648986179,
0.930480478202514));
#54724=CARTESIAN_POINT('Ctrl Pts',(-23.609642392499,-1.73911128973787,-0.978674964300812));
#54725=CARTESIAN_POINT('Ctrl Pts',(-23.4984960476217,-0.120806040775277,
-1.99191331748023));
#54726=CARTESIAN_POINT('Ctrl Pts',(-23.3873497027442,1.6080897519042,-1.18167682285115));
#54727=CARTESIAN_POINT('Ctrl Pts',(-23.2762033578668,1.86487770239841,0.710312550177829));
#54728=CARTESIAN_POINT('Ctrl Pts',(-23.1650570129894,0.414484143175073,
1.9520542151537));
#54729=CARTESIAN_POINT('Ctrl Pts',(-23.053910668112,-1.4153443057408,1.40680960334012));
#54730=CARTESIAN_POINT('Ctrl Pts',(-22.9427643232345,-1.94951158312934,
-0.426283181802225));
#54731=CARTESIAN_POINT('Ctrl Pts',(-22.8316179783571,-0.699020207879015,
-1.86913977883402));
#54732=CARTESIAN_POINT('Ctrl Pts',(-22.7204716334796,1.19138142651335,-1.60091319577356));
#54733=CARTESIAN_POINT('Ctrl Pts',(-22.6093252886023,1.99114621123524,0.132851531140779));
#54734=CARTESIAN_POINT('Ctrl Pts',(-22.4981789437248,0.968138387011664,
1.7449988044229));
#54735=CARTESIAN_POINT('Ctrl Pts',(-22.3870325988474,-0.941140934280283,
1.75970636916075));
#54736=CARTESIAN_POINT('Ctrl Pts',(-22.27588625397,-1.98886327573639,0.163510349122069));
#54737=CARTESIAN_POINT('Ctrl Pts',(-22.1647399090925,-1.21590289610751,
-1.58236939779569));
#54738=CARTESIAN_POINT('Ctrl Pts',(-22.0535935642152,0.670142239254753,
-1.87968671405889));
#54739=CARTESIAN_POINT('Ctrl Pts',(-21.9424472193377,1.94271313002443,-0.456265775917509));
#54740=CARTESIAN_POINT('Ctrl Pts',(-21.8313008744603,1.43684893628544,1.38483858197925));
#54741=CARTESIAN_POINT('Ctrl Pts',(-21.7201545295828,-0.384362603356758,
1.95820789319819));
#54742=CARTESIAN_POINT('Ctrl Pts',(-21.6090081847055,-1.85371368124662,
0.738957611640905));
#54743=CARTESIAN_POINT('Ctrl Pts',(-21.497861839828,-1.62610322816601,-1.15676318025385));
#54744=CARTESIAN_POINT('Ctrl Pts',(-21.3867154949506,0.0901053031943518,
-1.9935380102168));
#54745=CARTESIAN_POINT('Ctrl Pts',(-21.2755691500732,1.72382793891499,-1.00535068551179));
#54746=CARTESIAN_POINT('Ctrl Pts',(-21.1644228051957,1.77949149898398,0.903173720214814));
#54747=CARTESIAN_POINT('Ctrl Pts',(-21.0532764603183,0.206139397673152,
1.98489780909996));
#54748=CARTESIAN_POINT('Ctrl Pts',(-20.9421301154409,-1.55592071793766,
1.24956931913971));
#54749=CARTESIAN_POINT('Ctrl Pts',(-20.8309837705635,-1.89363055211529,
-0.62966347832668));
#54750=CARTESIAN_POINT('Ctrl Pts',(-20.719837425686,-0.497837400735304,
-1.93247786178057));
#54751=CARTESIAN_POINT('Ctrl Pts',(-20.6086910808086,1.35369545104868,-1.46622692297373));
#54752=CARTESIAN_POINT('Ctrl Pts',(-20.4975447359312,1.96600288829374,0.342265112250096));
#54753=CARTESIAN_POINT('Ctrl Pts',(-20.3863983910538,0.778554891372885,
1.83743436480388));
#54754=CARTESIAN_POINT('Ctrl Pts',(-20.2752520461764,-1.12161250432815,
1.6505448052015));
#54755=CARTESIAN_POINT('Ctrl Pts',(-20.1641057012989,-1.99501223264037,
-0.0473176019910748));
#54756=CARTESIAN_POINT('Ctrl Pts',(-20.0529593564215,-1.04210024579629,
-1.7018636377672));
#54757=CARTESIAN_POINT('Ctrl Pts',(-19.9418130115441,0.86479079748002,-1.79845757259847));
#54758=CARTESIAN_POINT('Ctrl Pts',(-19.8306666666667,1.98001874277781,-0.248673565325042));
#54759=CARTESIAN_POINT('Ctrl Pts',(-19.7195203217893,1.28266059612054,1.52875588600751));
#54760=CARTESIAN_POINT('Ctrl Pts',(-19.6083739769118,-0.588894898772527,
1.90670279856159));
#54761=CARTESIAN_POINT('Ctrl Pts',(-19.4972276320344,-1.9213531214646,0.539179883231139));
#54762=CARTESIAN_POINT('Ctrl Pts',(-19.386081287157,-1.49493004143963,-1.32192924736697));
#54763=CARTESIAN_POINT('Ctrl Pts',(-19.2749349422796,0.300010084922888,
-1.97289298057129));
#54764=CARTESIAN_POINT('Ctrl Pts',(-19.1637885974021,1.82030932247515,-0.81779382142016));
#54765=CARTESIAN_POINT('Ctrl Pts',(-19.0526422525247,1.67422667702274,1.08594557772859));
#54766=CARTESIAN_POINT('Ctrl Pts',(-18.9414959076473,-0.00450812165834452,
1.9955681999576));
#54767=CARTESIAN_POINT('Ctrl Pts',(-18.8303495627698,-1.67911601060762,
1.07837015294568));
#54768=CARTESIAN_POINT('Ctrl Pts',(-18.7192032178924,-1.81659586038661,
-0.826009832792037));
#54769=CARTESIAN_POINT('Ctrl Pts',(-18.608056873015,-0.291093274645596,
-1.97422832248426));
#54770=CARTESIAN_POINT('Ctrl Pts',(-18.4969105281376,1.50088740530984,-1.31516149594839));
#54771=CARTESIAN_POINT('Ctrl Pts',(-18.3857641832602,1.91889743656399,0.547855265367661));
#54772=CARTESIAN_POINT('Ctrl Pts',(-18.2746178383827,0.580274194476223,
1.9093440295211));
#54773=CARTESIAN_POINT('Ctrl Pts',(-18.1634714935053,-1.28955459213706,
1.52294508034306));
#54774=CARTESIAN_POINT('Ctrl Pts',(-18.0523251486279,-1.97887499869068,
-0.257616970325887));
#54775=CARTESIAN_POINT('Ctrl Pts',(-17.9411788037505,-0.856656341067444,
-1.80234643649655));
#54776=CARTESIAN_POINT('Ctrl Pts',(-17.830032458873,1.04977881706505,-1.69713794344609));
#54777=CARTESIAN_POINT('Ctrl Pts',(-17.7188861139956,1.9952056562704,-0.0383034336519918));
#54778=CARTESIAN_POINT('Ctrl Pts',(-17.6077397691182,1.11414371281292,1.65559552761003));
#54779=CARTESIAN_POINT('Ctrl Pts',(-17.4965934242408,-0.786848676075942,
1.83389801374025));
#54780=CARTESIAN_POINT('Ctrl Pts',(-17.3854470793633,-1.96752921340748,
0.333379000884986));
#54781=CARTESIAN_POINT('Ctrl Pts',(-17.2743007344859,-1.3470570592577,-1.4723281030215));
#54782=CARTESIAN_POINT('Ctrl Pts',(-17.1631543896085,0.506563467646839,
-1.93020885323027));
#54783=CARTESIAN_POINT('Ctrl Pts',(-17.0520080447311,1.89645611344,-0.621101419768934));
#54784=CARTESIAN_POINT('Ctrl Pts',(-16.9408616998537,1.55025914505001,1.25658638661721));
#54785=CARTESIAN_POINT('Ctrl Pts',(-16.8297153549762,-0.215105280967968,
1.98394618927596));
#54786=CARTESIAN_POINT('Ctrl Pts',(-16.7185690100988,-1.78355397474313,
0.895124562851952));
#54787=CARTESIAN_POINT('Ctrl Pts',(-16.6074226652214,-1.71926805897861,
-1.01312886900871));
#54788=CARTESIAN_POINT('Ctrl Pts',(-16.496276320344,-0.0810973588330665,
-1.9939247684487));
#54789=CARTESIAN_POINT('Ctrl Pts',(-16.3851299754665,1.63131301467479,-1.14940445970753));
#54790=CARTESIAN_POINT('Ctrl Pts',(-16.2739836305891,1.85035606890338,0.747325352249846));
#54791=CARTESIAN_POINT('Ctrl Pts',(-16.1628372857117,0.375511280962539,
1.95992449898274));
#54792=CARTESIAN_POINT('Ctrl Pts',(-16.0516909408343,-1.44309112428753,
1.37833260530449));
#54793=CARTESIAN_POINT('Ctrl Pts',(-15.9405445959568,-1.94063184219332,
-0.465038511209882));
#54794=CARTESIAN_POINT('Ctrl Pts',(-15.8293982510794,-0.661642767340725,
-1.88269530521234));
#54795=CARTESIAN_POINT('Ctrl Pts',(-15.718251906202,1.22303980526226,-1.57685966356773));
#54796=CARTESIAN_POINT('Ctrl Pts',(-15.6071055613246,1.98810421818273,0.172494583935125));
#54797=CARTESIAN_POINT('Ctrl Pts',(-15.4959592164471,0.933180780796459,
1.76394058692321));
#54798=CARTESIAN_POINT('Ctrl Pts',(-15.3848128715697,-0.976012602630028,
1.74060683767192));
#54799=CARTESIAN_POINT('Ctrl Pts',(-15.2736665266923,-1.9917261260537,0.123853956892735));
#54800=CARTESIAN_POINT('Ctrl Pts',(-15.1625201818149,-1.18413616397418,
-1.60627964844588));
#54801=CARTESIAN_POINT('Ctrl Pts',(-15.0513738369374,0.707458052928451,
-1.86596245063764));
#54802=CARTESIAN_POINT('Ctrl Pts',(-14.94022749206,1.95141767947325,-0.417470722425096));
#54803=CARTESIAN_POINT('Ctrl Pts',(-14.8290811471826,1.40897373872346,1.41318992617077));
#54804=CARTESIAN_POINT('Ctrl Pts',(-14.7179348023052,-0.423299508973792,
1.95016160600743));
#54805=CARTESIAN_POINT('Ctrl Pts',(-14.6067884574277,-1.86806793860003,
0.70187957700558));
#54806=CARTESIAN_POINT('Ctrl Pts',(-14.4956421125503,-1.60273439233121,
-1.18893028873925));
#54807=CARTESIAN_POINT('Ctrl Pts',(-14.3844957676729,0.129804491884053,
-1.99134717157247));
#54808=CARTESIAN_POINT('Ctrl Pts',(-14.2733494227955,1.74351530059724,-0.970807478559067));
#54809=CARTESIAN_POINT('Ctrl Pts',(-14.1622030779181,1.7611444578106,0.938447101634346));
#54810=CARTESIAN_POINT('Ctrl Pts',(-14.0510567330406,0.166553548019546,
1.98861074106649));
#54811=CARTESIAN_POINT('Ctrl Pts',(-13.9399103881632,-1.58050695116664,
1.21832283946285));
#54812=CARTESIAN_POINT('Ctrl Pts',(-13.8287640432858,-1.88070997570899,
-0.667265128049994));
#54813=CARTESIAN_POINT('Ctrl Pts',(-13.7176176984084,-0.459238012372806,
-1.94201267035898));
#54814=CARTESIAN_POINT('Ctrl Pts',(-13.606471353531,1.38263827145797,-1.43896635615383));
#54815=CARTESIAN_POINT('Ctrl Pts',(-13.4953250086535,1.95879375835649,0.381365672375669));
#54816=CARTESIAN_POINT('Ctrl Pts',(-13.3841786637761,0.741793328748737,
1.85258074622047));
#54817=CARTESIAN_POINT('Ctrl Pts',(-13.2730323188987,-1.15427353682048,
1.6278714218386));
#54818=CARTESIAN_POINT('Ctrl Pts',(-13.1618859740213,-1.99367355679339,
-0.0870546540151287));
#54819=CARTESIAN_POINT('Ctrl Pts',(-13.0507396291438,-1.00798733749538,
-1.72228751702261));
#54820=CARTESIAN_POINT('Ctrl Pts',(-12.9395932842664,0.900449656498692,
-1.78087146643273));
#54821=CARTESIAN_POINT('Ctrl Pts',(-12.828446939389,1.98458004742218,-0.209176478640999));
#54822=CARTESIAN_POINT('Ctrl Pts',(-12.7173005945116,1.25194875088693,1.5540067853763));
#54823=CARTESIAN_POINT('Ctrl Pts',(-12.6061542496341,-0.626765077430113,
1.89459185619408));
#54824=CARTESIAN_POINT('Ctrl Pts',(-12.4950079047567,-1.93171380053448,
0.500793926348479));
#54825=CARTESIAN_POINT('Ctrl Pts',(-12.3838615598793,-1.46829665273085,
-1.35145022232501));
#54826=CARTESIAN_POINT('Ctrl Pts',(-12.2727152150019,0.33925630253003,-1.96652432607292));
#54827=CARTESIAN_POINT('Ctrl Pts',(-12.1615688701244,1.83624085644772,-0.781365651251085));
#54828=CARTESIAN_POINT('Ctrl Pts',(-12.050422525247,1.65225918213296,1.1190855011572));
#54829=CARTESIAN_POINT('Ctrl Pts',(-11.9392761803696,-0.0442647470282004,
1.99508230306758));
#54830=CARTESIAN_POINT('Ctrl Pts',(-11.8281298354922,-1.70026700682643,
1.04470324462997));
#54831=CARTESIAN_POINT('Ctrl Pts',(-11.7169834906148,-1.79977878368105,
-0.862037756513309));
#54832=CARTESIAN_POINT('Ctrl Pts',(-11.6058371457373,-0.251703130469517,
-1.97963590035004));
#54833=CARTESIAN_POINT('Ctrl Pts',(-11.4946908008599,1.52679134844995,-1.28499842106567));
#54834=CARTESIAN_POINT('Ctrl Pts',(-11.3835444559825,1.90760170260443,0.585976542246873));
#54835=CARTESIAN_POINT('Ctrl Pts',(-11.272398111105,0.542119337186086,1.92052581031649));
#54836=CARTESIAN_POINT('Ctrl Pts',(-11.1612517662276,-1.31964013386451,
1.49695112843972));
#54837=CARTESIAN_POINT('Ctrl Pts',(-11.0501054213502,-1.97334975096636,
-0.296990781345034));
#54838=CARTESIAN_POINT('Ctrl Pts',(-10.9389590764728,-0.820578330345012,
-1.81905579013154));
#54839=CARTESIAN_POINT('Ctrl Pts',(-10.8278127315954,1.08338237793752,-1.67588644812748));
#54840=CARTESIAN_POINT('Ctrl Pts',(-10.7166663867179,1.99557276198374,0.00145446606594789));
#54841=CARTESIAN_POINT('Ctrl Pts',(-10.6055200418405,1.08093830053302,1.67746390550846));
#54842=CARTESIAN_POINT('Ctrl Pts',(-10.4943736969631,-0.823229081731838,
1.817857706982));
#54843=CARTESIAN_POINT('Ctrl Pts',(-10.3832273520857,-1.97378057551948,
0.294113929532303));
#54844=CARTESIAN_POINT('Ctrl Pts',(-10.2720810072083,-1.31745663804804,
-1.49887316698446));
#54845=CARTESIAN_POINT('Ctrl Pts',(-10.1609346623308,0.544918296460699,
-1.91973352682743));
#54846=CARTESIAN_POINT('Ctrl Pts',(-10.0497883174534,1.90845384926197,-0.583195223814541));
#54847=CARTESIAN_POINT('Ctrl Pts',(-9.93864197257597,1.52491659432944,1.28722264747851));
#54848=CARTESIAN_POINT('Ctrl Pts',(-9.82749562769855,-0.254588562601471,
1.97926689146143));
#54849=CARTESIAN_POINT('Ctrl Pts',(-9.71634928282112,-1.80103345713564,
0.859413317397949));
#54850=CARTESIAN_POINT('Ctrl Pts',(-9.60520293794371,-1.69874234477226,
-1.04718060043171));
#54851=CARTESIAN_POINT('Ctrl Pts',(-9.49405659306628,-0.0413564843513104,
-1.99514470779566));
#54852=CARTESIAN_POINT('Ctrl Pts',(-9.38291024818885,1.65388870877585,-1.11667582709874));
#54853=CARTESIAN_POINT('Ctrl Pts',(-9.27176390331144,1.83509991505148,0.784041494833618));
#54854=CARTESIAN_POINT('Ctrl Pts',(-9.16061755843401,0.336389355180736,
1.96701676799259));
#54855=CARTESIAN_POINT('Ctrl Pts',(-9.04947121355659,-1.47026509103269,
1.3493084621144));
#54856=CARTESIAN_POINT('Ctrl Pts',(-8.93832486867916,-1.93098174488252,
-0.503609238173173));
#54857=CARTESIAN_POINT('Ctrl Pts',(-8.82717852380175,-0.62400268001261,
-1.89550347379793));
#54858=CARTESIAN_POINT('Ctrl Pts',(-8.71603217892431,1.25421268413938,-1.55218017858327));
#54859=CARTESIAN_POINT('Ctrl Pts',(-8.60488583404689,1.9842730240438,0.212069162998644));
#54860=CARTESIAN_POINT('Ctrl Pts',(-8.49373948916947,0.897852737619631,
1.78218215269705));
#54861=CARTESIAN_POINT('Ctrl Pts',(-8.38259314429204,-1.01049683142839,
1.7208163520597));
#54862=CARTESIAN_POINT('Ctrl Pts',(-8.27144679941463,-1.99379833752617,
0.084148399395079));
#54863=CARTESIAN_POINT('Ctrl Pts',(-8.16030045453719,-1.15189937522182,
-1.62955226771236));
#54864=CARTESIAN_POINT('Ctrl Pts',(-8.04915410965978,0.744493032901956,
-1.8514974717248));
#54865=CARTESIAN_POINT('Ctrl Pts',(-7.93800776478235,1.95934759098379,-0.378509949075211));
#54866=CARTESIAN_POINT('Ctrl Pts',(-7.82686141990493,1.38053923265282,1.44098028818902));
#54867=CARTESIAN_POINT('Ctrl Pts',(-7.71571507502751,-0.46206838092876,
1.94134117949132));
#54868=CARTESIAN_POINT('Ctrl Pts',(-7.60456873015007,-1.88168064466396,
0.664522923110952));
#54869=CARTESIAN_POINT('Ctrl Pts',(-7.49342238527267,-1.57872933244332,
-1.22062543752209));
#54870=CARTESIAN_POINT('Ctrl Pts',(-7.38227604039523,0.169452153171387,
-1.98836584451364));
#54871=CARTESIAN_POINT('Ctrl Pts',(-7.27112969551781,1.76251055360792,-0.93587889828952));
#54872=CARTESIAN_POINT('Ctrl Pts',(-7.1599833506404,1.74209830986671,0.973347955564964));
#54873=CARTESIAN_POINT('Ctrl Pts',(-7.04883700576295,0.126901582998413,
1.99153427087645));
#54874=CARTESIAN_POINT('Ctrl Pts',(-6.93769066088555,-1.60446578378376,
1.18659273236863));
#54875=CARTESIAN_POINT('Ctrl Pts',(-6.82654431600812,-1.86704282960959,
-0.704601899122013));
#54876=CARTESIAN_POINT('Ctrl Pts',(-6.71539797113069,-0.420456324141416,
-1.9507765744268));
#54877=CARTESIAN_POINT('Ctrl Pts',(-6.60425162625326,1.41103223752855,-1.41113457490704));
#54878=CARTESIAN_POINT('Ctrl Pts',(-6.49310528137585,1.95080706246068,0.420314844963218));
#54879=CARTESIAN_POINT('Ctrl Pts',(-6.38195893649842,0.704737302637404,
1.86699172416866));
#54880=CARTESIAN_POINT('Ctrl Pts',(-6.27081259162099,-1.18647636701088,
1.60455183598647));
#54881=CARTESIAN_POINT('Ctrl Pts',(-6.15966624674359,-1.99154346904629,
-0.126757148682046));
#54882=CARTESIAN_POINT('Ctrl Pts',(-6.04851990186614,-0.9734742969003,-1.74202771422195));
#54883=CARTESIAN_POINT('Ctrl Pts',(-5.93737355698873,0.935751071556099,
-1.76257842263103));
#54884=CARTESIAN_POINT('Ctrl Pts',(-5.82622721211131,1.98835354994073,-0.169596356921512));
#54885=CARTESIAN_POINT('Ctrl Pts',(-5.71508086723387,1.2207399300394,1.57864080368217));
#54886=CARTESIAN_POINT('Ctrl Pts',(-5.60393452235647,-0.664386454402397,
1.88172883355958));
#54887=CARTESIAN_POINT('Ctrl Pts',(-5.49278817747902,-1.94130766334994,
0.462209173493692));
#54888=CARTESIAN_POINT('Ctrl Pts',(-5.38164183260162,-1.44108040659289,
-1.38043472340309));
#54889=CARTESIAN_POINT('Ctrl Pts',(-5.27049548772418,0.37836784840312,-1.95937503687724));
#54890=CARTESIAN_POINT('Ctrl Pts',(-5.15934914284677,1.85144347326116,-0.744627308901291));
#54891=CARTESIAN_POINT('Ctrl Pts',(-5.04820279796934,1.6296358037489,1.15178119058377));
#54892=CARTESIAN_POINT('Ctrl Pts',(-4.93705645309192,-0.0840038009920192,
1.99380443505921));
#54893=CARTESIAN_POINT('Ctrl Pts',(-4.8259101082145,-1.72074306228678,1.01062162921386));
#54894=CARTESIAN_POINT('Ctrl Pts',(-4.71476376333707,-1.78224726386006,
-0.89772348432365));
#54895=CARTESIAN_POINT('Ctrl Pts',(-4.60361741845965,-0.2122130698091,-1.98425763872665));
#54896=CARTESIAN_POINT('Ctrl Pts',(-4.49247107358223,1.55208921401132,-1.25432525111822));
#54897=CARTESIAN_POINT('Ctrl Pts',(-4.3813247287048,1.89554872396803,0.623865208924149));
#54898=CARTESIAN_POINT('Ctrl Pts',(-4.27017838382738,0.503749279321564,
1.93094521606016));
#54899=CARTESIAN_POINT('Ctrl Pts',(-4.15903203894995,-1.34920182909664,
1.4703629443801));
#54900=CARTESIAN_POINT('Ctrl Pts',(-4.04788569407253,-1.96704115911265,
-0.336246698420522));
#54901=CARTESIAN_POINT('Ctrl Pts',(-3.93673934919511,-0.784174581513545,
-1.83504304841865));
#54902=CARTESIAN_POINT('Ctrl Pts',(-3.82559300431769,1.11655587757895,-1.65396969019784));
#54903=CARTESIAN_POINT('Ctrl Pts',(-3.71444665944026,1.99514770188327,0.041211788418896));
#54904=CARTESIAN_POINT('Ctrl Pts',(-3.60330031456284,1.04730379722992,1.69866639460034));
#54905=CARTESIAN_POINT('Ctrl Pts',(-3.49215396968541,-0.859282697039027,
1.80109578047766));
#54906=CARTESIAN_POINT('Ctrl Pts',(-3.38100762480799,-1.97924842246725,
0.254732106220004));
#54907=CARTESIAN_POINT('Ctrl Pts',(-3.26986127993057,-1.28733323713422,
-1.52482323578601));
#54908=CARTESIAN_POINT('Ctrl Pts',(-3.15871493505314,0.583056813672423,
-1.90849613993501));
#54909=CARTESIAN_POINT('Ctrl Pts',(-3.04756859017572,1.91969400203911,-0.545057521628532));
#54910=CARTESIAN_POINT('Ctrl Pts',(-2.9364222452983,1.49896871042294,1.31734793014021));
#54911=CARTESIAN_POINT('Ctrl Pts',(-2.82527590042087,-0.293970782701203,
1.97380190102493));
#54912=CARTESIAN_POINT('Ctrl Pts',(-2.71412955554345,-1.81779799767748,
0.8233609171026));
#54913=CARTESIAN_POINT('Ctrl Pts',(-2.60298321066602,-1.67754229632962,
-1.08081663994663));
#54914=CARTESIAN_POINT('Ctrl Pts',(-2.49183686578861,-0.00159919047849908,
-1.99557265390096));
#54915=CARTESIAN_POINT('Ctrl Pts',(-2.38069052091117,1.67580786785562,-1.08350391199696));
#54916=CARTESIAN_POINT('Ctrl Pts',(-2.26954417603376,1.8191153058292,0.82044639344388));
#54917=CARTESIAN_POINT('Ctrl Pts',(-2.15839783115632,0.297133878843009,
1.97332822505901));
#54918=CARTESIAN_POINT('Ctrl Pts',(-2.04725148627891,-1.49685538682514,
1.31974866055417));
#54919=CARTESIAN_POINT('Ctrl Pts',(-1.93610514140148,-1.92056518303343,
-0.54197998561013));
#54920=CARTESIAN_POINT('Ctrl Pts',(-1.82495879652407,-0.586114771301867,
-1.9075593257576));
#54921=CARTESIAN_POINT('Ctrl Pts',(-1.71381245164663,1.28488746754462,-1.52688429885936));
#54922=CARTESIAN_POINT('Ctrl Pts',(-1.60266610676922,1.9796545703674,0.251559104539083));
#54923=CARTESIAN_POINT('Ctrl Pts',(-1.49151976189179,0.862167481052224,
1.79971712455831));
#54924=CARTESIAN_POINT('Ctrl Pts',(-1.38037341701437,-1.04457840936319,
1.70034112479895));
#54925=CARTESIAN_POINT('Ctrl Pts',(-1.26922707213694,-1.99508198357073,
0.0444125647564481));
#54926=CARTESIAN_POINT('Ctrl Pts',(-1.15808072725952,-1.1191998176419,-1.65218396478253));
#54927=CARTESIAN_POINT('Ctrl Pts',(-1.04693438238209,0.78122199815978,-1.83628620557567));
#54928=CARTESIAN_POINT('Ctrl Pts',(-0.935788037504671,1.96651965162107,
-0.339420443694009));
#54929=CARTESIAN_POINT('Ctrl Pts',(-0.82464169262725,1.35151878363549,1.46823957714146));
#54930=CARTESIAN_POINT('Ctrl Pts',(-0.713495347749821,-0.500581689657017,
1.93167223103872));
#54931=CARTESIAN_POINT('Ctrl Pts',(-0.602349002872402,-1.89468364489563,
0.627050666299228));
#54932=CARTESIAN_POINT('Ctrl Pts',(-0.491202657994974,-1.55383632121744,
-1.25211820325569));
#54933=CARTESIAN_POINT('Ctrl Pts',(-0.380056313117557,0.208534092580134,
-1.98405617855194));
#54934=CARTESIAN_POINT('Ctrl Pts',(-0.268909968240128,1.78176704590796,
-0.90162390006292));
#54935=CARTESIAN_POINT('Ctrl Pts',(-0.157763623362708,1.72042361801685,
1.01001860971832));
#54936=CARTESIAN_POINT('Ctrl Pts',(-0.0836660601110885,0.634691421918637,
1.66218726645698));
#54937=CARTESIAN_POINT('Ctrl Pts',(-0.0466172784852814,0.0737739821678156,
1.68672073681435));
#54938=CARTESIAN_POINT('Ctrl Pts',(-29.646,0.903606778650087,-1.26612599672292));
#54939=CARTESIAN_POINT('Ctrl Pts',(-29.6089512183742,1.32465582191086,-0.965632388172658));
#54940=CARTESIAN_POINT('Ctrl Pts',(-29.5348536551225,1.83614857151059,0.0831884196457774));
#54941=CARTESIAN_POINT('Ctrl Pts',(-29.4237073102452,0.924038956922092,
1.59090722470862));
#54942=CARTESIAN_POINT('Ctrl Pts',(-29.3125609653677,-0.83473688776688,
1.63754421834404));
#54943=CARTESIAN_POINT('Ctrl Pts',(-29.2014146204903,-1.82895987007768,
0.187471477219877));
#54944=CARTESIAN_POINT('Ctrl Pts',(-29.0902682756128,-1.14909344713552,
-1.43544860892843));
#54945=CARTESIAN_POINT('Ctrl Pts',(-28.9791219307355,0.582808968573894,
-1.74365887083216));
#54946=CARTESIAN_POINT('Ctrl Pts',(-28.867975585858,1.78112695043666,-0.455994626000207));
#54947=CARTESIAN_POINT('Ctrl Pts',(-28.7568292409806,1.34896284622222,1.24928278177877));
#54948=CARTESIAN_POINT('Ctrl Pts',(-28.6456828961032,-0.318110417184717,
1.81082463803951));
#54949=CARTESIAN_POINT('Ctrl Pts',(-28.5345365512258,-1.69396455183104,
0.714716438603391));
#54950=CARTESIAN_POINT('Ctrl Pts',(-28.4233902063484,-1.51910218013106,
-1.0356968120803));
#54951=CARTESIAN_POINT('Ctrl Pts',(-28.3122438614709,0.046407699775919,
-1.83797936794685));
#54952=CARTESIAN_POINT('Ctrl Pts',(-28.2010975165935,1.56943293437681,-0.95771133892945));
#54953=CARTESIAN_POINT('Ctrl Pts',(-28.089951171716,1.65573892814966,0.799286617882397));
#54954=CARTESIAN_POINT('Ctrl Pts',(-27.9788048268387,0.226316831424914,
1.82458457360074));
#54955=CARTESIAN_POINT('Ctrl Pts',(-27.8676584819612,-1.41028430723429,
1.1795879531954));
#54956=CARTESIAN_POINT('Ctrl Pts',(-27.7565121370838,-1.75585648782649,
-0.545249858763614));
#54957=CARTESIAN_POINT('Ctrl Pts',(-27.6453657922064,-0.494049365075557,
-1.77094447718388));
#54958=CARTESIAN_POINT('Ctrl Pts',(-27.534219447329,1.22002971701301,-1.37544786085574));
#54959=CARTESIAN_POINT('Ctrl Pts',(-27.4230731024515,1.81724620484857,0.279187250412826));
#54960=CARTESIAN_POINT('Ctrl Pts',(-27.3119267575741,0.750884899378822,
1.67824346299867));
#54961=CARTESIAN_POINT('Ctrl Pts',(-27.2007804126967,-1.00286561528311,
1.54097042230253));
#54962=CARTESIAN_POINT('Ctrl Pts',(-27.0896340678193,-1.83855398075809,
-0.00696682981420152));
#54963=CARTESIAN_POINT('Ctrl Pts',(-26.9784877229418,-0.991158593083783,
-1.54852636916561));
#54964=CARTESIAN_POINT('Ctrl Pts',(-26.8673413780644,0.763581882211757,
-1.67250470444365));
#54965=CARTESIAN_POINT('Ctrl Pts',(-26.756195033187,1.81930983338734,-0.265407245427431));
#54966=CARTESIAN_POINT('Ctrl Pts',(-26.6450486883096,1.20957087255313,1.38465431773148));
#54967=CARTESIAN_POINT('Ctrl Pts',(-26.5339023434321,-0.507456263538371,
1.76714951732695));
#54968=CARTESIAN_POINT('Ctrl Pts',(-26.4227559985548,-1.75993821851123,
0.531927384863541));
#54969=CARTESIAN_POINT('Ctrl Pts',(-26.3116096536772,-1.4013043447814,-1.1902417439339));
#54970=CARTESIAN_POINT('Ctrl Pts',(-26.2004633087999,0.240137974670818,
-1.8228173328443));
#54971=CARTESIAN_POINT('Ctrl Pts',(-26.0893169639224,1.66174866141038,-0.786715108572567));
#54972=CARTESIAN_POINT('Ctrl Pts',(-25.978170619045,1.56213005525038,0.969576694355506));
#54973=CARTESIAN_POINT('Ctrl Pts',(-25.8670242741676,0.032476899015307,
1.8382803177961));
#54974=CARTESIAN_POINT('Ctrl Pts',(-25.7558779292902,-1.52690687248867,
1.02415071083631));
#54975=CARTESIAN_POINT('Ctrl Pts',(-25.6447315844127,-1.68850076403338,
-0.727526250810708));
#54976=CARTESIAN_POINT('Ctrl Pts',(-25.5335852395354,-0.304375448471892,
-1.81319741399803));
#54977=CARTESIAN_POINT('Ctrl Pts',(-25.4224388946579,1.35838697931157,-1.23899721153737));
#54978=CARTESIAN_POINT('Ctrl Pts',(-25.3112925497805,1.77762918529204,0.469429180344255));
#54979=CARTESIAN_POINT('Ctrl Pts',(-25.200146204903,0.569560564207642,1.74812186058649));
#54980=CARTESIAN_POINT('Ctrl Pts',(-25.0889998600256,-1.1599059279699,1.42651586532399));
#54981=CARTESIAN_POINT('Ctrl Pts',(-24.9778535151482,-1.82754946484302,
-0.200978181185898));
#54982=CARTESIAN_POINT('Ctrl Pts',(-24.8667071702708,-0.822183211067854,
-1.64448899151042));
#54983=CARTESIAN_POINT('Ctrl Pts',(-24.7555608253933,0.935841500540801,
-1.58257068139984));
#54984=CARTESIAN_POINT('Ctrl Pts',(-24.644414480516,1.8371605398714,-0.071905677802479));
#54985=CARTESIAN_POINT('Ctrl Pts',(-24.5332681356385,1.05667143702865,1.50458457719352));
#54986=CARTESIAN_POINT('Ctrl Pts',(-24.4221217907611,-0.691135756872815,
1.70371964869008));
#54987=CARTESIAN_POINT('Ctrl Pts',(-24.3109754458837,-1.80625042443839,
0.343203554726555));
#54988=CARTESIAN_POINT('Ctrl Pts',(-24.1998291010062,-1.26785327052907,
-1.3314944086137));
#54989=CARTESIAN_POINT('Ctrl Pts',(-24.0886827561288,0.431186030422094,
-1.78729065429483));
#54990=CARTESIAN_POINT('Ctrl Pts',(-23.9775364112514,1.73550088513296,-0.606931588783731));
#54991=CARTESIAN_POINT('Ctrl Pts',(-23.866390066374,1.45107079566491,1.12903623579104));
#54992=CARTESIAN_POINT('Ctrl Pts',(-23.7552437214966,-0.161725882381191,
1.83144042074233));
#54993=CARTESIAN_POINT('Ctrl Pts',(-23.6440973766191,-1.62647240373936,
0.857272882829682));
#54994=CARTESIAN_POINT('Ctrl Pts',(-23.5329510317417,-1.60228288915339,
-0.901675561877481));
#54995=CARTESIAN_POINT('Ctrl Pts',(-23.4218046868643,-0.111301360173381,
-1.83519516209704));
#54996=CARTESIAN_POINT('Ctrl Pts',(-23.3106583419868,1.48156975859047,-1.08870580332383));
#54997=CARTESIAN_POINT('Ctrl Pts',(-23.1995119971095,1.7181543530587,0.654427150129224));
#54998=CARTESIAN_POINT('Ctrl Pts',(-23.088365652232,0.381873692818719,1.79847206219441));
#54999=CARTESIAN_POINT('Ctrl Pts',(-22.9772193073546,-1.30398898375897,
1.29612576781578));
#55000=CARTESIAN_POINT('Ctrl Pts',(-22.8660729624772,-1.79612947732935,
-0.392744416165795));
#55001=CARTESIAN_POINT('Ctrl Pts',(-22.7549266175997,-0.644023257663918,
-1.72208110126926));
#55002=CARTESIAN_POINT('Ctrl Pts',(-22.6437802727223,1.09764687597715,-1.47495783377641));
#55003=CARTESIAN_POINT('Ctrl Pts',(-22.5326339278449,1.83448840962079,0.122399145126971));
#55004=CARTESIAN_POINT('Ctrl Pts',(-22.4214875829675,0.891967972949703,
1.6077071906889));
#55005=CARTESIAN_POINT('Ctrl Pts',(-22.3103412380901,-0.867094604110294,
1.6212576054667));
#55006=CARTESIAN_POINT('Ctrl Pts',(-22.1991948932126,-1.83238508908664,
0.150645813263272));
#55007=CARTESIAN_POINT('Ctrl Pts',(-22.0880485483352,-1.12023906509101,
-1.45787300983482));
#55008=CARTESIAN_POINT('Ctrl Pts',(-21.9769022034578,0.617417326649948,
-1.73179823319959));
#55009=CARTESIAN_POINT('Ctrl Pts',(-21.8657558585803,1.78986590745487,-0.420368063834038));
#55010=CARTESIAN_POINT('Ctrl Pts',(-21.7546095137029,1.32380169026185,1.27588336481854));
#55011=CARTESIAN_POINT('Ctrl Pts',(-21.6434631688255,-0.35412203130582,
1.80414158610255));
#55012=CARTESIAN_POINT('Ctrl Pts',(-21.532316823948,-1.70786868579214,0.680818498464482));
#55013=CARTESIAN_POINT('Ctrl Pts',(-21.4211704790707,-1.49816598504183,
-1.06575229627923));
#55014=CARTESIAN_POINT('Ctrl Pts',(-21.3100241341932,0.0830160705540191,
-1.83669202856401));
#55015=CARTESIAN_POINT('Ctrl Pts',(-21.1988777893158,1.58820198952549,-0.926252512130515));
#55016=CARTESIAN_POINT('Ctrl Pts',(-21.0877314444384,1.6394860967441,0.832114544004366));
#55017=CARTESIAN_POINT('Ctrl Pts',(-20.976585099561,0.189920927787188,1.82873161424777));
#55018=CARTESIAN_POINT('Ctrl Pts',(-20.8654387546835,-1.43350523795772,
1.15125670834466));
#55019=CARTESIAN_POINT('Ctrl Pts',(-20.7542924098061,-1.74464500917001,
-0.580123321147311));
#55020=CARTESIAN_POINT('Ctrl Pts',(-20.6431460649287,-0.458668949759455,
-1.78043592142131));
#55021=CARTESIAN_POINT('Ctrl Pts',(-20.5319997200512,1.24719048811815,-1.35086829932027));
#55022=CARTESIAN_POINT('Ctrl Pts',(-20.4208533751738,1.81132329283767,0.315336652776849));
#55023=CARTESIAN_POINT('Ctrl Pts',(-20.3097070302964,0.717300375240254,
1.69287018032718));
#55024=CARTESIAN_POINT('Ctrl Pts',(-20.198560685419,-1.03336717698855,1.52068456731945));
#55025=CARTESIAN_POINT('Ctrl Pts',(-20.0874143405416,-1.83805026330036,
-0.0435947857237916));
#55026=CARTESIAN_POINT('Ctrl Pts',(-19.9762679956642,-0.960110720041205,
-1.56796577801391));
#55027=CARTESIAN_POINT('Ctrl Pts',(-19.8651216507867,0.796751482021758,
-1.65695997285902));
#55028=CARTESIAN_POINT('Ctrl Pts',(-19.7539753059093,1.82423641918512,-0.229108626375055));
#55029=CARTESIAN_POINT('Ctrl Pts',(-19.6428289610319,1.18174445642581,1.40847765884577));
#55030=CARTESIAN_POINT('Ctrl Pts',(-19.5316826161545,-0.542562299135568,
1.75668876791466));
#55031=CARTESIAN_POINT('Ctrl Pts',(-19.420536271277,-1.77018644448459,0.49675872163839));
#55032=CARTESIAN_POINT('Ctrl Pts',(-19.3093899263996,-1.37731313689601,
-1.21792356028385));
#55033=CARTESIAN_POINT('Ctrl Pts',(-19.1982435815222,0.276406132535501,
-1.81767129197156));
#55034=CARTESIAN_POINT('Ctrl Pts',(-19.0870972366448,1.67709248831789,-0.75345209627986));
#55035=CARTESIAN_POINT('Ctrl Pts',(-18.9759508917673,1.5425032158592,1.0005064241797));
#55036=CARTESIAN_POINT('Ctrl Pts',(-18.8648045468899,-0.00415343528496038,
1.83856248866775));
#55037=CARTESIAN_POINT('Ctrl Pts',(-18.7536582020125,-1.54700787038504,
0.993527012580707));
#55038=CARTESIAN_POINT('Ctrl Pts',(-18.6425118571351,-1.67367119101565,
-0.761021694910901));
#55039=CARTESIAN_POINT('Ctrl Pts',(-18.5313655122577,-0.268190871892204,
-1.8189015729265));
#55040=CARTESIAN_POINT('Ctrl Pts',(-18.4202191673802,1.38280179207861,-1.21168827657323));
#55041=CARTESIAN_POINT('Ctrl Pts',(-18.3090728225028,1.76792396598735,0.504751549030178));
#55042=CARTESIAN_POINT('Ctrl Pts',(-18.1979264776254,0.534619847684823,
1.75912219422707));
#55043=CARTESIAN_POINT('Ctrl Pts',(-18.0867801327479,-1.18809605216334,
1.40312403108018));
#55044=CARTESIAN_POINT('Ctrl Pts',(-17.9756337878705,-1.82318266167623,
-0.237348389343613));
#55045=CARTESIAN_POINT('Ctrl Pts',(-17.8644874429931,-0.789257021834459,
-1.66054287184818));
#55046=CARTESIAN_POINT('Ctrl Pts',(-17.7533410981157,0.967185162849705,
-1.56361188807332));
#55047=CARTESIAN_POINT('Ctrl Pts',(-17.6421947532383,1.83822846890144,-0.0352898268780593));
#55048=CARTESIAN_POINT('Ctrl Pts',(-17.5310484083608,1.0264860090507,1.52533791304877));
#55049=CARTESIAN_POINT('Ctrl Pts',(-17.4199020634834,-0.724941628214821,
1.68961205945094));
#55050=CARTESIAN_POINT('Ctrl Pts',(-17.308755718606,-1.81272953097057,0.307149675741386));
#55051=CARTESIAN_POINT('Ctrl Pts',(-17.1976093737286,-1.24107438638229,
-1.35648945562677));
#55052=CARTESIAN_POINT('Ctrl Pts',(-17.0864630288511,0.466708474190256,
-1.7783454321025));
#55053=CARTESIAN_POINT('Ctrl Pts',(-16.9753166839737,1.74724826325126,-0.572234901352823));
#55054=CARTESIAN_POINT('Ctrl Pts',(-16.8641703390963,1.42828910175244,1.15772169262565));
#55055=CARTESIAN_POINT('Ctrl Pts',(-16.7530239942189,-0.19818140052057,
1.82785486520361));
#55056=CARTESIAN_POINT('Ctrl Pts',(-16.6418776493414,-1.64322894829983,
0.824698671776694));
#55057=CARTESIAN_POINT('Ctrl Pts',(-16.530731304464,-1.58400086815871,-0.933418729956337));
#55058=CARTESIAN_POINT('Ctrl Pts',(-16.4195849595866,-0.0747168460009575,
-1.83704835774251));
#55059=CARTESIAN_POINT('Ctrl Pts',(-16.3084386147092,1.50296588015394,-1.05897253923504));
#55060=CARTESIAN_POINT('Ctrl Pts',(-16.1972922698318,1.70477524097488,0.688527888701595));
#55061=CARTESIAN_POINT('Ctrl Pts',(-16.0861459249543,0.345967106142554,
1.80572313415655));
#55062=CARTESIAN_POINT('Ctrl Pts',(-15.9749995800769,-1.32955276041214,
1.26988926014879));
#55063=CARTESIAN_POINT('Ctrl Pts',(-15.8638532351995,-1.78794836951534,
-0.428450584908307));
#55064=CARTESIAN_POINT('Ctrl Pts',(-15.7527068903221,-0.609586569357517,
-1.73457011683579));
#55065=CARTESIAN_POINT('Ctrl Pts',(-15.6415605454446,1.12681446224207,-1.45279676604917));
#55066=CARTESIAN_POINT('Ctrl Pts',(-15.5304142005672,1.83168575205326,0.158923193668888));
#55067=CARTESIAN_POINT('Ctrl Pts',(-15.4192678556898,0.859760733185979,
1.6251586868464));
#55068=CARTESIAN_POINT('Ctrl Pts',(-15.3081215108124,-0.899222667358879,
1.60366077156884));
#55069=CARTESIAN_POINT('Ctrl Pts',(-15.1969751659349,-1.83502269836715,
0.114109474795715));
#55070=CARTESIAN_POINT('Ctrl Pts',(-15.0858288210575,-1.09097165038219,
-1.47990206899753));
#55071=CARTESIAN_POINT('Ctrl Pts',(-14.9746824761801,0.651797236720689,
-1.71915375634761));
#55072=CARTESIAN_POINT('Ctrl Pts',(-14.8635361313027,1.79788560735673,-0.384625296386388));
#55073=CARTESIAN_POINT('Ctrl Pts',(-14.7523897864252,1.29811963509442,1.30200410473359));
#55074=CARTESIAN_POINT('Ctrl Pts',(-14.6412434415478,-0.389995490350614,
1.79672835822976));
#55075=CARTESIAN_POINT('Ctrl Pts',(-14.5300970966704,-1.72109359041992,
0.646657659644004));
#55076=CARTESIAN_POINT('Ctrl Pts',(-14.418950751793,-1.47663574369473,-1.09538858685122));
#55077=CARTESIAN_POINT('Ctrl Pts',(-14.3078044069155,0.119591838376424,
-1.83467355896208));
#55078=CARTESIAN_POINT('Ctrl Pts',(-14.1966580620381,1.60634040478516,-0.894427067857099));
#55079=CARTESIAN_POINT('Ctrl Pts',(-14.0855117171607,1.62258254933333,0.864612714664634));
#55080=CARTESIAN_POINT('Ctrl Pts',(-13.9743653722833,0.153449581803269,
1.83215242313658));
#55081=CARTESIAN_POINT('Ctrl Pts',(-13.8632190274059,-1.45615709528508,
1.1224686140876));
#55082=CARTESIAN_POINT('Ctrl Pts',(-13.7520726825284,-1.73274098749183,
-0.614766578488641));
#55083=CARTESIAN_POINT('Ctrl Pts',(-13.640926337651,-0.423106453057855,
-1.78922055799212));
#55084=CARTESIAN_POINT('Ctrl Pts',(-13.5297799927736,1.27385616856038,-1.32575251747129));
#55085=CARTESIAN_POINT('Ctrl Pts',(-13.4186336478962,1.8046813570327,0.351360890452264));
#55086=CARTESIAN_POINT('Ctrl Pts',(-13.3074873030187,0.683431109300355,
1.70682488691761));
#55087=CARTESIAN_POINT('Ctrl Pts',(-13.1963409581413,-1.06345853101135,
1.49979506219349));
#55088=CARTESIAN_POINT('Ctrl Pts',(-13.0851946132639,-1.83681691071596,
-0.0802054378995563));
#55089=CARTESIAN_POINT('Ctrl Pts',(-12.9740482683865,-0.928681719728038,
-1.58678276370895));
#55090=CARTESIAN_POINT('Ctrl Pts',(-12.8629019235091,0.829604801984373,
-1.64075749222281));
#55091=CARTESIAN_POINT('Ctrl Pts',(-12.7517555786316,1.82843885316793,-0.192719059739105));
#55092=CARTESIAN_POINT('Ctrl Pts',(-12.6406092337542,1.15344893307288,1.43174188824448));
#55093=CARTESIAN_POINT('Ctrl Pts',(-12.5294628888768,-0.577452958307463,
1.74553068053895));
#55094=CARTESIAN_POINT('Ctrl Pts',(-12.4183165439994,-1.77973197437198,
0.461392864226164));
#55095=CARTESIAN_POINT('Ctrl Pts',(-12.3071701991219,-1.35277518854269,
-1.24512190769584));
#55096=CARTESIAN_POINT('Ctrl Pts',(-12.1960238542445,0.312564567770197,
-1.81180370535426));
#55097=CARTESIAN_POINT('Ctrl Pts',(-12.0848775093671,1.69177057386242,-0.719889992411354));
#55098=CARTESIAN_POINT('Ctrl Pts',(-11.9737311644897,1.52226406188029,1.0310389913425));
#55099=CARTESIAN_POINT('Ctrl Pts',(-11.8625848196122,-0.0407821208305537,
1.83811482078279));
#55100=CARTESIAN_POINT('Ctrl Pts',(-11.7514384747348,-1.56649476551932,
0.962508922224293));
#55101=CARTESIAN_POINT('Ctrl Pts',(-11.6402921298574,-1.6581772347577,-0.794215042600007));
#55102=CARTESIAN_POINT('Ctrl Pts',(-11.52914578498,-0.231899833827511,-1.82388369772625));
#55103=CARTESIAN_POINT('Ctrl Pts',(-11.4179994401025,1.40666768559556,-1.18389834785848));
#55104=CARTESIAN_POINT('Ctrl Pts',(-11.3068530952251,1.75751694870754,0.539873550719585));
#55105=CARTESIAN_POINT('Ctrl Pts',(-11.1957067503477,0.499466907597081,
1.7694242238582));
#55106=CARTESIAN_POINT('Ctrl Pts',(-11.0845604054703,-1.21581454781411,
1.37917521043716));
#55107=CARTESIAN_POINT('Ctrl Pts',(-10.9734140605928,-1.81809212495253,
-0.273624379298372));
#55108=CARTESIAN_POINT('Ctrl Pts',(-10.8622677157155,-0.756017527849028,
-1.67593758038474));
#55109=CARTESIAN_POINT('Ctrl Pts',(-10.751121370838,0.998144889762121,-1.54403240082667));
#55110=CARTESIAN_POINT('Ctrl Pts',(-10.6399750259606,1.83856669176645,0.00134003275348477));
#55111=CARTESIAN_POINT('Ctrl Pts',(-10.5288286810832,0.99589310551582,1.54548574828332));
#55112=CARTESIAN_POINT('Ctrl Pts',(-10.4176823362057,-0.758459725548137,
1.67483375905857));
#55113=CARTESIAN_POINT('Ctrl Pts',(-10.3065359913283,-1.81848905343763,
0.270973870120994));
#55114=CARTESIAN_POINT('Ctrl Pts',(-10.1953896464509,-1.21380284332704,
-1.38094602837764));
#55115=CARTESIAN_POINT('Ctrl Pts',(-10.0842433015735,0.502045652602867,
-1.76869427501289));
#55116=CARTESIAN_POINT('Ctrl Pts',(-9.97309695669603,1.75830205085506,-0.537311058624067));
#55117=CARTESIAN_POINT('Ctrl Pts',(-9.86195061181863,1.40494043187336,1.1859475783728));
#55118=CARTESIAN_POINT('Ctrl Pts',(-9.75080426694118,-0.234558248248651,
1.82354372142247));
#55119=CARTESIAN_POINT('Ctrl Pts',(-9.63965792206378,-1.65933319402237,
0.791797086996613));
#55120=CARTESIAN_POINT('Ctrl Pts',(-9.52851157718634,-1.56509005960118,
-0.964791366616839));
#55121=CARTESIAN_POINT('Ctrl Pts',(-9.41736523230892,-0.0381026721077461,
-1.83817231568183));
#55122=CARTESIAN_POINT('Ctrl Pts',(-9.30621888743151,1.5237653819353,-1.02881890368343));
#55123=CARTESIAN_POINT('Ctrl Pts',(-9.19507254255407,1.6907193985366,0.722355308122558));
#55124=CARTESIAN_POINT('Ctrl Pts',(-9.08392619767666,0.309923183800838,
1.81225740332426));
#55125=CARTESIAN_POINT('Ctrl Pts',(-8.97277985279922,-1.35458875563747,
1.24314865517416));
#55126=CARTESIAN_POINT('Ctrl Pts',(-8.86163350792181,-1.77905751480639,
-0.463986675209236));
#55127=CARTESIAN_POINT('Ctrl Pts',(-8.75048716304438,-0.574907898574367,
-1.74637057462545));
#55128=CARTESIAN_POINT('Ctrl Pts',(-8.63934081816696,1.15553474640397,-1.43005899375302));
#55129=CARTESIAN_POINT('Ctrl Pts',(-8.52819447328953,1.82815598552823,0.195384155801151));
#55130=CARTESIAN_POINT('Ctrl Pts',(-8.41704812841212,0.827212201402232,
1.64196505736636));
#55131=CARTESIAN_POINT('Ctrl Pts',(-8.30590178353469,-0.930993773713778,
1.58542734588091));
#55132=CARTESIAN_POINT('Ctrl Pts',(-8.19475543865727,-1.83693187405052,
0.0775278392453074));
#55133=CARTESIAN_POINT('Ctrl Pts',(-8.08360909377984,-1.0612711617913,-1.50134366382617));
#55134=CARTESIAN_POINT('Ctrl Pts',(-7.97246274890243,0.685918408299438,
-1.70582684142229));
#55135=CARTESIAN_POINT('Ctrl Pts',(-7.86131640402499,1.80519161566156,-0.348729847455048));
#55136=CARTESIAN_POINT('Ctrl Pts',(-7.75017005914758,1.27192227624375,1.32760799898003));
#55137=CARTESIAN_POINT('Ctrl Pts',(-7.63902371427015,-0.425714136150784,
1.7886018981434));
#55138=CARTESIAN_POINT('Ctrl Pts',(-7.52787736939272,-1.7336352869347,0.612240122546414));
#55139=CARTESIAN_POINT('Ctrl Pts',(-7.4167310245153,-1.45451933461935,-1.12459005018688));
#55140=CARTESIAN_POINT('Ctrl Pts',(-7.30558467963788,0.156120132828023,
-1.83192679435794));
#55141=CARTESIAN_POINT('Ctrl Pts',(-7.19443833476045,1.62384116454318,-0.862246570359003));
#55142=CARTESIAN_POINT('Ctrl Pts',(-7.08329198988304,1.60503489891277,0.896767667254413));
#55143=CARTESIAN_POINT('Ctrl Pts',(-6.97214564500561,0.116917322223582,
1.83484593781736));
#55144=CARTESIAN_POINT('Ctrl Pts',(-6.86099930012818,-1.47823091412176,
1.09323494286248));
#55145=CARTESIAN_POINT('Ctrl Pts',(-6.74985295525077,-1.72014913413095,
-0.649165797088362));
#55146=CARTESIAN_POINT('Ctrl Pts',(-6.63870661037334,-0.387375999329962,
-1.79729494265797));
#55147=CARTESIAN_POINT('Ctrl Pts',(-6.5275602654959,1.30001617698454,-1.30011046274511));
#55148=CARTESIAN_POINT('Ctrl Pts',(-6.4164139206185,1.79732303197884,0.387245651336726));
#55149=CARTESIAN_POINT('Ctrl Pts',(-6.30526757574106,0.649290547434899,
1.72010204952278));
#55150=CARTESIAN_POINT('Ctrl Pts',(-6.19412123086365,-1.09312773280473,
1.4783101959785));
#55151=CARTESIAN_POINT('Ctrl Pts',(-6.08297488598622,-1.83485441230099,
-0.11678425159416));
#55152=CARTESIAN_POINT('Ctrl Pts',(-5.9718285411088,-0.896884068407809,
-1.60496985753535));
#55153=CARTESIAN_POINT('Ctrl Pts',(-5.86068219623137,0.862128800674478,
-1.62390369382189));
#55154=CARTESIAN_POINT('Ctrl Pts',(-5.74953585135396,1.83191546708753,-0.156252991031506));
#55155=CARTESIAN_POINT('Ctrl Pts',(-5.63838950647652,1.12469553475403,1.45443777105284));
#55156=CARTESIAN_POINT('Ctrl Pts',(-5.5272431615991,-0.612114390813121,
1.73367968446316));
#55157=CARTESIAN_POINT('Ctrl Pts',(-5.41609681672168,-1.78857101895803,
0.42584385155156));
#55158=CARTESIAN_POINT('Ctrl Pts',(-5.30495047184425,-1.32770024034866,
-1.2718259894887));
#55159=CARTESIAN_POINT('Ctrl Pts',(-5.19380412696683,0.348598926865315,
-1.80521690218908));
#55160=CARTESIAN_POINT('Ctrl Pts',(-5.08265778208941,1.70577709140633,-0.686042119839725));
#55161=CARTESIAN_POINT('Ctrl Pts',(-4.97151143721198,1.50142062748163,1.06116227558912));
#55162=CARTESIAN_POINT('Ctrl Pts',(-4.86036509233456,-0.0773946174390751,
1.83693749184676));
#55163=CARTESIAN_POINT('Ctrl Pts',(-4.74921874745714,-1.58535982234177,
0.931108752759484));
#55164=CARTESIAN_POINT('Ctrl Pts',(-4.63807240257972,-1.64202504576567,
-0.827093117393093));
#55165=CARTESIAN_POINT('Ctrl Pts',(-4.52692605770229,-0.195516740427347,
-1.82814181068467));
#55166=CARTESIAN_POINT('Ctrl Pts',(-4.41577971282487,1.42997518601849,-1.15563845692861));
#55167=CARTESIAN_POINT('Ctrl Pts',(-4.30463336794744,1.74641226463907,0.57478124332561));
#55168=CARTESIAN_POINT('Ctrl Pts',(-4.19348702307002,0.464115698312818,
1.77902385996933));
#55169=CARTESIAN_POINT('Ctrl Pts',(-4.0823406781926,-1.24305041174318,1.35467891015794));
#55170=CARTESIAN_POINT('Ctrl Pts',(-3.97119433331518,-1.81227987541939,
-0.309791750874438));
#55171=CARTESIAN_POINT('Ctrl Pts',(-3.86004798843775,-0.72247792391575,
-1.69066700601096));
#55172=CARTESIAN_POINT('Ctrl Pts',(-3.74890164356033,1.02870839145545,-1.52383999196612));
#55173=CARTESIAN_POINT('Ctrl Pts',(-3.63775529868291,1.83817507420302,0.0379693604454949));
#55174=CARTESIAN_POINT('Ctrl Pts',(-3.52660895380548,0.964904870636465,
1.56502008497577));
#55175=CARTESIAN_POINT('Ctrl Pts',(-3.41546260892806,-0.791676743481206,
1.65939061393862));
#55176=CARTESIAN_POINT('Ctrl Pts',(-3.30431626405063,-1.82352670551695,
0.234690498257847));
#55177=CARTESIAN_POINT('Ctrl Pts',(-3.19316991917321,-1.18604946714455,
-1.4048544185183));
#55178=CARTESIAN_POINT('Ctrl Pts',(-3.08202357429579,0.537183538203758,
-1.75834101421655));
#55179=CARTESIAN_POINT('Ctrl Pts',(-2.97087722941836,1.76865785992407,-0.502173923924951));
#55180=CARTESIAN_POINT('Ctrl Pts',(-2.85973088454094,1.38103405472633,1.21370268825252));
#55181=CARTESIAN_POINT('Ctrl Pts',(-2.74858453966351,-0.27084198568111,
1.81850870111212));
#55182=CARTESIAN_POINT('Ctrl Pts',(-2.6374381947861,-1.67477874751467,0.758581188481656));
#55183=CARTESIAN_POINT('Ctrl Pts',(-2.52629184990866,-1.54555797153453,
-0.995781016843169));
#55184=CARTESIAN_POINT('Ctrl Pts',(-2.41514550503125,-0.00147337065513613,
-1.83856659218734));
#55185=CARTESIAN_POINT('Ctrl Pts',(-2.30399916015382,1.54396000303022,-0.998256861862604));
#55186=CARTESIAN_POINT('Ctrl Pts',(-2.1928528152764,1.67599241355422,0.755895971373255));
#55187=CARTESIAN_POINT('Ctrl Pts',(-2.08170647039897,0.273756218286524,
1.81807229264321));
#55188=CARTESIAN_POINT('Ctrl Pts',(-1.97056012552155,-1.3790870015043,1.21591453592819));
#55189=CARTESIAN_POINT('Ctrl Pts',(-1.85941378064413,-1.7694604988402,-0.499338519812307));
#55190=CARTESIAN_POINT('Ctrl Pts',(-1.74826743576671,-0.540000904300196,
-1.75747790595217));
#55191=CARTESIAN_POINT('Ctrl Pts',(-1.63712109088928,1.1837961238493,-1.40675332292743));
#55192=CARTESIAN_POINT('Ctrl Pts',(-1.52597474601186,1.82390089883899,0.231767139453362));
#55193=CARTESIAN_POINT('Ctrl Pts',(-1.41482840113443,0.794334560776014,
1.65812042680182));
#55194=CARTESIAN_POINT('Ctrl Pts',(-1.30368205625701,-0.962393908646208,
1.56656305209763));
#55195=CARTESIAN_POINT('Ctrl Pts',(-1.19253571137958,-1.83811452642306,
0.040918308674494));
#55196=CARTESIAN_POINT('Ctrl Pts',(-1.08138936650216,-1.03114431372679,
-1.52219476242003));
#55197=CARTESIAN_POINT('Ctrl Pts',(-0.970243021624738,0.719757641542406,
-1.69181235504817));
#55198=CARTESIAN_POINT('Ctrl Pts',(-0.859096676747318,1.81179939867516,
-0.312715794767707));
#55199=CARTESIAN_POINT('Ctrl Pts',(-0.747950331869893,1.24518507479472,
1.35272260350057));
#55200=CARTESIAN_POINT('Ctrl Pts',(-0.636803986992467,-0.461197325722433,
1.77969367544763));
#55201=CARTESIAN_POINT('Ctrl Pts',(-0.525657642115045,-1.74561524756276,
0.57771607784515));
#55202=CARTESIAN_POINT('Ctrl Pts',(-0.41451129723762,-1.43158483572782,
-1.15360505340423));
#55203=CARTESIAN_POINT('Ctrl Pts',(-0.303364952360201,0.192127214812409,
-1.82795620083171));
#55204=CARTESIAN_POINT('Ctrl Pts',(-0.192218607482774,1.64158261001566,
-0.830686659357144));
#55205=CARTESIAN_POINT('Ctrl Pts',(-0.0810722626053533,1.5850655110515,
0.930553177147139));
#55206=CARTESIAN_POINT('Ctrl Pts',(-0.00697469935373359,0.584755680233683,
1.53141103236355));
#55207=CARTESIAN_POINT('Ctrl Pts',(0.0300740822720735,0.067969652080238,
1.55401427805413));
#55208=CARTESIAN_POINT('Ctrl Pts',(-0.199999999999991,0.0853826423429707,
1.9521336543348));
#55209=CARTESIAN_POINT('Ctrl Pts',(-0.237048781625799,0.734562905288549,
1.92373973464384));
#55210=CARTESIAN_POINT('Ctrl Pts',(-0.274097563251607,1.36285136861803,
1.54634460475229));
#55211=CARTESIAN_POINT('Ctrl Pts',(-0.311146344877415,1.68882828124029,
0.988905730417313));
#55212=CARTESIAN_POINT('Ctrl Pts',(-0.348195126503225,2.01480519386257,
0.431466856082309));
#55213=CARTESIAN_POINT('Ctrl Pts',(-0.385243908129031,2.03847055577757,
-0.306015762696088));
#55214=CARTESIAN_POINT('Ctrl Pts',(-0.422292689754841,1.74683855847221,
-0.883550030838296));
#55215=CARTESIAN_POINT('Ctrl Pts',(-0.459341471380647,1.45520656116689,
-1.46108429898044));
#55216=CARTESIAN_POINT('Ctrl Pts',(-0.496390253006459,0.848277204641205,
-1.87867021648642));
#55217=CARTESIAN_POINT('Ctrl Pts',(-0.533439034632265,0.204864669659703,
-1.94627790340044));
#55218=CARTESIAN_POINT('Ctrl Pts',(-0.570487816258072,-0.438547865321837,
-2.01388559031446));
#55219=CARTESIAN_POINT('Ctrl Pts',(-0.607536597883876,-1.11844357875923,
-1.73151504663655));
#55220=CARTESIAN_POINT('Ctrl Pts',(-0.644585379509684,-1.52413829337206,
-1.22785238376993));
#55221=CARTESIAN_POINT('Ctrl Pts',(-0.669767022298391,-1.79988445657465,
-0.885518501095601));
#55222=CARTESIAN_POINT('Ctrl Pts',(-0.694948665087098,-1.94895609331017,
-0.440952771968191));
#55223=CARTESIAN_POINT('Ctrl Pts',(-0.720130307875805,-1.95236950710743,
0.00155959742907545));
#55224=CARTESIAN_POINT('Origin',(-0.2,0.,0.));
#55225=CARTESIAN_POINT('',(-0.2,-2.39295984553393E-16,1.954));
#55226=CARTESIAN_POINT('Origin',(-0.2,0.,0.));
#55227=CARTESIAN_POINT('',(0.,-2.6378892053634E-16,2.154));
#55228=CARTESIAN_POINT('Origin',(-0.2,-2.6378892053634E-16,2.154));
#55229=CARTESIAN_POINT('Origin',(0.,0.,0.));
#55230=CARTESIAN_POINT('Origin',(-0.2,0.,0.));
#55231=CARTESIAN_POINT('Origin',(-14.8,0.,0.));
#55232=CARTESIAN_POINT('Origin',(0.,3.5,0.));
#55233=CARTESIAN_POINT('',(-2.77555756156289E-16,-3.5,-4.28626379701574E-16));
#55234=CARTESIAN_POINT('Origin',(0.,0.,0.));
#55235=CARTESIAN_POINT('Origin',(0.3,3.51777354540171,-0.493350061591077));
#55236=CARTESIAN_POINT('',(3.5,3.46093394308575,-0.521475063255119));
#55237=CARTESIAN_POINT('',(0.3,3.46093394308575,-0.521475063255119));
#55238=CARTESIAN_POINT('',(1.8,3.46093394308575,-0.521475063255119));
#55239=CARTESIAN_POINT('',(3.5,3.32865020518126,-0.586930840514225));
#55240=CARTESIAN_POINT('',(3.5,3.51777354540171,-0.493350061591077));
#55241=CARTESIAN_POINT('',(0.3,3.32865020518126,-0.586930840514225));
#55242=CARTESIAN_POINT('',(0.3,3.32865020518126,-0.586930840514225));
#55243=CARTESIAN_POINT('',(0.3,3.51777354540171,-0.493350061591077));
#55244=CARTESIAN_POINT('Origin',(0.3,3.4123588641873,-0.601690935615914));
#55245=CARTESIAN_POINT('',(0.3,3.43056906322043,-0.69368285439016));
#55246=CARTESIAN_POINT('Origin',(0.3,0.,0.));
#55247=CARTESIAN_POINT('',(0.3,3.32865020518126,-0.586930840514225));
#55248=CARTESIAN_POINT('Origin',(0.3,3.32865020518126,-0.586930840514225));
#55249=CARTESIAN_POINT('',(3.5,3.43056906322043,-0.69368285439016));
#55250=CARTESIAN_POINT('',(1.8,3.43056906322043,-0.69368285439016));
#55251=CARTESIAN_POINT('',(3.5,3.32865020518126,-0.586930840514225));
#55252=CARTESIAN_POINT('Origin',(3.5,3.4123588641873,-0.601690935615914));
#55253=CARTESIAN_POINT('Origin',(3.5,0.,0.));
#55254=CARTESIAN_POINT('Origin',(0.3,3.37866132170568,-1.09670993120789));
#55255=CARTESIAN_POINT('',(3.5,3.31780138538096,-1.11453755753864));
#55256=CARTESIAN_POINT('',(0.3,3.31780138538096,-1.11453755753864));
#55257=CARTESIAN_POINT('',(1.8,3.31780138538096,-1.11453755753864));
#55258=CARTESIAN_POINT('',(3.5,3.17616105825637,-1.15602808444076));
#55259=CARTESIAN_POINT('',(3.5,3.37866132170568,-1.09670993120789));
#55260=CARTESIAN_POINT('',(0.3,3.17616105825637,-1.15602808444076));
#55261=CARTESIAN_POINT('',(0.3,3.17616105825637,-1.15602808444076));
#55262=CARTESIAN_POINT('',(0.3,3.37866132170568,-1.09670993120789));
#55263=CARTESIAN_POINT('Origin',(0.3,3.25603493102317,-1.18509979662344));
#55264=CARTESIAN_POINT('',(0.3,3.25799424715966,-1.27885631932385));
#55265=CARTESIAN_POINT('Origin',(0.3,0.,0.));
#55266=CARTESIAN_POINT('',(0.3,3.17616105825637,-1.15602808444076));
#55267=CARTESIAN_POINT('Origin',(0.3,3.17616105825637,-1.15602808444076));
#55268=CARTESIAN_POINT('',(3.5,3.25799424715966,-1.27885631932385));
#55269=CARTESIAN_POINT('',(1.8,3.25799424715966,-1.27885631932385));
#55270=CARTESIAN_POINT('',(3.5,3.17616105825637,-1.15602808444076));
#55271=CARTESIAN_POINT('Origin',(3.5,3.25603493102317,-1.18509979662344));
#55272=CARTESIAN_POINT('Origin',(3.5,0.,0.));
#55273=CARTESIAN_POINT('Origin',(0.3,3.13689018343476,-1.66674682452695));
#55274=CARTESIAN_POINT('',(3.5,3.07385911146988,-1.67373539211956));
#55275=CARTESIAN_POINT('',(0.3,3.07385911146988,-1.67373539211956));
#55276=CARTESIAN_POINT('',(1.8,3.07385911146988,-1.67373539211956));
#55277=CARTESIAN_POINT('',(3.5,2.9271658647914,-1.69));
#55278=CARTESIAN_POINT('',(3.5,3.13689018343476,-1.66674682452695));
#55279=CARTESIAN_POINT('',(0.3,2.9271658647914,-1.69));
#55280=CARTESIAN_POINT('',(0.3,2.9271658647914,-1.69));
#55281=CARTESIAN_POINT('',(0.3,3.13689018343476,-1.66674682452695));
#55282=CARTESIAN_POINT('Origin',(0.3,3.00077802411308,-1.7325));
#55283=CARTESIAN_POINT('',(0.3,2.98642692452359,-1.8251723821274));
#55284=CARTESIAN_POINT('Origin',(0.3,0.,0.));
#55285=CARTESIAN_POINT('',(0.3,2.9271658647914,-1.69));
#55286=CARTESIAN_POINT('Origin',(0.3,2.9271658647914,-1.69));
#55287=CARTESIAN_POINT('',(3.5,2.98642692452359,-1.8251723821274));
#55288=CARTESIAN_POINT('',(1.8,2.98642692452358,-1.8251723821274));
#55289=CARTESIAN_POINT('',(3.5,2.9271658647914,-1.69));
#55290=CARTESIAN_POINT('Origin',(3.5,3.00077802411308,-1.7325));
#55291=CARTESIAN_POINT('Origin',(3.5,0.,0.));
#55292=CARTESIAN_POINT('Origin',(0.3,2.79980622428319,-2.18614045899734));
#55293=CARTESIAN_POINT('',(3.5,2.73651918390454,-2.18207762376191));
#55294=CARTESIAN_POINT('',(0.3,2.73651918390454,-2.18207762376191));
#55295=CARTESIAN_POINT('',(1.8,2.73651918390454,-2.18207762376191));
#55296=CARTESIAN_POINT('',(3.5,2.58923021774214,-2.1726221207405));
#55297=CARTESIAN_POINT('',(3.5,2.79980622428319,-2.18614045899734));
#55298=CARTESIAN_POINT('',(0.3,2.58923021774214,-2.1726221207405));
#55299=CARTESIAN_POINT('',(0.3,2.58923021774214,-2.1726221207405));
#55300=CARTESIAN_POINT('',(0.3,2.79980622428319,-2.18614045899734));
#55301=CARTESIAN_POINT('Origin',(0.3,2.65434399540726,-2.22725906756386));
#55302=CARTESIAN_POINT('',(0.3,2.6241185309908,-2.3160315056818));
#55303=CARTESIAN_POINT('Origin',(0.3,0.,0.));
#55304=CARTESIAN_POINT('',(0.3,2.58923021774214,-2.1726221207405));
#55305=CARTESIAN_POINT('Origin',(0.3,2.58923021774214,-2.1726221207405));
#55306=CARTESIAN_POINT('',(3.5,2.6241185309908,-2.3160315056818));
#55307=CARTESIAN_POINT('',(1.8,2.6241185309908,-2.3160315056818));
#55308=CARTESIAN_POINT('',(3.5,2.58923021774214,-2.1726221207405));
#55309=CARTESIAN_POINT('Origin',(3.5,2.65434399540726,-2.22725906756386));
#55310=CARTESIAN_POINT('Origin',(3.5,0.,0.));
#55311=CARTESIAN_POINT('Origin',(0.3,2.37765156977709,-2.63910932186155));
#55312=CARTESIAN_POINT('',(3.5,2.3160315056818,-2.6241185309908));
#55313=CARTESIAN_POINT('',(0.3,2.3160315056818,-2.6241185309908));
#55314=CARTESIAN_POINT('',(1.8,2.3160315056818,-2.6241185309908));
#55315=CARTESIAN_POINT('',(3.5,2.1726221207405,-2.58923021774215));
#55316=CARTESIAN_POINT('',(3.5,2.37765156977709,-2.63910932186155));
#55317=CARTESIAN_POINT('',(0.3,2.1726221207405,-2.58923021774215));
#55318=CARTESIAN_POINT('',(0.3,2.1726221207405,-2.58923021774215));
#55319=CARTESIAN_POINT('',(0.3,2.37765156977709,-2.63910932186155));
#55320=CARTESIAN_POINT('Origin',(0.3,2.22725906756386,-2.65434399540726));
#55321=CARTESIAN_POINT('',(0.3,2.1820776237619,-2.73651918390455));
#55322=CARTESIAN_POINT('Origin',(0.3,0.,0.));
#55323=CARTESIAN_POINT('',(0.3,2.1726221207405,-2.58923021774215));
#55324=CARTESIAN_POINT('Origin',(0.3,2.1726221207405,-2.58923021774215));
#55325=CARTESIAN_POINT('',(3.5,2.1820776237619,-2.73651918390455));
#55326=CARTESIAN_POINT('',(1.8,2.1820776237619,-2.73651918390455));
#55327=CARTESIAN_POINT('',(3.5,2.1726221207405,-2.58923021774215));
#55328=CARTESIAN_POINT('Origin',(3.5,2.22725906756386,-2.65434399540726));
#55329=CARTESIAN_POINT('Origin',(3.5,0.,0.));
#55330=CARTESIAN_POINT('Origin',(0.3,1.88325317547306,-3.01189018343476));
#55331=CARTESIAN_POINT('',(3.5,1.8251723821274,-2.98642692452359));
#55332=CARTESIAN_POINT('',(0.3,1.8251723821274,-2.98642692452359));
#55333=CARTESIAN_POINT('',(1.8,1.8251723821274,-2.98642692452359));
#55334=CARTESIAN_POINT('',(3.5,1.69,-2.9271658647914));
#55335=CARTESIAN_POINT('',(3.5,1.88325317547306,-3.01189018343476));
#55336=CARTESIAN_POINT('',(0.3,1.69,-2.9271658647914));
#55337=CARTESIAN_POINT('',(0.3,1.69,-2.9271658647914));
#55338=CARTESIAN_POINT('',(0.3,1.88325317547306,-3.01189018343476));
#55339=CARTESIAN_POINT('Origin',(0.3,1.7325,-3.00077802411308));
#55340=CARTESIAN_POINT('',(0.3,1.67373539211956,-3.07385911146988));
#55341=CARTESIAN_POINT('Origin',(0.3,0.,0.));
#55342=CARTESIAN_POINT('',(0.3,1.69,-2.9271658647914));
#55343=CARTESIAN_POINT('Origin',(0.3,1.69,-2.9271658647914));
#55344=CARTESIAN_POINT('',(3.5,1.67373539211956,-3.07385911146988));
#55345=CARTESIAN_POINT('',(1.8,1.67373539211956,-3.07385911146988));
#55346=CARTESIAN_POINT('',(3.5,1.69,-2.9271658647914));
#55347=CARTESIAN_POINT('Origin',(3.5,1.7325,-3.00077802411308));
#55348=CARTESIAN_POINT('Origin',(3.5,0.,0.));
#55349=CARTESIAN_POINT('Origin',(0.3,1.33163308640436,-3.29315628587427));
#55350=CARTESIAN_POINT('',(3.5,1.27885631932384,-3.25799424715967));
#55351=CARTESIAN_POINT('',(0.3,1.27885631932384,-3.25799424715967));
#55352=CARTESIAN_POINT('',(1.8,1.27885631932384,-3.25799424715967));
#55353=CARTESIAN_POINT('',(3.5,1.15602808444076,-3.17616105825637));
#55354=CARTESIAN_POINT('',(3.5,1.33163308640436,-3.29315628587427));
#55355=CARTESIAN_POINT('',(0.3,1.15602808444076,-3.17616105825637));
#55356=CARTESIAN_POINT('',(0.3,1.15602808444076,-3.17616105825637));
#55357=CARTESIAN_POINT('',(0.3,1.33163308640436,-3.29315628587427));
#55358=CARTESIAN_POINT('Origin',(0.3,1.18509979662344,-3.25603493102317));
#55359=CARTESIAN_POINT('',(0.3,1.11453755753863,-3.31780138538096));
#55360=CARTESIAN_POINT('Origin',(0.3,0.,0.));
#55361=CARTESIAN_POINT('',(0.3,1.15602808444076,-3.17616105825637));
#55362=CARTESIAN_POINT('Origin',(0.3,1.15602808444076,-3.17616105825637));
#55363=CARTESIAN_POINT('',(3.5,1.11453755753863,-3.31780138538096));
#55364=CARTESIAN_POINT('',(1.8,1.11453755753863,-3.31780138538096));
#55365=CARTESIAN_POINT('',(3.5,1.15602808444076,-3.17616105825637));
#55366=CARTESIAN_POINT('Origin',(3.5,1.18509979662344,-3.25603493102317));
#55367=CARTESIAN_POINT('Origin',(3.5,0.,0.));
#55368=CARTESIAN_POINT('Origin',(0.3,0.739551999844127,-3.47436150098497));
#55369=CARTESIAN_POINT('',(3.5,0.693682854390159,-3.43056906322043));
#55370=CARTESIAN_POINT('',(0.3,0.693682854390159,-3.43056906322043));
#55371=CARTESIAN_POINT('',(1.8,0.693682854390159,-3.43056906322043));
#55372=CARTESIAN_POINT('',(3.5,0.586930840514223,-3.32865020518126));
#55373=CARTESIAN_POINT('',(3.5,0.739551999844127,-3.47436150098497));
#55374=CARTESIAN_POINT('',(0.3,0.586930840514223,-3.32865020518126));
#55375=CARTESIAN_POINT('',(0.3,0.586930840514223,-3.32865020518126));
#55376=CARTESIAN_POINT('',(0.3,0.739551999844127,-3.47436150098497));
#55377=CARTESIAN_POINT('Origin',(0.3,0.601690935615912,-3.4123588641873));
#55378=CARTESIAN_POINT('',(0.3,0.521475063255118,-3.46093394308575));
#55379=CARTESIAN_POINT('Origin',(0.3,0.,0.));
#55380=CARTESIAN_POINT('',(0.3,0.586930840514223,-3.32865020518126));
#55381=CARTESIAN_POINT('Origin',(0.3,0.586930840514223,-3.32865020518126));
#55382=CARTESIAN_POINT('',(3.5,0.521475063255118,-3.46093394308575));
#55383=CARTESIAN_POINT('',(1.8,0.521475063255118,-3.46093394308575));
#55384=CARTESIAN_POINT('',(3.5,0.586930840514223,-3.32865020518126));
#55385=CARTESIAN_POINT('Origin',(3.5,0.601690935615912,-3.4123588641873));
#55386=CARTESIAN_POINT('Origin',(3.5,0.,0.));
#55387=CARTESIAN_POINT('Origin',(0.3,0.124999999999999,-3.55));
#55388=CARTESIAN_POINT('',(3.5,0.0874321869462905,-3.49890777424696));
#55389=CARTESIAN_POINT('',(0.3,0.0874321869462905,-3.49890777424696));
#55390=CARTESIAN_POINT('',(1.8,0.0874321869462905,-3.49890777424696));
#55391=CARTESIAN_POINT('',(3.5,-6.20895927167708E-16,-3.38));
#55392=CARTESIAN_POINT('',(3.5,0.124999999999999,-3.55));
#55393=CARTESIAN_POINT('',(0.3,-6.20895927167708E-16,-3.38));
#55394=CARTESIAN_POINT('',(0.3,-6.20895927167708E-16,-3.38));
#55395=CARTESIAN_POINT('',(0.3,0.124999999999999,-3.55));
#55396=CARTESIAN_POINT('Origin',(0.3,-6.36510173856837E-16,-3.465));
#55397=CARTESIAN_POINT('',(0.3,-0.0874321869462918,-3.49890777424696));
#55398=CARTESIAN_POINT('Origin',(0.3,0.,0.));
#55399=CARTESIAN_POINT('',(0.3,-6.20895927167708E-16,-3.38));
#55400=CARTESIAN_POINT('Origin',(0.3,-6.20895927167708E-16,-3.38));
#55401=CARTESIAN_POINT('',(3.5,-0.0874321869462918,-3.49890777424696));
#55402=CARTESIAN_POINT('',(1.8,-0.0874321869462921,-3.49890777424696));
#55403=CARTESIAN_POINT('',(3.5,-6.20895927167708E-16,-3.38));
#55404=CARTESIAN_POINT('Origin',(3.5,-6.36510173856837E-16,-3.465));
#55405=CARTESIAN_POINT('Origin',(3.5,0.,0.));
#55406=CARTESIAN_POINT('Origin',(0.3,-0.493350061591077,-3.51777354540171));
#55407=CARTESIAN_POINT('',(3.5,-0.521475063255118,-3.46093394308575));
#55408=CARTESIAN_POINT('',(0.3,-0.521475063255118,-3.46093394308575));
#55409=CARTESIAN_POINT('',(1.8,-0.521475063255118,-3.46093394308575));
#55410=CARTESIAN_POINT('',(3.5,-0.586930840514225,-3.32865020518126));
#55411=CARTESIAN_POINT('',(3.5,-0.493350061591077,-3.51777354540171));
#55412=CARTESIAN_POINT('',(0.3,-0.586930840514225,-3.32865020518126));
#55413=CARTESIAN_POINT('',(0.3,-0.586930840514225,-3.32865020518126));
#55414=CARTESIAN_POINT('',(0.3,-0.493350061591077,-3.51777354540171));
#55415=CARTESIAN_POINT('Origin',(0.3,-0.601690935615914,-3.4123588641873));
#55416=CARTESIAN_POINT('',(0.3,-0.693682854390159,-3.43056906322043));
#55417=CARTESIAN_POINT('Origin',(0.3,0.,0.));
#55418=CARTESIAN_POINT('',(0.3,-0.586930840514225,-3.32865020518126));
#55419=CARTESIAN_POINT('Origin',(0.3,-0.586930840514225,-3.32865020518126));
#55420=CARTESIAN_POINT('',(3.5,-0.693682854390159,-3.43056906322043));
#55421=CARTESIAN_POINT('',(1.8,-0.69368285439016,-3.43056906322043));
#55422=CARTESIAN_POINT('',(3.5,-0.586930840514225,-3.32865020518126));
#55423=CARTESIAN_POINT('Origin',(3.5,-0.601690935615914,-3.4123588641873));
#55424=CARTESIAN_POINT('Origin',(3.5,0.,0.));
#55425=CARTESIAN_POINT('Origin',(0.3,-1.09670993120789,-3.37866132170568));
#55426=CARTESIAN_POINT('',(3.5,-1.11453755753864,-3.31780138538096));
#55427=CARTESIAN_POINT('',(0.3,-1.11453755753864,-3.31780138538096));
#55428=CARTESIAN_POINT('',(1.8,-1.11453755753864,-3.31780138538096));
#55429=CARTESIAN_POINT('',(3.5,-1.15602808444076,-3.17616105825637));
#55430=CARTESIAN_POINT('',(3.5,-1.09670993120789,-3.37866132170568));
#55431=CARTESIAN_POINT('',(0.3,-1.15602808444076,-3.17616105825637));
#55432=CARTESIAN_POINT('',(0.3,-1.15602808444076,-3.17616105825637));
#55433=CARTESIAN_POINT('',(0.3,-1.09670993120789,-3.37866132170568));
#55434=CARTESIAN_POINT('Origin',(0.3,-1.18509979662344,-3.25603493102317));
#55435=CARTESIAN_POINT('',(0.3,-1.27885631932385,-3.25799424715966));
#55436=CARTESIAN_POINT('Origin',(0.3,0.,0.));
#55437=CARTESIAN_POINT('',(0.3,-1.15602808444076,-3.17616105825637));
#55438=CARTESIAN_POINT('Origin',(0.3,-1.15602808444076,-3.17616105825637));
#55439=CARTESIAN_POINT('',(3.5,-1.27885631932385,-3.25799424715966));
#55440=CARTESIAN_POINT('',(1.8,-1.27885631932385,-3.25799424715966));
#55441=CARTESIAN_POINT('',(3.5,-1.15602808444076,-3.17616105825637));
#55442=CARTESIAN_POINT('Origin',(3.5,-1.18509979662344,-3.25603493102317));
#55443=CARTESIAN_POINT('Origin',(3.5,0.,0.));
#55444=CARTESIAN_POINT('Origin',(0.3,-1.66674682452695,-3.13689018343476));
#55445=CARTESIAN_POINT('',(3.5,-1.67373539211956,-3.07385911146988));
#55446=CARTESIAN_POINT('',(0.3,-1.67373539211956,-3.07385911146988));
#55447=CARTESIAN_POINT('',(1.8,-1.67373539211956,-3.07385911146988));
#55448=CARTESIAN_POINT('',(3.5,-1.69,-2.9271658647914));
#55449=CARTESIAN_POINT('',(3.5,-1.66674682452695,-3.13689018343476));
#55450=CARTESIAN_POINT('',(0.3,-1.69,-2.9271658647914));
#55451=CARTESIAN_POINT('',(0.3,-1.69,-2.9271658647914));
#55452=CARTESIAN_POINT('',(0.3,-1.66674682452695,-3.13689018343476));
#55453=CARTESIAN_POINT('Origin',(0.3,-1.7325,-3.00077802411308));
#55454=CARTESIAN_POINT('',(0.3,-1.8251723821274,-2.98642692452359));
#55455=CARTESIAN_POINT('Origin',(0.3,0.,0.));
#55456=CARTESIAN_POINT('',(0.3,-1.69,-2.9271658647914));
#55457=CARTESIAN_POINT('Origin',(0.3,-1.69,-2.9271658647914));
#55458=CARTESIAN_POINT('',(3.5,-1.8251723821274,-2.98642692452359));
#55459=CARTESIAN_POINT('',(1.8,-1.8251723821274,-2.98642692452358));
#55460=CARTESIAN_POINT('',(3.5,-1.69,-2.9271658647914));
#55461=CARTESIAN_POINT('Origin',(3.5,-1.7325,-3.00077802411308));
#55462=CARTESIAN_POINT('Origin',(3.5,0.,0.));
#55463=CARTESIAN_POINT('Origin',(0.3,-2.18614045899734,-2.79980622428319));
#55464=CARTESIAN_POINT('',(3.5,-2.1820776237619,-2.73651918390454));
#55465=CARTESIAN_POINT('',(0.3,-2.1820776237619,-2.73651918390454));
#55466=CARTESIAN_POINT('',(1.8,-2.1820776237619,-2.73651918390454));
#55467=CARTESIAN_POINT('',(3.5,-2.1726221207405,-2.58923021774214));
#55468=CARTESIAN_POINT('',(3.5,-2.18614045899734,-2.79980622428319));
#55469=CARTESIAN_POINT('',(0.3,-2.1726221207405,-2.58923021774214));
#55470=CARTESIAN_POINT('',(0.3,-2.1726221207405,-2.58923021774214));
#55471=CARTESIAN_POINT('',(0.3,-2.18614045899734,-2.79980622428319));
#55472=CARTESIAN_POINT('Origin',(0.3,-2.22725906756386,-2.65434399540726));
#55473=CARTESIAN_POINT('',(0.3,-2.3160315056818,-2.6241185309908));
#55474=CARTESIAN_POINT('Origin',(0.3,0.,0.));
#55475=CARTESIAN_POINT('',(0.3,-2.1726221207405,-2.58923021774214));
#55476=CARTESIAN_POINT('Origin',(0.3,-2.1726221207405,-2.58923021774214));
#55477=CARTESIAN_POINT('',(3.5,-2.3160315056818,-2.6241185309908));
#55478=CARTESIAN_POINT('',(1.8,-2.3160315056818,-2.6241185309908));
#55479=CARTESIAN_POINT('',(3.5,-2.1726221207405,-2.58923021774214));
#55480=CARTESIAN_POINT('Origin',(3.5,-2.22725906756386,-2.65434399540726));
#55481=CARTESIAN_POINT('Origin',(3.5,0.,0.));
#55482=CARTESIAN_POINT('Origin',(0.3,-2.63910932186155,-2.37765156977709));
#55483=CARTESIAN_POINT('',(3.5,-2.6241185309908,-2.3160315056818));
#55484=CARTESIAN_POINT('',(0.3,-2.6241185309908,-2.3160315056818));
#55485=CARTESIAN_POINT('',(1.8,-2.6241185309908,-2.3160315056818));
#55486=CARTESIAN_POINT('',(3.5,-2.58923021774215,-2.1726221207405));
#55487=CARTESIAN_POINT('',(3.5,-2.63910932186155,-2.37765156977709));
#55488=CARTESIAN_POINT('',(0.3,-2.58923021774215,-2.1726221207405));
#55489=CARTESIAN_POINT('',(0.3,-2.58923021774215,-2.1726221207405));
#55490=CARTESIAN_POINT('',(0.3,-2.63910932186155,-2.37765156977709));
#55491=CARTESIAN_POINT('Origin',(0.3,-2.65434399540726,-2.22725906756386));
#55492=CARTESIAN_POINT('',(0.3,-2.73651918390455,-2.1820776237619));
#55493=CARTESIAN_POINT('Origin',(0.3,0.,0.));
#55494=CARTESIAN_POINT('',(0.3,-2.58923021774215,-2.1726221207405));
#55495=CARTESIAN_POINT('Origin',(0.3,-2.58923021774215,-2.1726221207405));
#55496=CARTESIAN_POINT('',(3.5,-2.73651918390455,-2.1820776237619));
#55497=CARTESIAN_POINT('',(1.8,-2.73651918390455,-2.1820776237619));
#55498=CARTESIAN_POINT('',(3.5,-2.58923021774215,-2.1726221207405));
#55499=CARTESIAN_POINT('Origin',(3.5,-2.65434399540726,-2.22725906756386));
#55500=CARTESIAN_POINT('Origin',(3.5,0.,0.));
#55501=CARTESIAN_POINT('Origin',(0.3,-3.01189018343476,-1.88325317547305));
#55502=CARTESIAN_POINT('',(3.5,-2.98642692452359,-1.8251723821274));
#55503=CARTESIAN_POINT('',(0.3,-2.98642692452359,-1.8251723821274));
#55504=CARTESIAN_POINT('',(1.8,-2.98642692452359,-1.8251723821274));
#55505=CARTESIAN_POINT('',(3.5,-2.9271658647914,-1.69));
#55506=CARTESIAN_POINT('',(3.5,-3.01189018343476,-1.88325317547305));
#55507=CARTESIAN_POINT('',(0.3,-2.9271658647914,-1.69));
#55508=CARTESIAN_POINT('',(0.3,-2.9271658647914,-1.69));
#55509=CARTESIAN_POINT('',(0.3,-3.01189018343476,-1.88325317547305));
#55510=CARTESIAN_POINT('Origin',(0.3,-3.00077802411308,-1.7325));
#55511=CARTESIAN_POINT('',(0.3,-3.07385911146988,-1.67373539211956));
#55512=CARTESIAN_POINT('Origin',(0.3,0.,0.));
#55513=CARTESIAN_POINT('',(0.3,-2.9271658647914,-1.69));
#55514=CARTESIAN_POINT('Origin',(0.3,-2.9271658647914,-1.69));
#55515=CARTESIAN_POINT('',(3.5,-3.07385911146988,-1.67373539211956));
#55516=CARTESIAN_POINT('',(1.8,-3.07385911146988,-1.67373539211956));
#55517=CARTESIAN_POINT('',(3.5,-2.9271658647914,-1.69));
#55518=CARTESIAN_POINT('Origin',(3.5,-3.00077802411308,-1.7325));
#55519=CARTESIAN_POINT('Origin',(3.5,0.,0.));
#55520=CARTESIAN_POINT('Origin',(0.3,-3.29315628587427,-1.33163308640436));
#55521=CARTESIAN_POINT('',(3.5,-3.25799424715966,-1.27885631932384));
#55522=CARTESIAN_POINT('',(0.3,-3.25799424715966,-1.27885631932384));
#55523=CARTESIAN_POINT('',(1.8,-3.25799424715966,-1.27885631932384));
#55524=CARTESIAN_POINT('',(3.5,-3.17616105825637,-1.15602808444076));
#55525=CARTESIAN_POINT('',(3.5,-3.29315628587427,-1.33163308640436));
#55526=CARTESIAN_POINT('',(0.3,-3.17616105825637,-1.15602808444076));
#55527=CARTESIAN_POINT('',(0.3,-3.17616105825637,-1.15602808444076));
#55528=CARTESIAN_POINT('',(0.3,-3.29315628587427,-1.33163308640436));
#55529=CARTESIAN_POINT('Origin',(0.3,-3.25603493102317,-1.18509979662344));
#55530=CARTESIAN_POINT('',(0.3,-3.31780138538096,-1.11453755753864));
#55531=CARTESIAN_POINT('Origin',(0.3,0.,0.));
#55532=CARTESIAN_POINT('',(0.3,-3.17616105825637,-1.15602808444076));
#55533=CARTESIAN_POINT('Origin',(0.3,-3.17616105825637,-1.15602808444076));
#55534=CARTESIAN_POINT('',(3.5,-3.31780138538096,-1.11453755753864));
#55535=CARTESIAN_POINT('',(1.8,-3.31780138538096,-1.11453755753864));
#55536=CARTESIAN_POINT('',(3.5,-3.17616105825637,-1.15602808444076));
#55537=CARTESIAN_POINT('Origin',(3.5,-3.25603493102317,-1.18509979662344));
#55538=CARTESIAN_POINT('Origin',(3.5,0.,0.));
#55539=CARTESIAN_POINT('Origin',(0.3,-3.47436150098497,-0.739551999844128));
#55540=CARTESIAN_POINT('',(3.5,-3.43056906322043,-0.693682854390159));
#55541=CARTESIAN_POINT('',(0.3,-3.43056906322043,-0.693682854390159));
#55542=CARTESIAN_POINT('',(1.8,-3.43056906322043,-0.693682854390159));
#55543=CARTESIAN_POINT('',(3.5,-3.32865020518126,-0.586930840514224));
#55544=CARTESIAN_POINT('',(3.5,-3.47436150098497,-0.739551999844128));
#55545=CARTESIAN_POINT('',(0.3,-3.32865020518126,-0.586930840514224));
#55546=CARTESIAN_POINT('',(0.3,-3.32865020518126,-0.586930840514224));
#55547=CARTESIAN_POINT('',(0.3,-3.47436150098497,-0.739551999844128));
#55548=CARTESIAN_POINT('Origin',(0.3,-3.4123588641873,-0.601690935615913));
#55549=CARTESIAN_POINT('',(0.3,-3.46093394308575,-0.521475063255118));
#55550=CARTESIAN_POINT('Origin',(0.3,0.,0.));
#55551=CARTESIAN_POINT('',(0.3,-3.32865020518126,-0.586930840514224));
#55552=CARTESIAN_POINT('Origin',(0.3,-3.32865020518126,-0.586930840514224));
#55553=CARTESIAN_POINT('',(3.5,-3.46093394308575,-0.521475063255118));
#55554=CARTESIAN_POINT('',(1.8,-3.46093394308575,-0.521475063255118));
#55555=CARTESIAN_POINT('',(3.5,-3.32865020518126,-0.586930840514224));
#55556=CARTESIAN_POINT('Origin',(3.5,-3.4123588641873,-0.601690935615913));
#55557=CARTESIAN_POINT('Origin',(3.5,0.,0.));
#55558=CARTESIAN_POINT('Origin',(0.3,-3.55,-0.125));
#55559=CARTESIAN_POINT('',(3.5,-3.49890777424696,-0.087432186946291));
#55560=CARTESIAN_POINT('',(0.3,-3.49890777424696,-0.087432186946291));
#55561=CARTESIAN_POINT('',(1.8,-3.49890777424696,-0.087432186946291));
#55562=CARTESIAN_POINT('',(3.5,-3.38,4.13930618111805E-16));
#55563=CARTESIAN_POINT('',(3.5,-3.55,-0.125));
#55564=CARTESIAN_POINT('',(0.3,-3.38,4.13930618111805E-16));
#55565=CARTESIAN_POINT('',(0.3,-3.38,4.13930618111805E-16));
#55566=CARTESIAN_POINT('',(0.3,-3.55,-0.125));
#55567=CARTESIAN_POINT('Origin',(0.3,-3.465,4.24340115904558E-16));
#55568=CARTESIAN_POINT('',(0.3,-3.5,-4.28626379701574E-16));
#55569=CARTESIAN_POINT('Origin',(0.3,0.,0.));
#55570=CARTESIAN_POINT('',(0.3,-3.49890777424696,0.0874321869462918));
#55571=CARTESIAN_POINT('',(0.3,-3.38,4.13930618111805E-16));
#55572=CARTESIAN_POINT('Origin',(0.3,0.,0.));
#55573=CARTESIAN_POINT('Origin',(0.3,-3.38,4.13930618111805E-16));
#55574=CARTESIAN_POINT('',(3.5,-3.49890777424696,0.0874321869462918));
#55575=CARTESIAN_POINT('',(1.8,-3.49890777424696,0.0874321869462913));
#55576=CARTESIAN_POINT('',(3.5,-3.38,4.13930618111805E-16));
#55577=CARTESIAN_POINT('Origin',(3.5,-3.465,4.24340115904558E-16));
#55578=CARTESIAN_POINT('',(3.5,-3.5,-4.28626379701574E-16));
#55579=CARTESIAN_POINT('Origin',(3.5,0.,0.));
#55580=CARTESIAN_POINT('Origin',(3.5,0.,0.));
#55581=CARTESIAN_POINT('Origin',(0.3,-3.5177735454017,0.493350061591078));
#55582=CARTESIAN_POINT('',(3.5,-3.46093394308575,0.52147506325512));
#55583=CARTESIAN_POINT('',(0.3,-3.46093394308575,0.52147506325512));
#55584=CARTESIAN_POINT('',(1.8,-3.46093394308575,0.52147506325512));
#55585=CARTESIAN_POINT('',(3.5,-3.32865020518126,0.586930840514226));
#55586=CARTESIAN_POINT('',(3.5,-3.5177735454017,0.493350061591078));
#55587=CARTESIAN_POINT('',(0.3,-3.32865020518126,0.586930840514226));
#55588=CARTESIAN_POINT('',(0.3,-3.32865020518126,0.586930840514226));
#55589=CARTESIAN_POINT('',(0.3,-3.5177735454017,0.493350061591078));
#55590=CARTESIAN_POINT('Origin',(0.3,-3.4123588641873,0.601690935615915));
#55591=CARTESIAN_POINT('',(0.3,-3.43056906322043,0.693682854390161));
#55592=CARTESIAN_POINT('Origin',(0.3,0.,0.));
#55593=CARTESIAN_POINT('',(0.3,-3.32865020518126,0.586930840514226));
#55594=CARTESIAN_POINT('Origin',(0.3,-3.32865020518126,0.586930840514226));
#55595=CARTESIAN_POINT('',(3.5,-3.43056906322043,0.693682854390161));
#55596=CARTESIAN_POINT('',(1.8,-3.43056906322043,0.693682854390161));
#55597=CARTESIAN_POINT('',(3.5,-3.32865020518126,0.586930840514226));
#55598=CARTESIAN_POINT('Origin',(3.5,-3.4123588641873,0.601690935615915));
#55599=CARTESIAN_POINT('Origin',(3.5,0.,0.));
#55600=CARTESIAN_POINT('Origin',(0.3,-3.37866132170568,1.09670993120789));
#55601=CARTESIAN_POINT('',(3.5,-3.31780138538096,1.11453755753864));
#55602=CARTESIAN_POINT('',(0.3,-3.31780138538096,1.11453755753864));
#55603=CARTESIAN_POINT('',(1.8,-3.31780138538096,1.11453755753864));
#55604=CARTESIAN_POINT('',(3.5,-3.17616105825637,1.15602808444076));
#55605=CARTESIAN_POINT('',(3.5,-3.37866132170568,1.09670993120789));
#55606=CARTESIAN_POINT('',(0.3,-3.17616105825637,1.15602808444076));
#55607=CARTESIAN_POINT('',(0.3,-3.17616105825637,1.15602808444076));
#55608=CARTESIAN_POINT('',(0.3,-3.37866132170568,1.09670993120789));
#55609=CARTESIAN_POINT('Origin',(0.3,-3.25603493102317,1.18509979662344));
#55610=CARTESIAN_POINT('',(0.3,-3.25799424715966,1.27885631932384));
#55611=CARTESIAN_POINT('Origin',(0.3,0.,0.));
#55612=CARTESIAN_POINT('',(0.3,-3.17616105825637,1.15602808444076));
#55613=CARTESIAN_POINT('Origin',(0.3,-3.17616105825637,1.15602808444076));
#55614=CARTESIAN_POINT('',(3.5,-3.25799424715966,1.27885631932384));
#55615=CARTESIAN_POINT('',(1.8,-3.25799424715966,1.27885631932384));
#55616=CARTESIAN_POINT('',(3.5,-3.17616105825637,1.15602808444076));
#55617=CARTESIAN_POINT('Origin',(3.5,-3.25603493102317,1.18509979662344));
#55618=CARTESIAN_POINT('Origin',(3.5,0.,0.));
#55619=CARTESIAN_POINT('Origin',(0.3,-3.13689018343476,1.66674682452694));
#55620=CARTESIAN_POINT('',(3.5,-3.07385911146988,1.67373539211956));
#55621=CARTESIAN_POINT('',(0.3,-3.07385911146988,1.67373539211956));
#55622=CARTESIAN_POINT('',(1.8,-3.07385911146988,1.67373539211956));
#55623=CARTESIAN_POINT('',(3.5,-2.9271658647914,1.69));
#55624=CARTESIAN_POINT('',(3.5,-3.13689018343476,1.66674682452694));
#55625=CARTESIAN_POINT('',(0.3,-2.9271658647914,1.69));
#55626=CARTESIAN_POINT('',(0.3,-2.9271658647914,1.69));
#55627=CARTESIAN_POINT('',(0.3,-3.13689018343476,1.66674682452694));
#55628=CARTESIAN_POINT('Origin',(0.3,-3.00077802411308,1.7325));
#55629=CARTESIAN_POINT('',(0.3,-2.98642692452359,1.8251723821274));
#55630=CARTESIAN_POINT('Origin',(0.3,0.,0.));
#55631=CARTESIAN_POINT('',(0.3,-2.9271658647914,1.69));
#55632=CARTESIAN_POINT('Origin',(0.3,-2.9271658647914,1.69));
#55633=CARTESIAN_POINT('',(3.5,-2.98642692452359,1.8251723821274));
#55634=CARTESIAN_POINT('',(1.8,-2.98642692452359,1.8251723821274));
#55635=CARTESIAN_POINT('',(3.5,-2.9271658647914,1.69));
#55636=CARTESIAN_POINT('Origin',(3.5,-3.00077802411308,1.7325));
#55637=CARTESIAN_POINT('Origin',(3.5,0.,0.));
#55638=CARTESIAN_POINT('Origin',(0.3,-2.79980622428319,2.18614045899734));
#55639=CARTESIAN_POINT('',(3.5,-2.73651918390454,2.1820776237619));
#55640=CARTESIAN_POINT('',(0.3,-2.73651918390454,2.1820776237619));
#55641=CARTESIAN_POINT('',(1.8,-2.73651918390454,2.1820776237619));
#55642=CARTESIAN_POINT('',(3.5,-2.58923021774214,2.1726221207405));
#55643=CARTESIAN_POINT('',(3.5,-2.79980622428319,2.18614045899734));
#55644=CARTESIAN_POINT('',(0.3,-2.58923021774214,2.1726221207405));
#55645=CARTESIAN_POINT('',(0.3,-2.58923021774214,2.1726221207405));
#55646=CARTESIAN_POINT('',(0.3,-2.79980622428319,2.18614045899734));
#55647=CARTESIAN_POINT('Origin',(0.3,-2.65434399540726,2.22725906756386));
#55648=CARTESIAN_POINT('',(0.3,-2.6241185309908,2.3160315056818));
#55649=CARTESIAN_POINT('Origin',(0.3,0.,0.));
#55650=CARTESIAN_POINT('',(0.3,-2.58923021774214,2.1726221207405));
#55651=CARTESIAN_POINT('Origin',(0.3,-2.58923021774214,2.1726221207405));
#55652=CARTESIAN_POINT('',(3.5,-2.6241185309908,2.3160315056818));
#55653=CARTESIAN_POINT('',(1.8,-2.6241185309908,2.3160315056818));
#55654=CARTESIAN_POINT('',(3.5,-2.58923021774214,2.1726221207405));
#55655=CARTESIAN_POINT('Origin',(3.5,-2.65434399540726,2.22725906756386));
#55656=CARTESIAN_POINT('Origin',(3.5,0.,0.));
#55657=CARTESIAN_POINT('Origin',(0.3,-2.37765156977709,2.63910932186155));
#55658=CARTESIAN_POINT('',(3.5,-2.3160315056818,2.6241185309908));
#55659=CARTESIAN_POINT('',(0.3,-2.3160315056818,2.6241185309908));
#55660=CARTESIAN_POINT('',(1.8,-2.3160315056818,2.6241185309908));
#55661=CARTESIAN_POINT('',(3.5,-2.1726221207405,2.58923021774215));
#55662=CARTESIAN_POINT('',(3.5,-2.37765156977709,2.63910932186155));
#55663=CARTESIAN_POINT('',(0.3,-2.1726221207405,2.58923021774215));
#55664=CARTESIAN_POINT('',(0.3,-2.1726221207405,2.58923021774215));
#55665=CARTESIAN_POINT('',(0.3,-2.37765156977709,2.63910932186155));
#55666=CARTESIAN_POINT('Origin',(0.3,-2.22725906756386,2.65434399540726));
#55667=CARTESIAN_POINT('',(0.3,-2.1820776237619,2.73651918390455));
#55668=CARTESIAN_POINT('Origin',(0.3,0.,0.));
#55669=CARTESIAN_POINT('',(0.3,-2.1726221207405,2.58923021774215));
#55670=CARTESIAN_POINT('Origin',(0.3,-2.1726221207405,2.58923021774215));
#55671=CARTESIAN_POINT('',(3.5,-2.1820776237619,2.73651918390455));
#55672=CARTESIAN_POINT('',(1.8,-2.1820776237619,2.73651918390455));
#55673=CARTESIAN_POINT('',(3.5,-2.1726221207405,2.58923021774215));
#55674=CARTESIAN_POINT('Origin',(3.5,-2.22725906756386,2.65434399540726));
#55675=CARTESIAN_POINT('Origin',(3.5,0.,0.));
#55676=CARTESIAN_POINT('Origin',(0.3,-1.88325317547305,3.01189018343476));
#55677=CARTESIAN_POINT('',(3.5,-1.8251723821274,2.98642692452359));
#55678=CARTESIAN_POINT('',(0.3,-1.8251723821274,2.98642692452359));
#55679=CARTESIAN_POINT('',(1.8,-1.8251723821274,2.98642692452359));
#55680=CARTESIAN_POINT('',(3.5,-1.69,2.9271658647914));
#55681=CARTESIAN_POINT('',(3.5,-1.88325317547305,3.01189018343476));
#55682=CARTESIAN_POINT('',(0.3,-1.69,2.9271658647914));
#55683=CARTESIAN_POINT('',(0.3,-1.69,2.9271658647914));
#55684=CARTESIAN_POINT('',(0.3,-1.88325317547305,3.01189018343476));
#55685=CARTESIAN_POINT('Origin',(0.3,-1.7325,3.00077802411308));
#55686=CARTESIAN_POINT('',(0.3,-1.67373539211956,3.07385911146988));
#55687=CARTESIAN_POINT('Origin',(0.3,0.,0.));
#55688=CARTESIAN_POINT('',(0.3,-1.69,2.9271658647914));
#55689=CARTESIAN_POINT('Origin',(0.3,-1.69,2.9271658647914));
#55690=CARTESIAN_POINT('',(3.5,-1.67373539211956,3.07385911146988));
#55691=CARTESIAN_POINT('',(1.8,-1.67373539211956,3.07385911146988));
#55692=CARTESIAN_POINT('',(3.5,-1.69,2.9271658647914));
#55693=CARTESIAN_POINT('Origin',(3.5,-1.7325,3.00077802411308));
#55694=CARTESIAN_POINT('Origin',(3.5,0.,0.));
#55695=CARTESIAN_POINT('Origin',(0.3,-1.33163308640436,3.29315628587427));
#55696=CARTESIAN_POINT('',(3.5,-1.27885631932384,3.25799424715966));
#55697=CARTESIAN_POINT('',(0.3,-1.27885631932384,3.25799424715966));
#55698=CARTESIAN_POINT('',(1.8,-1.27885631932384,3.25799424715966));
#55699=CARTESIAN_POINT('',(3.5,-1.15602808444076,3.17616105825637));
#55700=CARTESIAN_POINT('',(3.5,-1.33163308640436,3.29315628587427));
#55701=CARTESIAN_POINT('',(0.3,-1.15602808444076,3.17616105825637));
#55702=CARTESIAN_POINT('',(0.3,-1.15602808444076,3.17616105825637));
#55703=CARTESIAN_POINT('',(0.3,-1.33163308640436,3.29315628587427));
#55704=CARTESIAN_POINT('Origin',(0.3,-1.18509979662344,3.25603493102317));
#55705=CARTESIAN_POINT('',(0.3,-1.11453755753864,3.31780138538096));
#55706=CARTESIAN_POINT('Origin',(0.3,0.,0.));
#55707=CARTESIAN_POINT('',(0.3,-1.15602808444076,3.17616105825637));
#55708=CARTESIAN_POINT('Origin',(0.3,-1.15602808444076,3.17616105825637));
#55709=CARTESIAN_POINT('',(3.5,-1.11453755753864,3.31780138538096));
#55710=CARTESIAN_POINT('',(1.8,-1.11453755753864,3.31780138538096));
#55711=CARTESIAN_POINT('',(3.5,-1.15602808444076,3.17616105825637));
#55712=CARTESIAN_POINT('Origin',(3.5,-1.18509979662344,3.25603493102317));
#55713=CARTESIAN_POINT('Origin',(3.5,0.,0.));
#55714=CARTESIAN_POINT('Origin',(0.3,-0.739551999844129,3.47436150098497));
#55715=CARTESIAN_POINT('',(3.5,-0.69368285439016,3.43056906322043));
#55716=CARTESIAN_POINT('',(0.3,-0.69368285439016,3.43056906322043));
#55717=CARTESIAN_POINT('',(1.8,-0.69368285439016,3.43056906322043));
#55718=CARTESIAN_POINT('',(3.5,-0.586930840514225,3.32865020518126));
#55719=CARTESIAN_POINT('',(3.5,-0.739551999844129,3.47436150098497));
#55720=CARTESIAN_POINT('',(0.3,-0.586930840514225,3.32865020518126));
#55721=CARTESIAN_POINT('',(0.3,-0.586930840514225,3.32865020518126));
#55722=CARTESIAN_POINT('',(0.3,-0.739551999844129,3.47436150098497));
#55723=CARTESIAN_POINT('Origin',(0.3,-0.601690935615914,3.4123588641873));
#55724=CARTESIAN_POINT('',(0.3,-0.521475063255119,3.46093394308575));
#55725=CARTESIAN_POINT('Origin',(0.3,0.,0.));
#55726=CARTESIAN_POINT('',(0.3,-0.586930840514225,3.32865020518126));
#55727=CARTESIAN_POINT('Origin',(0.3,-0.586930840514225,3.32865020518126));
#55728=CARTESIAN_POINT('',(3.5,-0.521475063255119,3.46093394308575));
#55729=CARTESIAN_POINT('',(1.8,-0.521475063255119,3.46093394308575));
#55730=CARTESIAN_POINT('',(3.5,-0.586930840514225,3.32865020518126));
#55731=CARTESIAN_POINT('Origin',(3.5,-0.601690935615914,3.4123588641873));
#55732=CARTESIAN_POINT('Origin',(3.5,0.,0.));
#55733=CARTESIAN_POINT('Origin',(0.3,-0.125,3.55));
#55734=CARTESIAN_POINT('',(3.5,-0.0874321869462913,3.49890777424696));
#55735=CARTESIAN_POINT('',(0.3,-0.0874321869462913,3.49890777424696));
#55736=CARTESIAN_POINT('',(1.8,-0.0874321869462916,3.49890777424696));
#55737=CARTESIAN_POINT('',(3.5,2.06965309055903E-16,3.38));
#55738=CARTESIAN_POINT('',(3.5,-0.125,3.55));
#55739=CARTESIAN_POINT('',(0.3,2.06965309055903E-16,3.38));
#55740=CARTESIAN_POINT('',(0.3,2.06965309055903E-16,3.38));
#55741=CARTESIAN_POINT('',(0.3,-0.125,3.55));
#55742=CARTESIAN_POINT('Origin',(0.3,2.12170057952279E-16,3.465));
#55743=CARTESIAN_POINT('',(0.3,0.0874321869462921,3.49890777424696));
#55744=CARTESIAN_POINT('Origin',(0.3,0.,0.));
#55745=CARTESIAN_POINT('',(0.3,2.06965309055903E-16,3.38));
#55746=CARTESIAN_POINT('Origin',(0.3,2.06965309055903E-16,3.38));
#55747=CARTESIAN_POINT('',(3.5,0.0874321869462921,3.49890777424696));
#55748=CARTESIAN_POINT('',(1.8,0.0874321869462918,3.49890777424696));
#55749=CARTESIAN_POINT('',(3.5,2.06965309055903E-16,3.38));
#55750=CARTESIAN_POINT('Origin',(3.5,2.12170057952279E-16,3.465));
#55751=CARTESIAN_POINT('Origin',(3.5,0.,0.));
#55752=CARTESIAN_POINT('Origin',(0.3,0.493350061591077,3.51777354540171));
#55753=CARTESIAN_POINT('',(3.5,0.521475063255119,3.46093394308575));
#55754=CARTESIAN_POINT('',(0.3,0.521475063255119,3.46093394308575));
#55755=CARTESIAN_POINT('',(1.8,0.521475063255119,3.46093394308575));
#55756=CARTESIAN_POINT('',(3.5,0.586930840514225,3.32865020518126));
#55757=CARTESIAN_POINT('',(3.5,0.493350061591077,3.51777354540171));
#55758=CARTESIAN_POINT('',(0.3,0.586930840514225,3.32865020518126));
#55759=CARTESIAN_POINT('',(0.3,0.586930840514225,3.32865020518126));
#55760=CARTESIAN_POINT('',(0.3,0.493350061591077,3.51777354540171));
#55761=CARTESIAN_POINT('Origin',(0.3,0.601690935615914,3.4123588641873));
#55762=CARTESIAN_POINT('',(0.3,0.693682854390159,3.43056906322043));
#55763=CARTESIAN_POINT('Origin',(0.3,0.,0.));
#55764=CARTESIAN_POINT('',(0.3,0.586930840514225,3.32865020518126));
#55765=CARTESIAN_POINT('Origin',(0.3,0.586930840514225,3.32865020518126));
#55766=CARTESIAN_POINT('',(3.5,0.693682854390159,3.43056906322043));
#55767=CARTESIAN_POINT('',(1.8,0.693682854390159,3.43056906322043));
#55768=CARTESIAN_POINT('',(3.5,0.586930840514225,3.32865020518126));
#55769=CARTESIAN_POINT('Origin',(3.5,0.601690935615914,3.4123588641873));
#55770=CARTESIAN_POINT('Origin',(3.5,0.,0.));
#55771=CARTESIAN_POINT('Origin',(0.3,1.09670993120789,3.37866132170568));
#55772=CARTESIAN_POINT('',(3.5,1.11453755753864,3.31780138538096));
#55773=CARTESIAN_POINT('',(0.3,1.11453755753864,3.31780138538096));
#55774=CARTESIAN_POINT('',(1.8,1.11453755753864,3.31780138538096));
#55775=CARTESIAN_POINT('',(3.5,1.15602808444076,3.17616105825637));
#55776=CARTESIAN_POINT('',(3.5,1.09670993120789,3.37866132170568));
#55777=CARTESIAN_POINT('',(0.3,1.15602808444076,3.17616105825637));
#55778=CARTESIAN_POINT('',(0.3,1.15602808444076,3.17616105825637));
#55779=CARTESIAN_POINT('',(0.3,1.09670993120789,3.37866132170568));
#55780=CARTESIAN_POINT('Origin',(0.3,1.18509979662344,3.25603493102317));
#55781=CARTESIAN_POINT('',(0.3,1.27885631932384,3.25799424715966));
#55782=CARTESIAN_POINT('Origin',(0.3,0.,0.));
#55783=CARTESIAN_POINT('',(0.3,1.15602808444076,3.17616105825637));
#55784=CARTESIAN_POINT('Origin',(0.3,1.15602808444076,3.17616105825637));
#55785=CARTESIAN_POINT('',(3.5,1.27885631932384,3.25799424715966));
#55786=CARTESIAN_POINT('',(1.8,1.27885631932384,3.25799424715966));
#55787=CARTESIAN_POINT('',(3.5,1.15602808444076,3.17616105825637));
#55788=CARTESIAN_POINT('Origin',(3.5,1.18509979662344,3.25603493102317));
#55789=CARTESIAN_POINT('Origin',(3.5,0.,0.));
#55790=CARTESIAN_POINT('Origin',(0.3,1.66674682452695,3.13689018343476));
#55791=CARTESIAN_POINT('',(3.5,1.67373539211956,3.07385911146988));
#55792=CARTESIAN_POINT('',(0.3,1.67373539211956,3.07385911146988));
#55793=CARTESIAN_POINT('',(1.8,1.67373539211956,3.07385911146988));
#55794=CARTESIAN_POINT('',(3.5,1.69,2.9271658647914));
#55795=CARTESIAN_POINT('',(3.5,1.66674682452695,3.13689018343476));
#55796=CARTESIAN_POINT('',(0.3,1.69,2.9271658647914));
#55797=CARTESIAN_POINT('',(0.3,1.69,2.9271658647914));
#55798=CARTESIAN_POINT('',(0.3,1.66674682452695,3.13689018343476));
#55799=CARTESIAN_POINT('Origin',(0.3,1.7325,3.00077802411308));
#55800=CARTESIAN_POINT('',(0.3,1.8251723821274,2.98642692452359));
#55801=CARTESIAN_POINT('Origin',(0.3,0.,0.));
#55802=CARTESIAN_POINT('',(0.3,1.69,2.9271658647914));
#55803=CARTESIAN_POINT('Origin',(0.3,1.69,2.9271658647914));
#55804=CARTESIAN_POINT('',(3.5,1.8251723821274,2.98642692452359));
#55805=CARTESIAN_POINT('',(1.8,1.8251723821274,2.98642692452359));
#55806=CARTESIAN_POINT('',(3.5,1.69,2.9271658647914));
#55807=CARTESIAN_POINT('Origin',(3.5,1.7325,3.00077802411308));
#55808=CARTESIAN_POINT('Origin',(3.5,0.,0.));
#55809=CARTESIAN_POINT('Origin',(0.3,2.18614045899734,2.79980622428319));
#55810=CARTESIAN_POINT('',(3.5,2.1820776237619,2.73651918390455));
#55811=CARTESIAN_POINT('',(0.3,2.1820776237619,2.73651918390455));
#55812=CARTESIAN_POINT('',(1.8,2.1820776237619,2.73651918390455));
#55813=CARTESIAN_POINT('',(3.5,2.1726221207405,2.58923021774215));
#55814=CARTESIAN_POINT('',(3.5,2.18614045899734,2.79980622428319));
#55815=CARTESIAN_POINT('',(0.3,2.1726221207405,2.58923021774215));
#55816=CARTESIAN_POINT('',(0.3,2.1726221207405,2.58923021774215));
#55817=CARTESIAN_POINT('',(0.3,2.18614045899734,2.79980622428319));
#55818=CARTESIAN_POINT('Origin',(0.3,2.22725906756386,2.65434399540726));
#55819=CARTESIAN_POINT('',(0.3,2.3160315056818,2.6241185309908));
#55820=CARTESIAN_POINT('Origin',(0.3,0.,0.));
#55821=CARTESIAN_POINT('',(0.3,2.1726221207405,2.58923021774215));
#55822=CARTESIAN_POINT('Origin',(0.3,2.1726221207405,2.58923021774215));
#55823=CARTESIAN_POINT('',(3.5,2.3160315056818,2.6241185309908));
#55824=CARTESIAN_POINT('',(1.8,2.3160315056818,2.6241185309908));
#55825=CARTESIAN_POINT('',(3.5,2.1726221207405,2.58923021774215));
#55826=CARTESIAN_POINT('Origin',(3.5,2.22725906756386,2.65434399540726));
#55827=CARTESIAN_POINT('Origin',(3.5,0.,0.));
#55828=CARTESIAN_POINT('Origin',(0.3,2.63910932186155,2.37765156977709));
#55829=CARTESIAN_POINT('',(3.5,2.6241185309908,2.3160315056818));
#55830=CARTESIAN_POINT('',(0.3,2.6241185309908,2.3160315056818));
#55831=CARTESIAN_POINT('',(1.8,2.6241185309908,2.3160315056818));
#55832=CARTESIAN_POINT('',(3.5,2.58923021774215,2.1726221207405));
#55833=CARTESIAN_POINT('',(3.5,2.63910932186155,2.37765156977709));
#55834=CARTESIAN_POINT('',(0.3,2.58923021774215,2.1726221207405));
#55835=CARTESIAN_POINT('',(0.3,2.58923021774215,2.1726221207405));
#55836=CARTESIAN_POINT('',(0.3,2.63910932186155,2.37765156977709));
#55837=CARTESIAN_POINT('Origin',(0.3,2.65434399540726,2.22725906756386));
#55838=CARTESIAN_POINT('',(0.3,2.73651918390455,2.1820776237619));
#55839=CARTESIAN_POINT('Origin',(0.3,0.,0.));
#55840=CARTESIAN_POINT('',(0.3,2.58923021774215,2.1726221207405));
#55841=CARTESIAN_POINT('Origin',(0.3,2.58923021774215,2.1726221207405));
#55842=CARTESIAN_POINT('',(3.5,2.73651918390455,2.1820776237619));
#55843=CARTESIAN_POINT('',(1.8,2.73651918390455,2.1820776237619));
#55844=CARTESIAN_POINT('',(3.5,2.58923021774215,2.1726221207405));
#55845=CARTESIAN_POINT('Origin',(3.5,2.65434399540726,2.22725906756386));
#55846=CARTESIAN_POINT('Origin',(3.5,0.,0.));
#55847=CARTESIAN_POINT('Origin',(0.3,3.01189018343476,1.88325317547305));
#55848=CARTESIAN_POINT('',(3.5,2.98642692452359,1.8251723821274));
#55849=CARTESIAN_POINT('',(0.3,2.98642692452359,1.8251723821274));
#55850=CARTESIAN_POINT('',(1.8,2.98642692452359,1.8251723821274));
#55851=CARTESIAN_POINT('',(3.5,2.9271658647914,1.69));
#55852=CARTESIAN_POINT('',(3.5,3.01189018343476,1.88325317547305));
#55853=CARTESIAN_POINT('',(0.3,2.9271658647914,1.69));
#55854=CARTESIAN_POINT('',(0.3,2.9271658647914,1.69));
#55855=CARTESIAN_POINT('',(0.3,3.01189018343476,1.88325317547305));
#55856=CARTESIAN_POINT('Origin',(0.3,3.00077802411308,1.7325));
#55857=CARTESIAN_POINT('',(0.3,3.07385911146988,1.67373539211956));
#55858=CARTESIAN_POINT('Origin',(0.3,0.,0.));
#55859=CARTESIAN_POINT('',(0.3,2.9271658647914,1.69));
#55860=CARTESIAN_POINT('Origin',(0.3,2.9271658647914,1.69));
#55861=CARTESIAN_POINT('',(3.5,3.07385911146988,1.67373539211956));
#55862=CARTESIAN_POINT('',(1.8,3.07385911146988,1.67373539211956));
#55863=CARTESIAN_POINT('',(3.5,2.9271658647914,1.69));
#55864=CARTESIAN_POINT('Origin',(3.5,3.00077802411308,1.7325));
#55865=CARTESIAN_POINT('Origin',(3.5,0.,0.));
#55866=CARTESIAN_POINT('Origin',(0.3,3.29315628587427,1.33163308640436));
#55867=CARTESIAN_POINT('',(3.5,3.25799424715966,1.27885631932384));
#55868=CARTESIAN_POINT('',(0.3,3.25799424715966,1.27885631932384));
#55869=CARTESIAN_POINT('',(1.8,3.25799424715966,1.27885631932384));
#55870=CARTESIAN_POINT('',(3.5,3.17616105825637,1.15602808444076));
#55871=CARTESIAN_POINT('',(3.5,3.29315628587427,1.33163308640436));
#55872=CARTESIAN_POINT('',(0.3,3.17616105825637,1.15602808444076));
#55873=CARTESIAN_POINT('',(0.3,3.17616105825637,1.15602808444076));
#55874=CARTESIAN_POINT('',(0.3,3.29315628587427,1.33163308640436));
#55875=CARTESIAN_POINT('Origin',(0.3,3.25603493102317,1.18509979662344));
#55876=CARTESIAN_POINT('',(0.3,3.31780138538096,1.11453755753864));
#55877=CARTESIAN_POINT('Origin',(0.3,0.,0.));
#55878=CARTESIAN_POINT('',(0.3,3.17616105825637,1.15602808444076));
#55879=CARTESIAN_POINT('Origin',(0.3,3.17616105825637,1.15602808444076));
#55880=CARTESIAN_POINT('',(3.5,3.31780138538096,1.11453755753864));
#55881=CARTESIAN_POINT('',(1.8,3.31780138538096,1.11453755753864));
#55882=CARTESIAN_POINT('',(3.5,3.17616105825637,1.15602808444076));
#55883=CARTESIAN_POINT('Origin',(3.5,3.25603493102317,1.18509979662344));
#55884=CARTESIAN_POINT('Origin',(3.5,0.,0.));
#55885=CARTESIAN_POINT('Origin',(0.3,3.47436150098497,0.739551999844129));
#55886=CARTESIAN_POINT('',(3.5,3.43056906322043,0.69368285439016));
#55887=CARTESIAN_POINT('',(0.3,3.43056906322043,0.69368285439016));
#55888=CARTESIAN_POINT('',(1.8,3.43056906322043,0.69368285439016));
#55889=CARTESIAN_POINT('',(3.5,3.32865020518126,0.586930840514225));
#55890=CARTESIAN_POINT('',(3.5,3.47436150098497,0.739551999844129));
#55891=CARTESIAN_POINT('',(0.3,3.32865020518126,0.586930840514225));
#55892=CARTESIAN_POINT('',(0.3,3.32865020518126,0.586930840514225));
#55893=CARTESIAN_POINT('',(0.3,3.47436150098497,0.739551999844129));
#55894=CARTESIAN_POINT('Origin',(0.3,3.4123588641873,0.601690935615914));
#55895=CARTESIAN_POINT('',(0.3,3.46093394308575,0.521475063255119));
#55896=CARTESIAN_POINT('Origin',(0.3,0.,0.));
#55897=CARTESIAN_POINT('',(0.3,3.32865020518126,0.586930840514225));
#55898=CARTESIAN_POINT('Origin',(0.3,3.32865020518126,0.586930840514225));
#55899=CARTESIAN_POINT('',(3.5,3.46093394308575,0.521475063255119));
#55900=CARTESIAN_POINT('',(1.8,3.46093394308575,0.521475063255119));
#55901=CARTESIAN_POINT('',(3.5,3.32865020518126,0.586930840514225));
#55902=CARTESIAN_POINT('Origin',(3.5,3.4123588641873,0.601690935615914));
#55903=CARTESIAN_POINT('Origin',(3.5,0.,0.));
#55904=CARTESIAN_POINT('Origin',(0.3,3.55,0.125));
#55905=CARTESIAN_POINT('',(3.5,3.49890777424696,0.0874321869462918));
#55906=CARTESIAN_POINT('',(0.3,3.49890777424696,0.0874321869462918));
#55907=CARTESIAN_POINT('',(1.8,3.49890777424696,0.0874321869462916));
#55908=CARTESIAN_POINT('',(3.5,3.38,0.));
#55909=CARTESIAN_POINT('',(3.5,3.55,0.125));
#55910=CARTESIAN_POINT('',(0.3,3.38,0.));
#55911=CARTESIAN_POINT('',(0.3,3.38,0.));
#55912=CARTESIAN_POINT('',(0.3,3.55,0.125));
#55913=CARTESIAN_POINT('Origin',(0.3,3.465,0.));
#55914=CARTESIAN_POINT('',(0.3,3.49890777424696,-0.0874321869462918));
#55915=CARTESIAN_POINT('Origin',(0.3,0.,0.));
#55916=CARTESIAN_POINT('',(0.3,3.38,0.));
#55917=CARTESIAN_POINT('Origin',(0.3,3.38,0.));
#55918=CARTESIAN_POINT('',(3.5,3.49890777424696,-0.0874321869462918));
#55919=CARTESIAN_POINT('',(1.8,3.49890777424696,-0.0874321869462916));
#55920=CARTESIAN_POINT('',(3.5,3.38,0.));
#55921=CARTESIAN_POINT('Origin',(3.5,3.465,0.));
#55922=CARTESIAN_POINT('Origin',(3.5,0.,0.));
#55923=CARTESIAN_POINT('Origin',(1.55435453572933,0.,0.));
#55924=CARTESIAN_POINT('',(1.09870907145866,0.,0.));
#55925=CARTESIAN_POINT('',(2.,-1.483539833954,1.81681230905937E-16));
#55926=CARTESIAN_POINT('',(1.55435453572933,-0.75,-9.18485099360515E-17));
#55927=CARTESIAN_POINT('Origin',(2.,0.,0.));
#55928=CARTESIAN_POINT('Origin',(4.,0.,1.73205080756888));
#55929=CARTESIAN_POINT('',(4.,1.06057523872491E-16,1.73205080756888));
#55930=CARTESIAN_POINT('',(4.,1.5,0.866025403784439));
#55931=CARTESIAN_POINT('',(4.,0.375,1.51554445662277));
#55932=CARTESIAN_POINT('',(2.,0.,1.73205080756888));
#55933=CARTESIAN_POINT('',(4.,1.06057523872491E-16,1.73205080756888));
#55934=CARTESIAN_POINT('',(2.,1.5,0.866025403784439));
#55935=CARTESIAN_POINT('',(2.,1.5,0.866025403784439));
#55936=CARTESIAN_POINT('',(4.,1.5,0.866025403784439));
#55937=CARTESIAN_POINT('Origin',(4.,-1.5,0.866025403784439));
#55938=CARTESIAN_POINT('',(4.,-1.5,0.866025403784439));
#55939=CARTESIAN_POINT('',(4.,-1.125,1.08253175473055));
#55940=CARTESIAN_POINT('',(2.,-1.5,0.866025403784439));
#55941=CARTESIAN_POINT('',(4.,-1.5,0.866025403784439));
#55942=CARTESIAN_POINT('',(2.,1.06057523872491E-16,1.73205080756888));
#55943=CARTESIAN_POINT('Origin',(4.,-1.5,-0.866025403784439));
#55944=CARTESIAN_POINT('',(4.,-1.5,-0.866025403784439));
#55945=CARTESIAN_POINT('',(4.,-1.5,-0.43301270189222));
#55946=CARTESIAN_POINT('',(2.,-1.5,-0.866025403784439));
#55947=CARTESIAN_POINT('',(4.,-1.5,-0.866025403784439));
#55948=CARTESIAN_POINT('',(2.,-1.5,0.866025403784439));
#55949=CARTESIAN_POINT('Origin',(4.,-2.77555756156289E-16,-1.73205080756888));
#55950=CARTESIAN_POINT('',(4.,-3.18172571617472E-16,-1.73205080756888));
#55951=CARTESIAN_POINT('',(4.,-0.375,-1.51554445662277));
#55952=CARTESIAN_POINT('',(2.,-2.77555756156289E-16,-1.73205080756888));
#55953=CARTESIAN_POINT('',(4.,-3.18172571617472E-16,-1.73205080756888));
#55954=CARTESIAN_POINT('',(2.,-1.5,-0.866025403784439));
#55955=CARTESIAN_POINT('Origin',(4.,1.5,-0.866025403784439));
#55956=CARTESIAN_POINT('',(4.,1.5,-0.866025403784439));
#55957=CARTESIAN_POINT('',(4.,1.125,-1.08253175473055));
#55958=CARTESIAN_POINT('',(2.,1.5,-0.866025403784439));
#55959=CARTESIAN_POINT('',(4.,1.5,-0.866025403784439));
#55960=CARTESIAN_POINT('',(2.,-3.18172571617472E-16,-1.73205080756888));
#55961=CARTESIAN_POINT('Origin',(4.,1.5,0.866025403784439));
#55962=CARTESIAN_POINT('',(4.,1.5,0.433012701892219));
#55963=CARTESIAN_POINT('',(2.,1.5,-0.866025403784439));
#55964=CARTESIAN_POINT('Origin',(2.,0.,0.));
#55965=CARTESIAN_POINT('Origin',(-30.,1.6,0.));
#55966=CARTESIAN_POINT('',(-30.,-1.6,-1.95943487863576E-16));
#55967=CARTESIAN_POINT('Origin',(-30.,0.,0.));
#55968=CARTESIAN_POINT('Origin',(-29.8,0.,0.));
#55969=CARTESIAN_POINT('',(-29.8,-1.8,-2.20436423846524E-16));
#55970=CARTESIAN_POINT('Origin',(1.8,0.,0.));
#55971=CARTESIAN_POINT('',(3.6,-3.5,-4.28626379701574E-16));
#55972=CARTESIAN_POINT('Origin',(3.6,0.,0.));
#55973=CARTESIAN_POINT('',(1.8,-3.5,-4.28626379701574E-16));
#55974=CARTESIAN_POINT('',(1.8,-3.5,-4.28626379701574E-16));
#55975=CARTESIAN_POINT('Origin',(3.8,0.,0.));
#55976=CARTESIAN_POINT('',(4.,-3.1,-3.79640507735679E-16));
#55977=CARTESIAN_POINT('Origin',(4.,0.,0.));
#55978=CARTESIAN_POINT('',(3.8,-3.3,-4.04133443718627E-16));
#55979=CARTESIAN_POINT('Origin',(4.,0.,0.));
#55980=CARTESIAN_POINT('',(0.,0.,0.));
#55981=CARTESIAN_POINT('Origin',(0.,1.2,0.));
#55982=CARTESIAN_POINT('',(-5.72458747072346E-16,-1.2,-1.46957615897682E-16));
#55983=CARTESIAN_POINT('Origin',(0.,0.,0.));
#55984=CARTESIAN_POINT('Origin',(0.149999999999999,0.,0.));
#55985=CARTESIAN_POINT('',(0.3,-1.5,-1.83697019872103E-16));
#55986=CARTESIAN_POINT('Origin',(0.3,0.,0.));
#55987=CARTESIAN_POINT('',(0.149999999999999,-1.35,-1.65327317884893E-16));
#55988=CARTESIAN_POINT('Origin',(9.,0.,0.));
#55989=CARTESIAN_POINT('',(17.7,-1.5,-1.83697019872103E-16));
#55990=CARTESIAN_POINT('Origin',(17.7,0.,0.));
#55991=CARTESIAN_POINT('',(9.,-1.5,-1.83697019872103E-16));
#55992=CARTESIAN_POINT('Origin',(17.85,0.,0.));
#55993=CARTESIAN_POINT('',(18.,-1.2,-1.46957615897682E-16));
#55994=CARTESIAN_POINT('Origin',(18.,0.,0.));
#55995=CARTESIAN_POINT('',(17.85,-1.35,-1.65327317884893E-16));
#55996=CARTESIAN_POINT('Origin',(18.,0.,0.));
#55997=CARTESIAN_POINT('',(0.,0.,0.));
#55998=CARTESIAN_POINT('Origin',(-17.3,0.,0.));
#55999=CARTESIAN_POINT('',(-34.4758449541571,-1.46537014458274,0.000897397219902993));
#56000=CARTESIAN_POINT('',(-34.5471550458428,-1.46483013109474,0.00162234200369738));
#56001=CARTESIAN_POINT('',(-17.3,-1.4635,-1.79227059055215E-16));
#56002=CARTESIAN_POINT('',(-34.6365,0.634777570163803,1.32001124579653));
#56003=CARTESIAN_POINT('Ctrl Pts',(-34.4758449541571,-1.46537014458274,
0.000897397219902993));
#56004=CARTESIAN_POINT('Ctrl Pts',(-34.4783310796223,-1.46566838207244,
0.0464499273981202));
#56005=CARTESIAN_POINT('Ctrl Pts',(-34.4808172050875,-1.46372976632423,
0.0919749017138783));
#56006=CARTESIAN_POINT('Ctrl Pts',(-34.4833033305527,-1.4594716333831,0.137279627198249));
#56007=CARTESIAN_POINT('Ctrl Pts',(-34.5098178729584,-1.41405862104037,
0.620454785430562));
#56008=CARTESIAN_POINT('Ctrl Pts',(-34.5363324153641,-1.10481827728657,
1.07857832446841));
#56009=CARTESIAN_POINT('Ctrl Pts',(-34.5628469577697,-0.673702411121009,
1.30178944989929));
#56010=CARTESIAN_POINT('Ctrl Pts',(-34.5873979718465,-0.274512731095817,
1.50847072686393));
#56011=CARTESIAN_POINT('Ctrl Pts',(-34.6119489859233,0.22916992251388,1.51374407429557));
#56012=CARTESIAN_POINT('Ctrl Pts',(-34.6365,0.635548045752396,1.32098221395621));
#56013=CARTESIAN_POINT('',(-34.6365,-0.63400709457496,1.31904027763697));
#56014=CARTESIAN_POINT('Origin',(-34.6365,0.,0.));
#56015=CARTESIAN_POINT('Ctrl Pts',(-34.6365,-0.63400709457496,1.31904027763697));
#56016=CARTESIAN_POINT('Ctrl Pts',(-34.6099854575943,-1.07350019101018,
1.10779446059807));
#56017=CARTESIAN_POINT('Ctrl Pts',(-34.5834709151886,-1.39526457424107,
0.66143532399529));
#56018=CARTESIAN_POINT('Ctrl Pts',(-34.5569563727829,-1.45465419899784,
0.18052244014254));
#56019=CARTESIAN_POINT('Ctrl Pts',(-34.5536892638029,-1.46197215958701,
0.121264589208655));
#56020=CARTESIAN_POINT('Ctrl Pts',(-34.5504221548229,-1.46530647157864,
0.0614821070656839));
#56021=CARTESIAN_POINT('Ctrl Pts',(-34.5471550458428,-1.46483013109474,
0.00162234200369738));
#56022=CARTESIAN_POINT('Origin',(-17.3,0.,0.));
#56023=CARTESIAN_POINT('',(-33.9758449541571,-1.4616392812288,0.000897080157781296));
#56024=CARTESIAN_POINT('',(-34.0471550458428,-1.461397981138,0.000713649214188957));
#56025=CARTESIAN_POINT('',(-17.3,-1.4635,-1.79227059055215E-16));
#56026=CARTESIAN_POINT('Ctrl Pts',(-33.9758449541571,-1.4616392812288,0.000897080157781296));
#56027=CARTESIAN_POINT('Ctrl Pts',(-33.9859104918548,-1.46267180320561,
0.186551578039893));
#56028=CARTESIAN_POINT('Ctrl Pts',(-33.9959760295526,-1.42989485312375,
0.371854708030454));
#56029=CARTESIAN_POINT('Ctrl Pts',(-34.0060415672503,-1.36164030601831,
0.543008955714544));
#56030=CARTESIAN_POINT('Ctrl Pts',(-34.032556109656,-1.18184483577603,0.993861825616221));
#56031=CARTESIAN_POINT('Ctrl Pts',(-34.0590706520617,-0.755871778961322,
1.3465361831291));
#56032=CARTESIAN_POINT('Ctrl Pts',(-34.0855851944674,-0.279385519054958,
1.43904678126577));
#56033=CARTESIAN_POINT('Ctrl Pts',(-34.1120997368731,0.197100740851406,
1.53155737940244));
#56034=CARTESIAN_POINT('Ctrl Pts',(-34.1386142792788,0.724100203849429,
1.3639042181629));
#56035=CARTESIAN_POINT('Ctrl Pts',(-34.1651288216845,1.05953716804195,1.01307402656519));
#56036=CARTESIAN_POINT('Ctrl Pts',(-34.1916433640901,1.39497413223448,0.662243834967482));
#56037=CARTESIAN_POINT('Ctrl Pts',(-34.2181579064958,1.53884859762151,0.128236613011602));
#56038=CARTESIAN_POINT('Ctrl Pts',(-34.2446724489015,1.42508057453266,-0.34361308056253));
#56039=CARTESIAN_POINT('Ctrl Pts',(-34.2711869913072,1.31131255144381,-0.815462774136661));
#56040=CARTESIAN_POINT('Ctrl Pts',(-34.2977015337129,0.939902039879098,
-1.22515493932904));
#56041=CARTESIAN_POINT('Ctrl Pts',(-34.3242160761186,0.481438861446158,
-1.38458468548627));
#56042=CARTESIAN_POINT('Ctrl Pts',(-34.3507306185242,0.0229756830132183,
-1.54401443164349));
#56043=CARTESIAN_POINT('Ctrl Pts',(-34.3772451609299,-0.522540162287944,
-1.45318175876555));
#56044=CARTESIAN_POINT('Ctrl Pts',(-34.4037597033356,-0.904505244472703,
-1.1536520336132));
#56045=CARTESIAN_POINT('Ctrl Pts',(-34.4277881202761,-1.25065552347862,
-0.88220759335438));
#56046=CARTESIAN_POINT('Ctrl Pts',(-34.4518165372166,-1.46248767752697,
-0.439368069321345));
#56047=CARTESIAN_POINT('Ctrl Pts',(-34.4758449541571,-1.46537014458274,
0.000897397219902993));
#56048=CARTESIAN_POINT('Ctrl Pts',(-34.5471550458428,-1.46483013109474,
0.00162234200369738));
#56049=CARTESIAN_POINT('Ctrl Pts',(-34.5239076124172,-1.46144068380198,
-0.424315669752557));
#56050=CARTESIAN_POINT('Ctrl Pts',(-34.5006601789915,-1.26511130217635,
-0.854166649541362));
#56051=CARTESIAN_POINT('Ctrl Pts',(-34.4774127455659,-0.938168170832327,
-1.12676217466842));
#56052=CARTESIAN_POINT('Ctrl Pts',(-34.4508982031602,-0.565277651627364,
-1.4376672745239));
#56053=CARTESIAN_POINT('Ctrl Pts',(-34.4243836607545,-0.0224817469347706,
-1.54401084313214));
#56054=CARTESIAN_POINT('Ctrl Pts',(-34.3978691183488,0.440521457961799,
-1.39802412172701));
#56055=CARTESIAN_POINT('Ctrl Pts',(-34.3713545759431,0.903524662858368,
-1.25203740032188));
#56056=CARTESIAN_POINT('Ctrl Pts',(-34.3448400335375,1.28673516795891,-0.853720388903368));
#56057=CARTESIAN_POINT('Ctrl Pts',(-34.3183254911318,1.41432065046245,-0.385486997806588));
#56058=CARTESIAN_POINT('Ctrl Pts',(-34.2918109487261,1.54190613296599,0.0827463932901925));
#56059=CARTESIAN_POINT('Ctrl Pts',(-34.2652964063204,1.41386659287251,0.620896164065243));
#56060=CARTESIAN_POINT('Ctrl Pts',(-34.2387818639147,1.08891519320202,0.981481756368469));
#56061=CARTESIAN_POINT('Ctrl Pts',(-34.212267321509,0.763963793531522,1.34206734867169));
#56062=CARTESIAN_POINT('Ctrl Pts',(-34.1857527791033,0.242100534284002,
1.5250887625031));
#56063=CARTESIAN_POINT('Ctrl Pts',(-34.1592382366976,-0.236909082514337,
1.44662785965613));
#56064=CARTESIAN_POINT('Ctrl Pts',(-34.132723694292,-0.715918699312675,
1.36816695680916));
#56065=CARTESIAN_POINT('Ctrl Pts',(-34.1062091518863,-1.15207467366184,
1.02822373728382));
#56066=CARTESIAN_POINT('Ctrl Pts',(-34.0796946094806,-1.34506104653608,
0.582868204388268));
#56067=CARTESIAN_POINT('Ctrl Pts',(-34.068848088268,-1.42400756407709,0.400682965782681));
#56068=CARTESIAN_POINT('Ctrl Pts',(-34.0580015670554,-1.46226087156527,
0.200857506589857));
#56069=CARTESIAN_POINT('Ctrl Pts',(-34.0471550458428,-1.461397981138,0.000713649214188957));
#56070=CARTESIAN_POINT('Origin',(-17.3,0.,0.));
#56071=CARTESIAN_POINT('',(-33.4758449541571,-1.46210997131077,-0.00113575995333209));
#56072=CARTESIAN_POINT('',(-33.5471550458428,-1.46247549057344,-0.00124878738715978));
#56073=CARTESIAN_POINT('',(-17.3,-1.4635,-1.79227059055215E-16));
#56074=CARTESIAN_POINT('Ctrl Pts',(-33.4758449541571,-1.46210997131077,
-0.00113575995333209));
#56075=CARTESIAN_POINT('Ctrl Pts',(-33.4934899040874,-1.45976617832587,
0.324054087244827));
#56076=CARTESIAN_POINT('Ctrl Pts',(-33.5111348540177,-1.35274610243324,
0.650643945905838));
#56077=CARTESIAN_POINT('Ctrl Pts',(-33.528779803948,-1.15337718085729,0.904788922614451));
#56078=CARTESIAN_POINT('Ctrl Pts',(-33.5552943463537,-0.853791421397257,
1.28668503389574));
#56079=CARTESIAN_POINT('Ctrl Pts',(-33.5818088887594,-0.345680300135375,
1.50499929303762));
#56080=CARTESIAN_POINT('Ctrl Pts',(-33.608323431165,0.137560532310046,1.45945151745205));
#56081=CARTESIAN_POINT('Ctrl Pts',(-33.6348379735707,0.620801364755467,
1.41390374186649));
#56082=CARTESIAN_POINT('Ctrl Pts',(-33.6613525159764,1.07917190838443,1.10449393155347));
#56083=CARTESIAN_POINT('Ctrl Pts',(-33.6878670583821,1.30212421740846,0.673345854018389));
#56084=CARTESIAN_POINT('Ctrl Pts',(-33.7143816007878,1.5250765264325,0.242197776483304));
#56085=CARTESIAN_POINT('Ctrl Pts',(-33.7408961431935,1.51261060085162,-0.310688568273853));
#56086=CARTESIAN_POINT('Ctrl Pts',(-33.7674106855992,1.27045269311141,-0.731349505481218));
#56087=CARTESIAN_POINT('Ctrl Pts',(-33.7939252280048,1.0282947853712,-1.15201044268858));
#56088=CARTESIAN_POINT('Ctrl Pts',(-33.8204397704105,0.556444895471674,
-1.44044597234615));
#56089=CARTESIAN_POINT('Ctrl Pts',(-33.8469543128162,0.071642192326496,
-1.46416793330233));
#56090=CARTESIAN_POINT('Ctrl Pts',(-33.8734688552219,-0.413160510818682,
-1.48788989425851));
#56091=CARTESIAN_POINT('Ctrl Pts',(-33.8999833976276,-0.91091602720951,
-1.24689828651329));
#56092=CARTESIAN_POINT('Ctrl Pts',(-33.9264979400333,-1.19298484356999,
-0.851886791495445));
#56093=CARTESIAN_POINT('Ctrl Pts',(-33.9429469447412,-1.36797376916733,
-0.606830857969515));
#56094=CARTESIAN_POINT('Ctrl Pts',(-33.9593959494492,-1.45995194376432,
-0.302497711200068));
#56095=CARTESIAN_POINT('Ctrl Pts',(-33.9758449541571,-1.4616392812288,0.000897080157781296));
#56096=CARTESIAN_POINT('Ctrl Pts',(-34.0471550458428,-1.461397981138,0.000713649214188957));
#56097=CARTESIAN_POINT('Ctrl Pts',(-34.0314870246497,-1.46015151831025,
-0.288398236298732));
#56098=CARTESIAN_POINT('Ctrl Pts',(-34.0158190034566,-1.37728366376588,
-0.578174503939485));
#56099=CARTESIAN_POINT('Ctrl Pts',(-34.0001509822635,-1.21754783627738,
-0.81640383976837));
#56100=CARTESIAN_POINT('Ctrl Pts',(-33.9736364398579,-0.947231481745092,
-1.2195525047637));
#56101=CARTESIAN_POINT('Ctrl Pts',(-33.9471218974522,-0.456782001281173,
-1.47508198848859));
#56102=CARTESIAN_POINT('Ctrl Pts',(-33.9206073550465,0.0285098714968319,
-1.46563947024646));
#56103=CARTESIAN_POINT('Ctrl Pts',(-33.8940928126408,0.513801744274836,
-1.45619695200433));
#56104=CARTESIAN_POINT('Ctrl Pts',(-33.8675782702351,0.993936009366925,
-1.18178243179517));
#56105=CARTESIAN_POINT('Ctrl Pts',(-33.8410637278294,1.24837193381408,-0.76843381664129));
#56106=CARTESIAN_POINT('Ctrl Pts',(-33.8145491854237,1.50280785826124,-0.355085201487411));
#56107=CARTESIAN_POINT('Ctrl Pts',(-33.7880346430181,1.53154544206345,0.197197508611189));
#56108=CARTESIAN_POINT('Ctrl Pts',(-33.7615201006124,1.32138222003508,0.634722724967845));
#56109=CARTESIAN_POINT('Ctrl Pts',(-33.7350055582067,1.1112189980067,1.0722479413245));
#56110=CARTESIAN_POINT('Ctrl Pts',(-33.708491015801,0.662154970147739,1.39501566393922));
#56111=CARTESIAN_POINT('Ctrl Pts',(-33.6819764733953,0.180464277792477,
1.4547690367785));
#56112=CARTESIAN_POINT('Ctrl Pts',(-33.6554619309896,-0.301226414562783,
1.51452240961778));
#56113=CARTESIAN_POINT('Ctrl Pts',(-33.6289473885839,-0.815543771414339,
1.31126143268162));
#56114=CARTESIAN_POINT('Ctrl Pts',(-33.6024328461783,-1.12624192354582,
0.938350275931457));
#56115=CARTESIAN_POINT('Ctrl Pts',(-33.5840069127331,-1.34215752884309,
0.679200559142212));
#56116=CARTESIAN_POINT('Ctrl Pts',(-33.565580979288,-1.45973783110767,0.33812044750393));
#56117=CARTESIAN_POINT('Ctrl Pts',(-33.5471550458428,-1.46247549057344,
-0.00124878738715978));
#56118=CARTESIAN_POINT('Origin',(-17.3,0.,0.));
#56119=CARTESIAN_POINT('',(-32.9758449541571,-1.46576386267191,-0.000435669595795773));
#56120=CARTESIAN_POINT('',(-33.0471550458428,-1.46589447233764,-0.0001750908953165));
#56121=CARTESIAN_POINT('',(-17.3,-1.4635,-1.79227059055215E-16));
#56122=CARTESIAN_POINT('Ctrl Pts',(-32.9758449541571,-1.46576386267191,
-0.000435669595795773));
#56123=CARTESIAN_POINT('Ctrl Pts',(-33.0010693163199,-1.46395560202229,
0.461460515586922));
#56124=CARTESIAN_POINT('Ctrl Pts',(-33.0262936784828,-1.22744187685039,
0.924951081530073));
#56125=CARTESIAN_POINT('Ctrl Pts',(-33.0515180406456,-0.851584434241105,
1.19319982047713));
#56126=CARTESIAN_POINT('Ctrl Pts',(-33.0780325830513,-0.456502567107242,
1.47516899449099));
#56127=CARTESIAN_POINT('Ctrl Pts',(-33.104547125457,0.0925419150148735,
1.54141303362098));
#56128=CARTESIAN_POINT('Ctrl Pts',(-33.1310616678627,0.543350994710775,
1.36150341542638));
#56129=CARTESIAN_POINT('Ctrl Pts',(-33.1575762102684,0.994160074406676,
1.18159379723179));
#56130=CARTESIAN_POINT('Ctrl Pts',(-33.1840907526741,1.34673375167636,0.755530521712624));
#56131=CARTESIAN_POINT('Ctrl Pts',(-33.2106052950797,1.43912087941628,0.279021425816014));
#56132=CARTESIAN_POINT('Ctrl Pts',(-33.2371198374854,1.53150800715619,-0.197487670080597));
#56133=CARTESIAN_POINT('Ctrl Pts',(-33.2636343798911,1.36370858536632,-0.724442586354652));
#56134=CARTESIAN_POINT('Ctrl Pts',(-33.2901489222968,1.01279958114557,-1.05979190284854));
#56135=CARTESIAN_POINT('Ctrl Pts',(-33.3166634647025,0.661890576924812,
-1.39514121934244));
#56136=CARTESIAN_POINT('Ctrl Pts',(-33.3431780071082,0.127871990273167,
-1.53888493605617));
#56137=CARTESIAN_POINT('Ctrl Pts',(-33.3696925495139,-0.34396015959519,
-1.42499587153609));
#56138=CARTESIAN_POINT('Ctrl Pts',(-33.3962070919196,-0.815792309463548,
-1.31110680701601));
#56139=CARTESIAN_POINT('Ctrl Pts',(-33.4227216343252,-1.22543802254862,
-0.939584961262129));
#56140=CARTESIAN_POINT('Ctrl Pts',(-33.4492361767309,-1.38473068026206,
-0.481085056674836));
#56141=CARTESIAN_POINT('Ctrl Pts',(-33.4581057692063,-1.43801694621464,
-0.327708572122606));
#56142=CARTESIAN_POINT('Ctrl Pts',(-33.4669753616817,-1.46328812646025,
-0.164599041695517));
#56143=CARTESIAN_POINT('Ctrl Pts',(-33.4758449541571,-1.46210997131077,
-0.00113575995333209));
#56144=CARTESIAN_POINT('Ctrl Pts',(-33.5471550458428,-1.46247549057344,
-0.00124878738715978));
#56145=CARTESIAN_POINT('Ctrl Pts',(-33.5390664368823,-1.46367726724064,
-0.150224959609039));
#56146=CARTESIAN_POINT('Ctrl Pts',(-33.5309778279217,-1.44274851149922,
-0.298871440590991));
#56147=CARTESIAN_POINT('Ctrl Pts',(-33.5228892189612,-1.39829282246071,
-0.44011278706805));
#56148=CARTESIAN_POINT('Ctrl Pts',(-33.4963746765555,-1.25256662183269,
-0.903103356753219));
#56149=CARTESIAN_POINT('Ctrl Pts',(-33.4698601341498,-0.854035273165233,
-1.28652315955938));
#56150=CARTESIAN_POINT('Ctrl Pts',(-33.4433455917441,-0.385760277856051,
-1.41425266684387));
#56151=CARTESIAN_POINT('Ctrl Pts',(-33.4168310493384,0.0825147174531302,
-1.54198217412836));
#56152=CARTESIAN_POINT('Ctrl Pts',(-33.3903165069327,0.620533359404036,
-1.41402138589117));
#56153=CARTESIAN_POINT('Ctrl Pts',(-33.3638019645271,0.981162324775984,
-1.08914754473287));
#56154=CARTESIAN_POINT('Ctrl Pts',(-33.3372874221214,1.34179129014793,-0.764273703574562));
#56155=CARTESIAN_POINT('Ctrl Pts',(-33.3107728797157,1.52503057894092,-0.242486809495135));
#56156=CARTESIAN_POINT('Ctrl Pts',(-33.28425833731,1.44671103502957,0.236535484996721));
#56157=CARTESIAN_POINT('Ctrl Pts',(-33.2577437949043,1.36839149111822,0.715557779488577));
#56158=CARTESIAN_POINT('Ctrl Pts',(-33.2312292524986,1.02851311450254,1.15181547439287));
#56159=CARTESIAN_POINT('Ctrl Pts',(-33.2047147100929,0.583195617041653,
1.34491808800433));
#56160=CARTESIAN_POINT('Ctrl Pts',(-33.1782001676873,0.137878119580767,
1.5380207016158));
#56161=CARTESIAN_POINT('Ctrl Pts',(-33.1516856252816,-0.412878498725314,
1.48796823393444));
#56162=CARTESIAN_POINT('Ctrl Pts',(-33.1251710828759,-0.816089779884158,
1.21775174235156));
#56163=CARTESIAN_POINT('Ctrl Pts',(-33.0991657371982,-1.21155761739175,
0.95272460502037));
#56164=CARTESIAN_POINT('Ctrl Pts',(-33.0731603915205,-1.46509275032866,
0.475908495121908));
#56165=CARTESIAN_POINT('Ctrl Pts',(-33.0471550458428,-1.46589447233764,
-0.0001750908953165));
#56166=CARTESIAN_POINT('Origin',(-17.3,0.,0.));
#56167=CARTESIAN_POINT('',(-32.4758449541571,-1.46343401324079,0.00135214320468362));
#56168=CARTESIAN_POINT('',(-32.5471550458428,-1.46300356173616,0.00133575934057721));
#56169=CARTESIAN_POINT('',(-17.3,-1.4635,-1.79227059055215E-16));
#56170=CARTESIAN_POINT('Ctrl Pts',(-32.4758449541571,-1.46343401324079,
0.00135214320468362));
#56171=CARTESIAN_POINT('Ctrl Pts',(-32.4821341861468,-1.46449987346685,
0.116994707761757));
#56172=CARTESIAN_POINT('Ctrl Pts',(-32.4884234181365,-1.45195163790634,
0.232408645151303));
#56173=CARTESIAN_POINT('Ctrl Pts',(-32.4947126501262,-1.42490895575888,
0.344320092666205));
#56174=CARTESIAN_POINT('Ctrl Pts',(-32.5212271925319,-1.31090070423688,
0.816123458430666));
#56175=CARTESIAN_POINT('Ctrl Pts',(-32.5477417349376,-0.939275356078788,
1.22567530827207));
#56176=CARTESIAN_POINT('Ctrl Pts',(-32.5742562773433,-0.480735248577563,
1.38485215067918));
#56177=CARTESIAN_POINT('Ctrl Pts',(-32.6007708197489,-0.0221951410763392,
1.54402899308628));
#56178=CARTESIAN_POINT('Ctrl Pts',(-32.6272853621546,0.523259725768014,
1.45283082805909));
#56179=CARTESIAN_POINT('Ctrl Pts',(-32.6537999045603,0.905080187032809,
1.15314860853539));
#56180=CARTESIAN_POINT('Ctrl Pts',(-32.680314446966,1.2869006482976,0.853466389011679));
#56181=CARTESIAN_POINT('Ctrl Pts',(-32.7068289893717,1.50508670398284,0.345300114991455));
#56182=CARTESIAN_POINT('Ctrl Pts',(-32.7333435317774,1.45941680067057,-0.13792918600512));
#56183=CARTESIAN_POINT('Ctrl Pts',(-32.7598580741831,1.41374689735831,-0.621158487001693));
#56184=CARTESIAN_POINT('Ctrl Pts',(-32.7863726165887,1.10422103504854,-1.07945081497461));
#56185=CARTESIAN_POINT('Ctrl Pts',(-32.8128871589944,0.673016781644122,
-1.30229423339842));
#56186=CARTESIAN_POINT('Ctrl Pts',(-32.8394017014001,0.2418125282397,-1.52513765182224));
#56187=CARTESIAN_POINT('Ctrl Pts',(-32.8659162438058,-0.311070116259374,
-1.51253216069693));
#56188=CARTESIAN_POINT('Ctrl Pts',(-32.8924307862115,-0.731670112660202,
-1.27026796542771));
#56189=CARTESIAN_POINT('Ctrl Pts',(-32.9189453286172,-1.15227010906103,
-1.02800377015849));
#56190=CARTESIAN_POINT('Ctrl Pts',(-32.9454598710229,-1.44058745736361,
-0.55608087074537));
#56191=CARTESIAN_POINT('Ctrl Pts',(-32.9719744134285,-1.46418650544209,
-0.071272266589932));
#56192=CARTESIAN_POINT('Ctrl Pts',(-32.9732645936714,-1.46533481964322,
-0.0476817978927391));
#56193=CARTESIAN_POINT('Ctrl Pts',(-32.9745547739142,-1.465856351915,-0.0240608193030587));
#56194=CARTESIAN_POINT('Ctrl Pts',(-32.9758449541571,-1.46576386267191,
-0.000435669595795773));
#56195=CARTESIAN_POINT('Ctrl Pts',(-33.0471550458428,-1.46589447233764,
-0.0001750908953165));
#56196=CARTESIAN_POINT('Ctrl Pts',(-33.0466458491148,-1.46591017042636,
-0.00949702828685));
#56197=CARTESIAN_POINT('Ctrl Pts',(-33.0461366523868,-1.46582897190017,
-0.0188186848327125));
#56198=CARTESIAN_POINT('Ctrl Pts',(-33.0456274556588,-1.46565004497337,
-0.0281384651248314));
#56199=CARTESIAN_POINT('Ctrl Pts',(-33.0191129132531,-1.45633308489213,
-0.513431665533941));
#56200=CARTESIAN_POINT('Ctrl Pts',(-32.9925983708474,-1.18203322071805,
-0.993637550867758));
#56201=CARTESIAN_POINT('Ctrl Pts',(-32.9660838284418,-0.768747318591459,
-1.24817842464081));
#56202=CARTESIAN_POINT('Ctrl Pts',(-32.9395692860361,-0.35546141646487,
-1.50271929841385));
#56203=CARTESIAN_POINT('Ctrl Pts',(-32.9130547436304,0.196810523614232,
-1.53159516062613));
#56204=CARTESIAN_POINT('Ctrl Pts',(-32.8865402012247,0.634387985068444,
-1.32154217130706));
#56205=CARTESIAN_POINT('Ctrl Pts',(-32.860025658819,1.07196544652266,-1.11148918198798));
#56206=CARTESIAN_POINT('Ctrl Pts',(-32.8335111164133,1.39484842935199,-0.662507341137544));
#56207=CARTESIAN_POINT('Ctrl Pts',(-32.8069965740076,1.45472390680499,-0.180831909756413));
#56208=CARTESIAN_POINT('Ctrl Pts',(-32.780482031602,1.51459938425799,0.300843521624713));
#56209=CARTESIAN_POINT('Ctrl Pts',(-32.7539674891963,1.31146735633467,0.815212543536533));
#56210=CARTESIAN_POINT('Ctrl Pts',(-32.7274529467906,0.938634461852072,
1.12600496032996));
#56211=CARTESIAN_POINT('Ctrl Pts',(-32.7009384043849,0.565801567369472,
1.4367973771234));
#56212=CARTESIAN_POINT('Ctrl Pts',(-32.6744238619792,0.0232678063275967,
1.54401318879844));
#56213=CARTESIAN_POINT('Ctrl Pts',(-32.6479093195735,-0.439759436949033,
1.39840389810825));
#56214=CARTESIAN_POINT('Ctrl Pts',(-32.6213947771678,-0.902786680225661,
1.25279460741805));
#56215=CARTESIAN_POINT('Ctrl Pts',(-32.5948802347622,-1.28630740573704,
0.854360214362621));
#56216=CARTESIAN_POINT('Ctrl Pts',(-32.5683656923565,-1.41415525502841,
0.38611751970031));
#56217=CARTESIAN_POINT('Ctrl Pts',(-32.5612954768519,-1.44824642780646,
0.261258613631341));
#56218=CARTESIAN_POINT('Ctrl Pts',(-32.5542252613474,-1.46415811092022,
0.131436023825928));
#56219=CARTESIAN_POINT('Ctrl Pts',(-32.5471550458428,-1.46300356173616,
0.00133575934057721));
#56220=CARTESIAN_POINT('Origin',(-17.3,0.,0.));
#56221=CARTESIAN_POINT('',(-31.9758449541571,-1.4610973901521,-0.000186288173925353));
#56222=CARTESIAN_POINT('',(-32.0471550458428,-1.46118615381657,-0.000418794261562428));
#56223=CARTESIAN_POINT('',(-17.3,-1.4635,-1.79227059055215E-16));
#56224=CARTESIAN_POINT('Ctrl Pts',(-31.9758449541571,-1.4610973901521,-0.000186288173925353));
#56225=CARTESIAN_POINT('Ctrl Pts',(-31.9897135983793,-1.46080759427907,
0.25585153086225));
#56226=CARTESIAN_POINT('Ctrl Pts',(-32.0035822426016,-1.39685690896212,
0.512024759540195));
#56227=CARTESIAN_POINT('Ctrl Pts',(-32.0174508868239,-1.27008311131556,
0.731990948556328));
#56228=CARTESIAN_POINT('Ctrl Pts',(-32.0439654292295,-1.02771268348116,
1.15252973756993));
#56229=CARTESIAN_POINT('Ctrl Pts',(-32.0704799716352,-0.555716971662109,
1.44072787270177));
#56230=CARTESIAN_POINT('Ctrl Pts',(-32.0969945140409,-0.0709024224430543,
1.4642044614433));
#56231=CARTESIAN_POINT('Ctrl Pts',(-32.1235090564466,0.413912126776,1.48768105018482));
#56232=CARTESIAN_POINT('Ctrl Pts',(-32.1500235988523,0.91154551339507,1.24643609253604));
#56233=CARTESIAN_POINT('Ctrl Pts',(-32.176538141258,1.19341488474662,0.851283014796641));
#56234=CARTESIAN_POINT('Ctrl Pts',(-32.2030526836637,1.47528425609817,0.45612993705724));
#56235=CARTESIAN_POINT('Ctrl Pts',(-32.2295672260693,1.54138961218219,-0.0929312607727704));
#56236=CARTESIAN_POINT('Ctrl Pts',(-32.256081768475,1.3613661276533,-0.543694882167351));
#56237=CARTESIAN_POINT('Ctrl Pts',(-32.2825963108807,1.18134264312441,-0.994458503561922));
#56238=CARTESIAN_POINT('Ctrl Pts',(-32.3091108532864,0.755190317982634,
-1.34692454852107));
#56239=CARTESIAN_POINT('Ctrl Pts',(-32.3356253956921,0.278657903762824,
-1.43919131149949));
#56240=CARTESIAN_POINT('Ctrl Pts',(-32.3621399380978,-0.19787451045699,
-1.53145807447791));
#56241=CARTESIAN_POINT('Ctrl Pts',(-32.3886544805034,-0.724787013754835,
-1.3635255554756));
#56242=CARTESIAN_POINT('Ctrl Pts',(-32.4151690229091,-1.06004768796081,
-1.01253185513069));
#56243=CARTESIAN_POINT('Ctrl Pts',(-32.4353943333251,-1.31578475112933,
-0.744793629257785));
#56244=CARTESIAN_POINT('Ctrl Pts',(-32.4556196437411,-1.46000635244413,
-0.37053853745336));
#56245=CARTESIAN_POINT('Ctrl Pts',(-32.4758449541571,-1.46343401324079,
0.00135214320468362));
#56246=CARTESIAN_POINT('Ctrl Pts',(-32.5471550458428,-1.46300356173616,
0.00133575934057721));
#56247=CARTESIAN_POINT('Ctrl Pts',(-32.5277107189417,-1.45982834992771,
-0.356462679893697));
#56248=CARTESIAN_POINT('Ctrl Pts',(-32.5082663920405,-1.32757336974612,
-0.716361300512106));
#56249=CARTESIAN_POINT('Ctrl Pts',(-32.4888220651394,-1.0893953049412,-0.980887197291753));
#56250=CARTESIAN_POINT('Ctrl Pts',(-32.4623075227337,-0.764612532491269,
-1.34159822335231));
#56251=CARTESIAN_POINT('Ctrl Pts',(-32.4357929803281,-0.24287201452005,
-1.52496927920423));
#56252=CARTESIAN_POINT('Ctrl Pts',(-32.4092784379224,0.236170029881672,
-1.44677072867951));
#56253=CARTESIAN_POINT('Ctrl Pts',(-32.3827638955167,0.715212074283389,
-1.36857217815479));
#56254=CARTESIAN_POINT('Ctrl Pts',(-32.356249353111,1.15155564511561,-1.02880402125342));
#56255=CARTESIAN_POINT('Ctrl Pts',(-32.3297348107053,1.34477074540355,-0.583535317384259));
#56256=CARTESIAN_POINT('Ctrl Pts',(-32.3032202682996,1.53798584569149,-0.138266613515089));
#56257=CARTESIAN_POINT('Ctrl Pts',(-32.2767057258939,1.48807247543514,0.412502637321881));
#56258=CARTESIAN_POINT('Ctrl Pts',(-32.2501911834882,1.21795783540472,0.81578216178961));
#56259=CARTESIAN_POINT('Ctrl Pts',(-32.2236766410825,0.947843195374297,
1.21906168625734));
#56260=CARTESIAN_POINT('Ctrl Pts',(-32.1971620986768,0.457527285569812,
1.47485148435582));
#56261=CARTESIAN_POINT('Ctrl Pts',(-32.1706475562712,-0.0277682501593372,
1.46565710472151));
#56262=CARTESIAN_POINT('Ctrl Pts',(-32.1441330138655,-0.513063785888485,
1.4564627250872));
#56263=CARTESIAN_POINT('Ctrl Pts',(-32.1176184714598,-0.993338947542297,
1.1822841677201));
#56264=CARTESIAN_POINT('Ctrl Pts',(-32.0911039290541,-1.24798420716327,
0.76906257417729));
#56265=CARTESIAN_POINT('Ctrl Pts',(-32.076454301317,-1.38867900782723,0.54075229728431));
#56266=CARTESIAN_POINT('Ctrl Pts',(-32.0618046735799,-1.46049564483494,
0.269996276654853));
#56267=CARTESIAN_POINT('Ctrl Pts',(-32.0471550458428,-1.46118615381657,
-0.000418794261562428));
#56268=CARTESIAN_POINT('Origin',(-17.3,0.,0.));
#56269=CARTESIAN_POINT('',(-31.4758449541571,-1.46411995320351,-0.00128603361858132));
#56270=CARTESIAN_POINT('',(-31.5471550458428,-1.46454451199446,-0.00118531342847866));
#56271=CARTESIAN_POINT('',(-17.3,-1.4635,-1.79227059055215E-16));
#56272=CARTESIAN_POINT('Ctrl Pts',(-31.4758449541571,-1.46411995320351,
-0.00128603361858132));
#56273=CARTESIAN_POINT('Ctrl Pts',(-31.4972930106119,-1.4604966735953,0.392614030616494));
#56274=CARTESIAN_POINT('Ctrl Pts',(-31.5187410670667,-1.2962572267619,0.789177174870507));
#56275=CARTESIAN_POINT('Ctrl Pts',(-31.5401891235215,-1.01226406354304,
1.06030341132948));
#56276=CARTESIAN_POINT('Ctrl Pts',(-31.5667036659272,-0.661185690313245,
1.3954754167294));
#56277=CARTESIAN_POINT('Ctrl Pts',(-31.5932182083329,-0.127094551235654,
1.53894935940639));
#56278=CARTESIAN_POINT('Ctrl Pts',(-31.6197327507385,0.344680001926412,
1.42482193788896));
#56279=CARTESIAN_POINT('Ctrl Pts',(-31.6462472931442,0.816454555088478,
1.31069451637152));
#56280=CARTESIAN_POINT('Ctrl Pts',(-31.6727618355499,1.22591252233502,0.938965730659652));
#56281=CARTESIAN_POINT('Ctrl Pts',(-31.6992763779556,1.38497353623587,0.480385431027943));
#56282=CARTESIAN_POINT('Ctrl Pts',(-31.7257909203613,1.54403455013671,0.0218051313962338));
#56283=CARTESIAN_POINT('Ctrl Pts',(-31.752305462767,1.45269861069187,-0.523626682155316));
#56284=CARTESIAN_POINT('Ctrl Pts',(-31.7788200051727,1.15291995600268,-0.905371433980737));
#56285=CARTESIAN_POINT('Ctrl Pts',(-31.8053345475784,0.853141301313501,
-1.28711618580616));
#56286=CARTESIAN_POINT('Ctrl Pts',(-31.831849089984,0.344919931379984,-1.50517387590545));
#56287=CARTESIAN_POINT('Ctrl Pts',(-31.8583636323897,-0.138297818302765,
-1.45938191432897));
#56288=CARTESIAN_POINT('Ctrl Pts',(-31.8848781747954,-0.621515567985517,
-1.41358995275248));
#56289=CARTESIAN_POINT('Ctrl Pts',(-31.9113927172011,-1.0797296974175,-1.10394833950022));
#56290=CARTESIAN_POINT('Ctrl Pts',(-31.9379072596068,-1.30246419020861,
-0.672687811426406));
#56291=CARTESIAN_POINT('Ctrl Pts',(-31.9505531577902,-1.40869561878388,
-0.4670015640414));
#56292=CARTESIAN_POINT('Ctrl Pts',(-31.9631990559737,-1.46136163581632,
-0.233650218660073));
#56293=CARTESIAN_POINT('Ctrl Pts',(-31.9758449541571,-1.4610973901521,-0.000186288173925353));
#56294=CARTESIAN_POINT('Ctrl Pts',(-32.0471550458428,-1.46118615381657,
-0.000418794261562428));
#56295=CARTESIAN_POINT('Ctrl Pts',(-32.0352901311742,-1.46174540557996,
-0.219431304279028));
#56296=CARTESIAN_POINT('Ctrl Pts',(-32.0234252165056,-1.41564890171275,
-0.438220165590512));
#56297=CARTESIAN_POINT('Ctrl Pts',(-32.011560301837,-1.32170236948958,-0.634054154480603));
#56298=CARTESIAN_POINT('Ctrl Pts',(-31.9850457594313,-1.11175991460677,
-1.07168465987714));
#56299=CARTESIAN_POINT('Ctrl Pts',(-31.9585312170257,-0.662859647253007,
-1.3946810409517));
#56300=CARTESIAN_POINT('Ctrl Pts',(-31.93201667462,-0.181199355667255,-1.45467818359834));
#56301=CARTESIAN_POINT('Ctrl Pts',(-31.9055021322143,0.3004609359185,-1.51467532624497));
#56302=CARTESIAN_POINT('Ctrl Pts',(-31.8789875898086,0.814881251736254,
-1.31167323046369));
#56303=CARTESIAN_POINT('Ctrl Pts',(-31.8524730474029,1.1257678333244,-0.938918851542513));
#56304=CARTESIAN_POINT('Ctrl Pts',(-31.8259585049972,1.43665441491254,-0.566164472621339));
#56305=CARTESIAN_POINT('Ctrl Pts',(-31.7994439625915,1.54400726227108,-0.0236578105602783));
#56306=CARTESIAN_POINT('Ctrl Pts',(-31.7729294201859,1.39851493297882,0.439406197686252));
#56307=CARTESIAN_POINT('Ctrl Pts',(-31.7464148777802,1.25302260368656,0.902470205932789));
#56308=CARTESIAN_POINT('Ctrl Pts',(-31.7199003353745,0.854685097743509,
1.28609156036479));
#56309=CARTESIAN_POINT('Ctrl Pts',(-31.6933857929688,0.386474711384964,
1.41405767979603));
#56310=CARTESIAN_POINT('Ctrl Pts',(-31.6668712505631,-0.0817356749735745,
1.54202379922726));
#56311=CARTESIAN_POINT('Ctrl Pts',(-31.6403567081574,-0.619818941747609,
1.41433468365773));
#56312=CARTESIAN_POINT('Ctrl Pts',(-31.6138421657518,-0.980611993776293,
1.08964303420528));
#56313=CARTESIAN_POINT('Ctrl Pts',(-31.5916131257821,-1.28309065064331,
0.817430768835746));
#56314=CARTESIAN_POINT('Ctrl Pts',(-31.5693840858125,-1.46095786977572,
0.406751927520254));
#56315=CARTESIAN_POINT('Ctrl Pts',(-31.5471550458428,-1.46454451199446,
-0.00118531342847866));
#56316=CARTESIAN_POINT('Origin',(-17.3,0.,0.));
#56317=CARTESIAN_POINT('',(-30.9758449541571,-1.46537689164811,0.00080145734256621));
#56318=CARTESIAN_POINT('',(-31.0471550458428,-1.46504041338933,0.000995257504430862));
#56319=CARTESIAN_POINT('',(-17.3,-1.4635,-1.79227059055215E-16));
#56320=CARTESIAN_POINT('Ctrl Pts',(-30.9758449541571,-1.46537689164811,
0.00080145734256621));
#56321=CARTESIAN_POINT('Ctrl Pts',(-30.9783578804388,-1.46568003330817,
0.0468491384676566));
#56322=CARTESIAN_POINT('Ctrl Pts',(-30.9808708067204,-1.4636984540663,0.092870385363776));
#56323=CARTESIAN_POINT('Ctrl Pts',(-30.9833837330021,-1.45934693488595,
0.138666441710288));
#56324=CARTESIAN_POINT('Ctrl Pts',(-31.0098982754078,-1.41343291795737,
0.621872609306444));
#56325=CARTESIAN_POINT('Ctrl Pts',(-31.0364128178134,-1.10367557347831,
1.08000851120647));
#56326=CARTESIAN_POINT('Ctrl Pts',(-31.0629273602191,-0.672358798268734,
1.30263406404417));
#56327=CARTESIAN_POINT('Ctrl Pts',(-31.0894419026248,-0.241042023059151,
1.52525961688188));
#56328=CARTESIAN_POINT('Ctrl Pts',(-31.1159564450305,0.311834182880956,
1.51237482065725));
#56329=CARTESIAN_POINT('Ctrl Pts',(-31.1424709874362,0.732311737710161,
1.26989817592968));
#56330=CARTESIAN_POINT('Ctrl Pts',(-31.1689855298419,1.15278929253936,1.02742153120211));
#56331=CARTESIAN_POINT('Ctrl Pts',(-31.1955000722476,1.44086819625767,0.555353037971591));
#56332=CARTESIAN_POINT('Ctrl Pts',(-31.2220146146532,1.46422232409926,0.070532574226254));
#56333=CARTESIAN_POINT('Ctrl Pts',(-31.2485291570589,1.48757645194085,-0.414287889519083));
#56334=CARTESIAN_POINT('Ctrl Pts',(-31.2750436994646,1.24620580390573,-0.911860323779238));
#56335=CARTESIAN_POINT('Ctrl Pts',(-31.3015582418703,0.850981540896159,
-1.19362987373457));
#56336=CARTESIAN_POINT('Ctrl Pts',(-31.328072784276,0.455757277886592,-1.4753994236899));
#56337=CARTESIAN_POINT('Ctrl Pts',(-31.3545873266817,-0.0933206000974209,
-1.54136608934041));
#56338=CARTESIAN_POINT('Ctrl Pts',(-31.3811018690874,-0.544038734665332,
-1.36122875138654));
#56339=CARTESIAN_POINT('Ctrl Pts',(-31.407616411493,-0.994756869233242,
-1.18109141343267));
#56340=CARTESIAN_POINT('Ctrl Pts',(-31.4341309538987,-1.34711526038505,
-0.754850071874408));
#56341=CARTESIAN_POINT('Ctrl Pts',(-31.4606454963044,-1.43926165226995,
-0.278294367033853));
#56342=CARTESIAN_POINT('Ctrl Pts',(-31.4657119822553,-1.45686928783713,
-0.187232535890486));
#56343=CARTESIAN_POINT('Ctrl Pts',(-31.4707784682062,-1.46497584871413,
-0.0943335853026628));
#56344=CARTESIAN_POINT('Ctrl Pts',(-31.4758449541571,-1.46411995320351,
-0.00128603361858132));
#56345=CARTESIAN_POINT('Ctrl Pts',(-31.5471550458428,-1.46454451199446,
-0.00118531342847866));
#56346=CARTESIAN_POINT('Ctrl Pts',(-31.5428695434068,-1.46523597523294,
-0.0798309068605571));
#56347=CARTESIAN_POINT('Ctrl Pts',(-31.5385840409707,-1.45944988408569,
-0.15837460215921));
#56348=CARTESIAN_POINT('Ctrl Pts',(-31.5342985385347,-1.44683033710717,
-0.23580458001566));
#56349=CARTESIAN_POINT('Ctrl Pts',(-31.507783996129,-1.36875279112603,-0.714866361448761));
#56350=CARTESIAN_POINT('Ctrl Pts',(-31.4812694537233,-1.02909486188039,
-1.15129574097958));
#56351=CARTESIAN_POINT('Ctrl Pts',(-31.4547549113176,-0.583874976762647,
-1.34462330629827));
#56352=CARTESIAN_POINT('Ctrl Pts',(-31.4282403689119,-0.1386550916449,-1.53795087161695));
#56353=CARTESIAN_POINT('Ctrl Pts',(-31.4017258265063,0.41212674934496,-1.48817662272349));
#56354=CARTESIAN_POINT('Ctrl Pts',(-31.3752112841006,0.815474489679166,
-1.21816385638901));
#56355=CARTESIAN_POINT('Ctrl Pts',(-31.3486967416949,1.21882223001337,-0.948151090054522));
#56356=CARTESIAN_POINT('Ctrl Pts',(-31.3221821992892,1.47473586969192,-0.457899806279018));
#56357=CARTESIAN_POINT('Ctrl Pts',(-31.2956676568835,1.46566407199324,0.0273980363937246));
#56358=CARTESIAN_POINT('Ctrl Pts',(-31.2691531144778,1.45659227429456,0.512695879066464));
#56359=CARTESIAN_POINT('Ctrl Pts',(-31.2426385720721,1.18253503921864,0.993040280636447));
#56360=CARTESIAN_POINT('Ctrl Pts',(-31.2161240296665,0.769377780148935,
1.24778990849547));
#56361=CARTESIAN_POINT('Ctrl Pts',(-31.1896094872608,0.356220521079224,
1.5025395363545));
#56362=CARTESIAN_POINT('Ctrl Pts',(-31.1630949448551,-0.19603676198427,
1.53169439050258));
#56363=CARTESIAN_POINT('Ctrl Pts',(-31.1365804024494,-0.633720283150774,
1.32186248416896));
#56364=CARTESIAN_POINT('Ctrl Pts',(-31.1100658600437,-1.07140380431728,
1.11203057783535));
#56365=CARTESIAN_POINT('Ctrl Pts',(-31.083551317638,-1.39451356358678,0.663211911020028));
#56366=CARTESIAN_POINT('Ctrl Pts',(-31.0570367752323,-1.45463236773102,
0.181566789582494));
#56367=CARTESIAN_POINT('Ctrl Pts',(-31.0537428654358,-1.4621009453476,0.121731867309701));
#56368=CARTESIAN_POINT('Ctrl Pts',(-31.0504489556393,-1.46551073892982,
0.0613903287927805));
#56369=CARTESIAN_POINT('Ctrl Pts',(-31.0471550458428,-1.46504041338933,
0.000995257504430862));
#56370=CARTESIAN_POINT('Origin',(-17.3,0.,0.));
#56371=CARTESIAN_POINT('',(-30.4758449541571,-1.46163047894353,0.000888967245564962));
#56372=CARTESIAN_POINT('',(-30.5471550458428,-1.46139501350857,0.000694879315414263));
#56373=CARTESIAN_POINT('',(-17.3,-1.4635,-1.79227059055215E-16));
#56374=CARTESIAN_POINT('Ctrl Pts',(-30.4758449541571,-1.46163047894353,
0.000888967245564962));
#56375=CARTESIAN_POINT('Ctrl Pts',(-30.4859372926713,-1.46265825863814,
0.187040242740951));
#56376=CARTESIAN_POINT('Ctrl Pts',(-30.4960296311855,-1.42970103069593,
0.372841193739307));
#56377=CARTESIAN_POINT('Ctrl Pts',(-30.5061219696997,-1.36109128827009,
0.544382552450832));
#56378=CARTESIAN_POINT('Ctrl Pts',(-30.5326365121054,-1.18084010838424,
0.995055171436328));
#56379=CARTESIAN_POINT('Ctrl Pts',(-30.5591510545111,-0.754509777603949,
1.34730588630464));
#56380=CARTESIAN_POINT('Ctrl Pts',(-30.5856655969168,-0.277930812548528,
1.43933190121449));
#56381=CARTESIAN_POINT('Ctrl Pts',(-30.6121801393225,0.198648152506894,
1.53135791612434));
#56382=CARTESIAN_POINT('Ctrl Pts',(-30.6386946817282,0.725475751837446,
1.36315923107573));
#56383=CARTESIAN_POINT('Ctrl Pts',(-30.6652092241338,1.06055906704721,1.01199620736521));
#56384=CARTESIAN_POINT('Ctrl Pts',(-30.6917237665395,1.39564238225697,0.66083318365468));
#56385=CARTESIAN_POINT('Ctrl Pts',(-30.7182383089452,1.53898141334595,0.126705821282239));
#56386=CARTESIAN_POINT('Ctrl Pts',(-30.7447528513509,1.4247348291133,-0.345039889185446));
#56387=CARTESIAN_POINT('Ctrl Pts',(-30.7712673937566,1.31048824488065,-0.816785599653127));
#56388=CARTESIAN_POINT('Ctrl Pts',(-30.7977819361623,0.938656045326382,
-1.22614965821605));
#56389=CARTESIAN_POINT('Ctrl Pts',(-30.824296478568,0.480035582825442,-1.38509483344609));
#56390=CARTESIAN_POINT('Ctrl Pts',(-30.8508110209736,0.0214151203245024,
-1.54404000867613));
#56391=CARTESIAN_POINT('Ctrl Pts',(-30.8773255633793,-0.523993605123111,
-1.45256630057329));
#56392=CARTESIAN_POINT('Ctrl Pts',(-30.903840105785,-0.905662623157868,
-1.15269122987573));
#56393=CARTESIAN_POINT('Ctrl Pts',(-30.927841721909,-1.25115880850179,-0.881236938041353));
#56394=CARTESIAN_POINT('Ctrl Pts',(-30.9518433380331,-1.46248150637196,
-0.439011987974939));
#56395=CARTESIAN_POINT('Ctrl Pts',(-30.9758449541571,-1.46537689164811,
0.00080145734256621));
#56396=CARTESIAN_POINT('Ctrl Pts',(-31.0471550458428,-1.46504041338933,
0.000995257504430862));
#56397=CARTESIAN_POINT('Ctrl Pts',(-31.0239344132336,-1.46172482272134,
-0.424763748792314));
#56398=CARTESIAN_POINT('Ctrl Pts',(-31.0007137806245,-1.26558138617169,
-0.853183139647398));
#56399=CARTESIAN_POINT('Ctrl Pts',(-30.9774931480153,-0.939203181247643,
-1.12553063426295));
#56400=CARTESIAN_POINT('Ctrl Pts',(-30.9509786056096,-0.566527341601074,
-1.4365113606111));
#56401=CARTESIAN_POINT('Ctrl Pts',(-30.9244640632039,-0.024047813288972,
-1.54400123724768));
#56402=CARTESIAN_POINT('Ctrl Pts',(-30.8979495207982,0.439052930346154,
-1.39862587874117));
#56403=CARTESIAN_POINT('Ctrl Pts',(-30.8714349783925,0.902153673981284,
-1.25325052023465));
#56404=CARTESIAN_POINT('Ctrl Pts',(-30.8449204359868,1.28587563293943,-0.855009926585044));
#56405=CARTESIAN_POINT('Ctrl Pts',(-30.8184058935812,1.41396001436526,-0.386831878347976));
#56406=CARTESIAN_POINT('Ctrl Pts',(-30.7918913511755,1.5420443957911,0.0813461698890949));
#56407=CARTESIAN_POINT('Ctrl Pts',(-30.7653768087698,1.4144911996846,0.619461672713624));
#56408=CARTESIAN_POINT('Ctrl Pts',(-30.7388622663641,1.08989069393563,0.980336727661757));
#56409=CARTESIAN_POINT('Ctrl Pts',(-30.7123477239584,0.765290188186653,
1.34121178260988));
#56410=CARTESIAN_POINT('Ctrl Pts',(-30.6858331815527,0.243642372795188,
1.52484638968162));
#56411=CARTESIAN_POINT('Ctrl Pts',(-30.659318639147,-0.235439115098553,
1.44688985324096));
#56412=CARTESIAN_POINT('Ctrl Pts',(-30.6328040967413,-0.714520602992297,
1.3689333168003));
#56413=CARTESIAN_POINT('Ctrl Pts',(-30.6062895543357,-1.15103576338832,
1.02938563684725));
#56414=CARTESIAN_POINT('Ctrl Pts',(-30.57977501193,-1.34447578140578,0.584214598879012));
#56415=CARTESIAN_POINT('Ctrl Pts',(-30.5689016899009,-1.42380340384888,
0.40165485563416));
#56416=CARTESIAN_POINT('Ctrl Pts',(-30.5580283678719,-1.46225235444837,
0.201332117172804));
#56417=CARTESIAN_POINT('Ctrl Pts',(-30.5471550458428,-1.46139501350857,
0.000694879315414263));
#56418=CARTESIAN_POINT('Origin',(-17.3,0.,0.));
#56419=CARTESIAN_POINT('',(-29.9758449541571,-1.46212182688944,-0.00114026912922158));
#56420=CARTESIAN_POINT('',(-30.0471550458428,-1.46248873579703,-0.0012520286611161));
#56421=CARTESIAN_POINT('',(-17.3,-1.4635,-1.79227059055215E-16));
#56422=CARTESIAN_POINT('Ctrl Pts',(-29.9758449541571,-1.46212182688944,
-0.00114026912922158));
#56423=CARTESIAN_POINT('Ctrl Pts',(-29.9935167049038,-1.45976391963976,
0.324536834983454));
#56424=CARTESIAN_POINT('Ctrl Pts',(-30.0111884556506,-1.35239124379562,
0.651624606709122));
#56425=CARTESIAN_POINT('Ctrl Pts',(-30.0288602063974,-1.15246243020409,
0.90595375455135));
#56426=CARTESIAN_POINT('Ctrl Pts',(-30.055374748803,-0.852490962630948,
1.287547014444));
#56427=CARTESIAN_POINT('Ctrl Pts',(-30.0818892912087,-0.344159498409212,
1.50534793168417));
#56428=CARTESIAN_POINT('Ctrl Pts',(-30.1084038336144,0.139035056270542,
1.45931186233288));
#56429=CARTESIAN_POINT('Ctrl Pts',(-30.1349183760201,0.6222296109503,1.41327579298159));
#56430=CARTESIAN_POINT('Ctrl Pts',(-30.1614329184258,1.08028725608808,1.10340273703883));
#56431=CARTESIAN_POINT('Ctrl Pts',(-30.1879474608315,1.3028038547683,0.672029742212693));
#56432=CARTESIAN_POINT('Ctrl Pts',(-30.2144620032372,1.52532045344853,0.240656747386556));
#56433=CARTESIAN_POINT('Ctrl Pts',(-30.2409765456428,1.51229600567119,-0.312216186322958));
#56434=CARTESIAN_POINT('Ctrl Pts',(-30.2674910880485,1.26971315952106,-0.732632480140392));
#56435=CARTESIAN_POINT('Ctrl Pts',(-30.2940056304542,1.02713031337092,-1.15304877395783));
#56436=CARTESIAN_POINT('Ctrl Pts',(-30.3205201728599,0.55498906884799,-1.44100842788317));
#56437=CARTESIAN_POINT('Ctrl Pts',(-30.3470347152656,0.0701627215092274,
-1.46424009333443));
#56438=CARTESIAN_POINT('Ctrl Pts',(-30.3735492576713,-0.414663625829532,
-1.48747175878569));
#56439=CARTESIAN_POINT('Ctrl Pts',(-30.400063800077,-0.912175075984127,
-1.24597543576286));
#56440=CARTESIAN_POINT('Ctrl Pts',(-30.4265783424827,-1.19384478656572,
-0.850680012700103));
#56441=CARTESIAN_POINT('Ctrl Pts',(-30.4430005463741,-1.36830140536949,
-0.60584750020262));
#56442=CARTESIAN_POINT('Ctrl Pts',(-30.4594227502656,-1.45995808084902,
-0.302015478194993));
#56443=CARTESIAN_POINT('Ctrl Pts',(-30.4758449541571,-1.46163047894353,
0.000888967245564962));
#56444=CARTESIAN_POINT('Ctrl Pts',(-30.5471550458428,-1.46139501350857,
0.000694879315414263));
#56445=CARTESIAN_POINT('Ctrl Pts',(-30.5315138254662,-1.46016173277417,
-0.28792080269058));
#56446=CARTESIAN_POINT('Ctrl Pts',(-30.5158726050895,-1.37759319561782,
-0.577187268273936));
#56447=CARTESIAN_POINT('Ctrl Pts',(-30.5002313847129,-1.21836979964959,
-0.815166765534423));
#56448=CARTESIAN_POINT('Ctrl Pts',(-30.4737168423072,-0.948458924237074,
-1.21858269599621));
#56449=CARTESIAN_POINT('Ctrl Pts',(-30.4472022999015,-0.458272297773157,
-1.47462016093639));
#56450=CARTESIAN_POINT('Ctrl Pts',(-30.4206877574959,0.0270278208791361,
-1.46567094575439));
#56451=CARTESIAN_POINT('Ctrl Pts',(-30.3941732150902,0.512327939531434,
-1.45672173057239));
#56452=CARTESIAN_POINT('Ctrl Pts',(-30.3676586726845,0.992741550372114,
-1.18278583526821));
#56453=CARTESIAN_POINT('Ctrl Pts',(-30.3411441302788,1.24759553021592,-0.769692937030927));
#56454=CARTESIAN_POINT('Ctrl Pts',(-30.3146295878731,1.50244951005973,-0.356600038793641));
#56455=CARTESIAN_POINT('Ctrl Pts',(-30.2881150454674,1.53174385890668,0.195649862376755));
#56456=CARTESIAN_POINT('Ctrl Pts',(-30.2616005030617,1.32202251450984,0.633386371387252));
#56457=CARTESIAN_POINT('Ctrl Pts',(-30.2350859606561,1.11230117011302,1.07112288039774));
#56458=CARTESIAN_POINT('Ctrl Pts',(-30.2085714182504,0.663564132472433,
1.39434599724833));
#56459=CARTESIAN_POINT('Ctrl Pts',(-30.1820568758447,0.181934211913454,
1.45458645905476));
#56460=CARTESIAN_POINT('Ctrl Pts',(-30.155542333439,-0.29969570864554,1.51482692086119));
#56461=CARTESIAN_POINT('Ctrl Pts',(-30.1290277910333,-0.814218512122926,
1.31208472762344));
#56462=CARTESIAN_POINT('Ctrl Pts',(-30.1025132486276,-1.12529336338979,
0.93948745102898));
#56463=CARTESIAN_POINT('Ctrl Pts',(-30.084060514366,-1.34178518429572,0.680179240975944));
#56464=CARTESIAN_POINT('Ctrl Pts',(-30.0656077801044,-1.45973837855422,
0.338602880955323));
#56465=CARTESIAN_POINT('Ctrl Pts',(-30.0471550458428,-1.46248873579703,
-0.0012520286611161));
#56466=CARTESIAN_POINT('Origin',(-17.3,0.,0.));
#56467=CARTESIAN_POINT('',(-29.4758449541571,-1.4657700110061,-0.000426988761815655));
#56468=CARTESIAN_POINT('',(-29.5471550458428,-1.46589706054516,-0.000165931013407645));
#56469=CARTESIAN_POINT('',(-17.3,-1.4635,-1.79227059055215E-16));
#56470=CARTESIAN_POINT('Ctrl Pts',(-29.4758449541571,-1.4657700110061,-0.000426988761815655));
#56471=CARTESIAN_POINT('Ctrl Pts',(-29.5010961171364,-1.46399203858896,
0.461954784892472));
#56472=CARTESIAN_POINT('Ctrl Pts',(-29.5263472801157,-1.22690634601226,
0.925906164443394));
#56473=CARTESIAN_POINT('Ctrl Pts',(-29.551598443095,-0.850378430228461,
1.19405962322649));
#56474=CARTESIAN_POINT('Ctrl Pts',(-29.5781129855007,-0.455011872333391,
1.4756294764631));
#56475=CARTESIAN_POINT('Ctrl Pts',(-29.6046275279064,0.0940992608542971,
1.54131874862981));
#56476=CARTESIAN_POINT('Ctrl Pts',(-29.631142070312,0.544726335503297,1.3609537383125));
#56477=CARTESIAN_POINT('Ctrl Pts',(-29.6576566127177,0.99535341015231,1.18058872799518));
#56478=CARTESIAN_POINT('Ctrl Pts',(-29.6841711551234,1.34749642626262,0.754169435193818));
#56479=CARTESIAN_POINT('Ctrl Pts',(-29.7106856975291,1.43940205832593,0.277567240330494));
#56480=CARTESIAN_POINT('Ctrl Pts',(-29.7372002399348,1.53130769038923,-0.199034954532819));
#56481=CARTESIAN_POINT('Ctrl Pts',(-29.7637147823405,1.36297593840554,-0.725820051458098));
#56482=CARTESIAN_POINT('Ctrl Pts',(-29.7902293247462,1.0117282866194,-1.06081465509852));
#56483=CARTESIAN_POINT('Ctrl Pts',(-29.8167438671519,0.66048063483325,-1.39580925873894));
#56484=CARTESIAN_POINT('Ctrl Pts',(-29.8432584095575,0.126317083244657,
-1.53901336909452));
#56485=CARTESIAN_POINT('Ctrl Pts',(-29.8697729519632,-0.345399754430043,
-1.42464762943588));
#56486=CARTESIAN_POINT('Ctrl Pts',(-29.8962874943689,-0.817116592104736,
-1.31028188977725));
#56487=CARTESIAN_POINT('Ctrl Pts',(-29.9228020367746,-1.22638671586554,
-0.938346300104411));
#56488=CARTESIAN_POINT('Ctrl Pts',(-29.9493165791803,-1.38521604228366,
-0.479685703995432));
#56489=CARTESIAN_POINT('Ctrl Pts',(-29.9581593708392,-1.43818677137845,
-0.326719077926747));
#56490=CARTESIAN_POINT('Ctrl Pts',(-29.9670021624982,-1.46330170334077,
-0.16410628313783));
#56491=CARTESIAN_POINT('Ctrl Pts',(-29.9758449541571,-1.46212182688944,
-0.00114026912922158));
#56492=CARTESIAN_POINT('Ctrl Pts',(-30.0471550458428,-1.46248873579703,
-0.0012520286611161));
#56493=CARTESIAN_POINT('Ctrl Pts',(-30.0390932376987,-1.4636903383403,-0.149731112536215));
#56494=CARTESIAN_POINT('Ctrl Pts',(-30.0310314295547,-1.44290288229849,
-0.297881618793177));
#56495=CARTESIAN_POINT('Ctrl Pts',(-30.0229696214106,-1.39873673526752,
-0.438699634993247));
#56496=CARTESIAN_POINT('Ctrl Pts',(-29.9964550790049,-1.25347835682203,
-0.901837084469851));
#56497=CARTESIAN_POINT('Ctrl Pts',(-29.9699405365992,-0.855334700874716,
-1.2856596234719));
#56498=CARTESIAN_POINT('Ctrl Pts',(-29.9434259941935,-0.387189020630112,
-1.41386225872025));
#56499=CARTESIAN_POINT('Ctrl Pts',(-29.9169114517878,0.0809566596144957,
-1.54206489396861));
#56500=CARTESIAN_POINT('Ctrl Pts',(-29.8903969093821,0.619104364156387,
-1.41464762546327));
#56501=CARTESIAN_POINT('Ctrl Pts',(-29.8638823669764,0.980061398999209,
-1.0901382841281));
#56502=CARTESIAN_POINT('Ctrl Pts',(-29.8373678245708,1.34101843384203,-0.765628942792929));
#56503=CARTESIAN_POINT('Ctrl Pts',(-29.8108532821651,1.52478479898578,-0.244027528627926));
#56504=CARTESIAN_POINT('Ctrl Pts',(-29.7843387397594,1.44694927705943,0.235073635159805));
#56505=CARTESIAN_POINT('Ctrl Pts',(-29.7578241973537,1.36911375513308,0.714174798947536));
#56506=CARTESIAN_POINT('Ctrl Pts',(-29.731309654948,1.02967634613663,1.150775712358));
#56507=CARTESIAN_POINT('Ctrl Pts',(-29.7047951125423,0.584554183720977,
1.34432817073226));
#56508=CARTESIAN_POINT('Ctrl Pts',(-29.6782805701366,0.139432021305321,
1.53788062910652));
#56509=CARTESIAN_POINT('Ctrl Pts',(-29.6517660277309,-0.411374894529538,
1.48838463244457));
#56510=CARTESIAN_POINT('Ctrl Pts',(-29.6252514853253,-0.814858989379939,
1.21857566517502));
#56511=CARTESIAN_POINT('Ctrl Pts',(-29.5992193388311,-1.21100224180705,
0.9536755038247));
#56512=CARTESIAN_POINT('Ctrl Pts',(-29.5731871923369,-1.465134583482,0.476406034057459));
#56513=CARTESIAN_POINT('Ctrl Pts',(-29.5471550458428,-1.46589706054516,
-0.000165931013407645));
#56514=CARTESIAN_POINT('Origin',(-17.3,0.,0.));
#56515=CARTESIAN_POINT('',(-28.9758449541571,-1.46341902613524,0.00135233047681406));
#56516=CARTESIAN_POINT('',(-29.0471550458428,-1.46298909506461,0.00133440455282766));
#56517=CARTESIAN_POINT('',(-17.3,-1.4635,-1.79227059055215E-16));
#56518=CARTESIAN_POINT('Ctrl Pts',(-28.9758449541571,-1.46341902613524,
0.00135233047681406));
#56519=CARTESIAN_POINT('Ctrl Pts',(-28.9821609869633,-1.46448859466354,
0.117490729182389));
#56520=CARTESIAN_POINT('Ctrl Pts',(-28.9884770197694,-1.45183179978412,
0.233398749586752));
#56521=CARTESIAN_POINT('Ctrl Pts',(-28.9947930525756,-1.42456033886225,
0.345759597637241));
#56522=CARTESIAN_POINT('Ctrl Pts',(-29.0213075949813,-1.31007545107446,
0.8174475324222));
#56523=CARTESIAN_POINT('Ctrl Pts',(-29.047822137387,-0.938036495013489,
1.2266236952684));
#56524=CARTESIAN_POINT('Ctrl Pts',(-29.0743366797926,-0.479335794560193,
1.38533716274088));
#56525=CARTESIAN_POINT('Ctrl Pts',(-29.1008512221983,-0.0206350941068899,
1.54405063021337));
#56526=CARTESIAN_POINT('Ctrl Pts',(-29.127365764604,0.524727350738727,1.45230140231214));
#56527=CARTESIAN_POINT('Ctrl Pts',(-29.1538803070097,0.906244828142636,
1.15223355700237));
#56528=CARTESIAN_POINT('Ctrl Pts',(-29.1803948494154,1.28776230554654,0.852165711692601));
#56529=CARTESIAN_POINT('Ctrl Pts',(-29.2069093918211,1.50543481550872,0.343779248974287));
#56530=CARTESIAN_POINT('Ctrl Pts',(-29.2334239342268,1.45927669667193,-0.139403661960002));
#56531=CARTESIAN_POINT('Ctrl Pts',(-29.2599384766324,1.41311857783515,-0.622586572894284));
#56532=CARTESIAN_POINT('Ctrl Pts',(-29.2864530190381,1.10312983019941,-1.08056593204455));
#56533=CARTESIAN_POINT('Ctrl Pts',(-29.3129675614438,0.671700643279443,
-1.30297356237016));
#56534=CARTESIAN_POINT('Ctrl Pts',(-29.3394821038495,0.240271456359465,
-1.52538119269578));
#56535=CARTESIAN_POINT('Ctrl Pts',(-29.3659966462552,-0.312598169844754,
-1.51221709419673));
#56536=CARTESIAN_POINT('Ctrl Pts',(-29.3925111886609,-0.732953175826774,
-1.26952806210145));
#56537=CARTESIAN_POINT('Ctrl Pts',(-29.4190257310666,-1.15330818180879,
-1.02683903000616));
#56538=CARTESIAN_POINT('Ctrl Pts',(-29.4455402734722,-1.44114856756861,
-0.554625064314648));
#56539=CARTESIAN_POINT('Ctrl Pts',(-29.4720548158779,-1.4642577691473,-0.0697928643156378));
#56540=CARTESIAN_POINT('Ctrl Pts',(-29.4733181953043,-1.46535888903042,
-0.0466913143301533));
#56541=CARTESIAN_POINT('Ctrl Pts',(-29.4745815747307,-1.46585896745433,
-0.023561116106705));
#56542=CARTESIAN_POINT('Ctrl Pts',(-29.4758449541571,-1.4657700110061,-0.000426988761815655));
#56543=CARTESIAN_POINT('Ctrl Pts',(-29.5471550458428,-1.46589706054516,
-0.000165931013407645));
#56544=CARTESIAN_POINT('Ctrl Pts',(-29.5466726499313,-1.46591118983788,
-0.00899718000605618));
#56545=CARTESIAN_POINT('Ctrl Pts',(-29.5461902540197,-1.46583831452614,
-0.017828189482769));
#56546=CARTESIAN_POINT('Ctrl Pts',(-29.5457078581082,-1.46567772600194,
-0.0266576036401217));
#56547=CARTESIAN_POINT('Ctrl Pts',(-29.5191933157025,-1.4568510939076,-0.511959967308562));
#56548=CARTESIAN_POINT('Ctrl Pts',(-29.4926787732968,-1.18303655585298,
-0.992442756768303));
#56549=CARTESIAN_POINT('Ctrl Pts',(-29.4661642308911,-0.770008044804517,
-1.24740107233655));
#56550=CARTESIAN_POINT('Ctrl Pts',(-29.4396496884855,-0.356979533756049,
-1.50235938790479));
#56551=CARTESIAN_POINT('Ctrl Pts',(-29.4131351460798,0.195262950286247,
-1.53179322958155));
#56552=CARTESIAN_POINT('Ctrl Pts',(-29.3866206036741,0.63305241921202,-1.32218246050227));
#56553=CARTESIAN_POINT('Ctrl Pts',(-29.3601060612684,1.07084188813778,-1.11257169142301));
#56554=CARTESIAN_POINT('Ctrl Pts',(-29.3335915188627,1.39417834194701,-0.663916311587708));
#56555=CARTESIAN_POINT('Ctrl Pts',(-29.307076976457,1.45454045757213,-0.182301622636509));
#56556=CARTESIAN_POINT('Ctrl Pts',(-29.2805624340513,1.51490257319725,0.299313066314696));
#56557=CARTESIAN_POINT('Ctrl Pts',(-29.2540478916456,1.31229035063826,0.813887064381816));
#56558=CARTESIAN_POINT('Ctrl Pts',(-29.22753334924,0.939771660868593,1.12505602072));
#56559=CARTESIAN_POINT('Ctrl Pts',(-29.2010188068343,0.567252971098922,
1.43622497705819));
#56560=CARTESIAN_POINT('Ctrl Pts',(-29.1745042644286,0.0248278141185692,
1.54398889166744));
#56561=CARTESIAN_POINT('Ctrl Pts',(-29.1479897220229,-0.438346311650147,
1.39884750255085));
#56562=CARTESIAN_POINT('Ctrl Pts',(-29.1214751796172,-0.901520437418864,
1.25370611343427));
#56563=CARTESIAN_POINT('Ctrl Pts',(-29.0949606372115,-1.28544353197594,
0.855659420591842));
#56564=CARTESIAN_POINT('Ctrl Pts',(-29.0684460948058,-1.41376441286716,
0.387546138208605));
#56565=CARTESIAN_POINT('Ctrl Pts',(-29.0613490784848,-1.44811142787792,
0.262248573033834));
#56566=CARTESIAN_POINT('Ctrl Pts',(-29.0542520621638,-1.4641459298896,0.131931116546837));
#56567=CARTESIAN_POINT('Ctrl Pts',(-29.0471550458428,-1.46298909506461,
0.00133440455282766));
#56568=CARTESIAN_POINT('Origin',(-17.3,0.,0.));
#56569=CARTESIAN_POINT('',(-28.4758449541571,-1.46109929919025,-0.000194400770703457));
#56570=CARTESIAN_POINT('',(-28.5471550458428,-1.46119040624119,-0.000426588110409748));
#56571=CARTESIAN_POINT('',(-17.3,-1.4635,-1.79227059055215E-16));
#56572=CARTESIAN_POINT('Ctrl Pts',(-28.4758449541571,-1.46109929919025,
-0.000194400770703457));
#56573=CARTESIAN_POINT('Ctrl Pts',(-28.4897403991958,-1.46079627679699,
0.256337369532174));
#56574=CARTESIAN_POINT('Ctrl Pts',(-28.5036358442345,-1.39658427978759,
0.513011004497548));
#56575=CARTESIAN_POINT('Ctrl Pts',(-28.5175312892732,-1.26934288368266,
0.733273824748846));
#56576=CARTESIAN_POINT('Ctrl Pts',(-28.5440458316789,-1.02654768112642,
1.15356751607571));
#56577=CARTESIAN_POINT('Ctrl Pts',(-28.5705603740846,-0.55426102439479,
1.44128861530504));
#56578=CARTESIAN_POINT('Ctrl Pts',(-28.5970749164903,-0.0694230026690815,
1.46427535153673));
#56579=CARTESIAN_POINT('Ctrl Pts',(-28.623589458896,0.415415019056634,1.48726208776842));
#56580=CARTESIAN_POINT('Ctrl Pts',(-28.6501040013017,0.912804405776441,
1.24551446100245));
#56581=CARTESIAN_POINT('Ctrl Pts',(-28.6766185437074,1.19427438370317,0.850076793500457));
#56582=CARTESIAN_POINT('Ctrl Pts',(-28.703133086113,1.4757443616299,0.45463912599847));
#56583=CARTESIAN_POINT('Ctrl Pts',(-28.7296476285187,1.54129493076356,-0.0944885822395179));
#56584=CARTESIAN_POINT('Ctrl Pts',(-28.7561621709244,1.36081610152252,-0.54507008380085));
#56585=CARTESIAN_POINT('Ctrl Pts',(-28.7826767133301,1.18033727228147,-0.995651585362183));
#56586=CARTESIAN_POINT('Ctrl Pts',(-28.8091912557358,0.753829044665707,
-1.34768688024685));
#56587=CARTESIAN_POINT('Ctrl Pts',(-28.8357057981415,0.277203650402953,
-1.43947212359979));
#56588=CARTESIAN_POINT('Ctrl Pts',(-28.8622203405472,-0.199421743859794,
-1.53125736695273));
#56589=CARTESIAN_POINT('Ctrl Pts',(-28.8887348829528,-0.726164304769535,
-1.36279255877395));
#56590=CARTESIAN_POINT('Ctrl Pts',(-28.9152494253585,-1.0610701754671,-1.01146030132271));
#56591=CARTESIAN_POINT('Ctrl Pts',(-28.935447934958,-1.31619807247997,-0.743818949412031));
#56592=CARTESIAN_POINT('Ctrl Pts',(-28.9556464445576,-1.45999857363774,
-0.370055265575945));
#56593=CARTESIAN_POINT('Ctrl Pts',(-28.9758449541571,-1.46341902613524,
0.00135233047681406));
#56594=CARTESIAN_POINT('Ctrl Pts',(-29.0471550458428,-1.46298909506461,
0.00133440455282766));
#56595=CARTESIAN_POINT('Ctrl Pts',(-29.0277375197581,-1.459823980406,-0.355979845128287));
#56596=CARTESIAN_POINT('Ctrl Pts',(-29.0083199936734,-1.32796855895135,
-0.715384535896872));
#56597=CARTESIAN_POINT('Ctrl Pts',(-28.9889024675888,-1.09038580476693,
-0.979786007806199));
#56598=CARTESIAN_POINT('Ctrl Pts',(-28.9623879251831,-0.765967648550108,
-1.34082499951372));
#56599=CARTESIAN_POINT('Ctrl Pts',(-28.9358733827774,-0.244412668891087,
-1.52472311100471));
#56600=CARTESIAN_POINT('Ctrl Pts',(-28.9093588403717,0.234708140222739,
-1.44700860855878));
#56601=CARTESIAN_POINT('Ctrl Pts',(-28.882844297966,0.713828949336565,-1.36929410611286));
#56602=CARTESIAN_POINT('Ctrl Pts',(-28.8563297555604,1.1505155879052,-1.02996698973001));
#56603=CARTESIAN_POINT('Ctrl Pts',(-28.8298152131547,1.34418047428712,-0.58489373126688));
#56604=CARTESIAN_POINT('Ctrl Pts',(-28.803300670749,1.53784536066904,-0.139820472803748));
#56605=CARTESIAN_POINT('Ctrl Pts',(-28.7767861283433,1.48848849486424,0.410998927739651));
#56606=CARTESIAN_POINT('Ctrl Pts',(-28.7502715859376,1.21878145295217,0.814551161235334));
#56607=CARTESIAN_POINT('Ctrl Pts',(-28.7237570435319,0.94907441104011,1.21810339473101));
#56608=CARTESIAN_POINT('Ctrl Pts',(-28.6972425011262,0.45901719302078,1.47438846117896));
#56609=CARTESIAN_POINT('Ctrl Pts',(-28.6707279587205,-0.0262873847002612,
1.46568441273545));
#56610=CARTESIAN_POINT('Ctrl Pts',(-28.6442134163149,-0.511591962421303,
1.45698036429194));
#56611=CARTESIAN_POINT('Ctrl Pts',(-28.6176988739092,-0.992143899844064,
1.18328720095696));
#56612=CARTESIAN_POINT('Ctrl Pts',(-28.5911843315035,-1.24720653486975,
0.77032310344961));
#56613=CARTESIAN_POINT('Ctrl Pts',(-28.5765079029499,-1.38838975735801,
0.541737673630878));
#56614=CARTESIAN_POINT('Ctrl Pts',(-28.5618314743964,-1.46048564494658,
0.270481227632335));
#56615=CARTESIAN_POINT('Ctrl Pts',(-28.5471550458428,-1.46119040624119,
-0.000426588110409748));
#56616=CARTESIAN_POINT('Origin',(-17.3,0.,0.));
#56617=CARTESIAN_POINT('',(-27.9758449541571,-1.46413482731608,-0.00128332369852588));
#56618=CARTESIAN_POINT('',(-28.0471550458428,-1.46455866562899,-0.00118106958518242));
#56619=CARTESIAN_POINT('',(-17.3,-1.4635,-1.79227059055215E-16));
#56620=CARTESIAN_POINT('Ctrl Pts',(-27.9758449541571,-1.46413482731608,
-0.00128332369852588));
#56621=CARTESIAN_POINT('Ctrl Pts',(-27.9973198114283,-1.46051051517567,
0.393098621091974));
#56622=CARTESIAN_POINT('Ctrl Pts',(-28.0187946686996,-1.29581441774694,
0.790148035238067));
#56623=CARTESIAN_POINT('Ctrl Pts',(-28.0402695259709,-1.01119225149223,
1.06132562813666));
#56624=CARTESIAN_POINT('Ctrl Pts',(-28.0667840683766,-0.659775410791775,
1.39614274452351));
#56625=CARTESIAN_POINT('Ctrl Pts',(-28.0932986107822,-0.125539583016236,
1.53907698601051));
#56626=CARTESIAN_POINT('Ctrl Pts',(-28.1198131531879,0.346119418784083,
1.42447295739799));
#56627=CARTESIAN_POINT('Ctrl Pts',(-28.1463276955936,0.817778420584388,
1.30986892878547));
#56628=CARTESIAN_POINT('Ctrl Pts',(-28.1728422379993,1.22686059640947,0.93772663007344));
#56629=CARTESIAN_POINT('Ctrl Pts',(-28.199356780405,1.38545819480999,0.478985854542129));
#56630=CARTESIAN_POINT('Ctrl Pts',(-28.2258713228107,1.54405579321051,0.0202450790108123));
#56631=CARTESIAN_POINT('Ctrl Pts',(-28.2523858652164,1.45216881418645,-0.5250941733398));
#56632=CARTESIAN_POINT('Ctrl Pts',(-28.2789004076221,1.15200461028516,-0.906535843913156));
#56633=CARTESIAN_POINT('Ctrl Pts',(-28.3054149500277,0.85184040638387,-1.28797751448652));
#56634=CARTESIAN_POINT('Ctrl Pts',(-28.3319294924334,0.343398977605346,
-1.50552160328263));
#56635=CARTESIAN_POINT('Ctrl Pts',(-28.3584440348391,-0.139772258755166,
-1.45924143790536));
#56636=CARTESIAN_POINT('Ctrl Pts',(-28.3849585772448,-0.622943495115664,
-1.41296127252808));
#56637=CARTESIAN_POINT('Ctrl Pts',(-28.4114731196505,-1.08084453905814,
-1.10285685297743));
#56638=CARTESIAN_POINT('Ctrl Pts',(-28.4379876620562,-1.30314318683895,
-0.671371501489916));
#56639=CARTESIAN_POINT('Ctrl Pts',(-28.4506067594232,-1.40894204385757,
-0.466014170424791));
#56640=CARTESIAN_POINT('Ctrl Pts',(-28.4632258567901,-1.46137448786354,
-0.233162785601588));
#56641=CARTESIAN_POINT('Ctrl Pts',(-28.4758449541571,-1.46109929919025,
-0.000194400770703457));
#56642=CARTESIAN_POINT('Ctrl Pts',(-28.5471550458428,-1.46119040624119,
-0.000426588110409748));
#56643=CARTESIAN_POINT('Ctrl Pts',(-28.5353169319907,-1.46175887181942,
-0.21894279963225));
#56644=CARTESIAN_POINT('Ctrl Pts',(-28.5234788181386,-1.41587918011866,
-0.437232186984281));
#56645=CARTESIAN_POINT('Ctrl Pts',(-28.5116407042864,-1.32234232213604,
-0.632718426646407));
#56646=CARTESIAN_POINT('Ctrl Pts',(-28.4851261618807,-1.11284214174804,
-1.07056082755534));
#56647=CARTESIAN_POINT('Ctrl Pts',(-28.458611619475,-0.664268448343429,
-1.39401059769349));
#56648=CARTESIAN_POINT('Ctrl Pts',(-28.4320970770694,-0.18266902172827,
-1.45449436328604));
#56649=CARTESIAN_POINT('Ctrl Pts',(-28.4055825346637,0.298930404886896,
-1.5149781288786));
#56650=CARTESIAN_POINT('Ctrl Pts',(-28.379067992258,0.813555564712618,-1.31249588992556));
#56651=CARTESIAN_POINT('Ctrl Pts',(-28.3525534498523,1.12481860626874,-0.940055810748326));
#56652=CARTESIAN_POINT('Ctrl Pts',(-28.3260389074466,1.43608164782485,-0.567615731571103));
#56653=CARTESIAN_POINT('Ctrl Pts',(-28.2995243650409,1.54398257111138,-0.0252178121697132));
#56654=CARTESIAN_POINT('Ctrl Pts',(-28.2730098226352,1.3989581805841,0.437992960339399));
#56655=CARTESIAN_POINT('Ctrl Pts',(-28.2464952802295,1.25393379005681,0.901203732848524));
#56656=CARTESIAN_POINT('Ctrl Pts',(-28.2199807378239,0.855984085715685,
1.28522735846536));
#56657=CARTESIAN_POINT('Ctrl Pts',(-28.1934661954182,0.387903231060652,
1.41366647681225));
#56658=CARTESIAN_POINT('Ctrl Pts',(-28.1669516530125,-0.0801776235943734,
1.54210559515913));
#56659=CARTESIAN_POINT('Ctrl Pts',(-28.1404371106068,-0.61838962856331,
1.41496020623609));
#56660=CARTESIAN_POINT('Ctrl Pts',(-28.1139225682011,-0.979510554100306,
1.09063325583633));
#56661=CARTESIAN_POINT('Ctrl Pts',(-28.091666727415,-1.28262911071393,0.818398915137616));
#56662=CARTESIAN_POINT('Ctrl Pts',(-28.0694108866289,-1.46097587203959,
0.407237771902873));
#56663=CARTESIAN_POINT('Ctrl Pts',(-28.0471550458428,-1.46455866562899,
-0.00118106958518242));
#56664=CARTESIAN_POINT('Origin',(-17.3,0.,0.));
#56665=CARTESIAN_POINT('',(-27.4758449541571,-1.46536634381812,0.000808685770614676));
#56666=CARTESIAN_POINT('',(-27.5471550458428,-1.46502789863774,0.00100125412595091));
#56667=CARTESIAN_POINT('',(-17.3,-1.4635,-1.79227059055215E-16));
#56668=CARTESIAN_POINT('Ctrl Pts',(-27.4758449541571,-1.46536634381812,
0.000808685770614676));
#56669=CARTESIAN_POINT('Ctrl Pts',(-27.4783846812552,-1.46567494044697,
0.0473483563683534));
#56670=CARTESIAN_POINT('Ctrl Pts',(-27.4809244083533,-1.46365077701734,
0.0938608341503805));
#56671=CARTESIAN_POINT('Ctrl Pts',(-27.4834641354515,-1.4592060860354,0.140140846632458));
#56672=CARTESIAN_POINT('Ctrl Pts',(-27.5099786778571,-1.41280387707044,
0.623300377591606));
#56673=CARTESIAN_POINT('Ctrl Pts',(-27.5364932202628,-1.10258380539034,
1.08112307711105));
#56674=CARTESIAN_POINT('Ctrl Pts',(-27.5630077626685,-0.671042316865148,
1.30331272816384));
#56675=CARTESIAN_POINT('Ctrl Pts',(-27.5895223050742,-0.239500828339974,
1.52550237921661));
#56676=CARTESIAN_POINT('Ctrl Pts',(-27.6160368474799,0.313362077030277,
1.51205898180275));
#56677=CARTESIAN_POINT('Ctrl Pts',(-27.6425513898856,0.733594426886151,
1.26915762427651));
#56678=CARTESIAN_POINT('Ctrl Pts',(-27.6690659322913,1.15382677674203,1.02625626675027));
#56679=CARTESIAN_POINT('Ctrl Pts',(-27.6955804746969,1.44142857108353,0.553896949111648));
#56680=CARTESIAN_POINT('Ctrl Pts',(-27.7220950171026,1.4642928405016,0.0690531365931595));
#56681=CARTESIAN_POINT('Ctrl Pts',(-27.7486095595083,1.48715710991968,-0.415790675925329));
#56682=CARTESIAN_POINT('Ctrl Pts',(-27.775124101914,1.24528385441433,-0.913118983323688));
#56683=CARTESIAN_POINT('Ctrl Pts',(-27.8016386443197,0.849775102535385,
-1.19448906798203));
#56684=CARTESIAN_POINT('Ctrl Pts',(-27.8281531867254,0.454266350656434,
-1.47585915264038));
#56685=CARTESIAN_POINT('Ctrl Pts',(-27.8546677291311,-0.0948778975961176,
-1.54127101455871));
#56686=CARTESIAN_POINT('Ctrl Pts',(-27.8811822715368,-0.545413797321521,
-1.36067837790895));
#56687=CARTESIAN_POINT('Ctrl Pts',(-27.9076968139424,-0.995949697046905,
-1.18008574125919));
#56688=CARTESIAN_POINT('Ctrl Pts',(-27.9342113563481,-1.34787724824515,
-0.753488606041366));
#56689=CARTESIAN_POINT('Ctrl Pts',(-27.9607258987538,-1.4395420970316,-0.27684004278912));
#56690=CARTESIAN_POINT('Ctrl Pts',(-27.9657655838882,-1.45696506321787,
-0.186242262830691));
#56691=CARTESIAN_POINT('Ctrl Pts',(-27.9708052690226,-1.46498537508856,
-0.0938362473031713));
#56692=CARTESIAN_POINT('Ctrl Pts',(-27.9758449541571,-1.46413482731608,
-0.00128332369852588));
#56693=CARTESIAN_POINT('Ctrl Pts',(-28.0471550458428,-1.46455866562899,
-0.00118106958518242));
#56694=CARTESIAN_POINT('Ctrl Pts',(-28.0428963442232,-1.46524424066561,
-0.0793328679570782));
#56695=CARTESIAN_POINT('Ctrl Pts',(-28.0386376426036,-1.45953072434846,
-0.157384255245247));
#56696=CARTESIAN_POINT('Ctrl Pts',(-28.0343789409841,-1.44706784773524,
-0.234342630310688));
#56697=CARTESIAN_POINT('Ctrl Pts',(-28.0078643985784,-1.36947436972812,
-0.713483054181464));
#56698=CARTESIAN_POINT('Ctrl Pts',(-27.9813498561727,-1.03025756760883,
-1.15025539004653));
#56699=CARTESIAN_POINT('Ctrl Pts',(-27.954835313767,-0.585233241495049,
-1.34403269207979));
#56700=CARTESIAN_POINT('Ctrl Pts',(-27.9283207713613,-0.140208915381278,
-1.53780999411304));
#56701=CARTESIAN_POINT('Ctrl Pts',(-27.9018062289556,0.41062293472698,-1.48859226231448));
#56702=CARTESIAN_POINT('Ctrl Pts',(-27.87529168655,0.814243281120257,-1.21898716296791));
#56703=CARTESIAN_POINT('Ctrl Pts',(-27.8487771441443,1.21786362751354,-0.94938206362134));
#56704=CARTESIAN_POINT('Ctrl Pts',(-27.8222626017386,1.47427247019185,-0.459389596726757));
#56705=CARTESIAN_POINT('Ctrl Pts',(-27.7957480593329,1.4656910059545,0.0259171640831991));
#56706=CARTESIAN_POINT('Ctrl Pts',(-27.7692335169272,1.45710954171716,0.511223924893148));
#56707=CARTESIAN_POINT('Ctrl Pts',(-27.7427189745215,1.18353777056415,0.991844979618477));
#56708=CARTESIAN_POINT('Ctrl Pts',(-27.7162044321158,0.770638112946094,
1.24701191782794));
#56709=CARTESIAN_POINT('Ctrl Pts',(-27.6896898897102,0.357738455328029,
1.50217885603741));
#56710=CARTESIAN_POINT('Ctrl Pts',(-27.6631753473044,-0.194489088755087,
1.53189167773102));
#56711=CARTESIAN_POINT('Ctrl Pts',(-27.6366608048988,-0.632384393711719,
1.32250209940094));
#56712=CARTESIAN_POINT('Ctrl Pts',(-27.6101462624931,-1.07027969866835,
1.11311252107087));
#56713=CARTESIAN_POINT('Ctrl Pts',(-27.5836317200874,-1.39384276449848,
0.664620542717102));
#56714=CARTESIAN_POINT('Ctrl Pts',(-27.5571171776817,-1.45444817619946,
0.183036409165274));
#56715=CARTESIAN_POINT('Ctrl Pts',(-27.5537964670688,-1.4620384649836,0.122722279701757));
#56716=CARTESIAN_POINT('Ctrl Pts',(-27.5504757564558,-1.46550417497613,
0.0618890887112012));
#56717=CARTESIAN_POINT('Ctrl Pts',(-27.5471550458428,-1.46502789863774,
0.00100125412595091));
#56718=CARTESIAN_POINT('Origin',(-17.3,0.,0.));
#56719=CARTESIAN_POINT('',(-26.9758449541571,-1.46162142615836,0.000882726340737661));
#56720=CARTESIAN_POINT('',(-27.0471550458428,-1.46138800853787,0.00068780616967229));
#56721=CARTESIAN_POINT('',(-17.3,-1.4635,-1.79227059055215E-16));
#56722=CARTESIAN_POINT('Ctrl Pts',(-26.9758449541571,-1.46162142615836,
0.000882726340737661));
#56723=CARTESIAN_POINT('Ctrl Pts',(-26.9859640934878,-1.46264431827847,
0.187531233801553));
#56724=CARTESIAN_POINT('Ctrl Pts',(-26.9960832328184,-1.42950625207749,
0.373830171742523));
#56725=CARTESIAN_POINT('Ctrl Pts',(-27.0062023721491,-1.36054056748059,
0.54575747604334));
#56726=CARTESIAN_POINT('Ctrl Pts',(-27.0327169145548,-1.17983413494441,
0.996247745187448));
#56727=CARTESIAN_POINT('Ctrl Pts',(-27.0592314569605,-0.753148119342491,
1.34806753024541));
#56728=CARTESIAN_POINT('Ctrl Pts',(-27.0857459993662,-0.276476417512137,
1.4396119786169));
#56729=CARTESIAN_POINT('Ctrl Pts',(-27.1122605417718,0.200195284318217,
1.53115642698839));
#56730=CARTESIAN_POINT('Ctrl Pts',(-27.1387750841775,0.726852672377007,
1.3624255386734));
#56731=CARTESIAN_POINT('Ctrl Pts',(-27.1652896265832,1.06158101309092,1.01092413714505));
#56732=CARTESIAN_POINT('Ctrl Pts',(-27.1918041689889,1.39630935380484,0.659422735616693));
#56733=CARTESIAN_POINT('Ctrl Pts',(-27.2183187113946,1.53910864717388,0.125150820874972));
#56734=CARTESIAN_POINT('Ctrl Pts',(-27.2448332538003,1.42438548504866,-0.346479217847628));
#56735=CARTESIAN_POINT('Ctrl Pts',(-27.271347796206,1.30966232292344,-0.818109256570215));
#56736=CARTESIAN_POINT('Ctrl Pts',(-27.2978623386116,0.937416705303969,
-1.22709741927369));
#56737=CARTESIAN_POINT('Ctrl Pts',(-27.3243768810173,0.478635883963488,
-1.38557913848329));
#56738=CARTESIAN_POINT('Ctrl Pts',(-27.350891423423,0.0198550626230001,
-1.5440608576929));
#56739=CARTESIAN_POINT('Ctrl Pts',(-27.3774059658287,-0.525460962438503,
-1.45203613340863));
#56740=CARTESIAN_POINT('Ctrl Pts',(-27.4039205082344,-0.906826801844342,
-1.15177559006708));
#56741=CARTESIAN_POINT('Ctrl Pts',(-27.427895323542,-1.25166305903765,-0.880275861328805));
#56742=CARTESIAN_POINT('Ctrl Pts',(-27.4518701388495,-1.46245321697601,
-0.438521984001684));
#56743=CARTESIAN_POINT('Ctrl Pts',(-27.4758449541571,-1.46536634381812,
0.000808685770614676));
#56744=CARTESIAN_POINT('Ctrl Pts',(-27.5471550458428,-1.46502789863774,
0.00100125412595091));
#56745=CARTESIAN_POINT('Ctrl Pts',(-27.5239612140501,-1.46170129943445,
-0.424275850141513));
#56746=CARTESIAN_POINT('Ctrl Pts',(-27.5007673822574,-1.26606638633314,
-0.852218721532124));
#56747=CARTESIAN_POINT('Ctrl Pts',(-27.4775735504647,-0.94033990065008,
-1.12458112005112));
#56748=CARTESIAN_POINT('Ctrl Pts',(-27.451059008059,-0.567978455827939,
-1.43593822696579));
#56749=CARTESIAN_POINT('Ctrl Pts',(-27.4245444656533,-0.0256078086118435,
-1.54397615204525));
#56750=CARTESIAN_POINT('Ctrl Pts',(-27.3980299232476,0.437639581083625,
-1.39906876936017));
#56751=CARTESIAN_POINT('Ctrl Pts',(-27.3715153808419,0.9008869707791,-1.2541613866751));
#56752=CARTESIAN_POINT('Ctrl Pts',(-27.3450008384362,1.28501110295395,-0.856308696225503));
#56753=CARTESIAN_POINT('Ctrl Pts',(-27.3184862960305,1.41356845056175,-0.388260299163449));
#56754=CARTESIAN_POINT('Ctrl Pts',(-27.2919717536248,1.54212579816955,0.0797880978986051));
#56755=CARTESIAN_POINT('Ctrl Pts',(-27.2654572112192,1.41511636121028,0.618032201573119));
#56756=CARTESIAN_POINT('Ctrl Pts',(-27.2389426688135,1.09088063732047,0.979235037899136));
#56757=CARTESIAN_POINT('Ctrl Pts',(-27.2124281264078,0.766644913430665,
1.34043787422515));
#56758=CARTESIAN_POINT('Ctrl Pts',(-27.1859135840021,0.245182902610327,
1.52459944320268));
#56759=CARTESIAN_POINT('Ctrl Pts',(-27.1593990415964,-0.23397710544699,
1.44712699458503));
#56760=CARTESIAN_POINT('Ctrl Pts',(-27.1328844991907,-0.713137113504306,
1.36965454596737));
#56761=CARTESIAN_POINT('Ctrl Pts',(-27.106369956785,-1.1499951187986,1.03054807975452));
#56762=CARTESIAN_POINT('Ctrl Pts',(-27.0798554143794,-1.3438848241197,0.585572714383804));
#56763=CARTESIAN_POINT('Ctrl Pts',(-27.0689552915338,-1.42359284148406,
0.402643434611333));
#56764=CARTESIAN_POINT('Ctrl Pts',(-27.0580551686883,-1.46223847794561,
0.201821989221122));
#56765=CARTESIAN_POINT('Ctrl Pts',(-27.0471550458428,-1.46138800853787,
0.00068780616967229));
#56766=CARTESIAN_POINT('Origin',(-17.3,0.,0.));
#56767=CARTESIAN_POINT('',(-26.4758449541571,-1.46213373306659,-0.00114472513446554));
#56768=CARTESIAN_POINT('',(-26.5471550458428,-1.46250200525633,-0.00125517408728269));
#56769=CARTESIAN_POINT('',(-17.3,-1.4635,-1.79227059055215E-16));
#56770=CARTESIAN_POINT('Ctrl Pts',(-26.4758449541571,-1.46213373306659,
-0.00114472513446554));
#56771=CARTESIAN_POINT('Ctrl Pts',(-26.4935435057203,-1.45976174366936,
0.325019611661761));
#56772=CARTESIAN_POINT('Ctrl Pts',(-26.5112420572835,-1.35203577341253,
0.652605278604839));
#56773=CARTESIAN_POINT('Ctrl Pts',(-26.5289406088467,-1.15154649636273,
0.90711770191763));
#56774=CARTESIAN_POINT('Ctrl Pts',(-26.5554551512524,-0.851189632738311,
1.28840768582383));
#56775=CARTESIAN_POINT('Ctrl Pts',(-26.5819696936581,-0.342638369162514,
1.50569489065639));
#56776=CARTESIAN_POINT('Ctrl Pts',(-26.6084842360638,0.140509425568441,
1.45917064106431));
#56777=CARTESIAN_POINT('Ctrl Pts',(-26.6349987784695,0.623657220299389,
1.41264639147224));
#56778=CARTESIAN_POINT('Ctrl Pts',(-26.6615133208752,1.08140154618549,1.10231068745555));
#56779=CARTESIAN_POINT('Ctrl Pts',(-26.6880278632808,1.30348218633397,0.67071308942618));
#56780=CARTESIAN_POINT('Ctrl Pts',(-26.7145424056865,1.52556282648246,0.239115491396808));
#56781=CARTESIAN_POINT('Ctrl Pts',(-26.7410569480922,1.51197978089332,-0.313744000645244));
#56782=CARTESIAN_POINT('Ctrl Pts',(-26.7675714904979,1.26897228389482,-0.733914982218229));
#56783=CARTESIAN_POINT('Ctrl Pts',(-26.7940860329036,1.02596478689631,-1.15408596379121));
#56784=CARTESIAN_POINT('Ctrl Pts',(-26.8206005753093,0.553532838488442,
-1.44156843489514));
#56785=CARTESIAN_POINT('Ctrl Pts',(-26.847115117715,0.0686832661114671,
-1.4643102360408));
#56786=CARTESIAN_POINT('Ctrl Pts',(-26.8736296601207,-0.416166306265507,
-1.48705203718647));
#56787=CARTESIAN_POINT('Ctrl Pts',(-26.9001442025263,-0.913433502611594,
-1.24505316837387));
#56788=CARTESIAN_POINT('Ctrl Pts',(-26.926658744932,-1.19470367604941,-0.849473357352444));
#56789=CARTESIAN_POINT('Ctrl Pts',(-26.943054148007,-1.36862852815262,-0.604864555480574));
#56790=CARTESIAN_POINT('Ctrl Pts',(-26.9594495510821,-1.45996409858695,
-0.301532075271507));
#56791=CARTESIAN_POINT('Ctrl Pts',(-26.9758449541571,-1.46162142615836,
0.000882726340737661));
#56792=CARTESIAN_POINT('Ctrl Pts',(-27.0471550458428,-1.46138800853787,
0.00068780616967229));
#56793=CARTESIAN_POINT('Ctrl Pts',(-27.0315406262826,-1.46016971161189,
-0.287436792659947));
#56794=CARTESIAN_POINT('Ctrl Pts',(-27.0159262067225,-1.37790325039224,
-0.576203146234523));
#56795=CARTESIAN_POINT('Ctrl Pts',(-27.0003117871623,-1.2191927952091,-0.813935349054367));
#56796=CARTESIAN_POINT('Ctrl Pts',(-26.9737972447566,-0.949689655629521,
-1.21762378259322));
#56797=CARTESIAN_POINT('Ctrl Pts',(-26.9472827023509,-0.459761971122466,
-1.47415638514234));
#56798=CARTESIAN_POINT('Ctrl Pts',(-26.9207681599452,0.0255469418125742,
-1.46569750565868));
#56799=CARTESIAN_POINT('Ctrl Pts',(-26.8942536175395,0.510855854747614,
-1.45723862617501));
#56800=CARTESIAN_POINT('Ctrl Pts',(-26.8677390751339,0.991545996110626,
-1.18378826465857));
#56801=CARTESIAN_POINT('Ctrl Pts',(-26.8412245327282,1.24681722122356,-0.770953073273854));
#56802=CARTESIAN_POINT('Ctrl Pts',(-26.8147099903225,1.5020884463365,-0.358117881889143));
#56803=CARTESIAN_POINT('Ctrl Pts',(-26.7881954479168,1.53194075519934,0.194102139363843));
#56804=CARTESIAN_POINT('Ctrl Pts',(-26.7616809055111,1.32266179228677,0.632050320429307));
#56805=CARTESIAN_POINT('Ctrl Pts',(-26.7351663631054,1.1133828293742,1.06999850149476));
#56806=CARTESIAN_POINT('Ctrl Pts',(-26.7086518206997,0.664972594686232,
1.39367484237271));
#56807=CARTESIAN_POINT('Ctrl Pts',(-26.6821372782941,0.18340378492406,1.45440189631531));
#56808=CARTESIAN_POINT('Ctrl Pts',(-26.6556227358884,-0.298165024838112,
1.51512895025791));
#56809=CARTESIAN_POINT('Ctrl Pts',(-26.6291081934827,-0.812892409674494,
1.31290671726514));
#56810=CARTESIAN_POINT('Ctrl Pts',(-26.602593651077,-1.12434356208232,0.940623930555713));
#56811=CARTESIAN_POINT('Ctrl Pts',(-26.5841141159989,-1.34141208274397,
0.681158286733034));
#56812=CARTESIAN_POINT('Ctrl Pts',(-26.5656345809209,-1.45973894627015,
0.339085538839498));
#56813=CARTESIAN_POINT('Ctrl Pts',(-26.5471550458428,-1.46250200525633,
-0.00125517408728269));
#56814=CARTESIAN_POINT('Origin',(-17.3,0.,0.));
#56815=CARTESIAN_POINT('',(-25.9758449541571,-1.46577604770729,-0.000418285830775106));
#56816=CARTESIAN_POINT('',(-26.0471550458428,-1.46589951635168,-0.000156764579445036));
#56817=CARTESIAN_POINT('',(-17.3,-1.4635,-1.79227059055215E-16));
#56818=CARTESIAN_POINT('Ctrl Pts',(-25.9758449541571,-1.46577604770729,
-0.000418285830775106));
#56819=CARTESIAN_POINT('Ctrl Pts',(-26.0011229179528,-1.46402865658604,
0.462449158555644));
#56820=CARTESIAN_POINT('Ctrl Pts',(-26.0264008817486,-1.22637013755602,
0.926861111284242));
#56821=CARTESIAN_POINT('Ctrl Pts',(-26.0516788455444,-0.849171557970889,
1.19491820789161));
#56822=CARTESIAN_POINT('Ctrl Pts',(-26.0781933879501,-0.453520713046003,
1.47608845216313));
#56823=CARTESIAN_POINT('Ctrl Pts',(-26.1047079303558,0.0956565101240506,
1.54122288713929));
#56824=CARTESIAN_POINT('Ctrl Pts',(-26.1312224727614,0.54610111994442,1.36040267024623));
#56825=CARTESIAN_POINT('Ctrl Pts',(-26.1577370151671,0.996545729764802,
1.17958245335315));
#56826=CARTESIAN_POINT('Ctrl Pts',(-26.1842515575728,1.34825772623547,0.752807584590828));
#56827=CARTESIAN_POINT('Ctrl Pts',(-26.2107660999785,1.43968176835123,0.276112774595261));
#56828=CARTESIAN_POINT('Ctrl Pts',(-26.2372806423842,1.53110581046699,-0.200582035400292));
#56829=CARTESIAN_POINT('Ctrl Pts',(-26.2637951847899,1.36224189822785,-0.727196786629095));
#56830=CARTESIAN_POINT('Ctrl Pts',(-26.2903097271955,1.0106559582983,-1.06183633031355));
#56831=CARTESIAN_POINT('Ctrl Pts',(-26.3168242696012,0.659070018368756,
-1.39647587399801));
#56832=CARTESIAN_POINT('Ctrl Pts',(-26.3433388120069,0.1247620507488,-1.53914021013813));
#56833=CARTESIAN_POINT('Ctrl Pts',(-26.3698533544126,-0.346838994804863,
-1.42429792181986));
#56834=CARTESIAN_POINT('Ctrl Pts',(-26.3963678968183,-0.818440040358527,
-1.30945563350158));
#56835=CARTESIAN_POINT('Ctrl Pts',(-26.422882439224,-1.22733416384589,-0.937106720724912));
#56836=CARTESIAN_POINT('Ctrl Pts',(-26.4493969816297,-1.38569999375305,
-0.478285882846657));
#56837=CARTESIAN_POINT('Ctrl Pts',(-26.4582129724721,-1.43835606772408,
-0.325729589655548));
#56838=CARTESIAN_POINT('Ctrl Pts',(-26.4670289633146,-1.46331526686215,
-0.163613489658279));
#56839=CARTESIAN_POINT('Ctrl Pts',(-26.4758449541571,-1.46213373306659,
-0.00114472513446554));
#56840=CARTESIAN_POINT('Ctrl Pts',(-26.5471550458428,-1.46250200525633,
-0.00125517408728269));
#56841=CARTESIAN_POINT('Ctrl Pts',(-26.5391200385152,-1.46370339907424,
-0.149237258631324));
#56842=CARTESIAN_POINT('Ctrl Pts',(-26.5310850311876,-1.44305676186228,
-0.296891891566712));
#56843=CARTESIAN_POINT('Ctrl Pts',(-26.5230500238599,-1.39917926887205,
-0.437286173905273));
#56844=CARTESIAN_POINT('Ctrl Pts',(-26.4965354814543,-1.25438890327467,
-0.900570151230718));
#56845=CARTESIAN_POINT('Ctrl Pts',(-26.4700209390486,-0.856633252100626,
-1.2847947654555));
#56846=CARTESIAN_POINT('Ctrl Pts',(-26.4435063966429,-0.388617342494253,
-1.41347033412192));
#56847=CARTESIAN_POINT('Ctrl Pts',(-26.4169918542372,0.0793985671121137,
-1.54214590278835));
#56848=CARTESIAN_POINT('Ctrl Pts',(-26.3904773118315,0.617674735150821,
-1.41527242589641));
#56849=CARTESIAN_POINT('Ctrl Pts',(-26.3639627694258,0.978959459220186,
-1.09112794920365));
#56850=CARTESIAN_POINT('Ctrl Pts',(-26.3374482270201,1.34024418328956,-0.766983472510881));
#56851=CARTESIAN_POINT('Ctrl Pts',(-26.3109336846144,1.52453746338961,-0.245567996017281));
#56852=CARTESIAN_POINT('Ctrl Pts',(-26.2844191422087,1.44718604910436,0.233611565654946));
#56853=CARTESIAN_POINT('Ctrl Pts',(-26.2579045998031,1.36983463481912,0.71279112732716));
#56854=CARTESIAN_POINT('Ctrl Pts',(-26.2313900573974,1.0308385261486,1.14973477417799));
#56855=CARTESIAN_POINT('Ctrl Pts',(-26.2048755149917,0.585912149911522,
1.34373687041627));
#56856=CARTESIAN_POINT('Ctrl Pts',(-26.178360972586,0.140985773674437,1.53773896665454));
#56857=CARTESIAN_POINT('Ctrl Pts',(-26.1518464301803,-0.409870870129208,
1.48879951228024));
#56858=CARTESIAN_POINT('Ctrl Pts',(-26.1253318877746,-0.813627365057277,
1.21939834966265));
#56859=CARTESIAN_POINT('Ctrl Pts',(-26.099272940464,-1.21044617741552,0.954626263663422));
#56860=CARTESIAN_POINT('Ctrl Pts',(-26.0732139931534,-1.4651766057368,0.476903693889965));
#56861=CARTESIAN_POINT('Ctrl Pts',(-26.0471550458428,-1.46589951635168,
-0.000156764579445036));
#56862=CARTESIAN_POINT('Origin',(-17.3,0.,0.));
#56863=CARTESIAN_POINT('',(-25.4758449541571,-1.4634040497188,0.00135246395512149));
#56864=CARTESIAN_POINT('',(-25.5471550458428,-1.462974653714,0.00133299795035805));
#56865=CARTESIAN_POINT('',(-17.3,-1.4635,-1.79227059055215E-16));
#56866=CARTESIAN_POINT('Ctrl Pts',(-25.4758449541571,-1.4634040497188,0.00135246395512149));
#56867=CARTESIAN_POINT('Ctrl Pts',(-25.4821877877797,-1.46447728228524,
0.117986719967053));
#56868=CARTESIAN_POINT('Ctrl Pts',(-25.4885306214023,-1.45171144302068,
0.234388849588667));
#56869=CARTESIAN_POINT('Ctrl Pts',(-25.494873455025,-1.42421026771716,0.347198749632873));
#56870=CARTESIAN_POINT('Ctrl Pts',(-25.5213879974306,-1.30924886053307,
0.818770771928236));
#56871=CARTESIAN_POINT('Ctrl Pts',(-25.5479025398363,-0.93679667635601,
1.22757083011101));
#56872=CARTESIAN_POINT('Ctrl Pts',(-25.574417082242,-0.477935851213949,
1.38582076061156));
#56873=CARTESIAN_POINT('Ctrl Pts',(-25.6009316246477,-0.0190750260718746,
1.54407069111212));
#56874=CARTESIAN_POINT('Ctrl Pts',(-25.6274461670534,0.526194440035206,
1.45177049393048));
#56875=CARTESIAN_POINT('Ctrl Pts',(-25.6539607094591,0.907408544114477,
1.15131732918673));
#56876=CARTESIAN_POINT('Ctrl Pts',(-25.6804752518648,1.28862264819373,0.850864164442985));
#56877=CARTESIAN_POINT('Ctrl Pts',(-25.7069897942705,1.50578139024517,0.342258032137153));
#56878=CARTESIAN_POINT('Ctrl Pts',(-25.7335043366762,1.45913510299437,-0.140877995539519));
#56879=CARTESIAN_POINT('Ctrl Pts',(-25.7600188790818,1.41248881574355,-0.624014023216204));
#56880=CARTESIAN_POINT('Ctrl Pts',(-25.7865334214875,1.10203749919048,-1.08167994626373));
#56881=CARTESIAN_POINT('Ctrl Pts',(-25.8130479638932,0.670383819193945,
-1.30365156133859));
#56882=CARTESIAN_POINT('Ctrl Pts',(-25.8395625062989,0.238730139197424,
-1.52562317641345));
#56883=CARTESIAN_POINT('Ctrl Pts',(-25.8660770487046,-0.314125904242543,
-1.51190048351566));
#56884=CARTESIAN_POINT('Ctrl Pts',(-25.8925915911103,-0.734235490724634,
-1.26878686254941));
#56885=CARTESIAN_POINT('Ctrl Pts',(-25.919106133516,-1.15434507720673,-1.02567324158315));
#56886=CARTESIAN_POINT('Ctrl Pts',(-25.9456206759216,-1.44170820673095,
-0.553168692548412));
#56887=CARTESIAN_POINT('Ctrl Pts',(-25.9721352183273,-1.46432753815322,
-0.0683133912476058));
#56888=CARTESIAN_POINT('Ctrl Pts',(-25.9733717969372,-1.46538245288565,
-0.0457008307393826));
#56889=CARTESIAN_POINT('Ctrl Pts',(-25.9746083755472,-1.46586152874133,
-0.023061406359889));
#56890=CARTESIAN_POINT('Ctrl Pts',(-25.9758449541571,-1.46577604770729,
-0.000418285830775106));
#56891=CARTESIAN_POINT('Ctrl Pts',(-26.0471550458428,-1.46589951635168,
-0.000156764579445036));
#56892=CARTESIAN_POINT('Ctrl Pts',(-26.0466994507477,-1.46591215517881,
-0.00849733192252772));
#56893=CARTESIAN_POINT('Ctrl Pts',(-26.0462438556526,-1.46584715304275,
-0.0168376968819965));
#56894=CARTESIAN_POINT('Ctrl Pts',(-26.0457882605576,-1.46570391184755,
-0.025176717911968));
#56895=CARTESIAN_POINT('Ctrl Pts',(-26.0192737181519,-1.45736761765727,
-0.510487752008116));
#56896=CARTESIAN_POINT('Ctrl Pts',(-25.9927591757462,-1.18403868322423,
-0.991246949339548));
#56897=CARTESIAN_POINT('Ctrl Pts',(-25.9662446333405,-0.771267984412847,
-1.24662244506899));
#56898=CARTESIAN_POINT('Ctrl Pts',(-25.9397300909348,-0.358497285601448,
-1.50199794079844));
#56899=CARTESIAN_POINT('Ctrl Pts',(-25.9132155485291,0.193715177588312,
-1.53198973492588));
#56900=CARTESIAN_POINT('Ctrl Pts',(-25.8867010061235,0.631716206820391,
-1.32282140078338));
#56901=CARTESIAN_POINT('Ctrl Pts',(-25.8601864637178,1.06971723605247,-1.11365306664087));
#56902=CARTESIAN_POINT('Ctrl Pts',(-25.8336719213121,1.39350683132687,-0.665324604228429));
#56903=CARTESIAN_POINT('Ctrl Pts',(-25.8071573789064,1.45435552363656,-0.183771148981231));
#56904=CARTESIAN_POINT('Ctrl Pts',(-25.7806428365007,1.51520421594625,0.297782306265959));
#56905=CARTESIAN_POINT('Ctrl Pts',(-25.754128294095,1.31311200529122,0.812560754347889));
#56906=CARTESIAN_POINT('Ctrl Pts',(-25.7276137516893,0.940907900447105,
1.12410593237749));
#56907=CARTESIAN_POINT('Ctrl Pts',(-25.7010992092837,0.568703795602993,
1.43565111040708));
#56908=CARTESIAN_POINT('Ctrl Pts',(-25.674584666878,0.0263877965697636,
1.54396301838436));
#56909=CARTESIAN_POINT('Ctrl Pts',(-25.6480701244723,-0.436932738826931,
1.39928967911267));
#56910=CARTESIAN_POINT('Ctrl Pts',(-25.6215555820666,-0.900253274223638,
1.25461633984098));
#56911=CARTESIAN_POINT('Ctrl Pts',(-25.5950410396609,-1.28457834598382,
0.856957753320337));
#56912=CARTESIAN_POINT('Ctrl Pts',(-25.5685264972552,-1.41337212749903,
0.388974361030265));
#56913=CARTESIAN_POINT('Ctrl Pts',(-25.5614026801177,-1.44797590583016,
0.263238526745882));
#56914=CARTESIAN_POINT('Ctrl Pts',(-25.5542788629803,-1.46413372082814,
0.132426176049788));
#56915=CARTESIAN_POINT('Ctrl Pts',(-25.5471550458428,-1.462974653714,0.00133299795035805));
#56916=CARTESIAN_POINT('Origin',(-17.3,0.,0.));
#56917=CARTESIAN_POINT('',(-24.9758449541571,-1.46110128969025,-0.00020250645966946));
#56918=CARTESIAN_POINT('',(-25.0471550458428,-1.4611947376406,-0.000434366747377157));
#56919=CARTESIAN_POINT('',(-17.3,-1.4635,-1.79227059055215E-16));
#56920=CARTESIAN_POINT('Ctrl Pts',(-24.9758449541571,-1.46110128969025,
-0.00020250645966946));
#56921=CARTESIAN_POINT('Ctrl Pts',(-24.9897672000123,-1.4607849998905,0.256823176151405));
#56922=CARTESIAN_POINT('Ctrl Pts',(-25.0036894458674,-1.39631108339353,
0.513997221673354));
#56923=CARTESIAN_POINT('Ctrl Pts',(-25.0176116917226,-1.26860136025212,
0.734555952384895));
#56924=CARTESIAN_POINT('Ctrl Pts',(-25.0441262341283,-1.02538163082939,
1.15460411697203));
#56925=CARTESIAN_POINT('Ctrl Pts',(-25.070640776534,-0.55280451131479,1.44184788658205));
#56926=CARTESIAN_POINT('Ctrl Pts',(-25.0971553189397,-0.0679435120251727,
1.46434474683774));
#56927=CARTESIAN_POINT('Ctrl Pts',(-25.1236698613453,0.416917487264431,
1.48684160709344));
#56928=CARTESIAN_POINT('Ctrl Pts',(-25.150184403751,0.914062366329063,1.24459155799483));
#56929=CARTESIAN_POINT('Ctrl Pts',(-25.1766989461567,1.1951326634949,0.848869704410039));
#56930=CARTESIAN_POINT('Ctrl Pts',(-25.2032134885624,1.47620296066076,0.45314785082523));
#56931=CARTESIAN_POINT('Ctrl Pts',(-25.2297280309681,1.5411986759278,-0.0960458072457594));
#56932=CARTESIAN_POINT('Ctrl Pts',(-25.2562425733738,1.36026468621463,-0.546444729002872));
#56933=CARTESIAN_POINT('Ctrl Pts',(-25.2827571157795,1.17933069650146,-0.996843650759966));
#56934=CARTESIAN_POINT('Ctrl Pts',(-25.3092716581851,0.752467001808086,
-1.34844783620318));
#56935=CARTESIAN_POINT('Ctrl Pts',(-25.3357862005908,0.275749114061697,
-1.43975146623013));
#56936=CARTESIAN_POINT('Ctrl Pts',(-25.3623007429965,-0.200968773684707,
-1.53105509625708));
#56937=CARTESIAN_POINT('Ctrl Pts',(-25.3888152854022,-0.727540854484134,
-1.36205817086775));
#56938=CARTESIAN_POINT('Ctrl Pts',(-25.4153298278079,-1.06209157978827,
-1.01038771496909));
#56939=CARTESIAN_POINT('Ctrl Pts',(-25.435501536591,-1.31661076781507,-0.74284419430576));
#56940=CARTESIAN_POINT('Ctrl Pts',(-25.455673245374,-1.45999091671316,-0.369572013396846));
#56941=CARTESIAN_POINT('Ctrl Pts',(-25.4758449541571,-1.4634040497188,0.00135246395512149));
#56942=CARTESIAN_POINT('Ctrl Pts',(-25.5471550458428,-1.462974653714,0.00133299795035805));
#56943=CARTESIAN_POINT('Ctrl Pts',(-25.5277643205746,-1.45981972265052,
-0.355497020564954));
#56944=CARTESIAN_POINT('Ctrl Pts',(-25.5083735953064,-1.32836312994779,
-0.714407703616101));
#56945=CARTESIAN_POINT('Ctrl Pts',(-25.4889828700381,-1.09137519147001,
-0.978683818081121));
#56946=CARTESIAN_POINT('Ctrl Pts',(-25.4624683276325,-0.767321982655538,
-1.34005040684294));
#56947=CARTESIAN_POINT('Ctrl Pts',(-25.4359537852268,-0.24595307375636,
-1.52447538630709));
#56948=CARTESIAN_POINT('Ctrl Pts',(-25.4094392428211,0.23324601095786,-1.44724501128948));
#56949=CARTESIAN_POINT('Ctrl Pts',(-25.3829247004154,0.71244509567208,-1.37001463627187));
#56950=CARTESIAN_POINT('Ctrl Pts',(-25.3564101580097,1.14947435620134,-1.0311289067725));
#56951=CARTESIAN_POINT('Ctrl Pts',(-25.329895615604,1.34358883097895,-0.586251548056509));
#56952=CARTESIAN_POINT('Ctrl Pts',(-25.3033810731983,1.53770330575656,-0.141374189340514));
#56953=CARTESIAN_POINT('Ctrl Pts',(-25.2768665307927,1.48890299478252,0.409494798592106));
#56954=CARTESIAN_POINT('Ctrl Pts',(-25.250351988387,1.21960382631541,0.813319329148672));
#56955=CARTESIAN_POINT('Ctrl Pts',(-25.2238374459813,0.950304657848305,
1.21714385970524));
#56956=CARTESIAN_POINT('Ctrl Pts',(-25.1973229035756,0.460506631888131,
1.47392393288575));
#56957=CARTESIAN_POINT('Ctrl Pts',(-25.1708083611699,-0.024806492405043,
1.46571022452073));
#56958=CARTESIAN_POINT('Ctrl Pts',(-25.1442938187642,-0.510119616698223,
1.4574965161557));
#56959=CARTESIAN_POINT('Ctrl Pts',(-25.1177792763586,-0.990947839324403,
1.18428902624514));
#56960=CARTESIAN_POINT('Ctrl Pts',(-25.0912647339529,-1.24642758937672,
0.771582846342876));
#56961=CARTESIAN_POINT('Ctrl Pts',(-25.0765615045829,-1.38809993306417,
0.542723017925664));
#56962=CARTESIAN_POINT('Ctrl Pts',(-25.0618582752128,-1.46047569528562,
0.270966149981189));
#56963=CARTESIAN_POINT('Ctrl Pts',(-25.0471550458428,-1.4611947376406,-0.000434366747377157));
#56964=CARTESIAN_POINT('Origin',(-17.3,0.,0.));
#56965=CARTESIAN_POINT('',(-24.4758449541571,-1.46414968530619,-0.00128056012016223));
#56966=CARTESIAN_POINT('',(-24.5471550458428,-1.46457278513142,-0.00117677452095056));
#56967=CARTESIAN_POINT('',(-17.3,-1.4635,-1.79227059055215E-16));
#56968=CARTESIAN_POINT('Ctrl Pts',(-24.4758449541571,-1.46414968530619,
-0.00128056012016223));
#56969=CARTESIAN_POINT('Ctrl Pts',(-24.4973466122448,-1.46052449486356,
0.393583248871125));
#56970=CARTESIAN_POINT('Ctrl Pts',(-24.5188482703325,-1.29537096979211,
0.791118806776767));
#56971=CARTESIAN_POINT('Ctrl Pts',(-24.5403499284202,-1.01011940717455,
1.06234676149878));
#56972=CARTESIAN_POINT('Ctrl Pts',(-24.5668644708259,-0.658364457744287,
1.39680864707739));
#56973=CARTESIAN_POINT('Ctrl Pts',(-24.5933790132316,-0.123984486640841,
1.53920304146123));
#56974=CARTESIAN_POINT('Ctrl Pts',(-24.6198935556373,0.347558482308701,
1.42412252274616));
#56975=CARTESIAN_POINT('Ctrl Pts',(-24.646408098043,0.819101451258258,1.30904200403109));
#56976=CARTESIAN_POINT('Ctrl Pts',(-24.6729226404487,1.22780741805391,0.936486572217083));
#56977=CARTESIAN_POINT('Ctrl Pts',(-24.6994371828544,1.38594143905111,0.477585789087716));
#56978=CARTESIAN_POINT('Ctrl Pts',(-24.72595172526,1.54407546004832,0.0186850059583487));
#56979=CARTESIAN_POINT('Ctrl Pts',(-24.7524662676657,1.45163753524709,-0.526561128486383));
#56980=CARTESIAN_POINT('Ctrl Pts',(-24.7789808100714,1.15108808855372,-0.907699328416276));
#56981=CARTESIAN_POINT('Ctrl Pts',(-24.8054953524771,0.850538641860351,
-1.28883752834616));
#56982=CARTESIAN_POINT('Ctrl Pts',(-24.8320098948828,0.341877673274856,
-1.50586779376121));
#56983=CARTESIAN_POINT('Ctrl Pts',(-24.8585244372885,-0.141246556522215,
-1.45909947182782));
#56984=CARTESIAN_POINT('Ctrl Pts',(-24.8850389796942,-0.6243707863193,-1.41233114989443));
#56985=CARTESIAN_POINT('Ctrl Pts',(-24.9115535220998,-1.08195827732796,
-1.10176424061258));
#56986=CARTESIAN_POINT('Ctrl Pts',(-24.9380680645055,-1.30382085316685,
-0.670054506189522));
#56987=CARTESIAN_POINT('Ctrl Pts',(-24.950660361056,-1.40918791195588,-0.465026755137965));
#56988=CARTESIAN_POINT('Ctrl Pts',(-24.9632526576066,-1.46138736529873,
-0.232675316536856));
#56989=CARTESIAN_POINT('Ctrl Pts',(-24.9758449541571,-1.46110128969025,
-0.00020250645966946));
#56990=CARTESIAN_POINT('Ctrl Pts',(-25.0471550458428,-1.4611947376406,-0.000434366747377157));
#56991=CARTESIAN_POINT('Ctrl Pts',(-25.0353437328071,-1.46177235457949,
-0.218454257510994));
#56992=CARTESIAN_POINT('Ctrl Pts',(-25.0235324197715,-1.41610890745192,
-0.436244189947807));
#56993=CARTESIAN_POINT('Ctrl Pts',(-25.0117211067358,-1.32298092488054,
-0.631382052906385));
#56994=CARTESIAN_POINT('Ctrl Pts',(-24.9852065643301,-1.11392323285356,
-1.06943590235947));
#56995=CARTESIAN_POINT('Ctrl Pts',(-24.9586920219244,-0.665676571321139,
-1.3933387313717));
#56996=CARTESIAN_POINT('Ctrl Pts',(-24.9321774795187,-0.184138501313287,
-1.45430905816616));
#56997=CARTESIAN_POINT('Ctrl Pts',(-24.9056629371131,0.297399568694545,
-1.51527938496062));
#56998=CARTESIAN_POINT('Ctrl Pts',(-24.8791483947074,0.812229047177795,
-1.31331720953735));
#56999=CARTESIAN_POINT('Ctrl Pts',(-24.8526338523017,1.12386823095177,-0.941191810306153));
#57000=CARTESIAN_POINT('Ctrl Pts',(-24.826119309896,1.43550741472577,-0.569066411074926));
#57001=CARTESIAN_POINT('Ctrl Pts',(-24.7996047674903,1.54395630379045,-0.0267777880357327));
#57002=CARTESIAN_POINT('Ctrl Pts',(-24.7730902250846,1.39940000007497,0.436579275871188));
#57003=CARTESIAN_POINT('Ctrl Pts',(-24.7465756826789,1.2548436963595,0.899936339778083));
#57004=CARTESIAN_POINT('Ctrl Pts',(-24.7200611402733,0.857282199863888,
1.28436184455272));
#57005=CARTESIAN_POINT('Ctrl Pts',(-24.6935465978676,0.389331354748685,
1.41327383069934));
#57006=CARTESIAN_POINT('Ctrl Pts',(-24.6670320554619,-0.0786194903665382,
1.54218581684597));
#57007=CARTESIAN_POINT('Ctrl Pts',(-24.6405175130562,-0.616959684101348,
1.41558428436456));
#57008=CARTESIAN_POINT('Ctrl Pts',(-24.6140029706505,-0.978408114499494,
1.09162236410381));
#57009=CARTESIAN_POINT('Ctrl Pts',(-24.5917203290479,-1.28216692387813,
0.819366963591972));
#57010=CARTESIAN_POINT('Ctrl Pts',(-24.5694376874454,-1.4609940220446,0.407723665612911));
#57011=CARTESIAN_POINT('Ctrl Pts',(-24.5471550458428,-1.46457278513142,
-0.00117677452095056));
#57012=CARTESIAN_POINT('Origin',(-17.3,0.,0.));
#57013=CARTESIAN_POINT('',(-23.9758449541571,-1.46535571869621,0.000815875462887895));
#57014=CARTESIAN_POINT('',(-24.0471550458428,-1.46501532673864,0.00100720506673913));
#57015=CARTESIAN_POINT('',(-17.3,-1.4635,-1.79227059055215E-16));
#57016=CARTESIAN_POINT('Ctrl Pts',(-23.9758449541571,-1.46535571869621,
0.000815875462887895));
#57017=CARTESIAN_POINT('Ctrl Pts',(-23.9784114820717,-1.46566979594398,
0.0478475604868917));
#57018=CARTESIAN_POINT('Ctrl Pts',(-23.9809780099863,-1.46360259269125,
0.0948512818988251));
#57019=CARTESIAN_POINT('Ctrl Pts',(-23.9835445379008,-1.45906374756695,
0.141615108493016));
#57020=CARTESIAN_POINT('Ctrl Pts',(-24.0100590803065,-1.41217339393492,
0.624727509585923));
#57021=CARTESIAN_POINT('Ctrl Pts',(-24.0365736227122,-1.10149091173927,
1.08223653936045));
#57022=CARTESIAN_POINT('Ctrl Pts',(-24.0630881651179,-0.669725150433888,
1.30399006180796));
#57023=CARTESIAN_POINT('Ctrl Pts',(-24.0896027075236,-0.237959389128517,
1.52574358425545));
#57024=CARTESIAN_POINT('Ctrl Pts',(-24.1161172499293,0.314889651286583,
1.51174159937593));
#57025=CARTESIAN_POINT('Ctrl Pts',(-24.142631792335,0.734876367178585,1.26841577701478));
#57026=CARTESIAN_POINT('Ctrl Pts',(-24.1691463347406,1.1548630830706,1.02508995465363));
#57027=CARTESIAN_POINT('Ctrl Pts',(-24.1956608771463,1.44198747443951,0.552440294810826));
#57028=CARTESIAN_POINT('Ctrl Pts',(-24.222175419552,1.46436186209328,0.0675736284677887));
#57029=CARTESIAN_POINT('Ctrl Pts',(-24.2486899619577,1.48673624974706,-0.417293037875236));
#57030=CARTESIAN_POINT('Ctrl Pts',(-24.2752045043634,1.24436063368571,-0.914376710718497));
#57031=CARTESIAN_POINT('Ctrl Pts',(-24.3017190467691,0.848567796689088,
-1.19534704284565));
#57032=CARTESIAN_POINT('Ctrl Pts',(-24.3282335891748,0.452774959692452,
-1.47631737497281));
#57033=CARTESIAN_POINT('Ctrl Pts',(-24.3547481315804,-0.0964350982394741,
-1.54117436638384));
#57034=CARTESIAN_POINT('Ctrl Pts',(-24.3812626739861,-0.546788303196699,
-1.36012661539464));
#57035=CARTESIAN_POINT('Ctrl Pts',(-24.4077772163918,-0.997141508153911,
-1.17907886440544));
#57036=CARTESIAN_POINT('Ctrl Pts',(-24.4342917587975,-1.34863786013643,
-0.752126371016021));
#57037=CARTESIAN_POINT('Ctrl Pts',(-24.4608063012032,-1.43982107224915,
-0.275385435934625));
#57038=CARTESIAN_POINT('Ctrl Pts',(-24.4658191855211,-1.45706032484753,
-0.185251986877209));
#57039=CARTESIAN_POINT('Ctrl Pts',(-24.4708320698391,-1.46499486014087,
-0.093338883610889));
#57040=CARTESIAN_POINT('Ctrl Pts',(-24.4758449541571,-1.46414968530619,
-0.00128056012016223));
#57041=CARTESIAN_POINT('Ctrl Pts',(-24.5471550458428,-1.46457278513142,
-0.00117677452095056));
#57042=CARTESIAN_POINT('Ctrl Pts',(-24.5429231450397,-1.46525246084723,
-0.0788348068074314));
#57043=CARTESIAN_POINT('Ctrl Pts',(-24.5386912442366,-1.45961105333077,
-0.156393906155542));
#57044=CARTESIAN_POINT('Ctrl Pts',(-24.5344593434335,-1.44730388113662,
-0.232880441379075));
#57045=CARTESIAN_POINT('Ctrl Pts',(-24.5079448010278,-1.37019455031415,
-0.71209901856115));
#57046=CARTESIAN_POINT('Ctrl Pts',(-24.4814302586221,-1.03141922160774,
-1.14921386488522));
#57047=CARTESIAN_POINT('Ctrl Pts',(-24.4549157162164,-0.586590908797168,
-1.34344070581718));
#57048=CARTESIAN_POINT('Ctrl Pts',(-24.4284011738107,-0.141762595986587,
-1.53766754674914));
#57049=CARTESIAN_POINT('Ctrl Pts',(-24.401886631405,0.409118700928145,-1.48900638228895));
#57050=CARTESIAN_POINT('Ctrl Pts',(-24.3753720889993,0.813011241348171,
-1.21980922515431));
#57051=CARTESIAN_POINT('Ctrl Pts',(-24.3488575465936,1.2169037817682,-0.950612068019661));
#57052=CARTESIAN_POINT('Ctrl Pts',(-24.322343004188,1.4738075656935,-0.460878918210565));
#57053=CARTESIAN_POINT('Ctrl Pts',(-24.2958284617823,1.46571644367779,0.0244362653153989));
#57054=CARTESIAN_POINT('Ctrl Pts',(-24.2693139193766,1.45762532166208,0.509751448841349));
#57055=CARTESIAN_POINT('Ctrl Pts',(-24.2427993769709,1.18453929370534,0.9906486660842));
#57056=CARTESIAN_POINT('Ctrl Pts',(-24.2162848345652,0.771897659043956,
1.24623265415913));
#57057=CARTESIAN_POINT('Ctrl Pts',(-24.1897702921595,0.359256024382572,
1.50181664223405));
#57058=CARTESIAN_POINT('Ctrl Pts',(-24.1632557497538,-0.192941216983452,
1.5320874011411));
#57059=CARTESIAN_POINT('Ctrl Pts',(-24.1367412073481,-0.631047858708569,
1.32314036456809));
#57060=CARTESIAN_POINT('Ctrl Pts',(-24.1102266649425,-1.06915450043368,
1.11419332799508));
#57061=CARTESIAN_POINT('Ctrl Pts',(-24.0837121225368,-1.39317054251788,
0.666028495942013));
#57062=CARTESIAN_POINT('Ctrl Pts',(-24.0571975801311,-1.45426249990707,
0.184505841896889));
#57063=CARTESIAN_POINT('Ctrl Pts',(-24.0538500687017,-1.46197547577055,
0.12371269060351));
#57064=CARTESIAN_POINT('Ctrl Pts',(-24.0505025572722,-1.46549756189357,
0.0623878308737869));
#57065=CARTESIAN_POINT('Ctrl Pts',(-24.0471550458428,-1.46501532673864,
0.00100720506673913));
#57066=CARTESIAN_POINT('Origin',(-17.3,0.,0.));
#57067=CARTESIAN_POINT('',(-23.4758449541571,-1.4616124403278,0.000876453398841459));
#57068=CARTESIAN_POINT('',(-23.5471550458428,-1.46138107708475,0.000680708301427907));
#57069=CARTESIAN_POINT('',(-17.3,-1.4635,-1.79227059055215E-16));
#57070=CARTESIAN_POINT('Ctrl Pts',(-23.4758449541571,-1.4616124403278,0.000876453398841459));
#57071=CARTESIAN_POINT('Ctrl Pts',(-23.4859908943042,-1.46263037628344,
0.188022186505176));
#57072=CARTESIAN_POINT('Ctrl Pts',(-23.4961368344513,-1.4293109343094,0.374819137226617));
#57073=CARTESIAN_POINT('Ctrl Pts',(-23.5062827745985,-1.35998845779505,
0.547131842504017));
#57074=CARTESIAN_POINT('Ctrl Pts',(-23.5327973170041,-1.17882695708114,
0.997439301927659));
#57075=CARTESIAN_POINT('Ctrl Pts',(-23.5593118594098,-0.751785692236323,
1.3488277980231));
#57076=CARTESIAN_POINT('Ctrl Pts',(-23.5858264018155,-0.275021740237209,
1.43989058640388));
#57077=CARTESIAN_POINT('Ctrl Pts',(-23.6123409442212,0.201742211761891,
1.53095337478465));
#57078=CARTESIAN_POINT('Ctrl Pts',(-23.6388554866269,0.728228850915275,
1.36169045545076));
#57079=CARTESIAN_POINT('Ctrl Pts',(-23.6653700290326,1.06260187542882,1.00985103493177));
#57080=CARTESIAN_POINT('Ctrl Pts',(-23.6918845714383,1.39697489994238,0.658011614412757));
#57081=CARTESIAN_POINT('Ctrl Pts',(-23.718399113844,1.53923430981608,0.123595692708635));
#57082=CARTESIAN_POINT('Ctrl Pts',(-23.7449136562497,1.42403468691244,-0.34791819280944));
#57083=CARTESIAN_POINT('Ctrl Pts',(-23.7714281986553,1.30883506400881,-0.819432078327503));
#57084=CARTESIAN_POINT('Ctrl Pts',(-23.797942741061,0.936176408327837,-1.22804392765955));
#57085=CARTESIAN_POINT('Ctrl Pts',(-23.8244572834667,0.477235696490234,
-1.38606202906403));
#57086=CARTESIAN_POINT('Ctrl Pts',(-23.8509718258724,0.0182949846526319,
-1.54408013046851));
#57087=CARTESIAN_POINT('Ctrl Pts',(-23.8774863682781,-0.526927783341603,
-1.45150448394547));
#57088=CARTESIAN_POINT('Ctrl Pts',(-23.9040009106838,-0.90799005480451,
-1.15085877447831));
#57089=CARTESIAN_POINT('Ctrl Pts',(-23.9279489251749,-1.25216664512165,
-0.879314664953531));
#57090=CARTESIAN_POINT('Ctrl Pts',(-23.951896939666,-1.46242509540613,-0.438032059172249));
#57091=CARTESIAN_POINT('Ctrl Pts',(-23.9758449541571,-1.46535571869621,
0.000815875462887895));
#57092=CARTESIAN_POINT('Ctrl Pts',(-24.0471550458428,-1.46501532673864,
0.00100720506673913));
#57093=CARTESIAN_POINT('Ctrl Pts',(-24.0239880148665,-1.46167793506498,
-0.423788016516127));
#57094=CARTESIAN_POINT('Ctrl Pts',(-24.0008209838903,-1.26655073000452,
-0.85125419400408));
#57095=CARTESIAN_POINT('Ctrl Pts',(-23.977653952914,-0.941475660114631,
-1.12363045782044));
#57096=CARTESIAN_POINT('Ctrl Pts',(-23.9511394105083,-0.569428990238878,
-1.43536362745538));
#57097=CARTESIAN_POINT('Ctrl Pts',(-23.9246248681026,-0.0271677777932092,
-1.54394949068812));
#57098=CARTESIAN_POINT('Ctrl Pts',(-23.898110325697,0.436225785060499,-1.39951023175195));
#57099=CARTESIAN_POINT('Ctrl Pts',(-23.8715957832913,0.899619347914234,
-1.25507097281577));
#57100=CARTESIAN_POINT('Ctrl Pts',(-23.8450812408856,1.28414526117601,-0.85760659171064));
#57101=CARTESIAN_POINT('Ctrl Pts',(-23.8185666984799,1.41317544372912,-0.389688323626757));
#57102=CARTESIAN_POINT('Ctrl Pts',(-23.7920521560742,1.54220562628224,0.0782299444571254));
#57103=CARTESIAN_POINT('Ctrl Pts',(-23.7655376136685,1.4157400781267,0.61660209951974));
#57104=CARTESIAN_POINT('Ctrl Pts',(-23.7390230712628,1.0918694670893,0.978132348492866));
#57105=CARTESIAN_POINT('Ctrl Pts',(-23.7125085288571,0.767998856051899,
1.33966259746599));
#57106=CARTESIAN_POINT('Ctrl Pts',(-23.6859939864515,0.246723182132623,
1.5243509403496));
#57107=CARTESIAN_POINT('Ctrl Pts',(-23.6594794440458,-0.232514856941934,
1.44736265864203));
#57108=CARTESIAN_POINT('Ctrl Pts',(-23.6329649016401,-0.711752896016477,
1.37037437693446));
#57109=CARTESIAN_POINT('Ctrl Pts',(-23.6064503592344,-1.14895330024632,
1.03170947063572));
#57110=CARTESIAN_POINT('Ctrl Pts',(-23.5799358168287,-1.34329249494042,
0.586930232111769));
#57111=CARTESIAN_POINT('Ctrl Pts',(-23.5690088931667,-1.42338173474176,
0.403631998583174));
#57112=CARTESIAN_POINT('Ctrl Pts',(-23.5580819695048,-1.4622246078077,0.202311822928828));
#57113=CARTESIAN_POINT('Ctrl Pts',(-23.5471550458428,-1.46138107708475,
0.000680708301427907));
#57114=CARTESIAN_POINT('Origin',(-17.3,0.,0.));
#57115=CARTESIAN_POINT('',(-22.9758449541571,-1.46214569129651,-0.00114913864106017));
#57116=CARTESIAN_POINT('',(-23.0471550458428,-1.4625153155714,-0.00125827208086059));
#57117=CARTESIAN_POINT('',(-17.3,-1.4635,-1.79227059055215E-16));
#57118=CARTESIAN_POINT('Ctrl Pts',(-22.9758449541571,-1.46214569129651,
-0.00114913864106017));
#57119=CARTESIAN_POINT('Ctrl Pts',(-22.9935703065368,-1.45975965690007,
0.32550238069992));
#57120=CARTESIAN_POINT('Ctrl Pts',(-23.0112956589164,-1.35167970161975,
0.653585897788354));
#57121=CARTESIAN_POINT('Ctrl Pts',(-23.0290210112961,-1.15062938697513,
0.908280723260628));
#57122=CARTESIAN_POINT('Ctrl Pts',(-23.0555355537018,-0.849887433916146,
1.28926704194381));
#57123=CARTESIAN_POINT('Ctrl Pts',(-23.0820500961075,-0.341116890136462,
1.506040312553));
#57124=CARTESIAN_POINT('Ctrl Pts',(-23.1085646385132,0.141983651428446,
1.45902793021404));
#57125=CARTESIAN_POINT('Ctrl Pts',(-23.1350791809189,0.625084192993341,
1.41201554787508));
#57126=CARTESIAN_POINT('Ctrl Pts',(-23.1615937233246,1.08251473234346,1.10121751258798));
#57127=CARTESIAN_POINT('Ctrl Pts',(-23.1881082657302,1.30415918725112,0.669395751948055));
#57128=CARTESIAN_POINT('Ctrl Pts',(-23.2146228081359,1.52580364215879,0.237573991308118));
#57129=CARTESIAN_POINT('Ctrl Pts',(-23.2411373505416,1.51166201262399,-0.315271494684653));
#57130=CARTESIAN_POINT('Ctrl Pts',(-23.2676518929473,1.26823011284921,-0.735196735085295));
#57131=CARTESIAN_POINT('Ctrl Pts',(-23.294166435353,1.02479821307445,-1.15512197548593));
#57132=CARTESIAN_POINT('Ctrl Pts',(-23.3206809777587,0.552076043059725,
-1.44212697029443));
#57133=CARTESIAN_POINT('Ctrl Pts',(-23.3471955201643,0.0672037405990306,
-1.46437888391874));
#57134=CARTESIAN_POINT('Ctrl Pts',(-23.37371006257,-0.417668561861677,-1.48663079754305));
#57135=CARTESIAN_POINT('Ctrl Pts',(-23.4002246049757,-0.914690996768357,
-1.24412962998315));
#57136=CARTESIAN_POINT('Ctrl Pts',(-23.4267391473814,-1.19556134593018,
-0.848265834827282));
#57137=CARTESIAN_POINT('Ctrl Pts',(-23.44310774964,-1.36895506177522,-0.603881567796481));
#57138=CARTESIAN_POINT('Ctrl Pts',(-23.4594763518985,-1.45997018849692,
-0.301048654100674));
#57139=CARTESIAN_POINT('Ctrl Pts',(-23.4758449541571,-1.4616124403278,0.000876453398841459));
#57140=CARTESIAN_POINT('Ctrl Pts',(-23.5471550458428,-1.46138107708475,
0.000680708301427907));
#57141=CARTESIAN_POINT('Ctrl Pts',(-23.5315674270991,-1.46017775255219,
-0.286952759169412));
#57142=CARTESIAN_POINT('Ctrl Pts',(-23.5159798083554,-1.37821272310039,
-0.575218986457016));
#57143=CARTESIAN_POINT('Ctrl Pts',(-23.5003921896117,-1.2200145461662,-0.812703101675466));
#57144=CARTESIAN_POINT('Ctrl Pts',(-23.473877647206,-0.950919417539503,
-1.21666362618954));
#57145=CARTESIAN_POINT('Ctrl Pts',(-23.4473631048003,-0.461251175127714,
-1.47369110446852));
#57146=CARTESIAN_POINT('Ctrl Pts',(-23.4208485623946,0.0240660366666584,
-1.46572256931836));
#57147=CARTESIAN_POINT('Ctrl Pts',(-23.3943340199889,0.509383248461031,
-1.45775403416819));
#57148=CARTESIAN_POINT('Ctrl Pts',(-23.3678194775832,0.990349429638006,
-1.1847894855889));
#57149=CARTESIAN_POINT('Ctrl Pts',(-23.3413049351775,1.24603763942864,-0.772212422496003));
#57150=CARTESIAN_POINT('Ctrl Pts',(-23.3147903927719,1.50172584921927,-0.3596353594031));
#57151=CARTESIAN_POINT('Ctrl Pts',(-23.2882758503662,1.53213608762356,0.192554218203404));
#57152=CARTESIAN_POINT('Ctrl Pts',(-23.2617613079605,1.32329971983588,0.630713624248227));
#57153=CARTESIAN_POINT('Ctrl Pts',(-23.2352467655548,1.11446335204819,1.06887303029306));
#57154=CARTESIAN_POINT('Ctrl Pts',(-23.2087322231491,0.666380378068528,
1.39300226477619));
#57155=CARTESIAN_POINT('Ctrl Pts',(-23.1822176807434,0.184873170708501,
1.45421584886227));
#57156=CARTESIAN_POINT('Ctrl Pts',(-23.1557031383377,-0.296634036651499,
1.51542943294835));
#57157=CARTESIAN_POINT('Ctrl Pts',(-23.1291885959321,-0.811565477391885,
1.31372736663739));
#57158=CARTESIAN_POINT('Ctrl Pts',(-23.1026740535264,-1.12339261299846,
0.941759449854651));
#57159=CARTESIAN_POINT('Ctrl Pts',(-23.0841677176319,-1.34103837222996,
0.682137273290514));
#57160=CARTESIAN_POINT('Ctrl Pts',(-23.0656613817373,-1.45973961344624,
0.339568196618657));
#57161=CARTESIAN_POINT('Ctrl Pts',(-23.0471550458428,-1.4625153155714,-0.00125827208086059));
#57162=CARTESIAN_POINT('Origin',(-17.3,0.,0.));
#57163=CARTESIAN_POINT('',(-22.4758449541571,-1.46578197197304,-0.000409560824215643));
#57164=CARTESIAN_POINT('',(-22.5471550458428,-1.46590183802103,-0.000147589276300086));
#57165=CARTESIAN_POINT('',(-17.3,-1.4635,-1.79227059055215E-16));
#57166=CARTESIAN_POINT('Ctrl Pts',(-22.4758449541571,-1.46578197197304,
-0.000409560824215643));
#57167=CARTESIAN_POINT('Ctrl Pts',(-22.5011497187693,-1.46406545630175,
0.462943637033072));
#57168=CARTESIAN_POINT('Ctrl Pts',(-22.5264544833815,-1.225833251475,0.927815920084082));
#57169=CARTESIAN_POINT('Ctrl Pts',(-22.5517592479938,-0.847963818843918,
1.1957755727348));
#57170=CARTESIAN_POINT('Ctrl Pts',(-22.5782737903995,-0.452029090785964,
1.47654592101102));
#57171=CARTESIAN_POINT('Ctrl Pts',(-22.6047883328051,0.0972136617436899,
1.54112545230473));
#57172=CARTESIAN_POINT('Ctrl Pts',(-22.6313028752108,0.547475346902943,
1.35985021342467));
#57173=CARTESIAN_POINT('Ctrl Pts',(-22.6578174176165,0.997737032062196,
1.1785749745446));
#57174=CARTESIAN_POINT('Ctrl Pts',(-22.6843319600222,1.34901764985106,0.751444965490751));
#57175=CARTESIAN_POINT('Ctrl Pts',(-22.7108465024279,1.43996000868985,0.274658026992733));
#57176=CARTESIAN_POINT('Ctrl Pts',(-22.7373610448335,1.53090236752864,-0.202128911505298));
#57177=CARTESIAN_POINT('Ctrl Pts',(-22.7638755872392,1.36150646741735,-0.728572779447481));
#57178=CARTESIAN_POINT('Ctrl Pts',(-22.7903901296449,1.00958259825787,-1.06285692156211));
#57179=CARTESIAN_POINT('Ctrl Pts',(-22.8169046720506,0.657658729098401,
-1.39714106367674));
#57180=CARTESIAN_POINT('Ctrl Pts',(-22.8434192144563,0.123206890890731,
-1.53926547996378));
#57181=CARTESIAN_POINT('Ctrl Pts',(-22.869933756862,-0.348277881112059,
-1.42394676022164));
#57182=CARTESIAN_POINT('Ctrl Pts',(-22.8964482992677,-0.819762653114848,
-1.3086280404795));
#57183=CARTESIAN_POINT('Ctrl Pts',(-22.9229628416734,-1.22828035891277,
-0.935866184708164));
#57184=CARTESIAN_POINT('Ctrl Pts',(-22.9494773840791,-1.38618253064258,
-0.47688557344392));
#57185=CARTESIAN_POINT('Ctrl Pts',(-22.9582665741051,-1.43852483290143,
-0.324740092336465));
#57186=CARTESIAN_POINT('Ctrl Pts',(-22.9670557641311,-1.46332881641976,
-0.163120659109465));
#57187=CARTESIAN_POINT('Ctrl Pts',(-22.9758449541571,-1.46214569129651,
-0.00114913864106017));
#57188=CARTESIAN_POINT('Ctrl Pts',(-23.0471550458428,-1.4625153155714,-0.00125827208086059));
#57189=CARTESIAN_POINT('Ctrl Pts',(-23.0391468393317,-1.4637164391195,-0.148743369151091));
#57190=CARTESIAN_POINT('Ctrl Pts',(-23.0311386328205,-1.44321011457532,
-0.295902157002481));
#57191=CARTESIAN_POINT('Ctrl Pts',(-23.0231304263093,-1.39962037413654,
-0.435872266417514));
#57192=CARTESIAN_POINT('Ctrl Pts',(-22.9966158839036,-1.25529816919524,
-0.899302298652362));
#57193=CARTESIAN_POINT('Ctrl Pts',(-22.9701013414979,-0.857930928839858,
-1.28392859586752));
#57194=CARTESIAN_POINT('Ctrl Pts',(-22.9435867990922,-0.390045267641704,
-1.41307696659466));
#57195=CARTESIAN_POINT('Ctrl Pts',(-22.9170722566866,0.0778403935564494,
-1.5422253373218));
#57196=CARTESIAN_POINT('Ctrl Pts',(-22.8905577142809,0.616244475597355,
-1.41589578156095));
#57197=CARTESIAN_POINT('Ctrl Pts',(-22.8640431718752,0.977856520078891,
-1.09211650041067));
#57198=CARTESIAN_POINT('Ctrl Pts',(-22.8375286294695,1.33946856456042,-0.768337219260394));
#57199=CARTESIAN_POINT('Ctrl Pts',(-22.8110140870638,1.52428857148255,-0.247108212720685));
#57200=CARTESIAN_POINT('Ctrl Pts',(-22.7844995446581,1.44742134380195,0.232149257669704));
#57201=CARTESIAN_POINT('Ctrl Pts',(-22.7579850022524,1.37055411612135,0.711406728060106));
#57202=CARTESIAN_POINT('Ctrl Pts',(-22.7314704598468,1.03199965383798,1.14869266230121));
#57203=CARTESIAN_POINT('Ctrl Pts',(-22.7049559174411,0.587269517978703,
1.34314419835813));
#57204=CARTESIAN_POINT('Ctrl Pts',(-22.6784413750354,0.142539382119435,
1.53759573441505));
#57205=CARTESIAN_POINT('Ctrl Pts',(-22.6519268326297,-0.408366427315716,
1.48921287228782));
#57206=CARTESIAN_POINT('Ctrl Pts',(-22.625412290224,-0.812394910150128,
1.22021978933805));
#57207=CARTESIAN_POINT('Ctrl Pts',(-22.599326542097,-1.2098894276161,0.95557687367356));
#57208=CARTESIAN_POINT('Ctrl Pts',(-22.5732407939699,-1.46521881735637,
0.477401475176739));
#57209=CARTESIAN_POINT('Ctrl Pts',(-22.5471550458428,-1.46590183802103,
-0.000147589276300086));
#57210=CARTESIAN_POINT('Origin',(-17.3,0.,0.));
#57211=CARTESIAN_POINT('',(-21.9758449541571,-1.46338908451446,0.00135254369621918));
#57212=CARTESIAN_POINT('',(-22.0471550458428,-1.46296023813343,0.0013315397042942));
#57213=CARTESIAN_POINT('',(-17.3,-1.4635,-1.79227059055215E-16));
#57214=CARTESIAN_POINT('Ctrl Pts',(-21.9758449541571,-1.46338908451446,
0.00135254369621918));
#57215=CARTESIAN_POINT('Ctrl Pts',(-21.9822145885962,-1.46446593650969,
0.118482680034951));
#57216=CARTESIAN_POINT('Ctrl Pts',(-21.9885842230352,-1.45159056750017,
0.235378945131374));
#57217=CARTESIAN_POINT('Ctrl Pts',(-21.9949538574743,-1.42385874267934,
0.348637547193684));
#57218=CARTESIAN_POINT('Ctrl Pts',(-22.02146839988,-1.3084209334563,0.820093175599227));
#57219=CARTESIAN_POINT('Ctrl Pts',(-22.0479829422857,-0.935555901377785,
1.22851671179854));
#57220=CARTESIAN_POINT('Ctrl Pts',(-22.0744974846914,-0.476535419971068,
1.3863029437791));
#57221=CARTESIAN_POINT('Ctrl Pts',(-22.1010120270971,-0.017514938564339,
1.54408917575967));
#57222=CARTESIAN_POINT('Ctrl Pts',(-22.1275265695028,0.527660992170594,
1.45123810352149));
#57223=CARTESIAN_POINT('Ctrl Pts',(-22.1540411119085,0.908571333766114,
1.15039992605879));
#57224=CARTESIAN_POINT('Ctrl Pts',(-22.1805556543141,1.28948167536163,0.849561748596095));
#57225=CARTESIAN_POINT('Ctrl Pts',(-22.2070701967198,1.50612642781774,0.340736465908889));
#57226=CARTESIAN_POINT('Ctrl Pts',(-22.2335847391255,1.45899201977136,-0.142352185304953));
#57227=CARTESIAN_POINT('Ctrl Pts',(-22.2600992815312,1.41185761172498,-0.625440836518782));
#57228=CARTESIAN_POINT('Ctrl Pts',(-22.2866138239369,1.10094404317614,-1.08279285625925));
#57229=CARTESIAN_POINT('Ctrl Pts',(-22.3131283663426,0.669066310753002,
-1.30432822948558));
#57230=CARTESIAN_POINT('Ctrl Pts',(-22.3396429087483,0.237188578329877,
-1.5258636027119));
#57231=CARTESIAN_POINT('Ctrl Pts',(-22.3661574511539,-0.315653317967536,
-1.51158232942409));
#57232=CARTESIAN_POINT('Ctrl Pts',(-22.3926719935596,-0.735517056084479,
-1.26804436776732));
#57233=CARTESIAN_POINT('Ctrl Pts',(-22.4191865359653,-1.15538079420146,
-1.02450640611054));
#57234=CARTESIAN_POINT('Ctrl Pts',(-22.445701078371,-1.44226637413794,-0.551711756084745));
#57235=CARTESIAN_POINT('Ctrl Pts',(-22.4722156207767,-1.46439581231304,
-0.0668338484424606));
#57236=CARTESIAN_POINT('Ctrl Pts',(-22.4734253985702,-1.46540551115968,
-0.0447103466963747));
#57237=CARTESIAN_POINT('Ctrl Pts',(-22.4746351763636,-1.46586403567025,
-0.0225616897963809));
#57238=CARTESIAN_POINT('Ctrl Pts',(-22.4758449541571,-1.46578197197304,
-0.000409560824215643));
#57239=CARTESIAN_POINT('Ctrl Pts',(-22.5471550458428,-1.46590183802103,
-0.000147589276300086));
#57240=CARTESIAN_POINT('Ctrl Pts',(-22.5467262515642,-1.46591306542964,
-0.00799748131699719));
#57241=CARTESIAN_POINT('Ctrl Pts',(-22.5462974572856,-1.46585548643462,
-0.0158472041198875));
#57242=CARTESIAN_POINT('Ctrl Pts',(-22.5458686630069,-1.46572860144202,
-0.023695806482401));
#57243=CARTESIAN_POINT('Ctrl Pts',(-22.5193541206012,-1.45788265366583,
-0.509015015580697));
#57244=CARTESIAN_POINT('Ctrl Pts',(-22.4928395781956,-1.18503960187983,
-0.990050130004957));
#57245=CARTESIAN_POINT('Ctrl Pts',(-22.4663250357899,-0.772527136678897,
-1.24584254519772));
#57246=CARTESIAN_POINT('Ctrl Pts',(-22.4398104933842,-0.360014671477961,
-1.50163496039049));
#57247=CARTESIAN_POINT('Ctrl Pts',(-22.4132959509785,0.1921672071379,-1.53218467635176));
#57248=CARTESIAN_POINT('Ctrl Pts',(-22.3867814085728,0.630379349546724,
-1.32345899067372));
#57249=CARTESIAN_POINT('Ctrl Pts',(-22.3602668661672,1.06859149195557,-1.11473330499566));
#57250=CARTESIAN_POINT('Ctrl Pts',(-22.3337523237614,1.39283389815735,-0.666732217678252));
#57251=CARTESIAN_POINT('Ctrl Pts',(-22.3072377813558,1.45416910503474,-0.185240487724726));
#57252=CARTESIAN_POINT('Ctrl Pts',(-22.2807232389501,1.51550431191213,0.296251242228773));
#57253=CARTESIAN_POINT('Ctrl Pts',(-22.2542086965444,1.31393231946513,0.811233614818408));
#57254=CARTESIAN_POINT('Ctrl Pts',(-22.2276941541387,0.942043179507886,
1.12315469650121));
#57255=CARTESIAN_POINT('Ctrl Pts',(-22.201179611733,0.570154039550644,1.435075778184));
#57256=CARTESIAN_POINT('Ctrl Pts',(-22.1746650693273,0.0279477520831708,
1.54393556896));
#57257=CARTESIAN_POINT('Ctrl Pts',(-22.1481505269216,-0.43551871996475,
1.39973042722172));
#57258=CARTESIAN_POINT('Ctrl Pts',(-22.121635984516,-0.898985192012657,
1.25552528548345));
#57259=CARTESIAN_POINT('Ctrl Pts',(-22.0951214421103,-1.283711848641,0.858255211230917));
#57260=CARTESIAN_POINT('Ctrl Pts',(-22.0686068997046,-1.41297839930219,
0.390402186770835));
#57261=CARTESIAN_POINT('Ctrl Pts',(-22.0614562817507,-1.44783986150876,
0.264228474801143));
#57262=CARTESIAN_POINT('Ctrl Pts',(-22.0543056637967,-1.46412148390715,
0.132921202336442));
#57263=CARTESIAN_POINT('Ctrl Pts',(-22.0471550458428,-1.46296023813343,
0.0013315397042942));
#57264=CARTESIAN_POINT('Origin',(-17.3,0.,0.));
#57265=CARTESIAN_POINT('',(-21.4758449541571,-1.46110336159793,-0.000210604951717125));
#57266=CARTESIAN_POINT('',(-21.5471550458428,-1.46119914789583,-0.000442129891295945));
#57267=CARTESIAN_POINT('',(-17.3,-1.4635,-1.79227059055215E-16));
#57268=CARTESIAN_POINT('Ctrl Pts',(-21.4758449541571,-1.46110336159793,
-0.000210604951717125));
#57269=CARTESIAN_POINT('Ctrl Pts',(-21.4897940008287,-1.46077376388658,
0.25730895082503));
#57270=CARTESIAN_POINT('Ctrl Pts',(-21.5037430475004,-1.39603731955723,
0.514983410928407));
#57271=CARTESIAN_POINT('Ctrl Pts',(-21.517692094172,-1.26785854178086,0.735837330155876));
#57272=CARTESIAN_POINT('Ctrl Pts',(-21.5442066365777,-1.0242145337804,1.15563953920073));
#57273=CARTESIAN_POINT('Ctrl Pts',(-21.5707211789834,-0.551347433909141,
1.44240568596109));
#57274=CARTESIAN_POINT('Ctrl Pts',(-21.597235721389,-0.0664639520217993,
1.4644126472751));
#57275=CARTESIAN_POINT('Ctrl Pts',(-21.6237502637947,0.418419529865584,
1.4864196085891));
#57276=CARTESIAN_POINT('Ctrl Pts',(-21.6502648062004,0.915319393769039,
1.24366738445671));
#57277=CARTESIAN_POINT('Ctrl Pts',(-21.6767793486061,1.19598972324583,0.847661748758301));
#57278=CARTESIAN_POINT('Ctrl Pts',(-21.7032938910118,1.47666005272259,0.451656113059926));
#57279=CARTESIAN_POINT('Ctrl Pts',(-21.7298084334175,1.54110084777271,-0.097602934204468));
#57280=CARTESIAN_POINT('Ctrl Pts',(-21.7563229758231,1.35971188229233,-0.547818816371488));
#57281=CARTESIAN_POINT('Ctrl Pts',(-21.7828375182288,1.17832291681194,-0.998034698538546));
#57282=CARTESIAN_POINT('Ctrl Pts',(-21.8093520606345,0.751104190801025,
-1.34920741560824));
#57283=CARTESIAN_POINT('Ctrl Pts',(-21.8358666030402,0.274294296224285,
-1.44002933910266));
#57284=CARTESIAN_POINT('Ctrl Pts',(-21.8623811454459,-0.202515598352415,
-1.53085126259707));
#57285=CARTESIAN_POINT('Ctrl Pts',(-21.8888956878516,-0.728916661494918,
-1.36132239251625));
#57286=CARTESIAN_POINT('Ctrl Pts',(-21.9154102302573,-1.06311189988241,
-1.00931409716997));
#57287=CARTESIAN_POINT('Ctrl Pts',(-21.9355551382239,-1.3170228374044,-0.741869364210416));
#57288=CARTESIAN_POINT('Ctrl Pts',(-21.9557000461905,-1.45998338132298,
-0.369088780563025));
#57289=CARTESIAN_POINT('Ctrl Pts',(-21.9758449541571,-1.46338908451446,
0.00135254369621918));
#57290=CARTESIAN_POINT('Ctrl Pts',(-22.0471550458428,-1.46296023813343,
0.0013315397042942));
#57291=CARTESIAN_POINT('Ctrl Pts',(-22.0277911213911,-1.45981557629061,
-0.355014205832619));
#57292=CARTESIAN_POINT('Ctrl Pts',(-22.0084271969393,-1.32875708300604,
-0.713430803933623));
#57293=CARTESIAN_POINT('Ctrl Pts',(-21.9890632724875,-1.09236346405217,
-0.97758062927514));
#57294=CARTESIAN_POINT('Ctrl Pts',(-21.9625487300818,-0.768675533446972,
-1.33927444619329));
#57295=CARTESIAN_POINT('Ctrl Pts',(-21.9360341876762,-0.24749322754258,
-1.52422610536196));
#57296=CARTESIAN_POINT('Ctrl Pts',(-21.9095196452705,0.23178364358579,-1.44747993661264));
#57297=CARTESIAN_POINT('Ctrl Pts',(-21.8830051028648,0.711060514714174,
-1.37073376786332));
#57298=CARTESIAN_POINT('Ctrl Pts',(-21.8564905604591,1.14843195106653,-1.03228977119599));
#57299=CARTESIAN_POINT('Ctrl Pts',(-21.8299760180534,1.34299581607976,-0.587608766376321));
#57300=CARTESIAN_POINT('Ctrl Pts',(-21.8034614756477,1.53755968109297,-0.142927761556679));
#57301=CARTESIAN_POINT('Ctrl Pts',(-21.7769469332421,1.48931597476708,0.40799025141529));
#57302=CARTESIAN_POINT('Ctrl Pts',(-21.7504323908364,1.22042495465668,0.812086666791963));
#57303=CARTESIAN_POINT('Ctrl Pts',(-21.7239178484307,0.95153393454626,1.21618308216867));
#57304=CARTESIAN_POINT('Ctrl Pts',(-21.697403306025,0.461995600651293,1.47345789995005));
#57305=CARTESIAN_POINT('Ctrl Pts',(-21.6708887636193,-0.0233255747863311,
1.46573454004841));
#57306=CARTESIAN_POINT('Ctrl Pts',(-21.6443742212136,-0.508646750223927,
1.45801118014677));
#57307=CARTESIAN_POINT('Ctrl Pts',(-21.6178596788079,-0.98975076720418,
1.18528964256214));
#57308=CARTESIAN_POINT('Ctrl Pts',(-21.5913451364022,-1.24564737147885,
0.772841801572525));
#57309=CARTESIAN_POINT('Ctrl Pts',(-21.5766151062158,-1.38780953471398,
0.543708330016934));
#57310=CARTESIAN_POINT('Ctrl Pts',(-21.5618850760293,-1.46046579618679,
0.271451043834622));
#57311=CARTESIAN_POINT('Ctrl Pts',(-21.5471550458428,-1.46119914789583,
-0.000442129891295945));
#57312=CARTESIAN_POINT('Origin',(-17.3,0.,0.));
#57313=CARTESIAN_POINT('',(-20.9758449541571,-1.46416452657485,-0.00127774293595062));
#57314=CARTESIAN_POINT('',(-21.0471550458428,-1.46458686986414,-0.00117242835359658));
#57315=CARTESIAN_POINT('',(-17.3,-1.4635,-1.79227059055215E-16));
#57316=CARTESIAN_POINT('Ctrl Pts',(-20.9758449541571,-1.46416452657485,
-0.00127774293595062));
#57317=CARTESIAN_POINT('Ctrl Pts',(-20.9973734130613,-1.46053861299378,
0.394067914350929));
#57318=CARTESIAN_POINT('Ctrl Pts',(-21.0189018719655,-1.29492688262452,
0.792089489186256));
#57319=CARTESIAN_POINT('Ctrl Pts',(-21.0404303308696,-1.00904553168518,
1.06336681037344));
#57320=CARTESIAN_POINT('Ctrl Pts',(-21.0669448732753,-0.656952832611104,
1.39747312371126));
#57321=CARTESIAN_POINT('Ctrl Pts',(-21.093459415681,-0.12242926369691,1.53932752562985));
#57322=CARTESIAN_POINT('Ctrl Pts',(-21.1199739580867,0.348997191031295,
1.42377063429117));
#57323=CARTESIAN_POINT('Ctrl Pts',(-21.1464885004924,0.820423645759539,
1.30821374295248));
#57324=CARTESIAN_POINT('Ctrl Pts',(-21.1730030428981,1.2287529863018,0.935245558356483));
#57325=CARTESIAN_POINT('Ctrl Pts',(-21.1995175853037,1.38642326846593,0.476185236093947));
#57326=CARTESIAN_POINT('Ctrl Pts',(-21.2260321277094,1.54409355063006,0.0171249138314507));
#57327=CARTESIAN_POINT('Ctrl Pts',(-21.2525466701151,1.45110477441612,-0.528027546097545));
#57328=CARTESIAN_POINT('Ctrl Pts',(-21.2790612125208,1.15017039174401,-0.908861886302333));
#57329=CARTESIAN_POINT('Ctrl Pts',(-21.3055757549265,0.849236009071873,
-1.28969622650715));
#57330=CARTESIAN_POINT('Ctrl Pts',(-21.3320902973322,0.340356019941503,
-1.50621244698771));
#57331=CARTESIAN_POINT('Ctrl Pts',(-21.3586048397379,-0.14272071009898,
-1.45895601624122));
#57332=CARTESIAN_POINT('Ctrl Pts',(-21.3851193821435,-0.625797440139435,
-1.41169958549474));
#57333=CARTESIAN_POINT('Ctrl Pts',(-21.4116339245492,-1.08307091109002,
-1.10067050352125));
#57334=CARTESIAN_POINT('Ctrl Pts',(-21.4381484669549,-1.30449718850049,
-0.668736826869823));
#57335=CARTESIAN_POINT('Ctrl Pts',(-21.450713962689,-1.4094332232862,-0.464039318298204));
#57336=CARTESIAN_POINT('Ctrl Pts',(-21.4632794584231,-1.46140026781191,
-0.232187811403527));
#57337=CARTESIAN_POINT('Ctrl Pts',(-21.4758449541571,-1.46110336159793,
-0.000210604951717125));
#57338=CARTESIAN_POINT('Ctrl Pts',(-21.5471550458428,-1.46119914789583,
-0.000442129891295945));
#57339=CARTESIAN_POINT('Ctrl Pts',(-21.5353705336236,-1.46178585356219,
-0.217965677876684));
#57340=CARTESIAN_POINT('Ctrl Pts',(-21.5235860214044,-1.41633808391013,
-0.435256174586171));
#57341=CARTESIAN_POINT('Ctrl Pts',(-21.5118015091852,-1.32361817707143,
-0.630045034625424));
#57342=CARTESIAN_POINT('Ctrl Pts',(-21.4852869667795,-1.11500318682023,
-1.06830988543918));
#57343=CARTESIAN_POINT('Ctrl Pts',(-21.4587724243738,-0.66708401474874,
-1.39266544267209));
#57344=CARTESIAN_POINT('Ctrl Pts',(-21.4322578819681,-0.185607792922169,
-1.45412226842745));
#57345=CARTESIAN_POINT('Ctrl Pts',(-21.4057433395624,0.295868428904401,
-1.51557909418281));
#57346=CARTESIAN_POINT('Ctrl Pts',(-21.3792287971567,0.810901700486049,
-1.31413718846062));
#57347=CARTESIAN_POINT('Ctrl Pts',(-21.3527142547511,1.12291670834372,-0.942326849056391));
#57348=CARTESIAN_POINT('Ctrl Pts',(-21.3261997123454,1.43493171620138,-0.570516509652169));
#57349=CARTESIAN_POINT('Ctrl Pts',(-21.2996851699397,1.54392846033508,-0.0283377365659148));
#57350=CARTESIAN_POINT('Ctrl Pts',(-21.273170627534,1.3998403910005,0.435165145724725));
#57351=CARTESIAN_POINT('Ctrl Pts',(-21.2466560851283,1.2557523216659,0.898668028015379));
#57352=CARTESIAN_POINT('Ctrl Pts',(-21.2201415427226,0.858579438863007,
1.28349501951041));
#57353=CARTESIAN_POINT('Ctrl Pts',(-21.1936270003169,0.390759080991175,
1.41287974185809));
#57354=CARTESIAN_POINT('Ctrl Pts',(-21.1671124579112,-0.0770612768806438,
1.54226446420576));
#57355=CARTESIAN_POINT('Ctrl Pts',(-21.1405979155056,-0.615529109821396,
1.41620691740608));
#57356=CARTESIAN_POINT('Ctrl Pts',(-21.1140833730999,-0.977304676099182,
1.09261035799809));
#57357=CARTESIAN_POINT('Ctrl Pts',(-21.0917739306809,-1.2817040898621,0.820334913879643));
#57358=CARTESIAN_POINT('Ctrl Pts',(-21.0694644882619,-1.46101232011646,
0.408209609079869));
#57359=CARTESIAN_POINT('Ctrl Pts',(-21.0471550458428,-1.46458686986414,
-0.00117242835359658));
#57360=CARTESIAN_POINT('Origin',(-17.3,0.,0.));
#57361=CARTESIAN_POINT('',(-20.4758449541571,-1.46534501698659,0.00082302614468642));
#57362=CARTESIAN_POINT('',(-20.5471550458428,-1.46500269836855,0.00101311012710306));
#57363=CARTESIAN_POINT('',(-17.3,-1.4635,-1.79227059055215E-16));
#57364=CARTESIAN_POINT('Ctrl Pts',(-20.4758449541571,-1.46534501698659,
0.00082302614468642));
#57365=CARTESIAN_POINT('Ctrl Pts',(-20.4784382828881,-1.46566459987453,
0.0483467506841562));
#57366=CARTESIAN_POINT('Ctrl Pts',(-20.4810316116192,-1.46355390104093,
0.0958417285952254));
#57367=CARTESIAN_POINT('Ctrl Pts',(-20.4836249403502,-1.45891991962591,
0.143089225787058));
#57368=CARTESIAN_POINT('Ctrl Pts',(-20.5101394827559,-1.4115414691944,0.626154003832599));
#57369=CARTESIAN_POINT('Ctrl Pts',(-20.5366540251616,-1.10039689364073,
1.08334889681806));
#57370=CARTESIAN_POINT('Ctrl Pts',(-20.5631685675672,-0.668407300319506,
1.30466606428511));
#57371=CARTESIAN_POINT('Ctrl Pts',(-20.5896831099729,-0.236417706998265,
1.52598323175217));
#57372=CARTESIAN_POINT('Ctrl Pts',(-20.6161976523786,0.316416904090545,
1.51142267370079));
#57373=CARTESIAN_POINT('Ctrl Pts',(-20.6427121947843,0.736157557278878,
1.26767263490177));
#57374=CARTESIAN_POINT('Ctrl Pts',(-20.66922673719,1.15589821046721,1.02392259610275));
#57375=CARTESIAN_POINT('Ctrl Pts',(-20.6957412795957,1.44254490575507,0.550983076556086));
#57376=CARTESIAN_POINT('Ctrl Pts',(-20.7222558220014,1.46442938880383,0.0660940513604433));
#57377=CARTESIAN_POINT('Ctrl Pts',(-20.7487703644071,1.4863138718526,-0.418794973835186));
#57378=CARTESIAN_POINT('Ctrl Pts',(-20.7752849068128,1.2434361426623,-0.915633504679789));
#57379=CARTESIAN_POINT('Ctrl Pts',(-20.8017994492184,0.84735962458967,-1.19620379744961));
#57380=CARTESIAN_POINT('Ctrl Pts',(-20.8283139916241,0.451283106517042,
-1.47677409021943));
#57381=CARTESIAN_POINT('Ctrl Pts',(-20.8548285340298,-0.09799220043791,
-1.54107614491446));
#57382=CARTESIAN_POINT('Ctrl Pts',(-20.8813430764355,-0.548162250887773,
-1.35957346440686));
#57383=CARTESIAN_POINT('Ctrl Pts',(-20.9078576188412,-0.998332301337649,
-1.17807078389924));
#57384=CARTESIAN_POINT('Ctrl Pts',(-20.9343721612469,-1.34939709528243,
-0.75076336818897));
#57385=CARTESIAN_POINT('Ctrl Pts',(-20.9608867036526,-1.44009857763784,
-0.273930547955271));
#57386=CARTESIAN_POINT('Ctrl Pts',(-20.9658727871541,-1.45715507281757,
-0.184261708057138));
#57387=CARTESIAN_POINT('Ctrl Pts',(-20.9708588706556,-1.46500430372587,
-0.0928414943390442));
#57388=CARTESIAN_POINT('Ctrl Pts',(-20.9758449541571,-1.46416452657485,
-0.00127774293595062));
#57389=CARTESIAN_POINT('Ctrl Pts',(-21.0471550458428,-1.46458686986414,
-0.00117242835359658));
#57390=CARTESIAN_POINT('Ctrl Pts',(-21.0429499458562,-1.46526063565416,
-0.0783367235349625));
#57391=CARTESIAN_POINT('Ctrl Pts',(-21.0387448458695,-1.45969087111027,
-0.155403554912202));
#57392=CARTESIAN_POINT('Ctrl Pts',(-21.0345397458828,-1.44753843707036,
-0.231418014713479));
#57393=CARTESIAN_POINT('Ctrl Pts',(-21.0080252034771,-1.37091333214893,
-0.710714256000721));
#57394=CARTESIAN_POINT('Ctrl Pts',(-20.9815106610714,-1.03257982269125,
-1.14817116655891));
#57395=CARTESIAN_POINT('Ctrl Pts',(-20.9549961186658,-0.587947977283016,
-1.34284734811476));
#57396=CARTESIAN_POINT('Ctrl Pts',(-20.9284815762601,-0.143316131874758,
-1.53752352967063));
#57397=CARTESIAN_POINT('Ctrl Pts',(-20.9019670338544,0.407614049484076,
-1.48941898222413));
#57398=CARTESIAN_POINT('Ctrl Pts',(-20.8754524914487,0.811778371620634,
-1.22063004210899));
#57399=CARTESIAN_POINT('Ctrl Pts',(-20.848937949043,1.21594269375717,-0.951841101993865));
#57400=CARTESIAN_POINT('Ctrl Pts',(-20.8224234066373,1.47334115667146,-0.462367769210122));
#57401=CARTESIAN_POINT('Ctrl Pts',(-20.7959088642316,1.46574038513714,0.0229553416020292));
#57402=CARTESIAN_POINT('Ctrl Pts',(-20.7693943218259,1.45813961360282,0.508278452414194));
#57403=CARTESIAN_POINT('Ctrl Pts',(-20.7428797794203,1.1855396076199,0.989451341254735));
#57404=CARTESIAN_POINT('Ctrl Pts',(-20.7163652370146,0.773156417156846,
1.24545211828445));
#57405=CARTESIAN_POINT('Ctrl Pts',(-20.6898506946089,0.3607732266938,1.50145289531416));
#57406=CARTESIAN_POINT('Ctrl Pts',(-20.6633361522032,-0.19139314824938,
1.53228156053303));
#57407=CARTESIAN_POINT('Ctrl Pts',(-20.6368216097975,-0.629710679505619,
1.32377727901887));
#57408=CARTESIAN_POINT('Ctrl Pts',(-20.6103070673918,-1.06802821076187,
1.11527299750471));
#57409=CARTESIAN_POINT('Ctrl Pts',(-20.5837925249862,-1.39249689833119,
0.667435769257517));
#57410=CARTESIAN_POINT('Ctrl Pts',(-20.5572779825805,-1.4540753390434,0.185975086277314));
#57411=CARTESIAN_POINT('Ctrl Pts',(-20.5539036703346,-1.46191197764716,
0.124703099997769));
#57412=CARTESIAN_POINT('Ctrl Pts',(-20.5505293580887,-1.46549089978,0.0628865551477272));
#57413=CARTESIAN_POINT('Ctrl Pts',(-20.5471550458428,-1.46500269836855,
0.00101311012710306));
#57414=CARTESIAN_POINT('Origin',(-17.3,0.,0.));
#57415=CARTESIAN_POINT('',(-19.9758449541571,-1.46160352170699,0.000870148659567124));
#57416=CARTESIAN_POINT('',(-20.0471550458428,-1.46137421934213,0.000673585972547344));
#57417=CARTESIAN_POINT('',(-17.3,-1.4635,-1.79227059055215E-16));
#57418=CARTESIAN_POINT('Ctrl Pts',(-19.9758449541571,-1.46160352170699,
0.000870148659567124));
#57419=CARTESIAN_POINT('Ctrl Pts',(-19.9860176951207,-1.46261643292029,
0.188513100842206));
#57420=CARTESIAN_POINT('Ctrl Pts',(-19.9961904360843,-1.42911507721764,
0.375808090111529));
#57421=CARTESIAN_POINT('Ctrl Pts',(-20.0063631770478,-1.35943495977707,
0.548505650429889));
#57422=CARTESIAN_POINT('Ctrl Pts',(-20.0328777194535,-1.17781857582257,
0.998629840440597));
#57423=CARTESIAN_POINT('Ctrl Pts',(-20.0593922618592,-0.750422497676223,
1.34958668886163));
#57424=CARTESIAN_POINT('Ctrl Pts',(-20.0859068042649,-0.273566782208699,
1.44016772429102));
#57425=CARTESIAN_POINT('Ctrl Pts',(-20.1124213466706,0.203288933258798,
1.53074875972041));
#57426=CARTESIAN_POINT('Ctrl Pts',(-20.1389358890763,0.729604286047465,
1.3609539821582));
#57427=CARTESIAN_POINT('Ctrl Pts',(-20.165450431482,1.06362165301883,1.00877690182077));
#57428=CARTESIAN_POINT('Ctrl Pts',(-20.1919649738876,1.39763901999021,0.656599821483317));
#57429=CARTESIAN_POINT('Ctrl Pts',(-20.2184795162933,1.53935840114426,0.122040438370631));
#57430=CARTESIAN_POINT('Ctrl Pts',(-20.244994058699,1.42368243506273,-0.349356812602059));
#57431=CARTESIAN_POINT('Ctrl Pts',(-20.2715086011047,1.3080064689812,-0.820754063574708));
#57432=CARTESIAN_POINT('Ctrl Pts',(-20.2980231435104,0.934935155664138,
-1.22898918240737));
#57433=CARTESIAN_POINT('Ctrl Pts',(-20.3245376859161,0.475835021835091,
-1.38654350469533));
#57434=CARTESIAN_POINT('Ctrl Pts',(-20.3510522283218,0.0167348880060186,
-1.54409782698329));
#57435=CARTESIAN_POINT('Ctrl Pts',(-20.3775667707274,-0.528394066335047,
-1.45097135272652));
#57436=CARTESIAN_POINT('Ctrl Pts',(-20.4040813131331,-0.909152380850908,
-1.14994078404531));
#57437=CARTESIAN_POINT('Ctrl Pts',(-20.4280025268078,-1.2526695670265,-0.878353349276634));
#57438=CARTESIAN_POINT('Ctrl Pts',(-20.4519237404825,-1.46239714136337,
-0.437542212986177));
#57439=CARTESIAN_POINT('Ctrl Pts',(-20.4758449541571,-1.46534501698659,
0.00082302614468642));
#57440=CARTESIAN_POINT('Ctrl Pts',(-20.5471550458428,-1.46500269836855,
0.00101311012710306));
#57441=CARTESIAN_POINT('Ctrl Pts',(-20.524014815683,-1.46165472930044,-0.423300247448411));
#57442=CARTESIAN_POINT('Ctrl Pts',(-20.5008745855232,-1.26703441745964,
-0.850289557404769));
#57443=CARTESIAN_POINT('Ctrl Pts',(-20.4777343553634,-0.942610458482033,
-1.12267864854122));
#57444=CARTESIAN_POINT('Ctrl Pts',(-20.4512198129577,-0.570878943353276,
-1.43478756266641));
#57445=CARTESIAN_POINT('Ctrl Pts',(-20.424705270552,-0.0287277192406266,
-1.54392125320354));
#57446=CARTESIAN_POINT('Ctrl Pts',(-20.3981907281463,0.434811543720077,
-1.39995026546581));
#57447=CARTESIAN_POINT('Ctrl Pts',(-20.3716761857407,0.898350806680754,
-1.25597927772809));
#57448=CARTESIAN_POINT('Ctrl Pts',(-20.345161643335,1.28327810848951,-0.858903611715504));
#57449=CARTESIAN_POINT('Ctrl Pts',(-20.3186471009293,1.41278099426858,-0.391115950280114));
#57450=CARTESIAN_POINT('Ctrl Pts',(-20.2921325585236,1.54228388004766,0.0766717111552901));
#57451=CARTESIAN_POINT('Ctrl Pts',(-20.2656180161179,1.41636234979709,0.615171368013523));
#57452=CARTESIAN_POINT('Ctrl Pts',(-20.2391034737122,1.09285718223258,0.977028660568718));
#57453=CARTESIAN_POINT('Ctrl Pts',(-20.2125889313065,0.769352014668082,
1.3388859531239));
#57454=CARTESIAN_POINT('Ctrl Pts',(-20.1860743889009,0.248263209789676,
1.52410088137606));
#57455=CARTESIAN_POINT('Ctrl Pts',(-20.1595598464952,-0.231052371076101,
1.44759684517139));
#57456=CARTESIAN_POINT('Ctrl Pts',(-20.1330453040895,-0.710367951941878,
1.37109280896672));
#57457=CARTESIAN_POINT('Ctrl Pts',(-20.1065307616838,-1.14791030879501,
1.03286980830523));
#57458=CARTESIAN_POINT('Ctrl Pts',(-20.0800162192781,-1.34269879447265,
0.58828715067707));
#57459=CARTESIAN_POINT('Ctrl Pts',(-20.0690624947997,-1.4231700834369,0.404620547458549));
#57460=CARTESIAN_POINT('Ctrl Pts',(-20.0581087703212,-1.4622107443168,0.202801618307486));
#57461=CARTESIAN_POINT('Ctrl Pts',(-20.0471550458428,-1.46137421934213,
0.000673585972547344));
#57462=CARTESIAN_POINT('Origin',(-17.3,0.,0.));
#57463=CARTESIAN_POINT('',(-19.4758449541571,-1.46215770122242,-0.00115350946124346));
#57464=CARTESIAN_POINT('',(-19.5471550458428,-1.46252866632904,-0.00126132249279813));
#57465=CARTESIAN_POINT('',(-17.3,-1.4635,-1.79227059055215E-16));
#57466=CARTESIAN_POINT('Ctrl Pts',(-19.4758449541571,-1.46215770122242,
-0.00115350946124346));
#57467=CARTESIAN_POINT('Ctrl Pts',(-19.4935971073532,-1.45975765968372,
0.325985142341861));
#57468=CARTESIAN_POINT('Ctrl Pts',(-19.5113492605494,-1.35132302816047,
0.654566464045283));
#57469=CARTESIAN_POINT('Ctrl Pts',(-19.5291014137455,-1.14971110297745,
0.909442817393143));
#57470=CARTESIAN_POINT('Ctrl Pts',(-19.5556159561512,-0.848584367493725,
1.2901250819267));
#57471=CARTESIAN_POINT('Ctrl Pts',(-19.5821304985569,-0.339595062884128,
1.5063841970214));
#57472=CARTESIAN_POINT('Ctrl Pts',(-19.6086450409625,0.143457732345712,
1.45888372992773));
#57473=CARTESIAN_POINT('Ctrl Pts',(-19.6351595833682,0.626510527575551,
1.41138326283405));
#57474=CARTESIAN_POINT('Ctrl Pts',(-19.6616741257739,1.08362681342564,1.10012321355205));
#57475=CARTESIAN_POINT('Ctrl Pts',(-19.6881886681796,1.30483485682866,0.668077731123071));
#57476=CARTESIAN_POINT('Ctrl Pts',(-19.7147032105853,1.52604290023169,0.236032248694066));
#57477=CARTESIAN_POINT('Ctrl Pts',(-19.741217752991,1.51134270118758,-0.316798666881903));
#57478=CARTESIAN_POINT('Ctrl Pts',(-19.7677322953967,1.26748664714187,-0.736477737433156));
#57479=CARTESIAN_POINT('Ctrl Pts',(-19.7942468378024,1.02363059309619,-1.15615680798437));
#57480=CARTESIAN_POINT('Ctrl Pts',(-19.820761380208,0.550618684048914,-1.44268403351091));
#57481=CARTESIAN_POINT('Ctrl Pts',(-19.8472759226137,0.0657241464821964,
-1.46444603689818));
#57482=CARTESIAN_POINT('Ctrl Pts',(-19.8737904650194,-0.419170391084549,
-1.48620804028545));
#57483=CARTESIAN_POINT('Ctrl Pts',(-19.9003050074251,-0.915947557170757,
-1.24320482153345));
#57484=CARTESIAN_POINT('Ctrl Pts',(-19.9268195498308,-1.19641779533251,
-0.847057446357269));
#57485=CARTESIAN_POINT('Ctrl Pts',(-19.9431613512729,-1.36928100648401,
-0.602898537337132));
#57486=CARTESIAN_POINT('Ctrl Pts',(-19.959503152715,-1.45997635023122,-0.300565214489629));
#57487=CARTESIAN_POINT('Ctrl Pts',(-19.9758449541571,-1.46160352170699,
0.000870148659567124));
#57488=CARTESIAN_POINT('Ctrl Pts',(-20.0471550458428,-1.46137421934213,
0.000673585972547344));
#57489=CARTESIAN_POINT('Ctrl Pts',(-20.0315942279156,-1.46018585525209,
-0.286468702055025));
#57490=CARTESIAN_POINT('Ctrl Pts',(-20.0160334099883,-1.37852161398207,
-0.574234789112791));
#57491=CARTESIAN_POINT('Ctrl Pts',(-20.000472592061,-1.22083505168199,-0.811470024655674));
#57492=CARTESIAN_POINT('Ctrl Pts',(-19.9739580496554,-0.952148208711604,
-1.21570222776534));
#57493=CARTESIAN_POINT('Ctrl Pts',(-19.9474435072497,-0.462739908268787,
-1.47322431938986));
#57494=CARTESIAN_POINT('Ctrl Pts',(-19.920928964844,0.0225851069530342,
-1.46574613670784));
#57495=CARTESIAN_POINT('Ctrl Pts',(-19.8944144224383,0.507910122174897,
-1.45826795402582));
#57496=CARTESIAN_POINT('Ctrl Pts',(-19.8678998800326,0.98915185217573,-1.18578949703718));
#57497=CARTESIAN_POINT('Ctrl Pts',(-19.8413853376269,1.24525678562698,-0.773470983411786));
#57498=CARTESIAN_POINT('Ctrl Pts',(-19.8148707952212,1.50136171907822,-0.361152469786414));
#57499=CARTESIAN_POINT('Ctrl Pts',(-19.7883562528155,1.53232985597991,0.191006100475701));
#57500=CARTESIAN_POINT('Ctrl Pts',(-19.7618417104099,1.3239362965059,0.629376284208643));
#57501=CARTESIAN_POINT('Ctrl Pts',(-19.7353271680042,1.11554273703188,1.06774646794161));
#57502=CARTESIAN_POINT('Ctrl Pts',(-19.7088126255985,0.667787481182143,
1.39232826514539));
#57503=CARTESIAN_POINT('Ctrl Pts',(-19.6822980831928,0.186342367766726,
1.45402831688559));
#57504=CARTESIAN_POINT('Ctrl Pts',(-19.6557835407871,-0.295102745648651,
1.51572836862577));
#57505=CARTESIAN_POINT('Ctrl Pts',(-19.6292689983814,-0.8102377166297,1.31454667490242));
#57506=CARTESIAN_POINT('Ctrl Pts',(-19.6027544559757,-1.12244051710899,
0.942894007766594));
#57507=CARTESIAN_POINT('Ctrl Pts',(-19.5842213192648,-1.340664052492,0.683116200417021));
#57508=CARTESIAN_POINT('Ctrl Pts',(-19.5656881825538,-1.45974038043436,
0.340050854567538));
#57509=CARTESIAN_POINT('Ctrl Pts',(-19.5471550458428,-1.46252866632904,
-0.00126132249279813));
#57510=CARTESIAN_POINT('Origin',(-17.3,0.,0.));
#57511=CARTESIAN_POINT('',(-18.9758449541571,-1.46578778306489,-0.000400814154694062));
#57512=CARTESIAN_POINT('',(-19.0471550458428,-1.46590402480283,-0.00013840560174719));
#57513=CARTESIAN_POINT('',(-17.3,-1.4635,-1.79227059055215E-16));
#57514=CARTESIAN_POINT('Ctrl Pts',(-18.9758449541571,-1.46578778306489,
-0.000400814154694062));
#57515=CARTESIAN_POINT('Ctrl Pts',(-19.0011765195858,-1.4641024380076,0.463438220880033));
#57516=CARTESIAN_POINT('Ctrl Pts',(-19.0265080850145,-1.22529568750056,
0.928770590448006));
#57517=CARTESIAN_POINT('Ctrl Pts',(-19.0518396504431,-0.846755214080442,
1.19663171688084));
#57518=CARTESIAN_POINT('Ctrl Pts',(-19.0783541928488,-0.450537007075949,
1.47700188253981));
#57519=CARTESIAN_POINT('Ctrl Pts',(-19.1048687352545,0.0987707141235838,
1.54102644422561));
#57520=CARTESIAN_POINT('Ctrl Pts',(-19.1313832776602,0.548849014975999,
1.35929636841179));
#57521=CARTESIAN_POINT('Ctrl Pts',(-19.1578978200659,0.998927315828401,
1.17756629259798));
#57522=CARTESIAN_POINT('Ctrl Pts',(-19.1844123624716,1.34977619633369,0.750081579284574));
#57523=CARTESIAN_POINT('Ctrl Pts',(-19.2109269048772,1.44023677905777,0.273202999007897));
#57524=CARTESIAN_POINT('Ctrl Pts',(-19.2374414472829,1.53069736178185,-0.203675581268794));
#57525=CARTESIAN_POINT('Ctrl Pts',(-19.2639559896886,1.36076964672472,-0.72994802850872));
#57526=CARTESIAN_POINT('Ctrl Pts',(-19.2904705320943,1.00850820759375,-1.06387642780243));
#57527=CARTESIAN_POINT('Ctrl Pts',(-19.3169850745,0.656246768462777,-1.39780482709613));
#57528=CARTESIAN_POINT('Ctrl Pts',(-19.3434996169057,0.121651605257916,
-1.5393891784436));
#57529=CARTESIAN_POINT('Ctrl Pts',(-19.3700141593114,-0.349716411882835,
-1.42359414499969));
#57530=CARTESIAN_POINT('Ctrl Pts',(-19.3965287017171,-0.821084429023599,
-1.30779911155578));
#57531=CARTESIAN_POINT('Ctrl Pts',(-19.4230432441227,-1.22922530010029,
-0.934624693320504));
#57532=CARTESIAN_POINT('Ctrl Pts',(-19.4495577865284,-1.38666365245969,
-0.475484777216653));
#57533=CARTESIAN_POINT('Ctrl Pts',(-19.458320175738,-1.43869306706458,-0.323750586032459));
#57534=CARTESIAN_POINT('Ctrl Pts',(-19.4670825649475,-1.46334235177432,
-0.162627791533922));
#57535=CARTESIAN_POINT('Ctrl Pts',(-19.4758449541571,-1.46215770122242,
-0.00115350946124346));
#57536=CARTESIAN_POINT('Ctrl Pts',(-19.5471550458428,-1.46252866632904,
-0.00126132249279813));
#57537=CARTESIAN_POINT('Ctrl Pts',(-19.5391736401481,-1.46372945825462,
-0.148249444155522));
#57538=CARTESIAN_POINT('Ctrl Pts',(-19.5311922344534,-1.4433629405794,-0.294912415154495));
#57539=CARTESIAN_POINT('Ctrl Pts',(-19.5232108287587,-1.40006005061068,
-0.434457913973326));
#57540=CARTESIAN_POINT('Ctrl Pts',(-19.496696286353,-1.25620615365555,-0.898033528029032));
#57541=CARTESIAN_POINT('Ctrl Pts',(-19.4701817439473,-0.85922772976778,
-1.2830611155921));
#57542=CARTESIAN_POINT('Ctrl Pts',(-19.4436672015416,-0.391472794614882,
-1.41268215653998));
#57543=CARTESIAN_POINT('Ctrl Pts',(-19.4171526591359,0.0762821405380149,
-1.54230319748786));
#57544=CARTESIAN_POINT('Ctrl Pts',(-19.3906381167303,0.614813586956024,
-1.41651769182055));
#57545=CARTESIAN_POINT('Ctrl Pts',(-19.3641235743246,0.976752582701203,
-1.09310393674004));
#57546=CARTESIAN_POINT('Ctrl Pts',(-19.3376090319189,1.33869157844639,-0.769690181659522));
#57547=CARTESIAN_POINT('Ctrl Pts',(-19.3110944895132,1.52403812351873,-0.248648177165766));
#57548=CARTESIAN_POINT('Ctrl Pts',(-19.2845799471075,1.44765516091198,0.230686712696983));
#57549=CARTESIAN_POINT('Ctrl Pts',(-19.2580654047018,1.37127219830524,0.710021602559718));
#57550=CARTESIAN_POINT('Ctrl Pts',(-19.2315508622961,1.03315972801944,1.14764937779147));
#57551=CARTESIAN_POINT('Ctrl Pts',(-19.2050363198904,0.588626286536881,
1.34255015516287));
#57552=CARTESIAN_POINT('Ctrl Pts',(-19.1785217774848,0.144092845054323,
1.53745093253427));
#57553=CARTESIAN_POINT('Ctrl Pts',(-19.1520072350791,-0.406861567624983,
1.48962471204531));
#57554=CARTESIAN_POINT('Ctrl Pts',(-19.1254926926734,-0.811161625916757,
1.22103998336259));
#57555=CARTESIAN_POINT('Ctrl Pts',(-19.0993801437299,-1.20933199214373,
0.956527333440112));
#57556=CARTESIAN_POINT('Ctrl Pts',(-19.0732675947863,-1.46526121859312,
0.477899378505275));
#57557=CARTESIAN_POINT('Ctrl Pts',(-19.0471550458428,-1.46590402480283,
-0.00013840560174719));
#57558=CARTESIAN_POINT('Origin',(-17.3,0.,0.));
#57559=CARTESIAN_POINT('',(-18.4758449541571,-1.46337413104549,0.00135256974678304));
#57560=CARTESIAN_POINT('',(-18.5471550458428,-1.46294584879644,0.00133002991220975));
#57561=CARTESIAN_POINT('',(-17.3,-1.4635,-1.79227059055215E-16));
#57562=CARTESIAN_POINT('Ctrl Pts',(-18.4758449541571,-1.46337413104549,
0.00135256974678304));
#57563=CARTESIAN_POINT('Ctrl Pts',(-18.4822413894126,-1.46445455751735,
0.11897860929348));
#57564=CARTESIAN_POINT('Ctrl Pts',(-18.4886378246682,-1.45146917310825,
0.236369036177189));
#57565=CARTESIAN_POINT('Ctrl Pts',(-18.4950342599237,-1.42350576410765,
0.350075988850877));
#57566=CARTESIAN_POINT('Ctrl Pts',(-18.5215488023294,-1.30759167068936,
0.821414742085207));
#57567=CARTESIAN_POINT('Ctrl Pts',(-18.5480633447351,-0.934314171345385,
1.22946133936544));
#57568=CARTESIAN_POINT('Ctrl Pts',(-18.5745778871408,-0.475134502261091,
1.3867837117513));
#57569=CARTESIAN_POINT('Ctrl Pts',(-18.6010924295465,-0.0159548331767707,
1.54410608413717));
#57570=CARTESIAN_POINT('Ctrl Pts',(-18.6276069719521,0.529127005647898,
1.45070423162863));
#57571=CARTESIAN_POINT('Ctrl Pts',(-18.6541215143578,0.909733195910636,
1.149481348555));
#57572=CARTESIAN_POINT('Ctrl Pts',(-18.6806360567635,1.29033938617334,0.848258465481405));
#57573=CARTESIAN_POINT('Ctrl Pts',(-18.7071505991692,1.50646992787416,0.339214551842755));
#57574=CARTESIAN_POINT('Ctrl Pts',(-18.7336651415749,1.45884744714899,-0.143826229751351));
#57575=CARTESIAN_POINT('Ctrl Pts',(-18.7601796839806,1.41122496642381,-0.626867011345499));
#57576=CARTESIAN_POINT('Ctrl Pts',(-18.7866942263863,1.09984946327261,-1.08390466089507));
#57577=CARTESIAN_POINT('Ctrl Pts',(-18.8132087687919,0.667748119301473,
-1.3050035661204));
#57578=CARTESIAN_POINT('Ctrl Pts',(-18.8397233111976,0.235646775330358,
-1.52610247134571));
#57579=CARTESIAN_POINT('Ctrl Pts',(-18.8662378536033,-0.317180409460681,
-1.51126263224677));
#57580=CARTESIAN_POINT('Ctrl Pts',(-18.892752396009,-0.736797870598213,
-1.26730057851306));
#57581=CARTESIAN_POINT('Ctrl Pts',(-18.9192669384147,-1.15641533173576,
-1.02333852477935));
#57582=CARTESIAN_POINT('Ctrl Pts',(-18.9457814808204,-1.4428230692198,-0.550254256410852));
#57583=CARTESIAN_POINT('Ctrl Pts',(-18.9722960232261,-1.46446259155709,
-0.065354237410539));
#57584=CARTESIAN_POINT('Ctrl Pts',(-18.9734790002031,-1.46542806387514,
-0.0437198622117143));
#57585=CARTESIAN_POINT('Ctrl Pts',(-18.9746619771801,-1.4658664882048,-0.0220619665627543));
#57586=CARTESIAN_POINT('Ctrl Pts',(-18.9758449541571,-1.46578778306489,
-0.000400814154694062));
#57587=CARTESIAN_POINT('Ctrl Pts',(-19.0471550458428,-1.46590402480283,
-0.00013840560174719));
#57588=CARTESIAN_POINT('Ctrl Pts',(-19.0467530523807,-1.46591392057724,
-0.00749762833770351));
#57589=CARTESIAN_POINT('Ctrl Pts',(-19.0463510589185,-1.46586331470994,
-0.0148567112060816));
#57590=CARTESIAN_POINT('Ctrl Pts',(-19.0459490654563,-1.46575179476014,
-0.0222148708632159));
#57591=CARTESIAN_POINT('Ctrl Pts',(-19.0194345230506,-1.45839620140749,
-0.507541759529738));
#57592=CARTESIAN_POINT('Ctrl Pts',(-18.9929199806449,-1.18603931079801,
-0.988852299986267));
#57593=CARTESIAN_POINT('Ctrl Pts',(-18.9664054382393,-0.773785500317309,
-1.24506137351889));
#57594=CARTESIAN_POINT('Ctrl Pts',(-18.9398908958336,-0.361531689836588,
-1.50127044705152));
#57595=CARTESIAN_POINT('Ctrl Pts',(-18.9133763534279,0.190619040515314,
-1.53237805366019));
#57596=CARTESIAN_POINT('Ctrl Pts',(-18.8868618110222,0.62904184875583,-1.32409522952237));
#57597=CARTESIAN_POINT('Ctrl Pts',(-18.8603472686165,1.06746465699632,-1.11581240538456));
#57598=CARTESIAN_POINT('Ctrl Pts',(-18.8338327262108,1.39215954312542,-0.66813915050023));
#57599=CARTESIAN_POINT('Ctrl Pts',(-18.8073181838051,1.45398120195699,-0.186709637367093));
#57600=CARTESIAN_POINT('Ctrl Pts',(-18.7808036413995,1.51580286078856,0.294719875766044));
#57601=CARTESIAN_POINT('Ctrl Pts',(-18.7542890989938,1.31475129232266,0.809905647148002));
#57602=CARTESIAN_POINT('Ctrl Pts',(-18.7277745565881,0.943177496892139,
1.12220231406209));
#57603=CARTESIAN_POINT('Ctrl Pts',(-18.7012600141824,0.571603701461615,
1.43449898097619));
#57604=CARTESIAN_POINT('Ctrl Pts',(-18.6747454717767,0.0295076790664164,
1.54390654342238));
#57605=CARTESIAN_POINT('Ctrl Pts',(-18.648230929371,-0.434104256506996,
1.40016974642811));
#57606=CARTESIAN_POINT('Ctrl Pts',(-18.6217163869653,-0.897716192080435,
1.25643294943382));
#57607=CARTESIAN_POINT('Ctrl Pts',(-18.5952018445597,-1.2828440408321,0.859551792999085));
#57608=CARTESIAN_POINT('Ctrl Pts',(-18.568687302154,-1.41258322867861,0.391829613972634));
#57609=CARTESIAN_POINT('Ctrl Pts',(-18.5615098833836,-1.44770329478633,
0.265218417154564));
#57610=CARTESIAN_POINT('Ctrl Pts',(-18.5543324646132,-1.46410921932681,
0.133416195328377));
#57611=CARTESIAN_POINT('Ctrl Pts',(-18.5471550458428,-1.46294584879644,
0.00133002991220975));
#57612=CARTESIAN_POINT('Origin',(-17.3,0.,0.));
#57613=CARTESIAN_POINT('',(-17.9758449541571,-1.46110551485691,-0.000218695958779103));
#57614=CARTESIAN_POINT('',(-18.0471550458428,-1.46120363688599,-0.000449877262721942));
#57615=CARTESIAN_POINT('',(-17.3,-1.4635,-1.79227059055215E-16));
#57616=CARTESIAN_POINT('Ctrl Pts',(-17.9758449541571,-1.46110551485691,
-0.000218695958779103));
#57617=CARTESIAN_POINT('Ctrl Pts',(-17.9898208016452,-1.4607625691127,0.257794693658319));
#57618=CARTESIAN_POINT('Ctrl Pts',(-18.0037966491333,-1.39576298805581,
0.515969572122497));
#57619=CARTESIAN_POINT('Ctrl Pts',(-18.0177724966213,-1.26711442902716,
0.737117956753728));
#57620=CARTESIAN_POINT('Ctrl Pts',(-18.044287039027,-1.02304639117082,1.15667378170486));
#57621=CARTESIAN_POINT('Ctrl Pts',(-18.0708015814327,-0.549889793665136,
1.44296201287282));
#57622=CARTESIAN_POINT('Ctrl Pts',(-18.0973161238384,-0.0649843241691522,
1.46447905277948));
#57623=CARTESIAN_POINT('Ctrl Pts',(-18.1238306662441,0.419921145326859,
1.48599609268614));
#57624=CARTESIAN_POINT('Ctrl Pts',(-18.1503452086498,0.916575486813129,
1.2427419413315));
#57625=CARTESIAN_POINT('Ctrl Pts',(-18.1768597510555,1.19684556208097,0.84645292777844));
#57626=CARTESIAN_POINT('Ctrl Pts',(-18.2033742934612,1.4771156373488,0.450163914225396));
#57627=CARTESIAN_POINT('Ctrl Pts',(-18.2298888358668,1.54100144639816,-0.0991599615260736));
#57628=CARTESIAN_POINT('Ctrl Pts',(-18.2564033782725,1.35915769031991,-0.549192344504046));
#57629=CARTESIAN_POINT('Ctrl Pts',(-18.2829179206782,1.17731393424166,-0.99922472748203));
#57630=CARTESIAN_POINT('Ctrl Pts',(-18.3094324630839,0.749740613035781,
-1.34996561768655));
#57631=CARTESIAN_POINT('Ctrl Pts',(-18.3359470054896,0.272839198375997,
-1.44030574193369));
#57632=CARTESIAN_POINT('Ctrl Pts',(-18.3624615478953,-0.204062216283761,
-1.53064586618082));
#57633=CARTESIAN_POINT('Ctrl Pts',(-18.388976090301,-0.730291724397424,
-1.3605852244706));
#57634=CARTESIAN_POINT('Ctrl Pts',(-18.4154906327066,-1.06413113470796,
-1.00823944902129));
#57635=CARTESIAN_POINT('Ctrl Pts',(-18.4356087398568,-1.31743428151736,
-0.740894459395029));
#57636=CARTESIAN_POINT('Ctrl Pts',(-18.455726847007,-1.45997596712131,-0.368605566732589));
#57637=CARTESIAN_POINT('Ctrl Pts',(-18.4758449541571,-1.46337413104549,
0.00135256974678304));
#57638=CARTESIAN_POINT('Ctrl Pts',(-18.5471550458428,-1.46294584879644,
0.00133002991220975));
#57639=CARTESIAN_POINT('Ctrl Pts',(-18.5278179222075,-1.45981154097644,
-0.354531400621349));
#57640=CARTESIAN_POINT('Ctrl Pts',(-18.5084807985722,-1.3291504183923,-0.712453837100621));
#57641=CARTESIAN_POINT('Ctrl Pts',(-18.4891436749369,-1.09335062150458,
-0.976476442514407));
#57642=CARTESIAN_POINT('Ctrl Pts',(-18.4626291325312,-0.770028299542674,
-1.33849711835691));
#57643=CARTESIAN_POINT('Ctrl Pts',(-18.4361145901255,-0.249033128677468,
-1.52397526842382));
#57644=CARTESIAN_POINT('Ctrl Pts',(-18.4096000477198,0.230321039599414,
-1.44771338428844));
#57645=CARTESIAN_POINT('Ctrl Pts',(-18.3830855053142,0.709675207876324,
-1.37145150015305));
#57646=CARTESIAN_POINT('Ctrl Pts',(-18.3565709629085,1.14738837356491,-1.03344958181541));
#57647=CARTESIAN_POINT('Ctrl Pts',(-18.3300564205028,1.34240143019492,-0.588965384840811));
#57648=CARTESIAN_POINT('Ctrl Pts',(-18.3035418780971,1.53741448682491,-0.144481187866252));
#57649=CARTESIAN_POINT('Ctrl Pts',(-18.2770273356914,1.48972743439631,0.406485287745245));
#57650=CARTESIAN_POINT('Ctrl Pts',(-18.2505127932857,1.22124483713764,0.810853175423698));
#57651=CARTESIAN_POINT('Ctrl Pts',(-18.22399825088,0.952762239878958,1.21522106310218));
#57652=CARTESIAN_POINT('Ctrl Pts',(-18.1974837084743,0.463484097790187,
1.47299036284763));
#57653=CARTESIAN_POINT('Ctrl Pts',(-18.1709691660687,-0.0218446333559495,
1.46575735929368));
#57654=CARTESIAN_POINT('Ctrl Pts',(-18.144454623663,-0.507173364502044,
1.45852435573973));
#57655=CARTESIAN_POINT('Ctrl Pts',(-18.1179400812573,-0.988552684705489,
1.18628904888644));
#57656=CARTESIAN_POINT('Ctrl Pts',(-18.0914255388516,-1.24486588197267,
0.774099967853279));
#57657=CARTESIAN_POINT('Ctrl Pts',(-18.0766687078487,-1.38751856207629,
0.544693609750165));
#57658=CARTESIAN_POINT('Ctrl Pts',(-18.0619118768458,-1.46045594798573,
0.271935909324877));
#57659=CARTESIAN_POINT('Ctrl Pts',(-18.0471550458428,-1.46120363688599,
-0.000449877262721942));
#57660=CARTESIAN_POINT('Origin',(-17.3,0.,0.));
#57661=CARTESIAN_POINT('',(-17.4758449541571,-1.46417935052163,-0.00127487220091121));
#57662=CARTESIAN_POINT('',(-17.5471550458428,-1.46460091918832,-0.00116803120312899));
#57663=CARTESIAN_POINT('',(-17.3,-1.4635,-1.79227059055215E-16));
#57664=CARTESIAN_POINT('Ctrl Pts',(-17.4758449541571,-1.46417935052163,
-0.00127487220091121));
#57665=CARTESIAN_POINT('Ctrl Pts',(-17.4974002138777,-1.46055286990098,
0.394552617929168));
#57666=CARTESIAN_POINT('Ctrl Pts',(-17.5189554735984,-1.29448215597133,
0.793060082165337));
#57667=CARTESIAN_POINT('Ctrl Pts',(-17.540510733319,-1.00797062612048,1.06438577371923));
#57668=CARTESIAN_POINT('Ctrl Pts',(-17.5670252757247,-0.655540536833363,
1.39813617374679));
#57669=CARTESIAN_POINT('Ctrl Pts',(-17.5935398181304,-0.120873915772161,
1.5394504383893));
#57670=CARTESIAN_POINT('Ctrl Pts',(-17.6200543605361,0.350435543483126,
1.42341729239225));
#57671=CARTESIAN_POINT('Ctrl Pts',(-17.6465689029417,0.821745002738413,
1.30738414639521));
#57672=CARTESIAN_POINT('Ctrl Pts',(-17.6730834453474,1.22969730018777,0.934003589758628));
#57673=CARTESIAN_POINT('Ctrl Pts',(-17.6995979877531,1.38690368256252,0.474784196990721));
#57674=CARTESIAN_POINT('Ctrl Pts',(-17.7261125301588,1.54411006493728,0.0155648042228135));
#57675=CARTESIAN_POINT('Ctrl Pts',(-17.7526270725645,1.4505705322374,-0.529493424676442));
#57676=CARTESIAN_POINT('Ctrl Pts',(-17.7791416149702,1.14925152079274,-0.9100235163847));
#57677=CARTESIAN_POINT('Ctrl Pts',(-17.8056561573759,0.847932509348076,
-1.29055360809297));
#57678=CARTESIAN_POINT('Ctrl Pts',(-17.8321706997815,0.338834019158619,
-1.50655556261026));
#57679=CARTESIAN_POINT('Ctrl Pts',(-17.8586852421872,-0.144194717980545,
-1.458811071292));
#57680=CARTESIAN_POINT('Ctrl Pts',(-17.8851997845929,-0.627223455119695,
-1.41106657997374));
#57681=CARTESIAN_POINT('Ctrl Pts',(-17.9117143269986,-1.08418243920854,
-1.09957564281995));
#57682=CARTESIAN_POINT('Ctrl Pts',(-17.9382288694043,-1.3051721921495,-0.66741846487589));
#57683=CARTESIAN_POINT('Ctrl Pts',(-17.9507675643219,-1.40967797805547,
-0.463051860022404));
#57684=CARTESIAN_POINT('Ctrl Pts',(-17.9633062592395,-1.46141319509337,
-0.231700270140578));
#57685=CARTESIAN_POINT('Ctrl Pts',(-17.9758449541571,-1.46110551485691,
-0.000218695958779103));
#57686=CARTESIAN_POINT('Ctrl Pts',(-18.0471550458428,-1.46120363688599,
-0.000449877262721942));
#57687=CARTESIAN_POINT('Ctrl Pts',(-18.0353973344401,-1.46179936847,-0.217477060692192));
#57688=CARTESIAN_POINT('Ctrl Pts',(-18.0236396230373,-1.41656670969026,
-0.434268141003884));
#57689=CARTESIAN_POINT('Ctrl Pts',(-18.0118819116345,-1.32425407805813,
-0.628707373168519));
#57690=CARTESIAN_POINT('Ctrl Pts',(-17.9853673692289,-1.1160820025455,-1.06718277794405));
#57691=CARTESIAN_POINT('Ctrl Pts',(-17.9588528268232,-0.668490777189342,
-1.39199073228205));
#57692=CARTESIAN_POINT('Ctrl Pts',(-17.9323382844175,-0.187076895054903,
-1.45393399426063));
#57693=CARTESIAN_POINT('Ctrl Pts',(-17.9058237420118,0.294336987079563,
-1.5158772562392));
#57694=CARTESIAN_POINT('Ctrl Pts',(-17.8793091996061,0.80957352599233,-1.31495582585831));
#57695=CARTESIAN_POINT('Ctrl Pts',(-17.8527946572004,1.12196403941587,-0.943460925840423));
#57696=CARTESIAN_POINT('Ctrl Pts',(-17.8262801147947,1.43435455283938,-0.571966025822565));
#57697=CARTESIAN_POINT('Ctrl Pts',(-17.7997655723891,1.54389904077372,-0.0298976561677314));
#57698=CARTESIAN_POINT('Ctrl Pts',(-17.7732510299834,1.40027935291106,0.433750571343731));
#57699=CARTESIAN_POINT('Ctrl Pts',(-17.7467364875777,1.2566596650484,0.897398798855233));
#57700=CARTESIAN_POINT('Ctrl Pts',(-17.720221945172,0.859875801388736,1.28262688422333));
#57701=CARTESIAN_POINT('Ctrl Pts',(-17.6937074027663,0.39218640833064,1.41248421069078));
#57702=CARTESIAN_POINT('Ctrl Pts',(-17.6671928603606,-0.0755029847274155,
1.54234153715822));
#57703=CARTESIAN_POINT('Ctrl Pts',(-17.6406783179549,-0.61409790718388,
1.41682810472502));
#57704=CARTESIAN_POINT('Ctrl Pts',(-17.6141637755493,-0.976200240025855,
1.09359723651055));
#57705=CARTESIAN_POINT('Ctrl Pts',(-17.5918275323138,-1.28124060839204,
0.821302765680679));
#57706=CARTESIAN_POINT('Ctrl Pts',(-17.5694912890783,-1.4610307665805,0.408695602734371));
#57707=CARTESIAN_POINT('Ctrl Pts',(-17.5471550458428,-1.46460091918832,
-0.00116803120312899));
#57708=CARTESIAN_POINT('Origin',(-17.3,0.,0.));
#57709=CARTESIAN_POINT('',(-16.9758449541571,-1.46533423939264,0.000830137543336423));
#57710=CARTESIAN_POINT('',(-17.0471550458428,-1.46499001420292,0.00101896910938441));
#57711=CARTESIAN_POINT('',(-17.3,-1.4635,-1.79227059055215E-16));
#57712=CARTESIAN_POINT('Ctrl Pts',(-16.9758449541571,-1.46533423939264,
0.000830137543336423));
#57713=CARTESIAN_POINT('Ctrl Pts',(-16.9784650837046,-1.46565935231474,
0.0488459268207528));
#57714=CARTESIAN_POINT('Ctrl Pts',(-16.9810852132521,-1.46350470201884,
0.0968321742252827));
#57715=CARTESIAN_POINT('Ctrl Pts',(-16.9837053427996,-1.4587746023591,0.144563197009661));
#57716=CARTESIAN_POINT('Ctrl Pts',(-17.0102198852053,-1.41090810349401,
0.627579858875393));
#57717=CARTESIAN_POINT('Ctrl Pts',(-17.0367344276109,-1.09930175221151,
1.0844601483484));
#57718=CARTESIAN_POINT('Ctrl Pts',(-17.0632489700166,-0.667088767867208,
1.30534073490527));
#57719=CARTESIAN_POINT('Ctrl Pts',(-17.0897635124223,-0.234875783522952,
1.52622132146211));
#57720=CARTESIAN_POINT('Ctrl Pts',(-17.116278054828,0.317943833883089,1.51110220510288));
#57721=CARTESIAN_POINT('Ctrl Pts',(-17.1427925972337,0.737437995879103,
1.26692819869613));
#57722=CARTESIAN_POINT('Ctrl Pts',(-17.1693071396394,1.15693215787514,1.02275419228936));
#57723=CARTESIAN_POINT('Ctrl Pts',(-17.1958216820451,1.44310086446115,0.549525295835037));
#57724=CARTESIAN_POINT('Ctrl Pts',(-17.2223362244507,1.46449542056432,0.0646144067815574));
#57725=CARTESIAN_POINT('Ctrl Pts',(-17.2488507668564,1.4858899766675,-0.420296482271922));
#57726=CARTESIAN_POINT('Ctrl Pts',(-17.2753653092621,1.24251038228787,-0.916889363924539));
#57727=CARTESIAN_POINT('Ctrl Pts',(-17.3018798516678,0.846150587470515,
-1.19705933091928));
#57728=CARTESIAN_POINT('Ctrl Pts',(-17.3283943940735,0.449790792653172,
-1.47722929791401));
#57729=CARTESIAN_POINT('Ctrl Pts',(-17.3549089364792,-0.0995492026018883,
-1.54097635025084));
#57730=CARTESIAN_POINT('Ctrl Pts',(-17.3814234788849,-0.549535638992197,
-1.35901892551025));
#57731=CARTESIAN_POINT('Ctrl Pts',(-17.4079380212906,-0.999522075382518,
-1.17706150076966));
#57732=CARTESIAN_POINT('Ctrl Pts',(-17.4344525636963,-1.35015495290811,
-0.749399598951582));
#57733=CARTESIAN_POINT('Ctrl Pts',(-17.4609671061019,-1.44037461291437,
-0.272475380336248));
#57734=CARTESIAN_POINT('Ctrl Pts',(-17.465926388787,-1.45724930721892,-0.183271426397507));
#57735=CARTESIAN_POINT('Ctrl Pts',(-17.4708856714721,-1.4650137056991,-0.0923440796015177));
#57736=CARTESIAN_POINT('Ctrl Pts',(-17.4758449541571,-1.46417935052163,
-0.00127487220091121));
#57737=CARTESIAN_POINT('Ctrl Pts',(-17.5471550458428,-1.46460091918832,
-0.00116803120312899));
#57738=CARTESIAN_POINT('Ctrl Pts',(-17.5429767466726,-1.46526876496353,
-0.0778386182632508));
#57739=CARTESIAN_POINT('Ctrl Pts',(-17.5387984475024,-1.45977017776411,
-0.154413201537133));
#57740=CARTESIAN_POINT('Ctrl Pts',(-17.5346201483322,-1.44777151529703,
-0.229955351806808));
#57741=CARTESIAN_POINT('Ctrl Pts',(-17.5081056059265,-1.3716307144987,-0.709328767913805));
#57742=CARTESIAN_POINT('Ctrl Pts',(-17.4815910635208,-1.0337393696746,-1.147127296132));
#57743=CARTESIAN_POINT('Ctrl Pts',(-17.4550765211151,-0.589304445567263,
-1.34225261957826));
#57744=CARTESIAN_POINT('Ctrl Pts',(-17.4285619787094,-0.144869521459913,
-1.53737794302453));
#57745=CARTESIAN_POINT('Ctrl Pts',(-17.4020474363038,0.406108981930661,
-1.48983006169885));
#57746=CARTESIAN_POINT('Ctrl Pts',(-17.3755328938981,0.810544673196106,
-1.22144961299411));
#57747=CARTESIAN_POINT('Ctrl Pts',(-17.3490183514924,1.21498036446153,-0.953069164289384));
#57748=CARTESIAN_POINT('Ctrl Pts',(-17.3225038090867,1.47287324360184,-0.46385614820559));
#57749=CARTESIAN_POINT('Ctrl Pts',(-17.295989266681,1.46576283030811,0.0214743944548562));
#57750=CARTESIAN_POINT('Ctrl Pts',(-17.2694747242753,1.45865241701438,0.506804937115344));
#57751=CARTESIAN_POINT('Ctrl Pts',(-17.2429601818696,1.18653871128658,0.988253006352498));
#57752=CARTESIAN_POINT('Ctrl Pts',(-17.216445639464,0.774414385999632,1.24467031100081));
#57753=CARTESIAN_POINT('Ctrl Pts',(-17.1899310970583,0.362290060712716,
1.5010876156491));
#57754=CARTESIAN_POINT('Ctrl Pts',(-17.1634165546526,-0.189844884133316,
1.53247415570858));
#57755=CARTESIAN_POINT('Ctrl Pts',(-17.1369020122469,-0.628372857468012,
1.32441284210307));
#57756=CARTESIAN_POINT('Ctrl Pts',(-17.1103874698412,-1.06690083080273,
1.11635152849754));
#57757=CARTESIAN_POINT('Ctrl Pts',(-17.0838729274355,-1.3918218326261,0.66884236122699));
#57758=CARTESIAN_POINT('Ctrl Pts',(-17.0573583850298,-1.45388669379952,
0.187444140806682));
#57759=CARTESIAN_POINT('Ctrl Pts',(-17.0539572719675,-1.46184797055169,
0.125693507867038));
#57760=CARTESIAN_POINT('Ctrl Pts',(-17.0505561589052,-1.46548418873406,
0.0633852614001415));
#57761=CARTESIAN_POINT('Ctrl Pts',(-17.0471550458428,-1.46499001420292,
0.00101896910938441));
#57762=CARTESIAN_POINT('Origin',(-17.3,0.,0.));
#57763=CARTESIAN_POINT('',(-16.4758449541571,-1.46159467054894,0.00086381236336773));
#57764=CARTESIAN_POINT('',(-16.5471550458428,-1.46136743550077,0.000666439445737842));
#57765=CARTESIAN_POINT('',(-17.3,-1.4635,-1.79227059055215E-16));
#57766=CARTESIAN_POINT('Ctrl Pts',(-16.4758449541571,-1.46159467054894,
0.00086381236336773));
#57767=CARTESIAN_POINT('Ctrl Pts',(-16.4860444959372,-1.46260248845685,
0.189003976803686));
#57768=CARTESIAN_POINT('Ctrl Pts',(-16.4962440377172,-1.42891868062783,
0.376797030316824));
#57769=CARTESIAN_POINT('Ctrl Pts',(-16.5064435794972,-1.35888007399166,
0.549878898418593));
#57770=CARTESIAN_POINT('Ctrl Pts',(-16.5329581219029,-1.17680899219806,
0.99981935951095));
#57771=CARTESIAN_POINT('Ctrl Pts',(-16.5594726643086,-0.749058537053789,
1.35034420198627));
#57772=CARTESIAN_POINT('Ctrl Pts',(-16.5859872067143,-0.272111544911907,
1.44044339199542));
#57773=CARTESIAN_POINT('Ctrl Pts',(-16.61250174912,0.204835447229961,1.53054258200456));
#57774=CARTESIAN_POINT('Ctrl Pts',(-16.6390162915256,0.730978976369435,
1.36021611954754));
#57775=CARTESIAN_POINT('Ctrl Pts',(-16.6655308339313,1.06464034481988,1.0077017389086));
#57776=CARTESIAN_POINT('Ctrl Pts',(-16.692045376337,1.39830171327034,0.655187358269641));
#57777=CARTESIAN_POINT('Ctrl Pts',(-16.7185599187427,1.53948092103175,0.120485059448733));
#57778=CARTESIAN_POINT('Ctrl Pts',(-16.7450744611484,1.42332872985914,-0.350795075756759));
#57779=CARTESIAN_POINT('Ctrl Pts',(-16.7715890035541,1.30717653868653,-0.822075210962224));
#57780=CARTESIAN_POINT('Ctrl Pts',(-16.7981035459598,0.933692948579942,
-1.22993318255228));
#57781=CARTESIAN_POINT('Ctrl Pts',(-16.8246180883655,0.474433861427808,
-1.38702356488573));
#57782=CARTESIAN_POINT('Ctrl Pts',(-16.8511326307711,0.0151747742756748,
-1.54411394721917));
#57783=CARTESIAN_POINT('Ctrl Pts',(-16.8776471731768,-0.529859809922002,
-1.45043674029601));
#57784=CARTESIAN_POINT('Ctrl Pts',(-16.9041617155825,-0.91031377879697,
-1.14902161970521));
#57785=CARTESIAN_POINT('Ctrl Pts',(-16.9280561284407,-1.2531718250248,-0.877391914658694));
#57786=CARTESIAN_POINT('Ctrl Pts',(-16.9519505412989,-1.46236935454806,
-0.437052444944582));
#57787=CARTESIAN_POINT('Ctrl Pts',(-16.9758449541571,-1.46533423939264,
0.000830137543336423));
#57788=CARTESIAN_POINT('Ctrl Pts',(-17.0471550458428,-1.46499001420292,
0.00101896910938441));
#57789=CARTESIAN_POINT('Ctrl Pts',(-17.0240416164995,-1.4616316818278,-0.4228125424722));
#57790=CARTESIAN_POINT('Ctrl Pts',(-17.0009281871561,-1.267517448972,-0.849324812075515));
#57791=CARTESIAN_POINT('Ctrl Pts',(-16.9778147578128,-0.943744294593583,
-1.12172569318533));
#57792=CARTESIAN_POINT('Ctrl Pts',(-16.9513002154071,-0.572328313690735,
-1.434210033187));
#57793=CARTESIAN_POINT('Ctrl Pts',(-16.9247856730014,-0.0302876313615806,
-1.5438914396203));
#57794=CARTESIAN_POINT('Ctrl Pts',(-16.8982711305957,0.433396858506015,
-1.40038887005259));
#57795=CARTESIAN_POINT('Ctrl Pts',(-16.87175658819,0.897081348373612,-1.25688630048487));
#57796=CARTESIAN_POINT('Ctrl Pts',(-16.8452420457843,1.28240964577962,-0.860199754916109));
#57797=CARTESIAN_POINT('Ctrl Pts',(-16.8187275033787,1.41238510258278,-0.39254317766618));
#57798=CARTESIAN_POINT('Ctrl Pts',(-16.792212960973,1.54236055938594,0.0751133995837501));
#57799=CARTESIAN_POINT('Ctrl Pts',(-16.7656984185673,1.41698317558626,0.61374000851487));
#57800=CARTESIAN_POINT('Ctrl Pts',(-16.7391838761616,1.09384378174213,0.975923975253261));
#57801=CARTESIAN_POINT('Ctrl Pts',(-16.7126693337559,0.770704387898002,
1.33810794199164));
#57802=CARTESIAN_POINT('Ctrl Pts',(-16.6861547913502,0.249802984009428,
1.52384926653732));
#57803=CARTESIAN_POINT('Ctrl Pts',(-16.6596402489445,-0.229589649342414,
1.44782955393405));
#57804=CARTESIAN_POINT('Ctrl Pts',(-16.6331257065389,-0.708982282694284,
1.37180984133078));
#57805=CARTESIAN_POINT('Ctrl Pts',(-16.6066111641332,-1.1468661455094,1.03402909157855));
#57806=CARTESIAN_POINT('Ctrl Pts',(-16.5800966217275,-1.34210372332243,
0.589643468694527));
#57807=CARTESIAN_POINT('Ctrl Pts',(-16.5691160964326,-1.422957887384,0.40560908114604));
#57808=CARTESIAN_POINT('Ctrl Pts',(-16.5581355711377,-1.46219688775553,
0.203291375369544));
#57809=CARTESIAN_POINT('Ctrl Pts',(-16.5471550458428,-1.46136743550077,
0.000666439445737842));
#57810=CARTESIAN_POINT('Origin',(-17.3,0.,0.));
#57811=CARTESIAN_POINT('',(-15.9758449541571,-1.46216976248559,-0.00115783740885875));
#57812=CARTESIAN_POINT('',(-16.0471550458428,-1.46254205711415,-0.00126432517610342));
#57813=CARTESIAN_POINT('',(-17.3,-1.4635,-1.79227059055215E-16));
#57814=CARTESIAN_POINT('Ctrl Pts',(-15.9758449541571,-1.46216976248559,
-0.00115783740885875));
#57815=CARTESIAN_POINT('Ctrl Pts',(-15.9936239081697,-1.45975575237227,
0.326467896832275));
#57816=CARTESIAN_POINT('Ctrl Pts',(-16.0114028621823,-1.35096575277778,
0.655546977160496));
#57817=CARTESIAN_POINT('Ctrl Pts',(-16.0291818161949,-1.14879164530715,
0.910603983128834));
#57818=CARTESIAN_POINT('Ctrl Pts',(-16.0556963586006,-0.847280434801294,
1.29098180489658));
#57819=CARTESIAN_POINT('Ctrl Pts',(-16.0822109010062,-0.338072888959171,
1.50672654371053));
#57820=CARTESIAN_POINT('Ctrl Pts',(-16.1087254434119,0.144931666815352,
1.4587380403526));
#57821=CARTESIAN_POINT('Ctrl Pts',(-16.1352399858176,0.627936222589903,
1.41074953699466));
#57822=CARTESIAN_POINT('Ctrl Pts',(-16.1617545282233,1.08473778829685,1.09902779146479));
#57823=CARTESIAN_POINT('Ctrl Pts',(-16.188269070629,1.30550919437688,0.666759028296608));
#57824=CARTESIAN_POINT('Ctrl Pts',(-16.2147836130347,1.5262806004569,0.234490265128449));
#57825=CARTESIAN_POINT('Ctrl Pts',(-16.2412981554403,1.51102184691004,-0.318325515678011));
#57826=CARTESIAN_POINT('Ctrl Pts',(-16.267812697846,1.26674188753176,-0.737757987954096));
#57827=CARTESIAN_POINT('Ctrl Pts',(-16.2943272402517,1.02246192815349,-1.15719046023018));
#57828=CARTESIAN_POINT('Ctrl Pts',(-16.3208417826574,0.549160762943808,
-1.44323962397589));
#57829=CARTESIAN_POINT('Ctrl Pts',(-16.3473563250631,0.0642444852714359,
-1.46451169491057));
#57830=CARTESIAN_POINT('Ctrl Pts',(-16.3738708674688,-0.420671792400949,
-1.48578376584524));
#57831=CARTESIAN_POINT('Ctrl Pts',(-16.4003854098745,-0.917203182536025,
-1.24227874396888));
#57832=CARTESIAN_POINT('Ctrl Pts',(-16.4268999522802,-1.1972730233821,-0.845848193175995));
#57833=CARTESIAN_POINT('Ctrl Pts',(-16.4432149529058,-1.36960636252544,
-0.601915464288857));
#57834=CARTESIAN_POINT('Ctrl Pts',(-16.4595299535315,-1.45998258344223,
-0.300081756246599));
#57835=CARTESIAN_POINT('Ctrl Pts',(-16.4758449541571,-1.46159467054894,
0.00086381236336773));
#57836=CARTESIAN_POINT('Ctrl Pts',(-16.5471550458428,-1.46136743550077,
0.000666439445737842));
#57837=CARTESIAN_POINT('Ctrl Pts',(-16.531621028732,-1.46019401936885,-0.285984621153708));
#57838=CARTESIAN_POINT('Ctrl Pts',(-16.5160870116212,-1.37882992327694,
-0.573250554372443));
#57839=CARTESIAN_POINT('Ctrl Pts',(-16.5005529945104,-1.22165431091895,
-0.810236119253631));
#57840=CARTESIAN_POINT('Ctrl Pts',(-16.4740384521047,-0.953376027891525,
-1.21473958830201));
#57841=CARTESIAN_POINT('Ctrl Pts',(-16.447523909699,-0.464228169025754,
-1.47275603038295));
#57842=CARTESIAN_POINT('Ctrl Pts',(-16.4210093672934,0.021104154183723,
-1.46576820780307));
#57843=CARTESIAN_POINT('Ctrl Pts',(-16.3944948248877,0.506436477393186,
-1.45878038522319));
#57844=CARTESIAN_POINT('Ctrl Pts',(-16.367980282482,0.987953264946341,-1.1867882979825));
#57845=CARTESIAN_POINT('Ctrl Pts',(-16.3414657400763,1.2444746606157,-0.774728754736447));
#57846=CARTESIAN_POINT('Ctrl Pts',(-16.3149511976706,1.50099605628506,-0.362669211490377));
#57847=CARTESIAN_POINT('Ctrl Pts',(-16.2884366552649,1.5325220600706,0.189457787761057));
#57848=CARTESIAN_POINT('Ctrl Pts',(-16.2619221128592,1.32457152164702,0.628038301675728));
#57849=CARTESIAN_POINT('Ctrl Pts',(-16.2354075704535,1.11662098322344,1.0666188155904));
#57850=CARTESIAN_POINT('Ctrl Pts',(-16.2088930280479,0.669193902590743,
1.3916528441683));
#57851=CARTESIAN_POINT('Ctrl Pts',(-16.1823784856422,0.187811374599038,
1.45383930057667));
#57852=CARTESIAN_POINT('Ctrl Pts',(-16.1558639432365,-0.293571153392639,
1.51602575698503));
#57853=CARTESIAN_POINT('Ctrl Pts',(-16.1293494008308,-0.808909128743352,
1.31536464122387));
#57854=CARTESIAN_POINT('Ctrl Pts',(-16.1028348584251,-1.12148727538583,
0.944027603133352));
#57855=CARTESIAN_POINT('Ctrl Pts',(-16.0842749208977,-1.34028912326836,
0.68409506788046));
#57856=CARTESIAN_POINT('Ctrl Pts',(-16.0657149833703,-1.45974124758651,
0.340533512961544));
#57857=CARTESIAN_POINT('Ctrl Pts',(-16.0471550458428,-1.46254205711415,
-0.00126432517610342));
#57858=CARTESIAN_POINT('Origin',(-17.3,0.,0.));
#57859=CARTESIAN_POINT('',(-15.4758449541571,-1.46579348024391,-0.000392046237105565));
#57860=CARTESIAN_POINT('',(-15.5471550458428,-1.46590607594638,-0.000129214056304876));
#57861=CARTESIAN_POINT('',(-17.3,-1.4635,-1.79227059055215E-16));
#57862=CARTESIAN_POINT('Ctrl Pts',(-15.4758449541571,-1.46579348024391,
-0.000392046237105564));
#57863=CARTESIAN_POINT('Ctrl Pts',(-15.5012033204023,-1.4641396019743,0.463932910653296));
#57864=CARTESIAN_POINT('Ctrl Pts',(-15.5265616866474,-1.22475744536399,
0.929725121980544));
#57865=CARTESIAN_POINT('Ctrl Pts',(-15.5519200528925,-0.845545744914202,
1.19748663945578));
#57866=CARTESIAN_POINT('Ctrl Pts',(-15.5784345952982,-0.449044463439101,
1.47745633628402));
#57867=CARTESIAN_POINT('Ctrl Pts',(-15.6049491377039,0.100327665674265,
1.54092586300297));
#57868=CARTESIAN_POINT('Ctrl Pts',(-15.6314636801096,0.550222122761289,
1.35874113577299));
#57869=CARTESIAN_POINT('Ctrl Pts',(-15.6579782225153,1.0001165798483,1.17655640854301));
#57870=CARTESIAN_POINT('Ctrl Pts',(-15.6844927649209,1.35053336490898,0.748717427364106));
#57871=CARTESIAN_POINT('Ctrl Pts',(-15.7110073073266,1.44051207917245,0.271747692126144));
#57872=CARTESIAN_POINT('Ctrl Pts',(-15.7375218497323,1.53049079343592,-0.205222043111832));
#57873=CARTESIAN_POINT('Ctrl Pts',(-15.764036392138,1.36003143690217,-0.731322532408869));
#57874=CARTESIAN_POINT('Ctrl Pts',(-15.7905509345437,1.00743278740271,-1.06489484799374));
#57875=CARTESIAN_POINT('Ctrl Pts',(-15.8170654769494,0.654834137903267,
-1.3984671635786));
#57876=CARTESIAN_POINT('Ctrl Pts',(-15.8435800193551,0.120096195438124,
-1.5395113054513));
#57877=CARTESIAN_POINT('Ctrl Pts',(-15.8700945617607,-0.35115458564864,
-1.42324007651399));
#57878=CARTESIAN_POINT('Ctrl Pts',(-15.8966091041664,-0.822405366735417,
-1.30696884757667));
#57879=CARTESIAN_POINT('Ctrl Pts',(-15.9231236465721,-1.23016898644384,
-0.933382247829284));
#57880=CARTESIAN_POINT('Ctrl Pts',(-15.9496381889778,-1.38714335871322,
-0.474083495594829));
#57881=CARTESIAN_POINT('Ctrl Pts',(-15.9583737773709,-1.43886077036718,
-0.322761070806314));
#57882=CARTESIAN_POINT('Ctrl Pts',(-15.967109365764,-1.46335587268711,-0.162134886975079));
#57883=CARTESIAN_POINT('Ctrl Pts',(-15.9758449541571,-1.46216976248559,
-0.00115783740885875));
#57884=CARTESIAN_POINT('Ctrl Pts',(-16.0471550458428,-1.46254205711415,
-0.00126432517610342));
#57885=CARTESIAN_POINT('Ctrl Pts',(-16.0392004409646,-1.46374245625874,
-0.14775548370561));
#57886=CARTESIAN_POINT('Ctrl Pts',(-16.0312458360863,-1.44351524001586,
-0.293922666076689));
#57887=CARTESIAN_POINT('Ctrl Pts',(-16.0232912312081,-1.40049829784565,
-0.433043118016538));
#57888=CARTESIAN_POINT('Ctrl Pts',(-15.9967766888024,-1.25711285572868,
-0.896763840655955));
#57889=CARTESIAN_POINT('Ctrl Pts',(-15.9702621463967,-0.860523653560479,
-1.28219232551488));
#57890=CARTESIAN_POINT('Ctrl Pts',(-15.943747603991,-0.392899921956407,
-1.41228590436097));
#57891=CARTESIAN_POINT('Ctrl Pts',(-15.9172330615853,0.074723809647678,
-1.54237948320706));
#57892=CARTESIAN_POINT('Ctrl Pts',(-15.8907185191796,0.613382070687635,
-1.4171381560403));
#57893=CARTESIAN_POINT('Ctrl Pts',(-15.8642039767739,0.975647648214161,
-1.09409025718367));
#57894=CARTESIAN_POINT('Ctrl Pts',(-15.8376894343682,1.33791322574068,-0.77104235832704));
#57895=CARTESIAN_POINT('Ctrl Pts',(-15.8111748919626,1.52378611975377,-0.250187887780555));
#57896=CARTESIAN_POINT('Ctrl Pts',(-15.7846603495569,1.44788750019579,0.229223932229647));
#57897=CARTESIAN_POINT('Ctrl Pts',(-15.7581458071512,1.37198888063781,0.708635752239876));
#57898=CARTESIAN_POINT('Ctrl Pts',(-15.7316312647455,1.03431874750873,1.14660492171382));
#57899=CARTESIAN_POINT('Ctrl Pts',(-15.7051167223398,0.589982454200974,
1.34195474143692));
#57900=CARTESIAN_POINT('Ctrl Pts',(-15.6786021799341,0.145646160893255,
1.53730456116001));
#57901=CARTESIAN_POINT('Ctrl Pts',(-15.6520876375285,-0.405356292593118,
1.49003503113232));
#57902=CARTESIAN_POINT('Ctrl Pts',(-15.6255730951228,-0.809927513616029,
1.22185893089906));
#57903=CARTESIAN_POINT('Ctrl Pts',(-15.5994337453628,-1.20877387073326,
0.957477642547655));
#57904=CARTESIAN_POINT('Ctrl Pts',(-15.5732943956028,-1.46530380969871,
0.478397404464385));
#57905=CARTESIAN_POINT('Ctrl Pts',(-15.5471550458428,-1.46590607594638,
-0.000129214056304876));
#57906=CARTESIAN_POINT('Origin',(-17.3,0.,0.));
#57907=CARTESIAN_POINT('',(-14.9758449541571,-1.46335918983354,0.00135254215526508));
#57908=CARTESIAN_POINT('',(-15.0471550458428,-1.46293148617486,0.00132846867353373));
#57909=CARTESIAN_POINT('',(-17.3,-1.4635,-1.79227059055215E-16));
#57910=CARTESIAN_POINT('Ctrl Pts',(-14.9758449541571,-1.46335918983354,
0.00135254215526508));
#57911=CARTESIAN_POINT('Ctrl Pts',(-14.9822681902291,-1.46444314548935,
0.119474507650463));
#57912=CARTESIAN_POINT('Ctrl Pts',(-14.9886914263011,-1.45134725973014,
0.237359122688176));
#57913=CARTESIAN_POINT('Ctrl Pts',(-14.9951146623731,-1.42315133236242,
0.351514073136027));
#57914=CARTESIAN_POINT('Ctrl Pts',(-15.0216292047788,-1.30676107307877,
0.822735470037065));
#57915=CARTESIAN_POINT('Ctrl Pts',(-15.0481437471844,-0.933071487526462,
1.23040471184739));
#57916=CARTESIAN_POINT('Ctrl Pts',(-15.0746582895901,-0.473733099514172,
1.38726306403735));
#57917=CARTESIAN_POINT('Ctrl Pts',(-15.1011728319958,-0.0143947115018555,
1.54412141622733));
#57918=CARTESIAN_POINT('Ctrl Pts',(-15.1276873744015,0.530592478970439,
1.45016887879692));
#57919=CARTESIAN_POINT('Ctrl Pts',(-15.1542019168072,0.910894129361871,
1.14856159761316));
#57920=CARTESIAN_POINT('Ctrl Pts',(-15.1807164592129,1.29119577975329,0.846954316429403));
#57921=CARTESIAN_POINT('Ctrl Pts',(-15.2072310016186,1.50681189006386,0.337692291492272));
#57922=CARTESIAN_POINT('Ctrl Pts',(-15.2337455440243,1.45870138527481,-0.145300127374153));
#57923=CARTESIAN_POINT('Ctrl Pts',(-15.2602600864299,1.41059088048578,-0.628292546240537));
#57924=CARTESIAN_POINT('Ctrl Pts',(-15.2867746288357,1.09875376059722,-1.08501535903624));
#57925=CARTESIAN_POINT('Ctrl Pts',(-15.3132891712413,0.666429246185057,
-1.30567757055363));
#57926=CARTESIAN_POINT('Ctrl Pts',(-15.339803713647,0.234104731772872,-1.52633978207103));
#57927=CARTESIAN_POINT('Ctrl Pts',(-15.3663182560527,-0.318707177162912,
-1.51094139231009));
#57928=CARTESIAN_POINT('Ctrl Pts',(-15.3928327984584,-0.738077932958183,
-1.266555495546));
#57929=CARTESIAN_POINT('Ctrl Pts',(-15.4193473408641,-1.15744868875347,
-1.02216959878192));
#57930=CARTESIAN_POINT('Ctrl Pts',(-15.4458618832698,-1.44337829140822,
-0.548796195014686));
#57931=CARTESIAN_POINT('Ctrl Pts',(-15.4723764256755,-1.46452787581717,
-0.06387455966231));
#57932=CARTESIAN_POINT('Ctrl Pts',(-15.473532601836,-1.46545011105417,-0.0427293772958018));
#57933=CARTESIAN_POINT('Ctrl Pts',(-15.4746887779966,-1.46586888630947,
-0.021562236805336));
#57934=CARTESIAN_POINT('Ctrl Pts',(-15.4758449541571,-1.46579348024391,
-0.000392046237105564));
#57935=CARTESIAN_POINT('Ctrl Pts',(-15.5471550458428,-1.46590607594638,
-0.000129214056304876));
#57936=CARTESIAN_POINT('Ctrl Pts',(-15.5467798531971,-1.46591472060927,
-0.00699777313276096));
#57937=CARTESIAN_POINT('Ctrl Pts',(-15.5464046605514,-1.46587063787642,
-0.0138662181499694));
#57938=CARTESIAN_POINT('Ctrl Pts',(-15.5460294679057,-1.46577349177823,
-0.0207339125660903));
#57939=CARTESIAN_POINT('Ctrl Pts',(-15.5195149255,-1.45890826035804,-0.506067985359095));
#57940=CARTESIAN_POINT('Ctrl Pts',(-15.4930003830943,-1.18703780895822,
-0.987653460506266));
#57941=CARTESIAN_POINT('Ctrl Pts',(-15.4664858406886,-0.775043074043492,
-1.24427893082992));
#57942=CARTESIAN_POINT('Ctrl Pts',(-15.439971298283,-0.363048339128761,
-1.50090440115358));
#57943=CARTESIAN_POINT('Ctrl Pts',(-15.4134567558773,0.189070679300894,
-1.53256986665373));
#57944=CARTESIAN_POINT('Ctrl Pts',(-15.3869422134716,0.627703705812936,
-1.3247301166799));
#57945=CARTESIAN_POINT('Ctrl Pts',(-15.3604276710659,1.06633673232499,-1.11689036670607));
#57946=CARTESIAN_POINT('Ctrl Pts',(-15.3339131286602,1.39148376691944,-0.66954540125823));
#57947=CARTESIAN_POINT('Ctrl Pts',(-15.3073985862545,1.45379181459511,-0.188178596408585));
#57948=CARTESIAN_POINT('Ctrl Pts',(-15.2808840438488,1.51609986227078,0.293188208441046));
#57949=CARTESIAN_POINT('Ctrl Pts',(-15.2543695014432,1.31556892302771,0.808576852692463));
#57950=CARTESIAN_POINT('Ctrl Pts',(-15.2278549590375,0.944310851441779,
1.1212487860325));
#57951=CARTESIAN_POINT('Ctrl Pts',(-15.2013404166318,0.573052779855828,
1.43392071937255));
#57952=CARTESIAN_POINT('Ctrl Pts',(-15.1748258742261,0.0310675759269861,
1.54387594180115));
#57953=CARTESIAN_POINT('Ctrl Pts',(-15.1483113318204,-0.432689349897711,
1.40060763628332));
#57954=CARTESIAN_POINT('Ctrl Pts',(-15.1217967894147,-0.896446275722394,
1.25733933076549));
#57955=CARTESIAN_POINT('Ctrl Pts',(-15.095282247009,-1.28197492344295,0.860847497301233));
#57956=CARTESIAN_POINT('Ctrl Pts',(-15.0687677046033,-1.41218661603166,
0.393256641178603));
#57957=CARTESIAN_POINT('Ctrl Pts',(-15.0615634850165,-1.44756620553502,
0.266208353761034));
#57958=CARTESIAN_POINT('Ctrl Pts',(-15.0543592654297,-1.46409692728797,
0.133911154947905));
#57959=CARTESIAN_POINT('Ctrl Pts',(-15.0471550458428,-1.46293148617486,
0.00132846867353373));
#57960=CARTESIAN_POINT('Origin',(-17.3,0.,0.));
#57961=CARTESIAN_POINT('',(-14.4758449541571,-1.4611077494086,-0.000226779192605414));
#57962=CARTESIAN_POINT('',(-14.5471550458428,-1.46120820448801,-0.00045760858243725));
#57963=CARTESIAN_POINT('',(-17.3,-1.4635,-1.79227059055215E-16));
#57964=CARTESIAN_POINT('Ctrl Pts',(-14.4758449541571,-1.4611077494086,-0.000226779192605414));
#57965=CARTESIAN_POINT('Ctrl Pts',(-14.4898476024617,-1.46075141589656,
0.258280404757669));
#57966=CARTESIAN_POINT('Ctrl Pts',(-14.5038502507662,-1.39548808866609,
0.516955705114966));
#57967=CARTESIAN_POINT('Ctrl Pts',(-14.5178528990707,-1.26636902275068,
0.738397830871059));
#57968=CARTESIAN_POINT('Ctrl Pts',(-14.5443674414764,-1.02187720419323,
1.15770684342856));
#57969=CARTESIAN_POINT('Ctrl Pts',(-14.5708819838821,-0.548431592070911,
1.44351686674928));
#57970=CARTESIAN_POINT('Ctrl Pts',(-14.5973965262878,-0.0635046299778209,
1.46454396328311));
#57971=CARTESIAN_POINT('Ctrl Pts',(-14.6239110686935,0.42142233211527,1.48557105981693));
#57972=CARTESIAN_POINT('Ctrl Pts',(-14.6504256110992,0.917830644179146,
1.24181522956387));
#57973=CARTESIAN_POINT('Ctrl Pts',(-14.6769401535048,1.19770017912673,0.845243242704368));
#57974=CARTESIAN_POINT('Ctrl Pts',(-14.7034546959105,1.47756971407433,0.448671255844851));
#57975=CARTESIAN_POINT('Ctrl Pts',(-14.7299692383162,1.54090047190564,-0.100716887621091));
#57976=CARTESIAN_POINT('Ctrl Pts',(-14.7564837807219,1.35860211086313,-0.550565311998352));
#57977=CARTESIAN_POINT('Ctrl Pts',(-14.7829983231276,1.17630374982063,-1.00041373637563));
#57978=CARTESIAN_POINT('Ctrl Pts',(-14.8095128655333,0.748376269904274,
-1.35072244166419));
#57979=CARTESIAN_POINT('Ctrl Pts',(-14.836027407939,0.271383822002094,-1.44058067444109));
#57980=CARTESIAN_POINT('Ctrl Pts',(-14.8625419503447,-0.20560862590006,
-1.53043890721798));
#57981=CARTESIAN_POINT('Ctrl Pts',(-14.8890564927503,-0.731666041788053,
-1.35984666748324));
#57982=CARTESIAN_POINT('Ctrl Pts',(-14.915571035156,-1.06514928322455,-1.00716377162));
#57983=CARTESIAN_POINT('Ctrl Pts',(-14.9356623414897,-1.31784510042325,
-0.739919480127962));
#57984=CARTESIAN_POINT('Ctrl Pts',(-14.9557536478234,-1.45996867376205,
-0.368122371564781));
#57985=CARTESIAN_POINT('Ctrl Pts',(-14.9758449541571,-1.46335918983354,
0.00135254215526508));
#57986=CARTESIAN_POINT('Ctrl Pts',(-15.0471550458428,-1.46293148617486,
0.00132846867353373));
#57987=CARTESIAN_POINT('Ctrl Pts',(-15.027844723024,-1.45980761635813,-0.354048604622195));
#57988=CARTESIAN_POINT('Ctrl Pts',(-15.0085344002051,-1.32954313637262,
-0.711476803367705));
#57989=CARTESIAN_POINT('Ctrl Pts',(-14.9892240773863,-1.09433666281944,
-0.975371258926184));
#57990=CARTESIAN_POINT('Ctrl Pts',(-14.9627095349806,-0.771380279561598,
-1.33771842412738));
#57991=CARTESIAN_POINT('Ctrl Pts',(-14.9361949925749,-0.250572775588987,
-1.52372287574874));
#57992=CARTESIAN_POINT('Ctrl Pts',(-14.9096804501692,0.228858200491881,
-1.44794535407855));
#57993=CARTESIAN_POINT('Ctrl Pts',(-14.8831659077635,0.708289176572695,
-1.37216783240837));
#57994=CARTESIAN_POINT('Ctrl Pts',(-14.8566513653579,1.1463436247618,-1.03460833744674));
#57995=CARTESIAN_POINT('Ctrl Pts',(-14.8301368229522,1.34180567393118,-0.590321402065126));
#57996=CARTESIAN_POINT('Ctrl Pts',(-14.8036222805465,1.53726772310058,-0.146034466683465));
#57997=CARTESIAN_POINT('Ctrl Pts',(-14.7771077381408,1.4901373732502,0.404979909118181));
#57998=CARTESIAN_POINT('Ctrl Pts',(-14.7505931957351,1.22206347292139,0.809618856302988));
#57999=CARTESIAN_POINT('Ctrl Pts',(-14.7240786533294,0.9539895725926,1.21425780348776));
#58000=CARTESIAN_POINT('Ctrl Pts',(-14.6975641109237,0.464972121785394,
1.47252132205572));
#58001=CARTESIAN_POINT('Ctrl Pts',(-14.671049568518,-0.0203636696255808,
1.46577868223324));
#58002=CARTESIAN_POINT('Ctrl Pts',(-14.6445350261124,-0.50569946103657,
1.45903604241077));
#58003=CARTESIAN_POINT('Ctrl Pts',(-14.6180204837067,-0.987353593051334,
1.18728724419787));
#58004=CARTESIAN_POINT('Ctrl Pts',(-14.591505941301,-1.24408312165593,0.775357343900782));
#58005=CARTESIAN_POINT('Ctrl Pts',(-14.5767223094816,-1.38722701491958,
0.545678856970483));
#58006=CARTESIAN_POINT('Ctrl Pts',(-14.5619386776622,-1.46044615101826,
0.27242074658531));
#58007=CARTESIAN_POINT('Ctrl Pts',(-14.5471550458428,-1.46120820448801,
-0.00045760858243725));
#58008=CARTESIAN_POINT('Origin',(-17.3,0.,0.));
#58009=CARTESIAN_POINT('',(-13.9758449541571,-1.46419415654471,-0.00127194797176891));
#58010=CARTESIAN_POINT('',(-14.0471550458428,-1.46461493246388,-0.00116358319217421));
#58011=CARTESIAN_POINT('',(-17.3,-1.4635,-1.79227059055215E-16));
#58012=CARTESIAN_POINT('Ctrl Pts',(-13.9758449541571,-1.46419415654471,
-0.00127194797176891));
#58013=CARTESIAN_POINT('Ctrl Pts',(-13.9974270146942,-1.46056726591937,
0.395037360005112));
#58014=CARTESIAN_POINT('Ctrl Pts',(-14.0190090752313,-1.29403678955949,
0.794030585412455));
#58015=CARTESIAN_POINT('Ctrl Pts',(-14.0405911357684,-1.00689469157767,
1.06540365049606));
#58016=CARTESIAN_POINT('Ctrl Pts',(-14.0671056781741,-0.654127571852718,
1.39879779650711));
#58017=CARTESIAN_POINT('Ctrl Pts',(-14.0936202205797,-0.119318444454299,
1.53957177961409));
#58018=CARTESIAN_POINT('Ctrl Pts',(-14.1201347629854,0.351873538195867,
1.42306249741012));
#58019=CARTESIAN_POINT('Ctrl Pts',(-14.1466493053911,0.82306552084606,1.30655321520615));
#58020=CARTESIAN_POINT('Ctrl Pts',(-14.1731638477968,1.23064035874799,0.932760667691196));
#58021=CARTESIAN_POINT('Ctrl Pts',(-14.1996783902025,1.38738268085055,0.473382673208));
#58022=CARTESIAN_POINT('Ctrl Pts',(-14.2261929326082,1.5441250029531,0.0140046787248296));
#58023=CARTESIAN_POINT('Ctrl Pts',(-14.2527074750139,1.4500348092563,-0.530958762726577));
#58024=CARTESIAN_POINT('Ctrl Pts',(-14.2792220174195,1.14833147663801,-0.911184217477438));
#58025=CARTESIAN_POINT('Ctrl Pts',(-14.3057365598252,0.846628144019725,
-1.2914096722283));
#58026=CARTESIAN_POINT('Ctrl Pts',(-14.3322511022309,0.337311672479953,
-1.50689714027861));
#58027=CARTESIAN_POINT('Ctrl Pts',(-14.3587656446366,-0.14566857866218,
-1.45866463712813));
#58028=CARTESIAN_POINT('Ctrl Pts',(-14.3852801870423,-0.628648829804313,
-1.41043213397765));
#58029=CARTESIAN_POINT('Ctrl Pts',(-14.411794729448,-1.08529286054881,-1.09847965962638));
#58030=CARTESIAN_POINT('Ctrl Pts',(-14.4383092718537,-1.30584586342477,
-0.666099421553594));
#58031=CARTESIAN_POINT('Ctrl Pts',(-14.4508211659548,-1.40992217647036,
-0.462064380426998));
#58032=CARTESIAN_POINT('Ctrl Pts',(-14.463333060056,-1.46142614683388,-0.231212692687603));
#58033=CARTESIAN_POINT('Ctrl Pts',(-14.4758449541571,-1.4611077494086,-0.000226779192605414));
#58034=CARTESIAN_POINT('Ctrl Pts',(-14.5471550458428,-1.46120820448801,
-0.00045760858243725));
#58035=CARTESIAN_POINT('Ctrl Pts',(-14.5354241352565,-1.46181289900589,
-0.216988405920967));
#58036=CARTESIAN_POINT('Ctrl Pts',(-14.5236932246702,-1.41679478498902,
-0.433280089304781));
#58037=CARTESIAN_POINT('Ctrl Pts',(-14.5119623140839,-1.32488862719155,
-0.627369069901061));
#58038=CARTESIAN_POINT('Ctrl Pts',(-14.4854477716782,-1.11715967892816,
-1.06605458102458));
#58039=CARTESIAN_POINT('Ctrl Pts',(-14.4589332292726,-0.669896857206923,
-1.39131460089034));
#58040=CARTESIAN_POINT('Ctrl Pts',(-14.4324186868669,-0.188545806211767,
-1.45374423585788));
#58041=CARTESIAN_POINT('Ctrl Pts',(-14.4059041444612,0.292805244783348,
-1.5161738708254));
#58042=CARTESIAN_POINT('Ctrl Pts',(-14.3793896020555,0.808244525052368,
-1.31577312089478));
#58043=CARTESIAN_POINT('Ctrl Pts',(-14.3528750596498,1.12101022514064,-0.944594039500663));
#58044=CARTESIAN_POINT('Ctrl Pts',(-14.3263605172441,1.43377592522893,-0.573414958106515));
#58045=CARTESIAN_POINT('Ctrl Pts',(-14.2998459748384,1.5438680451364,-0.031457545248834));
#58046=CARTESIAN_POINT('Ctrl Pts',(-14.2733314324327,1.40071688535858,0.43233555417222));
#58047=CARTESIAN_POINT('Ctrl Pts',(-14.2468168900271,1.25756572558076,0.896128653593288));
#58048=CARTESIAN_POINT('Ctrl Pts',(-14.2203023476214,0.861171286117661,
1.28175743957772));
#58049=CARTESIAN_POINT('Ctrl Pts',(-14.1937878052157,0.393613335309966,
1.41208723760121));
#58050=CARTESIAN_POINT('Ctrl Pts',(-14.16727326281,-0.0739446154976886,
1.54241703562468));
#58051=CARTESIAN_POINT('Ctrl Pts',(-14.1407587204043,-0.612666077649932,
1.41744784568724));
#58052=CARTESIAN_POINT('Ctrl Pts',(-14.1142441779986,-0.975094807407056,
1.09458299863365));
#58053=CARTESIAN_POINT('Ctrl Pts',(-14.0918811339467,-1.28077647919425,
0.822270518674362));
#58054=CARTESIAN_POINT('Ctrl Pts',(-14.0695180898948,-1.46104936176178,
0.40918164700796));
#58055=CARTESIAN_POINT('Ctrl Pts',(-14.0471550458428,-1.46461493246388,
-0.00116358319217421));
#58056=CARTESIAN_POINT('Origin',(-17.3,0.,0.));
#58057=CARTESIAN_POINT('',(-13.4758449541571,-1.46532338661684,0.000837209389326979));
#58058=CARTESIAN_POINT('',(-13.5471550458428,-1.46497727491618,0.00102478181900469));
#58059=CARTESIAN_POINT('',(-17.3,-1.4635,-1.79227059055215E-16));
#58060=CARTESIAN_POINT('Ctrl Pts',(-13.4758449541571,-1.46532338661684,
0.000837209389326979));
#58061=CARTESIAN_POINT('Ctrl Pts',(-13.4784918845211,-1.46565405334147,
0.0493450887578976));
#58062=CARTESIAN_POINT('Ctrl Pts',(-13.481138814885,-1.4634549955769,0.0978226187749106));
#58063=CARTESIAN_POINT('Ctrl Pts',(-13.4837857452489,-1.45862779591486,
0.146037020656259));
#58064=CARTESIAN_POINT('Ctrl Pts',(-13.5103002876546,-1.41027329748027,
0.629005073258751));
#58065=CARTESIAN_POINT('Ctrl Pts',(-13.5368148300603,-1.09820548856963,
1.08557029281694));
#58066=CARTESIAN_POINT('Ctrl Pts',(-13.563329372466,-0.665769554423191,
1.3060140729796));
#58067=CARTESIAN_POINT('Ctrl Pts',(-13.5898439148717,-0.233333620276776,
1.52645785314224));
#58068=CARTESIAN_POINT('Ctrl Pts',(-13.6163584572774,0.319470439105424,
1.51078019390938));
#58069=CARTESIAN_POINT('Ctrl Pts',(-13.6428729996831,0.73871768167217,1.26618246915778));
#58070=CARTESIAN_POINT('Ctrl Pts',(-13.6693875420888,1.15796492423892,1.02158474440618));
#58071=CARTESIAN_POINT('Ctrl Pts',(-13.6959020844944,1.44365534999021,0.548066954135844));
#58072=CARTESIAN_POINT('Ctrl Pts',(-13.7224166269001,1.46455995730734,0.0631346962416146));
#58073=CARTESIAN_POINT('Ctrl Pts',(-13.7489311693058,1.48546456462448,-0.421797561652615));
#58074=CARTESIAN_POINT('Ctrl Pts',(-13.7754457117115,1.24158335350746,-0.918144287170734));
#58075=CARTESIAN_POINT('Ctrl Pts',(-13.8019602541172,0.844940686565861,
-1.1979136423813));
#58076=CARTESIAN_POINT('Ctrl Pts',(-13.8284747965229,0.448298019624239,
-1.47768299759187));
#58077=CARTESIAN_POINT('Ctrl Pts',(-13.8549893389286,-0.101106103141984,
-1.54087498249487));
#58078=CARTESIAN_POINT('Ctrl Pts',(-13.8815038813343,-0.550908466108,-1.35846299927092));
#58079=CARTESIAN_POINT('Ctrl Pts',(-13.9080184237399,-1.00071082907399,
-1.17605101604698));
#58080=CARTESIAN_POINT('Ctrl Pts',(-13.9345329661456,-1.35091143223979,
-0.748035064696129));
#58081=CARTESIAN_POINT('Ctrl Pts',(-13.9610475085513,-1.44064917779694,
-0.271019934563134));
#58082=CARTESIAN_POINT('Ctrl Pts',(-13.9659799904199,-1.45734302814206,
-0.18228114192513));
#58083=CARTESIAN_POINT('Ctrl Pts',(-13.9709124722885,-1.46502306591684,
-0.0918466395122355));
#58084=CARTESIAN_POINT('Ctrl Pts',(-13.9758449541571,-1.46419415654471,
-0.00127194797176891));
#58085=CARTESIAN_POINT('Ctrl Pts',(-14.0471550458428,-1.46461493246388,
-0.00116358319217421));
#58086=CARTESIAN_POINT('Ctrl Pts',(-14.0430035474891,-1.46527684865318,
-0.0773404911163755));
#58087=CARTESIAN_POINT('Ctrl Pts',(-14.0388520491353,-1.45984897336895,
-0.153422846052185));
#58088=CARTESIAN_POINT('Ctrl Pts',(-14.0347005507816,-1.44800311557867,
-0.228492454152207));
#58089=CARTESIAN_POINT('Ctrl Pts',(-14.0081860083759,-1.37234669663114,
-0.70794255571478));
#58090=CARTESIAN_POINT('Ctrl Pts',(-13.9816714659702,-1.03489786137402,
-1.14608225467017));
#58091=CARTESIAN_POINT('Ctrl Pts',(-13.9551569235645,-0.590660312265092,
-1.34165652081483));
#58092=CARTESIAN_POINT('Ctrl Pts',(-13.9286423811588,-0.146422763156193,
-1.53723078695948));
#58093=CARTESIAN_POINT('Ctrl Pts',(-13.9021278387531,0.4046034998045,-1.49023962029342));
#58094=CARTESIAN_POINT('Ctrl Pts',(-13.8756132963474,0.809310147334135,
-1.22226793697292));
#58095=CARTESIAN_POINT('Ctrl Pts',(-13.8490987539418,1.21401679486377,-0.954296253652418));
#58096=CARTESIAN_POINT('Ctrl Pts',(-13.8225842115361,1.47240382696235,-0.465344053677463));
#58097=CARTESIAN_POINT('Ctrl Pts',(-13.7960696691304,1.46578377916778,0.0199934253858157));
#58098=CARTESIAN_POINT('Ctrl Pts',(-13.7695551267247,1.45916373137321,0.505330904449067));
#58099=CARTESIAN_POINT('Ctrl Pts',(-13.743040584319,1.18753660368553,0.987053662600641));
#58100=CARTESIAN_POINT('Ctrl Pts',(-13.7165260419133,0.775671564288337,
1.24388723310617));
#58101=CARTESIAN_POINT('Ctrl Pts',(-13.6900114995076,0.363806524891071,
1.50072080361175));
#58102=CARTESIAN_POINT('Ctrl Pts',(-13.663496957102,-0.188296426215764,
1.53266518647119));
#58103=CARTESIAN_POINT('Ctrl Pts',(-13.6369824146963,-0.62703439396149,
1.32504705317184));
#58104=CARTESIAN_POINT('Ctrl Pts',(-13.6104678722906,-1.06577236170717,
1.11742891987252));
#58105=CARTESIAN_POINT('Ctrl Pts',(-13.5839533298849,-1.39114534609176,
0.67024827041447));
#58106=CARTESIAN_POINT('Ctrl Pts',(-13.5574387874792,-1.45369656436799,
0.18891300398528));
#58107=CARTESIAN_POINT('Ctrl Pts',(-13.5540108736004,-1.46178345442188,
0.126683914193862));
#58108=CARTESIAN_POINT('Ctrl Pts',(-13.5505829597216,-1.46547742885513,
0.0638839494987724));
#58109=CARTESIAN_POINT('Ctrl Pts',(-13.5471550458428,-1.46497727491618,
0.00102478181900469));
#58110=CARTESIAN_POINT('Origin',(-17.3,0.,0.));
#58111=CARTESIAN_POINT('',(-12.9758449541571,-1.46158588710458,0.000857444751660996));
#58112=CARTESIAN_POINT('',(-13.0471550458428,-1.46136072574925,0.000659268984059629));
#58113=CARTESIAN_POINT('',(-17.3,-1.4635,-1.79227059055215E-16));
#58114=CARTESIAN_POINT('Ctrl Pts',(-12.9758449541571,-1.46158588710458,
0.000857444751660996));
#58115=CARTESIAN_POINT('Ctrl Pts',(-12.9860712967536,-1.46258854316142,
0.18949481438138));
#58116=CARTESIAN_POINT('Ctrl Pts',(-12.9962976393501,-1.42872174436519,
0.377785957761628));
#58117=CARTESIAN_POINT('Ctrl Pts',(-13.0065239819466,-1.35832380100528,
0.551251585068185));
#58118=CARTESIAN_POINT('Ctrl Pts',(-13.0330385243523,-1.17579820723828,
1.00100785792437));
#58119=CARTESIAN_POINT('Ctrl Pts',(-13.059553066758,-0.747693811761432,
1.35110033662373));
#58120=CARTESIAN_POINT('Ctrl Pts',(-13.0860676091637,-0.270656029832401,
1.44071758923565));
#58121=CARTESIAN_POINT('Ctrl Pts',(-13.1125821515694,0.206381752096632,
1.53033484184757));
#58122=CARTESIAN_POINT('Ctrl Pts',(-13.139096693975,0.732352920477846,1.35947686837204));
#58123=CARTESIAN_POINT('Ctrl Pts',(-13.1656112363807,1.06565794979205,1.00662554729284));
#58124=CARTESIAN_POINT('Ctrl Pts',(-13.1921257787864,1.39896297910629,0.653774226213604));
#58125=CARTESIAN_POINT('Ctrl Pts',(-13.2186403211921,1.53960186935347,0.118929557530643));
#58126=CARTESIAN_POINT('Ctrl Pts',(-13.2451548635978,1.42297357166271,-0.352232980805425));
#58127=CARTESIAN_POINT('Ctrl Pts',(-13.2716694060035,1.30634527397197,-0.823395519141413));
#58128=CARTESIAN_POINT('Ctrl Pts',(-13.2981839484092,0.932449788343379,
-1.23087592713053));
#58129=CARTESIAN_POINT('Ctrl Pts',(-13.3246984908148,0.473032216698865,
-1.38750220914511));
#58130=CARTESIAN_POINT('Ctrl Pts',(-13.3512130332205,0.0136146450543249,
-1.5441284911597));
#58131=CARTESIAN_POINT('Ctrl Pts',(-13.3777275756262,-0.531325012606148,
-1.44990064719972));
#58132=CARTESIAN_POINT('Ctrl Pts',(-13.4042421180319,-0.911474247457094,
-1.14810128239635));
#58133=CARTESIAN_POINT('Ctrl Pts',(-13.4281097300736,-1.25367341938933,
-0.876430361459512));
#58134=CARTESIAN_POINT('Ctrl Pts',(-13.4519773421154,-1.46234173466025,
-0.436562754549332));
#58135=CARTESIAN_POINT('Ctrl Pts',(-13.4758449541571,-1.46532338661684,
0.000837209389326979));
#58136=CARTESIAN_POINT('Ctrl Pts',(-13.5471550458428,-1.46497727491618,
0.00102478181900469));
#58137=CARTESIAN_POINT('Ctrl Pts',(-13.5240684173159,-1.46160879233375,
-0.422324901121936));
#58138=CARTESIAN_POINT('Ctrl Pts',(-13.500981788789,-1.26799982481547,-0.848359958356493));
#58139=CARTESIAN_POINT('Ctrl Pts',(-13.4778951602621,-0.944877167291941,
-1.12077159272548));
#58140=CARTESIAN_POINT('Ctrl Pts',(-13.4513806178565,-0.573777099771778,
-1.43363103960672));
#58141=CARTESIAN_POINT('Ctrl Pts',(-13.4248660754508,-0.0318475125635945,
-1.54386004996886));
#58142=CARTESIAN_POINT('Ctrl Pts',(-13.3983515330451,0.431981730862603,
-1.40082604506448));
#58143=CARTESIAN_POINT('Ctrl Pts',(-13.3718369906394,0.895810974288801,
-1.2577920401601));
#58144=CARTESIAN_POINT('Ctrl Pts',(-13.3453224482337,1.28153987393298,-0.861495019989192));
#58145=CARTESIAN_POINT('Ctrl Pts',(-13.318807905828,1.41198776907589,-0.3939700043279));
#58146=CARTESIAN_POINT('Ctrl Pts',(-13.2922933634223,1.54243566421881,0.0735550113334183));
#58147=CARTESIAN_POINT('Ctrl Pts',(-13.2657788210166,1.41760255486038,0.612308022485182));
#58148=CARTESIAN_POINT('Ctrl Pts',(-13.239264278611,1.0948292646106,0.974818293674386));
#58149=CARTESIAN_POINT('Ctrl Pts',(-13.2127497362053,0.772055974360851,
1.33732856486357));
#58150=CARTESIAN_POINT('Ctrl Pts',(-13.1862351937996,0.251342503219808,
1.52359609609029));
#58151=CARTESIAN_POINT('Ctrl Pts',(-13.1597206513939,-0.228126693234285,
1.44806078469242));
#58152=CARTESIAN_POINT('Ctrl Pts',(-13.1332061089882,-0.707595889688351,
1.37252547329456));
#58153=CARTESIAN_POINT('Ctrl Pts',(-13.1066915665825,-1.14582081145544,
1.03518731927217));
#58154=CARTESIAN_POINT('Ctrl Pts',(-13.0801770241769,-1.34150728209725,
0.590999184779553));
#58155=CARTESIAN_POINT('Ctrl Pts',(-13.0691696980655,-1.42274514639728,
0.406597599553718));
#58156=CARTESIAN_POINT('Ctrl Pts',(-13.0581623719542,-1.46218303840703,
0.203781094128016));
#58157=CARTESIAN_POINT('Ctrl Pts',(-13.0471550458428,-1.46136072574925,
0.000659268984059629));
#58158=CARTESIAN_POINT('Origin',(-17.3,0.,0.));
#58159=CARTESIAN_POINT('',(-12.4758449541571,-1.46218187472528,-0.00116212229894885));
#58160=CARTESIAN_POINT('',(-12.5471550458428,-1.46255548750974,-0.00126727998485326));
#58161=CARTESIAN_POINT('',(-17.3,-1.4635,-1.79227059055215E-16));
#58162=CARTESIAN_POINT('Ctrl Pts',(-12.4758449541571,-1.46218187472528,
-0.00116212229894885));
#58163=CARTESIAN_POINT('Ctrl Pts',(-12.4936507089862,-1.45975393531768,
0.326950644416945));
#58164=CARTESIAN_POINT('Ctrl Pts',(-12.5114564638152,-1.35060787521459,
0.656527436918317));
#58165=CARTESIAN_POINT('Ctrl Pts',(-12.5292622186442,-1.14787101490285,
0.911764219282333));
#58166=CARTESIAN_POINT('Ctrl Pts',(-12.5557767610499,-0.845975637169948,
1.29183720997888));
#58167=CARTESIAN_POINT('Ctrl Pts',(-12.5822913034556,-0.336550369915331,
1.50706735227095));
#58168=CARTESIAN_POINT('Ctrl Pts',(-12.6088058458613,0.146405453332879,
1.45859086163736));
#58169=CARTESIAN_POINT('Ctrl Pts',(-12.635320388267,0.62936127658109,1.41011437100376));
#58170=CARTESIAN_POINT('Ctrl Pts',(-12.6618349306727,1.08584765582289,1.09793124744451));
#58171=CARTESIAN_POINT('Ctrl Pts',(-12.6883494730784,1.30618219920735,0.665439644814965));
#58172=CARTESIAN_POINT('Ctrl Pts',(-12.714864015484,1.52651674259176,0.232948042185496));
#58173=CARTESIAN_POINT('Ctrl Pts',(-12.7413785578897,1.51069945011893,-0.319852039514211));
#58174=CARTESIAN_POINT('Ctrl Pts',(-12.7678931002954,1.26599583477921,-0.739037485341109));
#58175=CARTESIAN_POINT('Ctrl Pts',(-12.7944076427011,1.02129221943944,-1.15822293116808));
#58176=CARTESIAN_POINT('Ctrl Pts',(-12.8209221851068,0.547702281232709,
-1.44379374112219));
#58177=CARTESIAN_POINT('Ctrl Pts',(-12.8474367275125,0.0627647584772496,
-1.46457585788886));
#58178=CARTESIAN_POINT('Ctrl Pts',(-12.8739512699182,-0.42217276427821,
-1.48535797465554));
#58179=CARTESIAN_POINT('Ctrl Pts',(-12.9004658123239,-0.918457871582393,
-1.24135139823478));
#58180=CARTESIAN_POINT('Ctrl Pts',(-12.9269803547296,-1.19812702920591,
-0.844638076517884));
#58181=CARTESIAN_POINT('Ctrl Pts',(-12.9432685545387,-1.36993113014577,
-0.600932348837367));
#58182=CARTESIAN_POINT('Ctrl Pts',(-12.9595567543479,-1.45998888778252,
-0.299598279180735));
#58183=CARTESIAN_POINT('Ctrl Pts',(-12.9758449541571,-1.46158588710458,
0.000857444751660996));
#58184=CARTESIAN_POINT('Ctrl Pts',(-13.0471550458428,-1.46136072574925,
0.000659268984059629));
#58185=CARTESIAN_POINT('Ctrl Pts',(-13.0316478295485,-1.46020224455984,
-0.285500516303598));
#58186=CARTESIAN_POINT('Ctrl Pts',(-13.0161406132541,-1.3791376512242,-0.572266282406523));
#58187=CARTESIAN_POINT('Ctrl Pts',(-13.0006333969598,-1.2224723230406,-0.809001386729198));
#58188=CARTESIAN_POINT('Ctrl Pts',(-12.9741188545541,-0.954602873825676,
-1.21377570878235));
#58189=CARTESIAN_POINT('Ctrl Pts',(-12.9476043121484,-0.465715955879361,
-1.4722862379258));
#58190=CARTESIAN_POINT('Ctrl Pts',(-12.9210897697427,0.0196231798704193,
-1.46578878258152));
#58191=CARTESIAN_POINT('Ctrl Pts',(-12.894575227337,0.5049623156202,-1.45929132723724));
#58192=CARTESIAN_POINT('Ctrl Pts',(-12.8680606849314,0.986753669173477,
-1.18778588740522));
#58193=CARTESIAN_POINT('Ctrl Pts',(-12.8415461425257,1.24369126519327,-0.775985735185896));
#58194=CARTESIAN_POINT('Ctrl Pts',(-12.81503160012,1.50062886121308,-0.364185582966545));
#58195=CARTESIAN_POINT('Ctrl Pts',(-12.7885170577143,1.53271269969942,0.187909281640078));
#58196=CARTESIAN_POINT('Ctrl Pts',(-12.7620025153086,1.32520539461077,0.62669967801535));
#58197=CARTESIAN_POINT('Ctrl Pts',(-12.7354879729029,1.11769808952214,1.0654900743906));
#58198=CARTESIAN_POINT('Ctrl Pts',(-12.7089734304972,0.670599640858534,
1.39097600253446));
#58199=CARTESIAN_POINT('Ctrl Pts',(-12.6824588880916,0.189280189705736,
1.45364880012849));
#58200=CARTESIAN_POINT('Ctrl Pts',(-12.6559443456859,-0.292039261447089,
1.51632159772253));
#58201=CARTESIAN_POINT('Ctrl Pts',(-12.6294298032802,-0.807579715089139,
1.31618126476671));
#58202=CARTESIAN_POINT('Ctrl Pts',(-12.6029152608745,-1.12053288880213,
0.945160234797672));
#58203=CARTESIAN_POINT('Ctrl Pts',(-12.5843285225306,-1.3399135842971,0.685073875448221));
#58204=CARTESIAN_POINT('Ctrl Pts',(-12.5657417841867,-1.45974221525453,
0.341016172077363));
#58205=CARTESIAN_POINT('Ctrl Pts',(-12.5471550458428,-1.46255548750974,
-0.00126727998485326));
#58206=CARTESIAN_POINT('Origin',(-17.3,0.,0.));
#58207=CARTESIAN_POINT('',(-11.9758449541571,-1.46579906277062,-0.000383257489619121));
#58208=CARTESIAN_POINT('',(-12.0471550458428,-1.4659079907007,-0.000120015143960721));
#58209=CARTESIAN_POINT('',(-17.3,-1.4635,-1.79227059055215E-16));
#58210=CARTESIAN_POINT('Ctrl Pts',(-11.9758449541571,-1.46579906277062,
-0.000383257489619121));
#58211=CARTESIAN_POINT('Ctrl Pts',(-12.0012301212187,-1.46417694847208,
0.464427706910453));
#58212=CARTESIAN_POINT('Ctrl Pts',(-12.0266152882803,-1.22421852479684,
0.930679514285422));
#58213=CARTESIAN_POINT('Ctrl Pts',(-12.0520004553419,-0.844335412579876,
1.19834033958687));
#58214=CARTESIAN_POINT('Ctrl Pts',(-12.0785149977476,-0.44755146139907,
1.47790928177972));
#58215=CARTESIAN_POINT('Ctrl Pts',(-12.1050295401533,0.10188451480633,1.54082370873951));
#58216=CARTESIAN_POINT('Ctrl Pts',(-12.1315440825589,0.55159466885709,1.35818451607506));
#58217=CARTESIAN_POINT('Ctrl Pts',(-12.1580586249646,1.00130482290782,1.17554532341062));
#58218=CARTESIAN_POINT('Ctrl Pts',(-12.1845731673703,1.35128915480393,0.747352511121983));
#58219=CARTESIAN_POINT('Ctrl Pts',(-12.211087709776,1.44078590875282,0.270292107833193));
#58220=CARTESIAN_POINT('Ctrl Pts',(-12.2376022521817,1.53028266270173,-0.206768295455678));
#58221=CARTESIAN_POINT('Ctrl Pts',(-12.2641167945874,1.35929183870333,-0.732696289744717));
#58222=CARTESIAN_POINT('Ctrl Pts',(-12.2906313369931,1.00635633878264,-1.06591218109636));
#58223=CARTESIAN_POINT('Ctrl Pts',(-12.3171458793988,0.653420838862003,
-1.39912807244797));
#58224=CARTESIAN_POINT('Ctrl Pts',(-12.3436604218044,0.118540663019128,
-1.53963186086222));
#58225=CARTESIAN_POINT('Ctrl Pts',(-12.3701749642101,-0.352592400941366,
-1.42288455512596));
#58226=CARTESIAN_POINT('Ctrl Pts',(-12.3966895066158,-0.823725464901861,
-1.3061372493897));
#58227=CARTESIAN_POINT('Ctrl Pts',(-12.4232040490215,-1.23111141697998,
-0.932138849502929));
#58228=CARTESIAN_POINT('Ctrl Pts',(-12.4497185914272,-1.38762164891344,
-0.472681730009051));
#58229=CARTESIAN_POINT('Ctrl Pts',(-12.4584273790038,-1.43902794296241,
-0.321771546720627));
#58230=CARTESIAN_POINT('Ctrl Pts',(-12.4671361665805,-1.46336937892,-0.161641945476957));
#58231=CARTESIAN_POINT('Ctrl Pts',(-12.4758449541571,-1.46218187472528,
-0.00116212229894885));
#58232=CARTESIAN_POINT('Ctrl Pts',(-12.5471550458428,-1.46255548750974,
-0.00126727998485326));
#58233=CARTESIAN_POINT('Ctrl Pts',(-12.539227241781,-1.46375543291163,-0.147261487862684));
#58234=CARTESIAN_POINT('Ctrl Pts',(-12.5312994377192,-1.4436670130256,-0.292932909822579));
#58235=CARTESIAN_POINT('Ctrl Pts',(-12.5233716336574,-1.40093511539405,
-0.431627879991432));
#58236=CARTESIAN_POINT('Ctrl Pts',(-12.4968570912518,-1.25801827448904,
-0.895493237829282));
#58237=CARTESIAN_POINT('Ctrl Pts',(-12.4703425488461,-0.861818698895064,
-1.28132222652273));
#58238=CARTESIAN_POINT('Ctrl Pts',(-12.4438280064404,-0.394326648209448,
-1.41188821046213));
#58239=CARTESIAN_POINT('Ctrl Pts',(-12.4173134640347,0.0731654024761946,
-1.54245419440153));
#58240=CARTESIAN_POINT('Ctrl Pts',(-12.390798921629,0.611949928253461,-1.41775717358684));
#58241=CARTESIAN_POINT('Ctrl Pts',(-12.3642843792233,0.974541717745663,
-1.09507546073473));
#58242=CARTESIAN_POINT('Ctrl Pts',(-12.3377698368176,1.33713350723782,-0.772393747882646));
#58243=CARTESIAN_POINT('Ctrl Pts',(-12.3112552944119,1.52353256044495,-0.251727342993118));
#58244=CARTESIAN_POINT('Ctrl Pts',(-12.2847407520063,1.44811836141617,0.227760917761126));
#58245=CARTESIAN_POINT('Ctrl Pts',(-12.2582262096006,1.37270416238738,0.707249178515397));
#58246=CARTESIAN_POINT('Ctrl Pts',(-12.2317116671949,1.0354767111227,1.14555929513442));
#58247=CARTESIAN_POINT('Ctrl Pts',(-12.2051971247892,0.591338019586661,
1.34135795778807));
#58248=CARTESIAN_POINT('Ctrl Pts',(-12.1786825823835,0.147199328050593,
1.53715662044173));
#58249=CARTESIAN_POINT('Ctrl Pts',(-12.1521680399778,-0.403850603756823,
1.49044382912997));
#58250=CARTESIAN_POINT('Ctrl Pts',(-12.1256534975721,-0.808692574507879,
1.22267663111137));
#58251=CARTESIAN_POINT('Ctrl Pts',(-12.0994873469957,-1.20821506311994,
0.958427800579785));
#58252=CARTESIAN_POINT('Ctrl Pts',(-12.0733211964193,-1.46534659092428,
0.478895553643603));
#58253=CARTESIAN_POINT('Ctrl Pts',(-12.0471550458428,-1.4659079907007,-0.000120015143960721));
#58254=CARTESIAN_POINT('Origin',(-17.3,0.,0.));
#58255=CARTESIAN_POINT('',(-11.4758449541571,-1.4633442613986,0.00135246097216248));
#58256=CARTESIAN_POINT('',(-11.5471550458429,-1.46291715073871,0.0013268560893039));
#58257=CARTESIAN_POINT('',(-17.3,-1.4635,-1.79227059055215E-16));
#58258=CARTESIAN_POINT('Ctrl Pts',(-11.4758449541571,-1.4633442613986,0.00135246097216248));
#58259=CARTESIAN_POINT('Ctrl Pts',(-11.4822949910456,-1.46443170060753,
0.119970375014325));
#58260=CARTESIAN_POINT('Ctrl Pts',(-11.488745027934,-1.45122482725057,0.238349204626237));
#58261=CARTESIAN_POINT('Ctrl Pts',(-11.4951950648225,-1.42279544780548,
0.352951798581079));
#58262=CARTESIAN_POINT('Ctrl Pts',(-11.5217096072281,-1.30592914147246,
0.824055358106536));
#58263=CARTESIAN_POINT('Ctrl Pts',(-11.5482241496338,-0.931827851189581,
1.23134682828133));
#58264=CARTESIAN_POINT('Ctrl Pts',(-11.5747386920395,-0.472331213160919,
1.38774100014792));
#58265=CARTESIAN_POINT('Ctrl Pts',(-11.6012532344452,-0.0128345751322309,
1.54413517201451));
#58266=CARTESIAN_POINT('Ctrl Pts',(-11.6277677768509,0.532057410642251,
1.44963204557287));
#58267=CARTESIAN_POINT('Ctrl Pts',(-11.6542823192566,0.912054132934719,
1.14764067417215));
#58268=CARTESIAN_POINT('Ctrl Pts',(-11.6807968616623,1.29205085522717,0.84564930277145));
#58269=CARTESIAN_POINT('Ctrl Pts',(-11.707311404068,1.50715231403762,0.336169686411701));
#58270=CARTESIAN_POINT('Ctrl Pts',(-11.7338259464736,1.45855383429798,-0.146773876668371));
#58271=CARTESIAN_POINT('Ctrl Pts',(-11.7603404888793,1.40995535455835,-0.629717439748443));
#58272=CARTESIAN_POINT('Ctrl Pts',(-11.786855031285,1.09765693626862,-1.08612494954884));
#58273=CARTESIAN_POINT('Ctrl Pts',(-11.8133695736907,0.665109692750116,
-1.30635024209722));
#58274=CARTESIAN_POINT('Ctrl Pts',(-11.8398841160964,0.232562449231607,
-1.52657553464559));
#58275=CARTESIAN_POINT('Ctrl Pts',(-11.8663986585021,-0.320233619515688,
-1.51061860994196));
#58276=CARTESIAN_POINT('Ctrl Pts',(-11.8929132009078,-0.739357241857687,
-1.26580911962673));
#58277=CARTESIAN_POINT('Ctrl Pts',(-11.9194277433135,-1.15848086419971,
-1.02099962931149));
#58278=CARTESIAN_POINT('Ctrl Pts',(-11.9459422857191,-1.44393204013642,
-0.547337573384642));
#58279=CARTESIAN_POINT('Ctrl Pts',(-11.9724568281248,-1.46459166502666,
-0.0623948167082485));
#58280=CARTESIAN_POINT('Ctrl Pts',(-11.9735862034689,-1.46547165271841,
-0.041738891959084));
#58281=CARTESIAN_POINT('Ctrl Pts',(-11.974715578813,-1.46587122994957,-0.0210625006707822));
#58282=CARTESIAN_POINT('Ctrl Pts',(-11.9758449541571,-1.46579906277062,
-0.000383257489619121));
#58283=CARTESIAN_POINT('Ctrl Pts',(-12.0471550458428,-1.4659079907007,-0.000120015143960721));
#58284=CARTESIAN_POINT('Ctrl Pts',(-12.0468066540136,-1.46591546551418,
-0.00649791585064298));
#58285=CARTESIAN_POINT('Ctrl Pts',(-12.0464582621843,-1.46587745594124,
-0.01287572496136));
#58286=CARTESIAN_POINT('Ctrl Pts',(-12.0461098703551,-1.46579369247414,
-0.0192529331030128));
#58287=CARTESIAN_POINT('Ctrl Pts',(-12.0195953279494,-1.4594188299947,-0.50459369457341));
#58288=CARTESIAN_POINT('Ctrl Pts',(-11.9930807855437,-1.18803509534114,
-0.986453612788815));
#58289=CARTESIAN_POINT('Ctrl Pts',(-11.966566243138,-0.776299856573628,
-1.24349521792961));
#58290=CARTESIAN_POINT('Ctrl Pts',(-11.9400517007323,-0.364564617806093,
-1.50053682307042));
#58291=CARTESIAN_POINT('Ctrl Pts',(-11.9135371583266,0.187522125075435,
-1.5327601151366));
#58292=CARTESIAN_POINT('Ctrl Pts',(-11.8870226159209,0.6263649220843,-1.3253636514981));
#58293=CARTESIAN_POINT('Ctrl Pts',(-11.8605080735153,1.06520771909314,-1.11796718785961));
#58294=CARTESIAN_POINT('Ctrl Pts',(-11.8339935311096,1.39080657022936,-0.670950968516453));
#58295=CARTESIAN_POINT('Ctrl Pts',(-11.8074789887039,1.45360094314246,-0.189647363349462));
#58296=CARTESIAN_POINT('Ctrl Pts',(-11.7809644462982,1.51639531605555,0.291656241817557));
#58297=CARTESIAN_POINT('Ctrl Pts',(-11.7544499038925,1.31638521074554,0.807247232808381));
#58298=CARTESIAN_POINT('Ctrl Pts',(-11.7279353614868,0.945443241999734,
1.12029411338589));
#58299=CARTESIAN_POINT('Ctrl Pts',(-11.7014208190811,0.574501273253951,
1.43334099396338));
#58300=CARTESIAN_POINT('Ctrl Pts',(-11.6749062766755,0.0326274410723951,
1.54384376412751));
#58301=CARTESIAN_POINT('Ctrl Pts',(-11.6483917342698,-0.431274001581286,
1.40104409634033));
#58302=CARTESIAN_POINT('Ctrl Pts',(-11.6218771918641,-0.895175444234968,
1.25824442855316));
#58303=CARTESIAN_POINT('Ctrl Pts',(-11.5953626494584,-1.2811044973608,0.862142322814663));
#58304=CARTESIAN_POINT('Ctrl Pts',(-11.5688481070527,-1.41178856176624,
0.394683266931935));
#58305=CARTESIAN_POINT('Ctrl Pts',(-11.5616170866494,-1.44742859362655,
0.26719828457506));
#58306=CARTESIAN_POINT('Ctrl Pts',(-11.5543860662461,-1.46408460799211,
0.134406081117774));
#58307=CARTESIAN_POINT('Ctrl Pts',(-11.5471550458429,-1.46291715073871,
0.0013268560893039));
#58308=CARTESIAN_POINT('Origin',(-17.3,0.,0.));
#58309=CARTESIAN_POINT('',(-10.9758449541571,-1.46111006519219,-0.000234854365275122));
#58310=CARTESIAN_POINT('',(-11.0471550458429,-1.46121285057659,-0.000465323571519086));
#58311=CARTESIAN_POINT('',(-17.3,-1.4635,-1.79227059055215E-16));
#58312=CARTESIAN_POINT('Ctrl Pts',(-10.9758449541571,-1.46111006519219,
-0.000234854365275122));
#58313=CARTESIAN_POINT('Ctrl Pts',(-10.9898744032781,-1.4607403045662,0.258766084230319));
#58314=CARTESIAN_POINT('Ctrl Pts',(-11.0039038523991,-1.39521262116459,
0.51794180976467));
#58315=CARTESIAN_POINT('Ctrl Pts',(-11.0179333015201,-1.2656223237124,0.739676951201287));
#58316=CARTESIAN_POINT('Ctrl Pts',(-11.0444478439258,-1.0207069740412,1.15873872331721));
#58317=CARTESIAN_POINT('Ctrl Pts',(-11.0709623863315,-0.546972830615103,
1.44407024702402));
#58318=CARTESIAN_POINT('Ctrl Pts',(-11.0974769287372,-0.0620248709583785,
1.4646073787197));
#58319=CARTESIAN_POINT('Ctrl Pts',(-11.1239914711428,0.422923088698319,
1.48514451041539));
#58320=CARTESIAN_POINT('Ctrl Pts',(-11.1505060135485,0.919084864585646,
1.24088725009997));
#58321=CARTESIAN_POINT('Ctrl Pts',(-11.1770205559542,1.19855357351062,0.844032694771085));
#58322=CARTESIAN_POINT('Ctrl Pts',(-11.2035350983599,1.47802228243559,0.447178139442197));
#58323=CARTESIAN_POINT('Ctrl Pts',(-11.2300496407656,1.5407979243982,-0.102273710900164));
#58324=CARTESIAN_POINT('Ctrl Pts',(-11.2565641831713,1.35804514448916,-0.551937717452828));
#58325=CARTESIAN_POINT('Ctrl Pts',(-11.283078725577,1.1752923645801,-1.00160172400552));
#58326=CARTESIAN_POINT('Ctrl Pts',(-11.3095932679827,0.747011162799363,
-1.3514778867685));
#58327=CARTESIAN_POINT('Ctrl Pts',(-11.3361078103883,0.269928168588406,
-1.44085413634418));
#58328=CARTESIAN_POINT('Ctrl Pts',(-11.362622352794,-0.207154825622524,
-1.53023038591984));
#58329=CARTESIAN_POINT('Ctrl Pts',(-11.3891368951997,-0.733039612263668,
-1.35910672230823));
#58330=CARTESIAN_POINT('Ctrl Pts',(-11.4156514376054,-1.06616634439266,
-1.00608706606436));
#58331=CARTESIAN_POINT('Ctrl Pts',(-11.4357159431226,-1.31825529439125,
-0.738944426677143));
#58332=CARTESIAN_POINT('Ctrl Pts',(-11.4557804486399,-1.459961500899,-0.367639194719911));
#58333=CARTESIAN_POINT('Ctrl Pts',(-11.4758449541571,-1.4633442613986,0.00135246097216248));
#58334=CARTESIAN_POINT('Ctrl Pts',(-11.5471550458429,-1.46291715073871,
0.0013268560893039));
#58335=CARTESIAN_POINT('Ctrl Pts',(-11.5278715238405,-1.45980380208567,
-0.3535658175273));
#58336=CARTESIAN_POINT('Ctrl Pts',(-11.5085880018381,-1.32993523721296,
-0.710499702984862));
#58337=CARTESIAN_POINT('Ctrl Pts',(-11.4893044798357,-1.09532158699014,
-0.974265079638717));
#58338=CARTESIAN_POINT('Ctrl Pts',(-11.46278993743,-0.772731472123592,-1.3369383642996));
#58339=CARTESIAN_POINT('Ctrl Pts',(-11.4362753950243,-0.252112166705467,
-1.52346892759434));
#58340=CARTESIAN_POINT('Ctrl Pts',(-11.4097608526186,0.227395127756395,
-1.44817584574619));
#58341=CARTESIAN_POINT('Ctrl Pts',(-11.3832463102129,0.706902422218231,
-1.37288276389804));
#58342=CARTESIAN_POINT('Ctrl Pts',(-11.3567317678072,1.14529770572381,-1.03576603690705));
#58343=CARTESIAN_POINT('Ctrl Pts',(-11.3302172254015,1.3412085478968,-0.591676816664797));
#58344=CARTESIAN_POINT('Ctrl Pts',(-11.3037026829959,1.53711939006979,-0.147587596422573));
#58345=CARTESIAN_POINT('Ctrl Pts',(-11.2771881405902,1.49054579091022,0.403474117070884));
#58346=CARTESIAN_POINT('Ctrl Pts',(-11.2506735981845,1.22288086117226,0.808383710689811));
#58347=CARTESIAN_POINT('Ctrl Pts',(-11.2241590557788,0.955215931434269,
1.21329330430878));
#58348=CARTESIAN_POINT('Ctrl Pts',(-11.1976445133731,0.466459671117826,
1.47205077805319));
#58349=CARTESIAN_POINT('Ctrl Pts',(-11.1711299709674,-0.0188826851072191,
1.46579850884533));
#58350=CARTESIAN_POINT('Ctrl Pts',(-11.1446154285617,-0.504225041332237,
1.45954623963746));
#58351=CARTESIAN_POINT('Ctrl Pts',(-11.118100886156,-0.986153493465858,
1.18828422747734));
#58352=CARTESIAN_POINT('Ctrl Pts',(-11.0915863437504,-1.24329909132773,
0.776613928431419));
#58353=CARTESIAN_POINT('Ctrl Pts',(-11.0767759111145,-1.38693489301208,
0.546664071522495));
#58354=CARTESIAN_POINT('Ctrl Pts',(-11.0619654784787,-1.46043640562047,
0.272905555750272));
#58355=CARTESIAN_POINT('Ctrl Pts',(-11.0471550458429,-1.46121285057659,
-0.000465323571519086));
#58356=CARTESIAN_POINT('Origin',(-17.3,0.,0.));
#58357=CARTESIAN_POINT('',(-10.4758449541571,-1.46420894404091,-0.00126897030766321));
#58358=CARTESIAN_POINT('',(-10.5471550458429,-1.4646289090495,-0.00115908444552544));
#58359=CARTESIAN_POINT('',(-17.3,-1.4635,-1.79227059055215E-16));
#58360=CARTESIAN_POINT('Ctrl Pts',(-10.4758449541571,-1.46420894404091,
-0.00126897030766321));
#58361=CARTESIAN_POINT('Ctrl Pts',(-10.4974538155107,-1.46058180138299,
0.395522140978942));
#58362=CARTESIAN_POINT('Ctrl Pts',(-10.5190626768642,-1.29359078311601,
0.795000998625229));
#58363=CARTESIAN_POINT('Ctrl Pts',(-10.5406715382178,-1.00581772915512,
1.06642043966479));
#58364=CARTESIAN_POINT('Ctrl Pts',(-10.5671860806234,-0.652713939111602,
1.39945799131682));
#58365=CARTESIAN_POINT('Ctrl Pts',(-10.5937006230291,-0.117762851331239,
1.53969154918036));
#58366=CARTESIAN_POINT('Ctrl Pts',(-10.6202151654348,0.353311173701554,
1.42270624970696));
#58367=CARTESIAN_POINT('Ctrl Pts',(-10.6467297078405,0.824385198734346,
1.30572095023355));
#58368=CARTESIAN_POINT('Ctrl Pts',(-10.6732442502462,1.23158216101957,0.931516793423203));
#58369=CARTESIAN_POINT('Ctrl Pts',(-10.6997587926519,1.38786026284093,0.471980666176833));
#58370=CARTESIAN_POINT('Ctrl Pts',(-10.7262733350576,1.54413836466229,0.0124445389304362));
#58371=CARTESIAN_POINT('Ctrl Pts',(-10.7527878774632,1.44949760601975,-0.532423558751993));
#58372=CARTESIAN_POINT('Ctrl Pts',(-10.7793024198689,1.14741026021906,-0.912343988395626));
#58373=CARTESIAN_POINT('Ctrl Pts',(-10.8058169622746,0.845322914418391,
-1.29226441803924));
#58374=CARTESIAN_POINT('Ctrl Pts',(-10.8323315046803,0.335788981459602,
-1.50723717964407));
#58375=CARTESIAN_POINT('Ctrl Pts',(-10.858846047086,-0.147142290639309,
-1.4585167138991));
#58376=CARTESIAN_POINT('Ctrl Pts',(-10.8853605894917,-0.630073562738247,
-1.40979624815412));
#58377=CARTESIAN_POINT('Ctrl Pts',(-10.9118751318974,-1.0864021739773,-1.09738255505932));
#58378=CARTESIAN_POINT('Ctrl Pts',(-10.938389674303,-1.30651820163863,-0.664779698249398));
#58379=CARTESIAN_POINT('Ctrl Pts',(-10.9508747675877,-1.41016581873719,
-0.461076879627928));
#58380=CARTESIAN_POINT('Ctrl Pts',(-10.9633598608724,-1.46143912272459,
-0.230725078985094));
#58381=CARTESIAN_POINT('Ctrl Pts',(-10.9758449541571,-1.46111006519219,
-0.000234854365275122));
#58382=CARTESIAN_POINT('Ctrl Pts',(-11.0471550458429,-1.46121285057659,
-0.000465323571519086));
#58383=CARTESIAN_POINT('Ctrl Pts',(-11.035450936073,-1.46182644487326,-0.216499713527323));
#58384=CARTESIAN_POINT('Ctrl Pts',(-11.0237468263032,-1.41702231000271,
-0.432292019592519));
#58385=CARTESIAN_POINT('Ctrl Pts',(-11.0120427165333,-1.32552182382382,
-0.62603012618947));
#58386=CARTESIAN_POINT('Ctrl Pts',(-10.9855281741276,-1.11823621486794,
-1.0649252958326));
#58387=CARTESIAN_POINT('Ctrl Pts',(-10.9590136317219,-0.671302253366116,
-1.39063704918714));
#58388=CARTESIAN_POINT('Ctrl Pts',(-10.9324990893162,-0.19001452489336,
-1.4535529934129));
#58389=CARTESIAN_POINT('Ctrl Pts',(-10.9059845469106,0.291273203579423,
-1.51646893763866));
#58390=CARTESIAN_POINT('Ctrl Pts',(-10.8794700045049,0.806914699023168,
-1.31658907273557));
#58391=CARTESIAN_POINT('Ctrl Pts',(-10.8529554620992,1.12005526649198,-0.945726188880069));
#58392=CARTESIAN_POINT('Ctrl Pts',(-10.8264409196935,1.4331958339608,-0.574863305024572));
#58393=CARTESIAN_POINT('Ctrl Pts',(-10.7999263772878,1.54383547345474,-0.0330174022166808));
#58394=CARTESIAN_POINT('Ctrl Pts',(-10.7734118348821,1.40115298789638,0.430920095654743));
#58395=CARTESIAN_POINT('Ctrl Pts',(-10.7468972924764,1.25847050233803,0.89485759352614));
#58396=CARTESIAN_POINT('Ctrl Pts',(-10.7203827500707,0.862465891727416,
1.28088668646104));
#58397=CARTESIAN_POINT('Ctrl Pts',(-10.6938682076651,0.395039860472687,
1.41168882299456));
#58398=CARTESIAN_POINT('Ctrl Pts',(-10.6673536652594,-0.0723861707820682,
1.54249095952808));
#58399=CARTESIAN_POINT('Ctrl Pts',(-10.6408391228537,-0.611233622681002,
1.41806613966014));
#58400=CARTESIAN_POINT('Ctrl Pts',(-10.614324580448,-0.973988379371074,
1.09556764336126));
#58401=CARTESIAN_POINT('Ctrl Pts',(-10.5919347355796,-1.28031170199486,
0.8232381725396));
#58402=CARTESIAN_POINT('Ctrl Pts',(-10.5695448907112,-1.46106810598496,
0.409667742333545));
#58403=CARTESIAN_POINT('Ctrl Pts',(-10.5471550458429,-1.4646289090495,-0.00115908444552544));
#58404=CARTESIAN_POINT('Origin',(-17.3,0.,0.));
#58405=CARTESIAN_POINT('',(-9.97584495415713,-1.46531245936081,0.000844241415329933));
#58406=CARTESIAN_POINT('',(-10.0471550458429,-1.46496448118167,0.00103054806325355));
#58407=CARTESIAN_POINT('',(-17.3,-1.4635,-1.79227059055215E-16));
#58408=CARTESIAN_POINT('Ctrl Pts',(-9.97584495415713,-1.46531245936081,
0.000844241415329933));
#58409=CARTESIAN_POINT('Ctrl Pts',(-9.97851868533753,-1.46564870303239,
0.0498442363565879));
#58410=CARTESIAN_POINT('Ctrl Pts',(-9.98119241651793,-1.46340478166659,
0.098813062229553));
#58411=CARTESIAN_POINT('Ctrl Pts',(-9.98386614769833,-1.45847950044308,
0.147510695222105));
#58412=CARTESIAN_POINT('Ctrl Pts',(-10.010380690104,-1.40963705180129,0.630429645527651));
#58413=CARTESIAN_POINT('Ctrl Pts',(-10.0368952325097,-1.09710810383422,
1.08667932909043));
#58414=CARTESIAN_POINT('Ctrl Pts',(-10.0634097749154,-0.664449661334089,
1.30668607782077));
#58415=CARTESIAN_POINT('Ctrl Pts',(-10.0899243173211,-0.231791218834003,
1.52669282655109));
#58416=CARTESIAN_POINT('Ctrl Pts',(-10.1164388597268,0.320996718199095,
1.51045664044901));
#58417=CARTESIAN_POINT('Ctrl Pts',(-10.1429534021325,0.739996613351653,
1.26543544704805));
#58418=CARTESIAN_POINT('Ctrl Pts',(-10.1694679445381,1.15899650850421,1.02041425364709));
#58419=CARTESIAN_POINT('Ctrl Pts',(-10.1959824869438,1.4442083617762,0.546608052947263));
#58420=CARTESIAN_POINT('Ctrl Pts',(-10.2224970293495,1.46462299896701,0.0616549212511626));
#58421=CARTESIAN_POINT('Ctrl Pts',(-10.2490115717552,1.48503763615782,-0.42329821044491));
#58422=CARTESIAN_POINT('Ctrl Pts',(-10.2755261141609,1.24065505726743,-0.919398273137288));
#58423=CARTESIAN_POINT('Ctrl Pts',(-10.3020406565666,0.843729923110822,
-1.19876673096354));
#58424=CARTESIAN_POINT('Ctrl Pts',(-10.3285551989723,0.446804788954149,
-1.47813518878984));
#58425=CARTESIAN_POINT('Ctrl Pts',(-10.355069741378,-0.102662900468787,
-1.54077204175001));
#58426=CARTESIAN_POINT('Ctrl Pts',(-10.3815842837836,-0.552280730833664,
-1.35790568625639));
#58427=CARTESIAN_POINT('Ctrl Pts',(-10.4080988261893,-1.00189856119844,
-1.17503933076282));
#58428=CARTESIAN_POINT('Ctrl Pts',(-10.434613368595,-1.35166653250518,-0.746669766815594));
#58429=CARTESIAN_POINT('Ctrl Pts',(-10.4611279110007,-1.44092227200526,
-0.269564212121746));
#58430=CARTESIAN_POINT('Ctrl Pts',(-10.4660335920528,-1.45743623567702,
-0.181290854666609));
#58431=CARTESIAN_POINT('Ctrl Pts',(-10.470939273105,-1.46503238423608,-0.0913491741857221));
#58432=CARTESIAN_POINT('Ctrl Pts',(-10.4758449541571,-1.46420894404091,
-0.00126897030766321));
#58433=CARTESIAN_POINT('Ctrl Pts',(-10.5471550458429,-1.4646289090495,-0.00115908444552544));
#58434=CARTESIAN_POINT('Ctrl Pts',(-10.5430303483055,-1.46528488660171,
-0.0768423422186303));
#58435=CARTESIAN_POINT('Ctrl Pts',(-10.5389056507682,-1.45992725800098,
-0.152432488479017));
#58436=CARTESIAN_POINT('Ctrl Pts',(-10.5347809532309,-1.44823323767887,
-0.227029323243103));
#58437=CARTESIAN_POINT('Ctrl Pts',(-10.5082664108253,-1.37306127781532,
-0.706555620818703));
#58438=CARTESIAN_POINT('Ctrl Pts',(-10.4817518684196,-1.03605529660695,
-1.14503604324013));
#58439=CARTESIAN_POINT('Ctrl Pts',(-10.4552373260139,-0.592015575992571,
-1.3410590524329));
#58440=CARTESIAN_POINT('Ctrl Pts',(-10.4287227836082,-0.147975855378186,
-1.53708206162567));
#58441=CARTESIAN_POINT('Ctrl Pts',(-10.4022082412025,0.403097604642181,
-1.49064765758984));
#58442=CARTESIAN_POINT('Ctrl Pts',(-10.3756936987968,0.808074795294769,
-1.22308501321018));
#58443=CARTESIAN_POINT('Ctrl Pts',(-10.3491791563911,1.21305198594738,-0.955522368830519));
#58444=CARTESIAN_POINT('Ctrl Pts',(-10.3226646139855,1.47193290723213,-0.466831484106978));
#58445=CARTESIAN_POINT('Ctrl Pts',(-10.2961500715798,1.46580323169478,0.0185124359065781));
#58446=CARTESIAN_POINT('Ctrl Pts',(-10.2696355291741,1.45967355615742,0.503856355920134));
#58447=CARTESIAN_POINT('Ctrl Pts',(-10.2431209867684,1.18853328379795,0.985853311223747));
#58448=CARTESIAN_POINT('Ctrl Pts',(-10.2166064443627,0.776927950739231,
1.24310288540015));
#58449=CARTESIAN_POINT('Ctrl Pts',(-10.190091901957,0.365322617680536,1.50035245957654));
#58450=CARTESIAN_POINT('Ctrl Pts',(-10.1635773595513,-0.186747776077338,
1.53285465262578));
#58451=CARTESIAN_POINT('Ctrl Pts',(-10.1370628171456,-0.625695290352148,
1.3256799115779));
#58452=CARTESIAN_POINT('Ctrl Pts',(-10.11054827474,-1.06464280462698,1.11850517053001));
#58453=CARTESIAN_POINT('Ctrl Pts',(-10.0840337323343,-1.39046743941869,
0.671653495384919));
#58454=CARTESIAN_POINT('Ctrl Pts',(-10.0575191899286,-1.4535049509429,0.190381674313756));
#58455=CARTESIAN_POINT('Ctrl Pts',(-10.0540644752333,-1.46171842919503,
0.127674318960563));
#58456=CARTESIAN_POINT('Ctrl Pts',(-10.0506097605381,-1.46547062024338,
0.0643826193112584));
#58457=CARTESIAN_POINT('Ctrl Pts',(-10.0471550458429,-1.46496448118167,
0.00103054806325355));
#58458=CARTESIAN_POINT('Origin',(-17.3,0.,0.));
#58459=CARTESIAN_POINT('',(-9.47584495415713,-1.46157717162269,0.000851046066846911));
#58460=CARTESIAN_POINT('',(-9.54715504584286,-1.46135409027402,0.000652074851629444));
#58461=CARTESIAN_POINT('',(-17.3,-1.4635,-1.79227059055215E-16));
#58462=CARTESIAN_POINT('Ctrl Pts',(-9.47584495415713,-1.46157717162269,
0.000851046066846911));
#58463=CARTESIAN_POINT('Ctrl Pts',(-9.48609809757008,-1.46257459730285,
0.18998561356786));
#58464=CARTESIAN_POINT('Ctrl Pts',(-9.49635124098303,-1.42852426825454,
0.378774872364767));
#58465=CARTESIAN_POINT('Ctrl Pts',(-9.50660438439598,-1.35776614138582,
0.552623708977331));
#58466=CARTESIAN_POINT('Ctrl Pts',(-9.53311892680166,-1.17478622197511,
1.00219533446756));
#58467=CARTESIAN_POINT('Ctrl Pts',(-9.55963346920735,-0.74632832319233,
1.3518550920021));
#58468=CARTESIAN_POINT('Ctrl Pts',(-9.58614801161304,-0.26920023845603,
1.4409903157318));
#58469=CARTESIAN_POINT('Ctrl Pts',(-9.61266255401872,0.207927846280298,
1.5301255394615));
#58470=CARTESIAN_POINT('Ctrl Pts',(-9.63917709642441,0.733726116970183,
1.35873622938633));
#58471=CARTESIAN_POINT('Ctrl Pts',(-9.6656916388301,1.06667446689659,1.00554832807205));
#58472=CARTESIAN_POINT('Ctrl Pts',(-9.69220618123579,1.39962281682299,0.652360426757773));
#58473=CARTESIAN_POINT('Ctrl Pts',(-9.71872072364148,1.53972124598593,0.117373934204458));
#58474=CARTESIAN_POINT('Ctrl Pts',(-9.74523526604717,1.42261696083608,-0.353670526279942));
#58475=CARTESIAN_POINT('Ctrl Pts',(-9.77174980845285,1.30551267568624,-0.824714986764287));
#58476=CARTESIAN_POINT('Ctrl Pts',(-9.79826435085853,0.931205676223611,
-1.23181741517969));
#58477=CARTESIAN_POINT('Ctrl Pts',(-9.82477889326421,0.471630089079157,
-1.38797943698485));
#58478=CARTESIAN_POINT('Ctrl Pts',(-9.8512934356699,0.0120545019346503,
-1.54414145879004));
#58479=CARTESIAN_POINT('Ctrl Pts',(-9.87780797807559,-0.532789672891738,
-1.44936307398492));
#58480=CARTESIAN_POINT('Ctrl Pts',(-9.90432252048128,-0.912633785646623,
-1.14717977305823));
#58481=CARTESIAN_POINT('Ctrl Pts',(-9.92816333170656,-1.25417435039281,
-0.875468690038308));
#58482=CARTESIAN_POINT('Ctrl Pts',(-9.95200414293184,-1.46231428139932,
-0.436073141303719));
#58483=CARTESIAN_POINT('Ctrl Pts',(-9.97584495415713,-1.46531245936081,
0.000844241415329933));
#58484=CARTESIAN_POINT('Ctrl Pts',(-10.0471550458429,-1.46496448118167,
0.00103054806325355));
#58485=CARTESIAN_POINT('Ctrl Pts',(-10.0240952181324,-1.46158606050438,
-0.421837322933612));
#58486=CARTESIAN_POINT('Ctrl Pts',(-10.001035390422,-1.26848154526367,-0.847394996587496));
#58487=CARTESIAN_POINT('Ctrl Pts',(-9.97797556271152,-0.946009075420625,
-1.11981634813565));
#58488=CARTESIAN_POINT('Ctrl Pts',(-9.95146102030583,-0.575225300117436,
-1.4330505825166));
#58489=CARTESIAN_POINT('Ctrl Pts',(-9.92494647790015,-0.0334073612543562,
-1.54382708428126));
#58490=CARTESIAN_POINT('Ctrl Pts',(-9.89843193549447,0.430566162234381,
-1.40126179005523));
#58491=CARTESIAN_POINT('Ctrl Pts',(-9.87191739308878,0.894539685723119,
-1.25869649582921));
#58492=CARTESIAN_POINT('Ctrl Pts',(-9.84540285068308,1.28066879383748,-0.862789405612513));
#58493=CARTESIAN_POINT('Ctrl Pts',(-9.8188883082774,1.41158899415352,-0.395396428808714));
#58494=CARTESIAN_POINT('Ctrl Pts',(-9.79237376587171,1.54250919446956,0.071996547995058));
#58495=CARTESIAN_POINT('Ctrl Pts',(-9.76585922346603,1.41822048698725,0.610875411385968));
#58496=CARTESIAN_POINT('Ctrl Pts',(-9.73934468106035,1.09581362983228,0.973711616960512));
#58497=CARTESIAN_POINT('Ctrl Pts',(-9.71283013865466,0.773406772677265,
1.3365478225351));
#58498=CARTESIAN_POINT('Ctrl Pts',(-9.68631559624897,0.252881765849561,
1.52334137029334));
#58499=CARTESIAN_POINT('Ctrl Pts',(-9.65980105384328,-0.226663504244833,
1.44829053721051));
#58500=CARTESIAN_POINT('Ctrl Pts',(-9.63328651143759,-0.706208774339227,
1.37323970412768));
#58501=CARTESIAN_POINT('Ctrl Pts',(-9.60677196903191,-1.14477430770028,
1.03634449020378));
#58502=CARTESIAN_POINT('Ctrl Pts',(-9.58025742662622,-1.34090947140602,
0.592354297548066));
#58503=CARTESIAN_POINT('Ctrl Pts',(-9.56922329969844,-1.42253186029052,
0.407586102589327));
#58504=CARTESIAN_POINT('Ctrl Pts',(-9.55818917277065,-1.46216919655488,
0.204270774596894));
#58505=CARTESIAN_POINT('Ctrl Pts',(-9.54715504584286,-1.46135409027402,
0.000652074851629444));
#58506=CARTESIAN_POINT('Origin',(-17.3,0.,0.));
#58507=CARTESIAN_POINT('',(-8.97584495415714,-1.46219403757879,-0.00116636394747058));
#58508=CARTESIAN_POINT('',(-9.04715504584287,-1.46256895709697,-0.00127018677453484));
#58509=CARTESIAN_POINT('',(-17.3,-1.4635,-1.79227059055215E-16));
#58510=CARTESIAN_POINT('Ctrl Pts',(-8.97584495415714,-1.46219403757879,
-0.00116636394747058));
#58511=CARTESIAN_POINT('Ctrl Pts',(-8.99367750980264,-1.45975220887188,
0.327433385342918));
#58512=CARTESIAN_POINT('Ctrl Pts',(-9.01151006544813,-1.35024939521357,
0.657507843102589));
#58513=CARTESIAN_POINT('Ctrl Pts',(-9.02934262109362,-1.14694921270435,
0.912923524669222));
#58514=CARTESIAN_POINT('Ctrl Pts',(-9.05585716349931,-0.844669975931715,
1.29269129630033));
#58515=CARTESIAN_POINT('Ctrl Pts',(-9.082371705905,-0.335027507307018,1.50740662235469));
#58516=CARTESIAN_POINT('Ctrl Pts',(-9.10888624831068,0.147879090393584,
1.45844219393227));
#58517=CARTESIAN_POINT('Ctrl Pts',(-9.13540079071637,0.63078568809416,1.40947776550986));
#58518=CARTESIAN_POINT('Ctrl Pts',(-9.16191533312205,1.08695641487064,1.09683358261071));
#58519=CARTESIAN_POINT('Ctrl Pts',(-9.18842987552774,1.30685387063295,0.664119582025169));
#58520=CARTESIAN_POINT('Ctrl Pts',(-9.21494441793343,1.52675132639526,0.231405581439627));
#58521=CARTESIAN_POINT('Ctrl Pts',(-9.24145896033911,1.51037551114339,-0.321378236832304));
#58522=CARTESIAN_POINT('Ctrl Pts',(-9.26797350274479,1.26524848964568,-0.740316228288248));
#58523=CARTESIAN_POINT('Ctrl Pts',(-9.29448804515048,1.02012146814797,-1.15925421974419));
#58524=CARTESIAN_POINT('Ctrl Pts',(-9.32100258755617,0.546243240404423,
-1.44434638438415));
#58525=CARTESIAN_POINT('Ctrl Pts',(-9.34751712996185,0.0612849676102023,
-1.46463852576758));
#58526=CARTESIAN_POINT('Ctrl Pts',(-9.37403167236754,-0.423673305184046,
-1.48493066715101));
#58527=CARTESIAN_POINT('Ctrl Pts',(-9.40054621477323,-0.919711623028967,
-1.24042278527788));
#58528=CARTESIAN_POINT('Ctrl Pts',(-9.42706075717892,-1.19897981193209,
-0.843427097618339));
#58529=CARTESIAN_POINT('Ctrl Pts',(-9.44332215617166,-1.37025530959104,
-0.599949191167883));
#58530=CARTESIAN_POINT('Ctrl Pts',(-9.45958355516439,-1.4599952629048,-0.299114783102133));
#58531=CARTESIAN_POINT('Ctrl Pts',(-9.47584495415713,-1.46157717162269,
0.000851046066846911));
#58532=CARTESIAN_POINT('Ctrl Pts',(-9.54715504584286,-1.46135409027402,
0.000652074851629444));
#58533=CARTESIAN_POINT('Ctrl Pts',(-9.53167463036496,-1.46021053048274,
-0.285016387343409));
#58534=CARTESIAN_POINT('Ctrl Pts',(-9.51619421488706,-1.37944479806305,
-0.571281973384492));
#58535=CARTESIAN_POINT('Ctrl Pts',(-9.50071379940916,-1.22328908721203,
-0.807765828342601));
#58536=CARTESIAN_POINT('Ctrl Pts',(-9.47419925700348,-0.955828745261837,
-1.21281059019021));
#58537=CARTESIAN_POINT('Ctrl Pts',(-9.44768471459779,-0.467203267310972,
-1.47181494249797));
#58538=CARTESIAN_POINT('Ctrl Pts',(-9.42117017219211,0.0181421855248795,
-1.46580786102218));
#58539=CARTESIAN_POINT('Ctrl Pts',(-9.39465562978642,0.503487638360758,
-1.4598007795464));
#58540=CARTESIAN_POINT('Ctrl Pts',(-9.36814108738073,0.985553066081652,
-1.18878226428704));
#58541=CARTESIAN_POINT('Ctrl Pts',(-9.34162654497504,1.24290660015939,-0.777241923477027));
#58542=CARTESIAN_POINT('Ctrl Pts',(-9.31511200256935,1.50026013423713,-0.365701582667018));
#58543=CARTESIAN_POINT('Ctrl Pts',(-9.28859746016367,1.53290177467173,0.186360583693584));
#58544=CARTESIAN_POINT('Ctrl Pts',(-9.26208291775799,1.32583791475006,0.625360414594071));
#58545=CARTESIAN_POINT('Ctrl Pts',(-9.2355683753523,1.11877405482839,1.06436024549453));
#58546=CARTESIAN_POINT('Ctrl Pts',(-9.20905383294662,0.672004694550432,
1.39029774093484));
#58547=CARTESIAN_POINT('Ctrl Pts',(-9.18253929054093,0.190748811587309,
1.45345681573553));
#58548=CARTESIAN_POINT('Ctrl Pts',(-9.15602474813524,-0.290507071375815,
1.51661589053622));
#58549=CARTESIAN_POINT('Ctrl Pts',(-9.12951020572955,-0.806249477024134,
1.31699654469731));
#58550=CARTESIAN_POINT('Ctrl Pts',(-9.10299566332387,-1.11957735833208,
0.946291901603416));
#58551=CARTESIAN_POINT('Ctrl Pts',(-9.08438212416354,-1.33953743531608,
0.686052622887204));
#58552=CARTESIAN_POINT('Ctrl Pts',(-9.0657685850032,-1.45974328379025,0.341498832192847));
#58553=CARTESIAN_POINT('Ctrl Pts',(-9.04715504584287,-1.46256895709697,
-0.00127018677453484));
#58554=CARTESIAN_POINT('Origin',(-17.3,0.,0.));
#58555=CARTESIAN_POINT('',(-8.47584495415715,-1.46580452990507,-0.000374448332874922));
#58556=CARTESIAN_POINT('',(-8.54715504584287,-1.46590976831451,-0.000110809370955516));
#58557=CARTESIAN_POINT('',(-17.3,-1.4635,-1.79227059055215E-16));
#58558=CARTESIAN_POINT('Ctrl Pts',(-8.47584495415715,-1.46580452990507,
-0.000374448332874922));
#58559=CARTESIAN_POINT('Ctrl Pts',(-8.50125692203519,-1.46421447777039,
0.464922610210453));
#58560=CARTESIAN_POINT('Ctrl Pts',(-8.52666888991322,-1.22367892553067,
0.931633766965713));
#58561=CARTESIAN_POINT('Ctrl Pts',(-8.55208085779126,-0.843124218313088,
1.19919281640258));
#58562=CARTESIAN_POINT('Ctrl Pts',(-8.57859540019694,-0.446058002480036,
1.47836071856452));
#58563=CARTESIAN_POINT('Ctrl Pts',(-8.60510994260263,0.103441259930457,
1.5407199815395));
#58564=CARTESIAN_POINT('Ctrl Pts',(-8.63162448500832,0.552966651862248,
1.35762650988623));
#58565=CARTESIAN_POINT('Ctrl Pts',(-8.65813902741401,1.00249204379404,1.17453303823295));
#58566=CARTESIAN_POINT('Ctrl Pts',(-8.68465356981969,1.35204356524713,0.745986831951424));
#58567=CARTESIAN_POINT('Ctrl Pts',(-8.71116811222538,1.44105826751941,0.268836247614723));
#58568=CARTESIAN_POINT('Ctrl Pts',(-8.73768265463107,1.5300729697917,-0.208314336722033));
#58569=CARTESIAN_POINT('Ctrl Pts',(-8.76419719703676,1.35855085288313,-0.73406929911397));
#58570=CARTESIAN_POINT('Ctrl Pts',(-8.79071173944245,1.00527886283239,-1.06692842607179));
#58571=CARTESIAN_POINT('Ctrl Pts',(-8.81722628184813,0.65200687278171,-1.39978755302956));
#58572=CARTESIAN_POINT('Ctrl Pts',(-8.84374082425381,0.116985009588939,
-1.53975084455328));
#58573=CARTESIAN_POINT('Ctrl Pts',(-8.8702553666595,-0.354029856293153,
-1.42252758119857));
#58574=CARTESIAN_POINT('Ctrl Pts',(-8.89676990906518,-0.825044722175272,
-1.30530431784386));
#58575=CARTESIAN_POINT('Ctrl Pts',(-8.92328445147087,-1.2320525907467,-0.930894499610681));
#58576=CARTESIAN_POINT('Ctrl Pts',(-8.94979899387656,-1.38809852257213,
-0.471279481890183));
#58577=CARTESIAN_POINT('Ctrl Pts',(-8.95848098063676,-1.43919458500314,
-0.320782013837325));
#58578=CARTESIAN_POINT('Ctrl Pts',(-8.96716296739695,-1.46338287023551,
-0.161148967083977));
#58579=CARTESIAN_POINT('Ctrl Pts',(-8.97584495415714,-1.46219403757879,
-0.00116636394747058));
#58580=CARTESIAN_POINT('Ctrl Pts',(-9.04715504584287,-1.46256895709697,
-0.00127018677453484));
#58581=CARTESIAN_POINT('Ctrl Pts',(-9.03925404259752,-1.46376838799371,
-0.146767456688621));
#58582=CARTESIAN_POINT('Ctrl Pts',(-9.03135303935216,-1.44381825974912,
-0.291943146445416));
#58583=CARTESIAN_POINT('Ctrl Pts',(-9.02345203610681,-1.40137050280996,
-0.430212201342784));
#58584=CARTESIAN_POINT('Ctrl Pts',(-8.99693749370113,-1.25892240901231,
-0.894221720846118));
#58585=CARTESIAN_POINT('Ctrl Pts',(-8.97042295129543,-0.863112864449447,
-1.2804508195039));
#58586=CARTESIAN_POINT('Ctrl Pts',(-8.94390840888975,-0.395752971917505,
-1.41148907524943));
#58587=CARTESIAN_POINT('Ctrl Pts',(-8.91739386648406,0.0716069206144383,
-1.54252733099497));
#58588=CARTESIAN_POINT('Ctrl Pts',(-8.89087932407838,0.610517161115462,
-1.41837474382825));
#58589=CARTESIAN_POINT('Ctrl Pts',(-8.86436478167269,0.973434792424628,
-1.09605954638754));
#58590=CARTESIAN_POINT('Ctrl Pts',(-8.837850239267,1.33635242373379,-0.773744348946829));
#58591=CARTESIAN_POINT('Ctrl Pts',(-8.81133569686132,1.5232774458511,-0.253266541232123));
#58592=CARTESIAN_POINT('Ctrl Pts',(-8.78482115445563,1.44834774433747,0.226297670784763));
#58593=CARTESIAN_POINT('Ctrl Pts',(-8.75830661204994,1.37341804282383,0.705861882801677));
#58594=CARTESIAN_POINT('Ctrl Pts',(-8.73179206964426,1.03663361767922,1.14451249912077));
#58595=CARTESIAN_POINT('Ctrl Pts',(-8.70527752723857,0.592692981309976,
1.34075980482558));
#58596=CARTESIAN_POINT('Ctrl Pts',(-8.67876298483288,0.148752344940759,
1.53700711053039));
#58597=CARTESIAN_POINT('Ctrl Pts',(-8.6522484424272,-0.402344502653075,
1.49085110562094));
#58598=CARTESIAN_POINT('Ctrl Pts',(-8.62573390002151,-0.807456809852813,
1.2234930831649));
#58599=CARTESIAN_POINT('Ctrl Pts',(-8.59954094862863,-1.20765556903883,
0.95937780711978));
#58600=CARTESIAN_POINT('Ctrl Pts',(-8.57334799723575,-1.46538956251999,
0.479393826634133));
#58601=CARTESIAN_POINT('Ctrl Pts',(-8.54715504584287,-1.46590976831451,
-0.000110809370955516));
#58602=CARTESIAN_POINT('Origin',(-17.3,0.,0.));
#58603=CARTESIAN_POINT('',(-7.97584495415714,-1.46332934625901,0.0013523262496782));
#58604=CARTESIAN_POINT('',(-8.04715504584285,-1.46290284295625,0.00132519226194577));
#58605=CARTESIAN_POINT('',(-17.3,-1.4635,-1.79227059055215E-16));
#58606=CARTESIAN_POINT('Ctrl Pts',(-7.97584495415714,-1.46332934625901,
0.0013523262496782));
#58607=CARTESIAN_POINT('Ctrl Pts',(-7.98232179186204,-1.4644202230544,0.120466211293856));
#58608=CARTESIAN_POINT('Ctrl Pts',(-7.98879862956694,-1.45110187555386,
0.239339281952935));
#58609=CARTESIAN_POINT('Ctrl Pts',(-7.99527546727184,-1.42243811080014,
0.354389163718262));
#58610=CARTESIAN_POINT('Ctrl Pts',(-8.02179000967753,-1.30509587671973,
0.825374404946185));
#58611=CARTESIAN_POINT('Ctrl Pts',(-8.04830455208321,-0.930583263604335,
1.23228768770552));
#58612=CARTESIAN_POINT('Ctrl Pts',(-8.0748190944889,-0.470928844632437,
1.3882175195951));
#58613=CARTESIAN_POINT('Ctrl Pts',(-8.10133363689458,-0.0112744256605388,
1.54414735148468));
#58614=CARTESIAN_POINT('Ctrl Pts',(-8.12784817930028,0.533521799167859,
1.44909373250449));
#58615=CARTESIAN_POINT('Ctrl Pts',(-8.15436272170597,0.913213205445003,
1.1467185791721));
#58616=CARTESIAN_POINT('Ctrl Pts',(-8.18087726411166,1.29290461172213,0.844343425839718));
#58617=CARTESIAN_POINT('Ctrl Pts',(-8.20739180651734,1.50749119944801,0.334646738155148));
#58618=CARTESIAN_POINT('Ctrl Pts',(-8.23390634892302,1.45840479436909,-0.148247476129831));
#58619=CARTESIAN_POINT('Ctrl Pts',(-8.26042089132871,1.40931838929016,-0.63114169041481));
#58620=CARTESIAN_POINT('Ctrl Pts',(-8.2869354337344,1.09655899140643,-1.0872334313002));
#58621=CARTESIAN_POINT('Ctrl Pts',(-8.31344997614009,0.663789460343703,
-1.30702158006447));
#58622=CARTESIAN_POINT('Ctrl Pts',(-8.33996451854577,0.231019929280951,
-1.52680972882876));
#58623=CARTESIAN_POINT('Ctrl Pts',(-8.36647906095145,-0.321759734960807,
-1.5102942854719));
#58624=CARTESIAN_POINT('Ctrl Pts',(-8.39299360335714,-0.740635795990823,
-1.26506145151714));
#58625=CARTESIAN_POINT('Ctrl Pts',(-8.41950814576283,-1.15951185702082,
-1.01982861756239));
#58626=CARTESIAN_POINT('Ctrl Pts',(-8.44602268816852,-1.44448431483909,
-0.545878393009778));
#58627=CARTESIAN_POINT('Ctrl Pts',(-8.47253723057421,-1.46465395912042,
-0.0609150100590203));
#58628=CARTESIAN_POINT('Ctrl Pts',(-8.47363980510186,-1.46549268888901,
-0.0407484062119078));
#58629=CARTESIAN_POINT('Ctrl Pts',(-8.4747423796295,-1.46587351909118,-0.0205627583056027));
#58630=CARTESIAN_POINT('Ctrl Pts',(-8.47584495415715,-1.46580452990507,
-0.000374448332874922));
#58631=CARTESIAN_POINT('Ctrl Pts',(-8.54715504584287,-1.46590976831451,
-0.000110809370955516));
#58632=CARTESIAN_POINT('Ctrl Pts',(-8.54683345483006,-1.46591615528121,
-0.00599805663929943));
#58633=CARTESIAN_POINT('Ctrl Pts',(-8.54651186381725,-1.46588376891111,
-0.0118852316495221));
#58634=CARTESIAN_POINT('Ctrl Pts',(-8.54619027280445,-1.46581239682725,
-0.0177719339856615));
#58635=CARTESIAN_POINT('Ctrl Pts',(-8.51967573039876,-1.45992790979631,
-0.503118888677552));
#58636=CARTESIAN_POINT('Ctrl Pts',(-8.49316118799308,-1.18903116892879,
-0.98525275805866));
#58637=CARTESIAN_POINT('Ctrl Pts',(-8.46664664558739,-0.777555846624848,
-1.24271023561792));
#58638=CARTESIAN_POINT('Ctrl Pts',(-8.44013210318171,-0.366080524320909,
-1.50016771317719));
#58639=CARTESIAN_POINT('Ctrl Pts',(-8.41361756077602,0.185973379419495,
-1.53294879891458));
#58640=CARTESIAN_POINT('Ctrl Pts',(-8.38710301837033,0.625025498936305,
-1.32599583333036));
#58641=CARTESIAN_POINT('Ctrl Pts',(-8.36058847596464,1.06407761845314,-1.11904286774613));
#58642=CARTESIAN_POINT('Ctrl Pts',(-8.33407393355895,1.39012795374642,-0.672355850840293));
#58643=CARTESIAN_POINT('Ctrl Pts',(-8.30755939115327,1.45340858779386,-0.191115936690511));
#58644=CARTESIAN_POINT('Ctrl Pts',(-8.28104484874758,1.5166892218413,0.290123977459216));
#58645=CARTESIAN_POINT('Ctrl Pts',(-8.2545303063419,1.31720015464296,0.805916788852843));
#58646=CARTESIAN_POINT('Ctrl Pts',(-8.22801576393622,0.946574667410269,
1.11933829709663));
#58647=CARTESIAN_POINT('Ctrl Pts',(-8.20150122153053,0.575949180177555,
1.43275980534043));
#58648=CARTESIAN_POINT('Ctrl Pts',(-8.17498667912484,0.034187272910406,
1.54381001043435));
#58649=CARTESIAN_POINT('Ctrl Pts',(-8.14847213671915,-0.429858213002534,
1.40147912615362));
#58650=CARTESIAN_POINT('Ctrl Pts',(-8.12195759431346,-0.893903698915473,
1.25914824187289));
#58651=CARTESIAN_POINT('Ctrl Pts',(-8.09544305190777,-1.28023276347424,
0.863436268217562));
#58652=CARTESIAN_POINT('Ctrl Pts',(-8.06892850950209,-1.41138906628869,
0.396109489776231));
#58653=CARTESIAN_POINT('Ctrl Pts',(-8.06167068828234,-1.44729045893222,
0.2681882095508));
#58654=CARTESIAN_POINT('Ctrl Pts',(-8.0544128670626,-1.46407226164141,0.134900973761092));
#58655=CARTESIAN_POINT('Ctrl Pts',(-8.04715504584285,-1.46290284295625,
0.00132519226194577));
#58656=CARTESIAN_POINT('Origin',(-17.3,0.,0.));
#58657=CARTESIAN_POINT('',(-7.47584495415714,-1.46111246214465,-0.000242921189035072));
#58658=CARTESIAN_POINT('',(-7.54715504584287,-1.46121757502423,-0.000473021952020669));
#58659=CARTESIAN_POINT('',(-17.3,-1.4635,-1.79227059055215E-16));
#58660=CARTESIAN_POINT('Ctrl Pts',(-7.47584495415714,-1.46111246214465,
-0.000242921189035072));
#58661=CARTESIAN_POINT('Ctrl Pts',(-7.48990120409459,-1.46072923544993,
0.259251732184533));
#58662=CARTESIAN_POINT('Ctrl Pts',(-7.50395745403204,-1.39493658532748,
0.518927885930192));
#58663=CARTESIAN_POINT('Ctrl Pts',(-7.51801370396949,-1.26487433267444,
0.740955316438846));
#58664=CARTESIAN_POINT('Ctrl Pts',(-7.54452824637518,-1.01953570190919,
1.1597694203175));
#58665=CARTESIAN_POINT('Ctrl Pts',(-7.57104278878086,-0.545513510786813,
1.44462215313213));
#58666=CARTESIAN_POINT('Ctrl Pts',(-7.59755733118654,-0.0605450486214669,
1.46466929902454));
#58667=CARTESIAN_POINT('Ctrl Pts',(-7.62407187359223,0.424423413543935,
1.48471644491695));
#58668=CARTESIAN_POINT('Ctrl Pts',(-7.65058641599792,0.920338146752306,
1.23995800388708));
#58669=CARTESIAN_POINT('Ctrl Pts',(-7.67710095840361,1.19940574436146,0.842821285214332));
#58670=CARTESIAN_POINT('Ctrl Pts',(-7.70361550080929,1.4784733419706,0.445684566541602));
#58671=CARTESIAN_POINT('Ctrl Pts',(-7.73013004321498,1.54069380398054,-0.103830429773995));
#58672=CARTESIAN_POINT('Ctrl Pts',(-7.75664458562067,1.35748679176655,-0.553309559466464));
#58673=CARTESIAN_POINT('Ctrl Pts',(-7.78315912802635,1.17427977955254,-1.00278868915896));
#58674=CARTESIAN_POINT('Ctrl Pts',(-7.80967367043204,0.745645293114572,
-1.35223195222832));
#58675=CARTESIAN_POINT('Ctrl Pts',(-7.83618821283773,0.268472239620885,
-1.44112612736379));
#58676=CARTESIAN_POINT('Ctrl Pts',(-7.86270275524341,-0.208700813872774,
-1.53002030249926));
#58677=CARTESIAN_POINT('Ctrl Pts',(-7.8892172976491,-0.734412434422143,
-1.35836538970088));
#58678=CARTESIAN_POINT('Ctrl Pts',(-7.91573184005478,-1.06718231717409,
-1.00500933345345));
#58679=CARTESIAN_POINT('Ctrl Pts',(-7.93576954475557,-1.31866486369047,
-0.737969299309713));
#58680=CARTESIAN_POINT('Ctrl Pts',(-7.95580724945636,-1.45995444818576,
-0.367156035859364));
#58681=CARTESIAN_POINT('Ctrl Pts',(-7.97584495415714,-1.46332934625901,
0.0013523262496782));
#58682=CARTESIAN_POINT('Ctrl Pts',(-8.04715504584285,-1.46290284295625,
0.00132519226194577));
#58683=CARTESIAN_POINT('Ctrl Pts',(-8.02789832465691,-1.45980009780892,
-0.353083039030015));
#58684=CARTESIAN_POINT('Ctrl Pts',(-8.00864160347097,-1.33032672117917,
-0.709522536201345));
#58685=CARTESIAN_POINT('Ctrl Pts',(-7.98938488228503,-1.09630539301137,
-0.973157905781084));
#58686=CARTESIAN_POINT('Ctrl Pts',(-7.96287033987935,-0.774081875849499,
-1.33615693966975));
#58687=CARTESIAN_POINT('Ctrl Pts',(-7.93635579747366,-0.253651300455625,
-1.52321342421982));
#58688=CARTESIAN_POINT('Ctrl Pts',(-7.90984125506798,0.225931822886316,
-1.4484048590561));
#58689=CARTESIAN_POINT('Ctrl Pts',(-7.88332671266229,0.705514946228339,
-1.37359629389236));
#58690=CARTESIAN_POINT('Ctrl Pts',(-7.8568121702566,1.14425061751844,-1.03692267901471));
#58691=CARTESIAN_POINT('Ctrl Pts',(-7.83029762785091,1.34061005270123,-0.593031627256463));
#58692=CARTESIAN_POINT('Ctrl Pts',(-7.80378308544522,1.53696948788399,-0.149140575498266));
#58693=CARTESIAN_POINT('Ctrl Pts',(-7.77726854303954,1.49095268695951,0.401967913140544));
#58694=CARTESIAN_POINT('Ctrl Pts',(-7.75075400063385,1.22369700105575,0.80714773984519));
#58695=CARTESIAN_POINT('Ctrl Pts',(-7.72423945822817,0.956441315151998,
1.21232756654984));
#58696=CARTESIAN_POINT('Ctrl Pts',(-7.69772491582249,0.467946744269036,
1.47157873132032));
#58697=CARTESIAN_POINT('Ctrl Pts',(-7.6712103734168,-0.0174016813124656,
1.4658168391097));
#58698=CARTESIAN_POINT('Ctrl Pts',(-7.64469583101111,-0.502750106893995,
1.46005494689907));
#58699=CARTESIAN_POINT('Ctrl Pts',(-7.61818128860542,-0.984952387174048,
1.18927999770723));
#58700=CARTESIAN_POINT('Ctrl Pts',(-7.59166674619973,-1.24251379178837,
0.777869720162521));
#58701=CARTESIAN_POINT('Ctrl Pts',(-7.57682951274744,-1.38664219612179,
0.547649253250261));
#58702=CARTESIAN_POINT('Ctrl Pts',(-7.56199227929516,-1.46042671212876,
0.273390336954752));
#58703=CARTESIAN_POINT('Ctrl Pts',(-7.54715504584287,-1.46121757502423,
-0.000473021952020669));
#58704=CARTESIAN_POINT('Origin',(-17.3,0.,0.));
#58705=CARTESIAN_POINT('',(-6.97584495415715,-1.46422371240563,-0.00126593926974311));
#58706=CARTESIAN_POINT('',(-7.04715504584287,-1.46464284830267,-0.00115453508994419));
#58707=CARTESIAN_POINT('',(-17.3,-1.4635,-1.79227059055215E-16));
#58708=CARTESIAN_POINT('Ctrl Pts',(-6.97584495415715,-1.46422371240563,
-0.00126593926974311));
#58709=CARTESIAN_POINT('Ctrl Pts',(-6.99748061632714,-1.4605964766255,0.396006961252073));
#58710=CARTESIAN_POINT('Ctrl Pts',(-7.01911627849713,-1.29314413636782,
0.795971321500709));
#58711=CARTESIAN_POINT('Ctrl Pts',(-7.04075194066713,-1.00473973995226,
1.06743614018744));
#58712=CARTESIAN_POINT('Ctrl Pts',(-7.06726648307281,-0.651299640053113,
1.40011675750195));
#58713=CARTESIAN_POINT('Ctrl Pts',(-7.0937810254785,-0.116207137990993,
1.53980974696585));
#58714=CARTESIAN_POINT('Ctrl Pts',(-7.12029556788419,0.354748448532587,
1.42234854964644));
#58715=CARTESIAN_POINT('Ctrl Pts',(-7.14681011028988,0.825704035056194,
1.30488735232702));
#58716=CARTESIAN_POINT('Ctrl Pts',(-7.17332465269557,1.23252270604125,0.930271968224272));
#58717=CARTESIAN_POINT('Ctrl Pts',(-7.19983919510125,1.38833642804622,0.470578177328132));
#58718=CARTESIAN_POINT('Ctrl Pts',(-7.22635373750694,1.54415015005118,0.0108843864320189));
#58719=CARTESIAN_POINT('Ctrl Pts',(-7.25286827991262,1.44895892307608,-0.533887811257471));
#58720=CARTESIAN_POINT('Ctrl Pts',(-7.2793828223183,1.14648787247628,-0.913502827955351));
#58721=CARTESIAN_POINT('Ctrl Pts',(-7.30589736472399,0.844016821876477,
-1.29311784465323));
#58722=CARTESIAN_POINT('Ctrl Pts',(-7.33241190712968,0.334265947651977,
-1.5075756803595));
#58723=CARTESIAN_POINT('Ctrl Pts',(-7.35892644953537,-0.148615852407503,
-1.45836730175591));
#58724=CARTESIAN_POINT('Ctrl Pts',(-7.38544099194106,-0.631497652466983,
-1.40915892315231));
#58725=CARTESIAN_POINT('Ctrl Pts',(-7.41195553434673,-1.08751037836144,
-1.09628433023885));
#58726=CARTESIAN_POINT('Ctrl Pts',(-7.43847007675242,-1.30718920610463,
-0.66345929631075));
#58727=CARTESIAN_POINT('Ctrl Pts',(-7.45092836922066,-1.41040890506189,
-0.460089357740911));
#58728=CARTESIAN_POINT('Ctrl Pts',(-7.4633866616889,-1.46145212245702,-0.230237428974453));
#58729=CARTESIAN_POINT('Ctrl Pts',(-7.47584495415714,-1.46111246214465,
-0.000242921189035072));
#58730=CARTESIAN_POINT('Ctrl Pts',(-7.54715504584287,-1.46121757502423,
-0.000473021952020669));
#58731=CARTESIAN_POINT('Ctrl Pts',(-7.53547773688947,-1.46184000577589,
-0.216010983476512));
#58732=CARTESIAN_POINT('Ctrl Pts',(-7.52380042793608,-1.41724928492728,
-0.431303931970136));
#58733=CARTESIAN_POINT('Ctrl Pts',(-7.51212311898268,-1.32615366730869,
-0.624690543400295));
#58734=CARTESIAN_POINT('Ctrl Pts',(-7.48560857657699,-1.11931160926606,
-1.06379492352077));
#58735=CARTESIAN_POINT('Ctrl Pts',(-7.4590940341713,-0.672706964232189,
-1.38995807786417));
#58736=CARTESIAN_POINT('Ctrl Pts',(-7.43257949176561,-0.191483049600187,
-1.45336026712094));
#58737=CARTESIAN_POINT('Ctrl Pts',(-7.40606494935992,0.289740865031816,
-1.51676245637771));
#58738=CARTESIAN_POINT('Ctrl Pts',(-7.37955040695424,0.80558404926195,-1.31740368054786));
#58739=CARTESIAN_POINT('Ctrl Pts',(-7.35303586454856,1.1190991644445,-0.946857372823209));
#58740=CARTESIAN_POINT('Ctrl Pts',(-7.32652132214287,1.43261427962704,-0.576311065098553));
#58741=CARTESIAN_POINT('Ctrl Pts',(-7.30000677973718,1.543801325762,-0.0345772254790913));
#58742=CARTESIAN_POINT('Ctrl Pts',(-7.27349223733149,1.40158766007931,0.429504197236137));
#58743=CARTESIAN_POINT('Ctrl Pts',(-7.24697769492581,1.2593739943966,0.893585619951392));
#58744=CARTESIAN_POINT('Ctrl Pts',(-7.22046315252012,0.863759616896217,
1.2800146257624));
#58745=CARTESIAN_POINT('Ctrl Pts',(-7.19394861011444,0.396465982362147,
1.41128896727767));
#58746=CARTESIAN_POINT('Ctrl Pts',(-7.16743406770875,-0.0708276521718959,
1.54256330879292));
#58747=CARTESIAN_POINT('Ctrl Pts',(-7.14091952530306,-0.609800543739616,
1.41868298601245));
#58748=CARTESIAN_POINT('Ctrl Pts',(-7.11440498289737,-0.972880957047548,
1.09655116968807));
#58749=CARTESIAN_POINT('Ctrl Pts',(-7.09198833721254,-1.27984627652,0.824205726954458));
#58750=CARTESIAN_POINT('Ctrl Pts',(-7.0695716915277,-1.46108699957425,0.410153889145206));
#58751=CARTESIAN_POINT('Ctrl Pts',(-7.04715504584287,-1.46464284830267,
-0.00115453508994419));
#58752=CARTESIAN_POINT('Origin',(-17.3,0.,0.));
#58753=CARTESIAN_POINT('',(-6.47584495415715,-1.46530145832529,0.000851233357479376));
#58754=CARTESIAN_POINT('',(-6.54715504584287,-1.4649516336717,0.00103626765265278));
#58755=CARTESIAN_POINT('',(-17.3,-1.4635,-1.79227059055215E-16));
#58756=CARTESIAN_POINT('Ctrl Pts',(-6.47584495415715,-1.46530145832529,
0.000851233357479376));
#58757=CARTESIAN_POINT('Ctrl Pts',(-6.478545486154,-1.46564330146594,0.0503433694787354));
#58758=CARTESIAN_POINT('Ctrl Pts',(-6.48124601815086,-1.46335406023885,
0.0998035045751598));
#58759=CARTESIAN_POINT('Ctrl Pts',(-6.48394655014771,-1.45832971609511,
0.1489842192031));
#58760=CARTESIAN_POINT('Ctrl Pts',(-6.5104610925534,-1.40899936710646,0.631853574228028));
#58761=CARTESIAN_POINT('Ctrl Pts',(-6.53697563495909,-1.09600959912541,
1.08778725603681));
#58762=CARTESIAN_POINT('Ctrl Pts',(-6.56349017736478,-0.663129089947229,
1.30735674874281));
#58763=CARTESIAN_POINT('Ctrl Pts',(-6.59000471977046,-0.230248580769118,
1.52692624144877));
#58764=CARTESIAN_POINT('Ctrl Pts',(-6.61651926217615,0.322522669606081,
1.51013154505203));
#58765=CARTESIAN_POINT('Ctrl Pts',(-6.64303380458183,0.741274789612,1.26468713312949));
#58766=CARTESIAN_POINT('Ctrl Pts',(-6.66954834698752,1.16002690961794,1.01924272120694));
#58767=CARTESIAN_POINT('Ctrl Pts',(-6.6960628893932,1.44475989925459,0.545148593758567));
#58768=CARTESIAN_POINT('Ctrl Pts',(-6.72257743179889,1.46468454547897,0.0601750833208196));
#58769=CARTESIAN_POINT('Ctrl Pts',(-6.74909197420457,1.48460919170335,-0.424798427116929));
#58770=CARTESIAN_POINT('Ctrl Pts',(-6.77560651661026,1.23972549451545,-0.920651320544051));
#58771=CARTESIAN_POINT('Ctrl Pts',(-6.80212105901595,0.842518298341396,
-1.19961859579515));
#58772=CARTESIAN_POINT('Ctrl Pts',(-6.82863560142163,0.445311102167339,
-1.47858587104625));
#58773=CARTESIAN_POINT('Ctrl Pts',(-6.85515014382732,-0.10421959299288,
-1.54066752812133));
#58774=CARTESIAN_POINT('Ctrl Pts',(-6.88166468623301,-0.553652431768097,
-1.3573469870357));
#58775=CARTESIAN_POINT('Ctrl Pts',(-6.90817922863869,-1.00308527054334,
-1.17402644595006));
#58776=CARTESIAN_POINT('Ctrl Pts',(-6.93469377104438,-1.35242025293356,
-0.745303706703668));
#58777=CARTESIAN_POINT('Ctrl Pts',(-6.96120831345007,-1.44119389526058,
-0.268108214497904));
#58778=CARTESIAN_POINT('Ctrl Pts',(-6.96608719368576,-1.45752892991337,
-0.18030056464817));
#58779=CARTESIAN_POINT('Ctrl Pts',(-6.97096607392146,-1.46504166051458,
-0.0908516837366048));
#58780=CARTESIAN_POINT('Ctrl Pts',(-6.97584495415715,-1.46422371240563,
-0.00126593926974311));
#58781=CARTESIAN_POINT('Ctrl Pts',(-7.04715504584287,-1.46464284830267,
-0.00115453508994419));
#58782=CARTESIAN_POINT('Ctrl Pts',(-7.04305714912202,-1.46529287868852,
-0.0763441716942909));
#58783=CARTESIAN_POINT('Ctrl Pts',(-7.03895925240117,-1.46000503173595,
-0.151442128838845));
#58784=CARTESIAN_POINT('Ctrl Pts',(-7.03486135568032,-1.44846188136273,
-0.225565960572915));
#58785=CARTESIAN_POINT('Ctrl Pts',(-7.00834681327463,-1.37377445732185,
-0.705167964641356));
#58786=CARTESIAN_POINT('Ctrl Pts',(-6.98183227086895,-1.03721167419188,
-1.14398866290993));
#58787=CARTESIAN_POINT('Ctrl Pts',(-6.95531772846326,-0.593370235366074,
-1.34046021504245));
#58788=CARTESIAN_POINT('Ctrl Pts',(-6.92880318605757,-0.149528796540265,
-1.53693176717497));
#58789=CARTESIAN_POINT('Ctrl Pts',(-6.90228864365188,0.401591297981385,
-1.49105417317145));
#58790=CARTESIAN_POINT('Ctrl Pts',(-6.8757741012462,0.806838618339453,-1.22390084087157));
#58791=CARTESIAN_POINT('Ctrl Pts',(-6.84925955884051,1.2120859386975,-0.956747508571697));
#58792=CARTESIAN_POINT('Ctrl Pts',(-6.82274501643483,1.47146048489198,-0.468318437975495));
#58793=CARTESIAN_POINT('Ctrl Pts',(-6.79623047402914,1.46582118786923,0.0170314275291633));
#58794=CARTESIAN_POINT('Ctrl Pts',(-6.76971593162346,1.46018189084648,0.502381293033822));
#58795=CARTESIAN_POINT('Ctrl Pts',(-6.74320138921777,1.18952875060651,0.984651953446936));
#58796=CARTESIAN_POINT('Ctrl Pts',(-6.71668684681208,0.778183544070094,
1.24231726868323));
#58797=CARTESIAN_POINT('Ctrl Pts',(-6.69017230440639,0.366838337533681,
1.49998258391951));
#58798=CARTESIAN_POINT('Ctrl Pts',(-6.6636577620007,-0.185198935299168,
1.53304255397898));
#58799=CARTESIAN_POINT('Ctrl Pts',(-6.63714321959502,-0.624355548007335,
1.32631141667502));
#58800=CARTESIAN_POINT('Ctrl Pts',(-6.61062867718933,-1.06351216071555,
1.11958027937104));
#58801=CARTESIAN_POINT('Ctrl Pts',(-6.58411413478364,-1.38978811329906,
0.673058034703574));
#58802=CARTESIAN_POINT('Ctrl Pts',(-6.55759959237795,-1.45331185371989,
0.191850150292584));
#58803=CARTESIAN_POINT('Ctrl Pts',(-6.55411807686626,-1.46165289480791,
0.128664722149329));
#58804=CARTESIAN_POINT('Ctrl Pts',(-6.55063656135457,-1.46546376299974,
0.0648812707058691));
#58805=CARTESIAN_POINT('Ctrl Pts',(-6.54715504584287,-1.4649516336717,0.00103626765265278));
#58806=CARTESIAN_POINT('Origin',(-17.3,0.,0.));
#58807=CARTESIAN_POINT('',(-5.97584495415714,-1.46156852434996,0.000844616552042321));
#58808=CARTESIAN_POINT('',(-6.04715504584287,-1.46134752925932,0.000644857312986237));
#58809=CARTESIAN_POINT('',(-17.3,-1.4635,-1.79227059055215E-16));
#58810=CARTESIAN_POINT('Ctrl Pts',(-5.97584495415714,-1.46156852434996,
0.000844616552042321));
#58811=CARTESIAN_POINT('Ctrl Pts',(-5.98612489838655,-1.46256065115051,
0.190476374356358));
#58812=CARTESIAN_POINT('Ctrl Pts',(-5.99640484261595,-1.42832625212033,
0.37976377404471));
#58813=CARTESIAN_POINT('Ctrl Pts',(-6.00668478684535,-1.35720709570256,
0.553995268745348));
#58814=CARTESIAN_POINT('Ctrl Pts',(-6.03319932925104,-1.17377303744159,
1.00338178792832));
#58815=CARTESIAN_POINT('Ctrl Pts',(-6.05971387165673,-0.744962072740432,
1.35260846735091));
#58816=CARTESIAN_POINT('Ctrl Pts',(-6.08622841406242,-0.267744172268927,
1.44126157120546));
#58817=CARTESIAN_POINT('Ctrl Pts',(-6.1127429564681,0.20947372820258,1.52991467506002));
#58818=CARTESIAN_POINT('Ctrl Pts',(-6.13925749887378,0.735098564444436,
1.35799420334655));
#58819=CARTESIAN_POINT('Ctrl Pts',(-6.16577204127946,1.06768989509561,1.00447008234607));
#58820=CARTESIAN_POINT('Ctrl Pts',(-6.19228658368516,1.40028122574683,0.650945961345559));
#58821=CARTESIAN_POINT('Ctrl Pts',(-6.21880112609086,1.53983905080732,0.115818191058003));
#58822=CARTESIAN_POINT('Ctrl Pts',(-6.24531566849655,1.4222588977432,-0.355107710713123));
#58823=CARTESIAN_POINT('Ctrl Pts',(-6.27183021090223,1.3046787446791,-0.826033612484143));
#58824=CARTESIAN_POINT('Ctrl Pts',(-6.2983447533079,0.929960613490508,-1.23275764573877));
#58825=CARTESIAN_POINT('Ctrl Pts',(-6.32485929571358,0.470227479999877,
-1.38845524791783));
#58826=CARTESIAN_POINT('Ctrl Pts',(-6.35137383811927,0.0104943465091679,
-1.54415285009693));
#58827=CARTESIAN_POINT('Ctrl Pts',(-6.37788838052497,-0.534253789283616,
-1.44882402120037));
#58828=CARTESIAN_POINT('Ctrl Pts',(-6.40440292293066,-0.913792392181853,
-1.14625709263157));
#58829=CARTESIAN_POINT('Ctrl Pts',(-6.42821693333949,-1.25467461830821,
-0.874506900753448));
#58830=CARTESIAN_POINT('Ctrl Pts',(-6.45203094374832,-1.46228699446443,
-0.435583604711616));
#58831=CARTESIAN_POINT('Ctrl Pts',(-6.47584495415715,-1.46530145832529,
0.000851233357479376));
#58832=CARTESIAN_POINT('Ctrl Pts',(-6.54715504584287,-1.4649516336717,0.00103626765265278));
#58833=CARTESIAN_POINT('Ctrl Pts',(-6.52412201894888,-1.4615634860256,-0.42134980744384));
#58834=CARTESIAN_POINT('Ctrl Pts',(-6.50108899205489,-1.26896261059051,
-0.846429927107413));
#58835=CARTESIAN_POINT('Ctrl Pts',(-6.4780559651609,-0.947140017824197,
-1.11885996039094));
#58836=CARTESIAN_POINT('Ctrl Pts',(-6.45154142275521,-0.576672913249429,
-1.43246866250914));
#58837=CARTESIAN_POINT('Ctrl Pts',(-6.42502688034953,-0.0349671758416458,
-1.54379254259112));
#58838=CARTESIAN_POINT('Ctrl Pts',(-6.39851233794385,0.429150154066261,
-1.40169610458007));
#58839=CARTESIAN_POINT('Ctrl Pts',(-6.37199779553816,0.893267483974247,
-1.25959966656899));
#58840=CARTESIAN_POINT('Ctrl Pts',(-6.34548325313247,1.27979640638233,-0.864082910464783));
#58841=CARTESIAN_POINT('Ctrl Pts',(-6.31896871072678,1.41118877822275,-0.396822449652507));
#58842=CARTESIAN_POINT('Ctrl Pts',(-6.29245416832109,1.54258115006316,0.0704380111597157));
#58843=CARTESIAN_POINT('Ctrl Pts',(-6.2659396259154,1.418836971336,0.609442176679984));
#58844=CARTESIAN_POINT('Ctrl Pts',(-6.23942508350972,1.09679687640198,0.972603946241689));
#58845=CARTESIAN_POINT('Ctrl Pts',(-6.21291054110403,0.774756781467961,
1.33576571580339));
#58846=CARTESIAN_POINT('Ctrl Pts',(-6.18639599869835,0.254420770327094,
1.52308508940653));
#58847=CARTESIAN_POINT('Ctrl Pts',(-6.15988145629266,-0.225200083867905,
1.44851881125373));
#58848=CARTESIAN_POINT('Ctrl Pts',(-6.13336691388698,-0.704820938062904,
1.37395253310093));
#58849=CARTESIAN_POINT('Ctrl Pts',(-6.10685237148129,-1.14372663531203,
1.03750060319219));
#58850=CARTESIAN_POINT('Ctrl Pts',(-6.0803378290756,-1.34031029185887,0.593708805617051));
#58851=CARTESIAN_POINT('Ctrl Pts',(-6.06927690133136,-1.42231802887709,
0.408574590160477));
#58852=CARTESIAN_POINT('Ctrl Pts',(-6.05821597358711,-1.46215536248318,
0.204760416790964));
#58853=CARTESIAN_POINT('Ctrl Pts',(-6.04715504584287,-1.46134752925932,
0.000644857312986237));
#58854=CARTESIAN_POINT('Origin',(-17.3,0.,0.));
#58855=CARTESIAN_POINT('',(-5.47584495415715,-1.46220625068146,-0.00117056217213363));
#58856=CARTESIAN_POINT('',(-5.54715504584287,-1.46258246545509,-0.00127304540250365));
#58857=CARTESIAN_POINT('',(-17.3,-1.4635,-1.79227059055215E-16));
#58858=CARTESIAN_POINT('Ctrl Pts',(-5.47584495415715,-1.46220625068146,
-0.00117056217213363));
#58859=CARTESIAN_POINT('Ctrl Pts',(-5.4937043106191,-1.45975057338693,0.327916119857958));
#58860=CARTESIAN_POINT('Ctrl Pts',(-5.51156366708105,-1.34989031251731,
0.65848819549645));
#58861=CARTESIAN_POINT('Ctrl Pts',(-5.529423023543,-1.14602623965269,0.914081898106037));
#58862=CARTESIAN_POINT('Ctrl Pts',(-5.55593756594869,-0.843363452419451,
1.29354406298907));
#58863=CARTESIAN_POINT('Ctrl Pts',(-5.58245210835437,-0.333504302688776,
1.50774435361542));
#58864=CARTESIAN_POINT('Ctrl Pts',(-5.60896665076006,0.1493525764932,1.4582920373891));
#58865=CARTESIAN_POINT('Ctrl Pts',(-5.63548119316574,0.632209455675149,
1.40883972116278));
#58866=CARTESIAN_POINT('Ctrl Pts',(-5.66199573557143,1.0880640643084,1.09573479808381));
#58867=CARTESIAN_POINT('Ctrl Pts',(-5.68851027797711,1.30752420796813,0.662798841274575));
#58868=CARTESIAN_POINT('Ctrl Pts',(-5.7150248203828,1.52698435162785,0.229862884465363));
#58869=CARTESIAN_POINT('Ctrl Pts',(-5.74153936278849,1.51005003031407,-0.322904106074104));
#58870=CARTESIAN_POINT('Ctrl Pts',(-5.76805390519417,1.26449985289427,-0.741594215489832));
#58871=CARTESIAN_POINT('Ctrl Pts',(-5.79456844759986,1.01894967547444,-1.16028432490561));
#58872=CARTESIAN_POINT('Ctrl Pts',(-5.82108299000554,0.54478364194851,-1.44489755319761));
#58873=CARTESIAN_POINT('Ctrl Pts',(-5.84759753241123,0.0598051141809271,
-1.46469969848274));
#58874=CARTESIAN_POINT('Ctrl Pts',(-5.87411207481692,-0.425173413586656,
-1.48450184376786));
#58875=CARTESIAN_POINT('Ctrl Pts',(-5.90062661722261,-0.920964435595895,
-1.23949290604612));
#58876=CARTESIAN_POINT('Ctrl Pts',(-5.9271411596283,-1.19983137069012,-0.842215257713543));
#58877=CARTESIAN_POINT('Ctrl Pts',(-5.94337575780458,-1.37057890110706,
-0.598965991465038));
#58878=CARTESIAN_POINT('Ctrl Pts',(-5.95961035598086,-1.46000170846191,
-0.298631267821943));
#58879=CARTESIAN_POINT('Ctrl Pts',(-5.97584495415714,-1.46156852434996,
0.000844616552042321));
#58880=CARTESIAN_POINT('Ctrl Pts',(-6.04715504584287,-1.46134752925932,
0.000644857312986237));
#58881=CARTESIAN_POINT('Ctrl Pts',(-6.03170143118143,-1.46021887679535,
-0.284532234113107));
#58882=CARTESIAN_POINT('Ctrl Pts',(-6.01624781651998,-1.37975136403226,
-0.570297627475704));
#58883=CARTESIAN_POINT('Ctrl Pts',(-6.00079420185854,-1.22410460259934,
-0.806529445355322));
#58884=CARTESIAN_POINT('Ctrl Pts',(-5.97427965945285,-0.95705364094843,
-1.21184423351093));
#58885=CARTESIAN_POINT('Ctrl Pts',(-5.94776511704716,-0.468690101802097,
-1.47134214458061));
#58886=CARTESIAN_POINT('Ctrl Pts',(-5.92125057464148,0.0166611726591288,
-1.46582544310558));
#58887=CARTESIAN_POINT('Ctrl Pts',(-5.89473603223579,0.502012447120327,
-1.46030874163054));
#58888=CARTESIAN_POINT('Ctrl Pts',(-5.86822148983011,0.984351456896417,
-1.18977742761082));
#58889=CARTESIAN_POINT('Ctrl Pts',(-5.84170694742443,1.24212066631498,-0.778497318327611));
#58890=CARTESIAN_POINT('Ctrl Pts',(-5.81519240501874,1.49988987573356,-0.36721720904436));
#58891=CARTESIAN_POINT('Ctrl Pts',(-5.78867786261305,1.53308928479456,0.184811695502411));
#58892=CARTESIAN_POINT('Ctrl Pts',(-5.76216332020736,1.32646908141922,0.624020512778951));
#58893=CARTESIAN_POINT('Ctrl Pts',(-5.73564877780167,1.11984887804388,1.06322933005547));
#58894=CARTESIAN_POINT('Ctrl Pts',(-5.70913423539599,0.673409062232237,
1.38961806006177));
#58895=CARTESIAN_POINT('Ctrl Pts',(-5.68261969299031,0.19221723874469,1.45326334759375));
#58896=CARTESIAN_POINT('Ctrl Pts',(-5.65610515058462,-0.288974584742884,
1.51690863512575));
#58897=CARTESIAN_POINT('Ctrl Pts',(-5.62959060817893,-0.804918415906365,
1.31781048018338));
#58898=CARTESIAN_POINT('Ctrl Pts',(-5.60307606577324,-1.11862068495122,
0.9474226023952));
#58899=CARTESIAN_POINT('Ctrl Pts',(-5.58443572579645,-1.33916067606315,
0.687031309963428));
#58900=CARTESIAN_POINT('Ctrl Pts',(-5.56579538581966,-1.45974445354556,
0.341981493586538));
#58901=CARTESIAN_POINT('Ctrl Pts',(-5.54715504584287,-1.46258246545509,
-0.00127304540250365));
#58902=CARTESIAN_POINT('Origin',(-17.3,0.,0.));
#58903=CARTESIAN_POINT('',(-4.97584495415715,-1.46580988090682,-0.00036561919089767));
#58904=CARTESIAN_POINT('',(-5.04715504584287,-1.46591140803628,-0.000101597247445848));
#58905=CARTESIAN_POINT('',(-17.3,-1.4635,-1.79227059055215E-16));
#58906=CARTESIAN_POINT('Ctrl Pts',(-4.97584495415715,-1.46580988090682,
-0.00036561919089767));
#58907=CARTESIAN_POINT('Ctrl Pts',(-5.00128372285165,-1.46425219013824,
0.465417621113056));
#58908=CARTESIAN_POINT('Ctrl Pts',(-5.02672249154614,-1.22313864729725,
0.932587879623785));
#58909=CARTESIAN_POINT('Ctrl Pts',(-5.05216126024064,-0.841912163350243,
1.20004406903268));
#58910=CARTESIAN_POINT('Ctrl Pts',(-5.07867580264632,-0.444564088206552,
1.47881064617758));
#58911=CARTESIAN_POINT('Ctrl Pts',(-5.10519034505201,0.10499789945747,1.54061468150885));
#58912=CARTESIAN_POINT('Ctrl Pts',(-5.1317048874577,0.554338070376188,1.35706711777613));
#58913=CARTESIAN_POINT('Ctrl Pts',(-5.15821942986338,1.00367824129491,1.17351955404341));
#58914=CARTESIAN_POINT('Ctrl Pts',(-5.18473397226907,1.35279659546832,0.744620391246714));
#58915=CARTESIAN_POINT('Ctrl Pts',(-5.21124851467476,1.44132915519413,0.267380112957177));
#58916=CARTESIAN_POINT('Ctrl Pts',(-5.23776305708044,1.52986171491994,-0.209860165332388));
#58917=CARTESIAN_POINT('Ctrl Pts',(-5.26427759948613,1.35780848019811,-0.735441559114797));
#58918=CARTESIAN_POINT('Ctrl Pts',(-5.29079214189182,1.00420036065203,-1.06794358188246));
#58919=CARTESIAN_POINT('Ctrl Pts',(-5.3173066842975,0.650592241105968,-1.40044560465011));
#58920=CARTESIAN_POINT('Ctrl Pts',(-5.34382122670319,0.115429236735669,
-1.53986825640303));
#58921=CARTESIAN_POINT('Ctrl Pts',(-5.37033576910888,-0.355466950236626,
-1.42216915509621));
#58922=CARTESIAN_POINT('Ctrl Pts',(-5.39685031151456,-0.826363137208922,
-1.3044700537894));
#58923=CARTESIAN_POINT('Ctrl Pts',(-5.42336485392025,-1.23299250678321,
-0.929649199422844));
#58924=CARTESIAN_POINT('Ctrl Pts',(-5.44987939632593,-1.38857397920246,
-0.469876752669737));
#58925=CARTESIAN_POINT('Ctrl Pts',(-5.45853458226967,-1.43936069664173,
-0.319792472218341));
#58926=CARTESIAN_POINT('Ctrl Pts',(-5.46718976821341,-1.46339634639668,
-0.160655951841513));
#58927=CARTESIAN_POINT('Ctrl Pts',(-5.47584495415715,-1.46220625068146,
-0.00117056217213363));
#58928=CARTESIAN_POINT('Ctrl Pts',(-5.54715504584287,-1.46258246545509,
-0.00127304540250365));
#58929=CARTESIAN_POINT('Ctrl Pts',(-5.53928084341397,-1.463781321286,-0.146273390246097));
#58930=CARTESIAN_POINT('Ctrl Pts',(-5.53140664098508,-1.44396898032646,
-0.290953375998168));
#58931=CARTESIAN_POINT('Ctrl Pts',(-5.52353243855618,-1.40180445964895,
-0.428796083515654));
#58932=CARTESIAN_POINT('Ctrl Pts',(-5.4970178961505,-1.25982525837558,-0.892949291004386));
#58933=CARTESIAN_POINT('Ctrl Pts',(-5.47050335374481,-0.864406148902612,
-1.27957810534789));
#58934=CARTESIAN_POINT('Ctrl Pts',(-5.44398881133913,-0.397178891624646,
-1.41108849913032));
#58935=CARTESIAN_POINT('Ctrl Pts',(-5.41747426893344,0.0700483656533723,
-1.54259889291276));
#58936=CARTESIAN_POINT('Ctrl Pts',(-5.39095972652775,0.609083770736402,
-1.41899086613407));
#58937=CARTESIAN_POINT('Ctrl Pts',(-5.36444518412206,0.972326873381239,
-1.09704251313735));
#58938=CARTESIAN_POINT('Ctrl Pts',(-5.33793064171637,1.33556997602601,-0.775094160140676));
#58939=CARTESIAN_POINT('Ctrl Pts',(-5.31141609931069,1.52302077623267,-0.254805480926044));
#58940=CARTESIAN_POINT('Ctrl Pts',(-5.284901556905,1.4485756487255,0.224834192794464));
#58941=CARTESIAN_POINT('Ctrl Pts',(-5.25838701449932,1.37413052121833,0.704473866514999));
#58942=CARTESIAN_POINT('Ctrl Pts',(-5.23187247209363,1.0377894659973,1.14346453474141));
#58943=CARTESIAN_POINT('Ctrl Pts',(-5.20535792968795,0.594047337987869,
1.34016028316003));
#58944=CARTESIAN_POINT('Ctrl Pts',(-5.17884338728226,0.150305209978438,
1.53685603157865));
#58945=CARTESIAN_POINT('Ctrl Pts',(-5.15232884487657,-0.4008379908194,1.49125686018949));
#58946=CARTESIAN_POINT('Ctrl Pts',(-5.12581430247089,-0.806220220912455,
1.22430828622611));
#58947=CARTESIAN_POINT('Ctrl Pts',(-5.09959455026155,-1.20709538822551,
0.960327661749831));
#58948=CARTESIAN_POINT('Ctrl Pts',(-5.07337479805221,-1.46543272473564,
0.479892224027581));
#58949=CARTESIAN_POINT('Ctrl Pts',(-5.04715504584287,-1.46591140803628,
-0.000101597247445848));
#58950=CARTESIAN_POINT('Origin',(-17.3,0.,0.));
#58951=CARTESIAN_POINT('',(-4.47584495415716,-1.46331444493144,0.00135213804196392));
#58952=CARTESIAN_POINT('',(-4.54715504584288,-1.46288856329395,0.00132347729660035));
#58953=CARTESIAN_POINT('',(-17.3,-1.4635,-1.79227059055215E-16));
#58954=CARTESIAN_POINT('Ctrl Pts',(-4.47584495415716,-1.46331444493144,
0.00135213804196392));
#58955=CARTESIAN_POINT('Ctrl Pts',(-4.48234859267851,-1.46440871301316,
0.120962016398508));
#58956=CARTESIAN_POINT('Ctrl Pts',(-4.48885223119987,-1.45097840452381,
0.24032935462986));
#58957=CARTESIAN_POINT('Ctrl Pts',(-4.49535586972122,-1.42207932171114,
0.355826167080497));
#58958=CARTESIAN_POINT('Ctrl Pts',(-4.52187041212691,-1.3042612796711,0.826692609209612));
#58959=CARTESIAN_POINT('Ctrl Pts',(-4.54838495453259,-0.929337726041169,
1.23322728915951));
#58960=CARTESIAN_POINT('Ctrl Pts',(-4.57489949693828,-0.469525995360321,
1.38869262189244));
#58961=CARTESIAN_POINT('Ctrl Pts',(-4.60141403934397,-0.00971426467944604,
1.54415795462538));
#58962=CARTESIAN_POINT('Ctrl Pts',(-4.62792858174965,0.534985643052358,
1.44855394014133));
#58963=CARTESIAN_POINT('Ctrl Pts',(-4.65444312415534,0.914371345709493,
1.14579531355431));
#58964=CARTESIAN_POINT('Ctrl Pts',(-4.68095766656103,1.29375704836661,0.84303668696731));
#58965=CARTESIAN_POINT('Ctrl Pts',(-4.70747220896671,1.50782854594907,0.33312344827737));
#58966=CARTESIAN_POINT('Ctrl Pts',(-4.7339867513724,1.45825426564029,-0.149720924254138));
#58967=CARTESIAN_POINT('Ctrl Pts',(-4.76050129377809,1.40867998533151,-0.632565296785646));
#58968=CARTESIAN_POINT('Ctrl Pts',(-4.78701583618377,1.09545992713148,-1.08834080315872));
#58969=CARTESIAN_POINT('Ctrl Pts',(-4.81353037858946,0.662468550313567,
-1.30769158377006));
#58970=CARTESIAN_POINT('Ctrl Pts',(-4.84004492099515,0.22947717349565,-1.5270423643814));
#58971=CARTESIAN_POINT('Ctrl Pts',(-4.86655946340083,-0.32328552194016,
-1.509968419231));
#58972=CARTESIAN_POINT('Ctrl Pts',(-4.89307400580652,-0.741913594052176,
-1.2643124919806));
#58973=CARTESIAN_POINT('Ctrl Pts',(-4.9195885482122,-1.16054166616422,-1.01865656473018));
#58974=CARTESIAN_POINT('Ctrl Pts',(-4.94610309061789,-1.44503511495245,
-0.544418655379736));
#58975=CARTESIAN_POINT('Ctrl Pts',(-4.97261763302358,-1.46471475803487,
-0.0594351412252308));
#58976=CARTESIAN_POINT('Ctrl Pts',(-4.97369340673477,-1.46551321958664,
-0.0397579200646598));
#58977=CARTESIAN_POINT('Ctrl Pts',(-4.97476918044596,-1.46587575370118,
-0.0200630098566805));
#58978=CARTESIAN_POINT('Ctrl Pts',(-4.97584495415715,-1.46580988090682,
-0.00036561919089767));
#58979=CARTESIAN_POINT('Ctrl Pts',(-5.04715504584287,-1.46591140803628,
-0.000101597247445848));
#58980=CARTESIAN_POINT('Ctrl Pts',(-5.04686025564653,-1.46591678990042,
-0.00549819564738455));
#58981=CARTESIAN_POINT('Ctrl Pts',(-5.04656546545018,-1.46588957679224,
-0.0108947382241984));
#58982=CARTESIAN_POINT('Ctrl Pts',(-5.04627067525383,-1.46582960481847,
-0.016290916725986));
#58983=CARTESIAN_POINT('Ctrl Pts',(-5.01975613284814,-1.46043549924315,
-0.501643569177134));
#58984=CARTESIAN_POINT('Ctrl Pts',(-4.99324159044245,-1.1900260287042,-0.984050897541824));
#58985=CARTESIAN_POINT('Ctrl Pts',(-4.96672704803676,-0.778811042914844,
-1.2419239846963));
#58986=CARTESIAN_POINT('Ctrl Pts',(-4.94021250563108,-0.367596057125508,
-1.49979707185076));
#58987=CARTESIAN_POINT('Ctrl Pts',(-4.91369796322539,0.184424443914241,
-1.53313591779505));
#58988=CARTESIAN_POINT('Ctrl Pts',(-4.88718342081971,0.623685437736442,
-1.32662666153125));
#58989=CARTESIAN_POINT('Ctrl Pts',(-4.86066887841402,1.06294643155864,-1.12011740526745));
#58990=CARTESIAN_POINT('Ctrl Pts',(-4.83415433600833,1.38944791816332,-0.673760046795552));
#58991=CARTESIAN_POINT('Ctrl Pts',(-4.80763979360265,1.45321474874567,-0.192584314932677));
#58992=CARTESIAN_POINT('Ctrl Pts',(-4.78112525119696,1.51698157932803,0.288591416930226));
#58993=CARTESIAN_POINT('Ctrl Pts',(-4.75461070879128,1.31801375388804,0.804585522184146));
#58994=CARTESIAN_POINT('Ctrl Pts',(-4.72809616638559,0.947705126518188,
1.11838133814061));
#58995=CARTESIAN_POINT('Ctrl Pts',(-4.7015816239799,0.57739649914834,1.43217715409708));
#58996=CARTESIAN_POINT('Ctrl Pts',(-4.67506708157421,0.0357470698487191,
1.5437746807561));
#58997=CARTESIAN_POINT('Ctrl Pts',(-4.64855253916852,-0.428441985606666,
1.40191272527909));
#58998=CARTESIAN_POINT('Ctrl Pts',(-4.62203799676284,-0.892631041062025,
1.2600507698021));
#58999=CARTESIAN_POINT('Ctrl Pts',(-4.59552345435715,-1.2793597226731,0.864729332189069));
#59000=CARTESIAN_POINT('Ctrl Pts',(-4.56900891195147,-1.41098813000681,
0.397535308255665));
#59001=CARTESIAN_POINT('Ctrl Pts',(-4.56172428991527,-1.44715180132278,
0.269178128642617));
#59002=CARTESIAN_POINT('Ctrl Pts',(-4.55443966787907,-1.46405988843861,
0.135395832802253));
#59003=CARTESIAN_POINT('Ctrl Pts',(-4.54715504584288,-1.46288856329395,
0.00132347729660035));
#59004=CARTESIAN_POINT('Origin',(-17.3,0.,0.));
#59005=CARTESIAN_POINT('',(-3.97584495415716,-1.46111494020071,-0.00025097937605606));
#59006=CARTESIAN_POINT('',(-4.04715504584288,-1.46122237770127,-0.000480703445675848));
#59007=CARTESIAN_POINT('',(-17.3,-1.4635,-1.79227059055215E-16));
#59008=CARTESIAN_POINT('Ctrl Pts',(-3.97584495415716,-1.46111494020071,
-0.00025097937605606));
#59009=CARTESIAN_POINT('Ctrl Pts',(-3.98992800491106,-1.46071820887633,
0.259737348729522));
#59010=CARTESIAN_POINT('Ctrl Pts',(-4.00401105566496,-1.39465998093067,
0.519913933469384));
#59011=CARTESIAN_POINT('Ctrl Pts',(-4.01809410641886,-1.26412505040052,
0.742232925278513));
#59012=CARTESIAN_POINT('Ctrl Pts',(-4.04460864882455,-1.01836338899302,
1.16079893337724));
#59013=CARTESIAN_POINT('Ctrl Pts',(-4.07112319123024,-0.544053634075698,
1.44517258451028));
#59014=CARTESIAN_POINT('Ctrl Pts',(-4.09763773363593,-0.0590651644775016,
1.46472972413441));
#59015=CARTESIAN_POINT('Ctrl Pts',(-4.12415227604161,0.425923305120695,
1.48428686375854));
#59016=CARTESIAN_POINT('Ctrl Pts',(-4.1506668184473,0.921590489399769,1.23902749187376));
#59017=CARTESIAN_POINT('Ctrl Pts',(-4.17718136085298,1.20025669080933,0.841609015270768));
#59018=CARTESIAN_POINT('Ctrl Pts',(-4.20369590325867,1.4789228922189,0.444190538667776));
#59019=CARTESIAN_POINT('Ctrl Pts',(-4.23021044566436,1.54058811075896,-0.10538704265343));
#59020=CARTESIAN_POINT('Ctrl Pts',(-4.25672498807004,1.3569270532653,-0.554680836638826));
#59021=CARTESIAN_POINT('Ctrl Pts',(-4.28323953047573,1.17326599577164,-1.00397463062425));
#59022=CARTESIAN_POINT('Ctrl Pts',(-4.30975407288142,0.744278662244238,
-1.35298463727385));
#59023=CARTESIAN_POINT('Ctrl Pts',(-4.3362686152871,0.267016036585803,-1.44139664722228));
#59024=CARTESIAN_POINT('Ctrl Pts',(-4.36278315769279,-0.210246589072633,
-1.52980865717071));
#59025=CARTESIAN_POINT('Ctrl Pts',(-4.38929770009848,-0.735784506862102,
-1.35762267041797));
#59026=CARTESIAN_POINT('Ctrl Pts',(-4.41581224250417,-1.06819720053174,
-1.00393057488741));
#59027=CARTESIAN_POINT('Ctrl Pts',(-4.4358231463885,-1.31907380858995,-0.736994098292163));
#59028=CARTESIAN_POINT('Ctrl Pts',(-4.45583405027283,-1.45994751527582,
-0.366672894645548));
#59029=CARTESIAN_POINT('Ctrl Pts',(-4.47584495415716,-1.46331444493144,
0.00135213804196392));
#59030=CARTESIAN_POINT('Ctrl Pts',(-4.54715504584288,-1.46288856329395,
0.00132347729660035));
#59031=CARTESIAN_POINT('Ctrl Pts',(-4.52792512547339,-1.45979650317788,
-0.352600268824065));
#59032=CARTESIAN_POINT('Ctrl Pts',(-4.5086952051039,-1.33071758853706,-0.708545303265838));
#59033=CARTESIAN_POINT('Ctrl Pts',(-4.48946528473441,-1.09728807987873,
-0.972049738483633));
#59034=CARTESIAN_POINT('Ctrl Pts',(-4.46295074232872,-0.775431489360546,
-1.33537415103575));
#59035=CARTESIAN_POINT('Ctrl Pts',(-4.43643619992304,-0.255190175267832,
-1.52295636588615));
#59036=CARTESIAN_POINT('Ctrl Pts',(-4.40992165751735,0.22446828737602,-1.44863239377439));
#59037=CARTESIAN_POINT('Ctrl Pts',(-4.38340711511166,0.704126750019844,
-1.37430842166264));
#59038=CARTESIAN_POINT('Ctrl Pts',(-4.35689257270597,1.14320236121478,-1.03807826258876));
#59039=CARTESIAN_POINT('Ctrl Pts',(-4.33037803030029,1.34001018895549,-0.594385832456929));
#59040=CARTESIAN_POINT('Ctrl Pts',(-4.3038634878946,1.53681801669619,-0.150693402325121));
#59041=CARTESIAN_POINT('Ctrl Pts',(-4.27734894548891,1.49135806098265,0.400461298864684));
#59042=CARTESIAN_POINT('Ctrl Pts',(-4.25083440308323,1.2245118917388,0.805910945030719));
#59043=CARTESIAN_POINT('Ctrl Pts',(-4.22431986067754,0.957665722494918,
1.2113605911968));
#59044=CARTESIAN_POINT('Ctrl Pts',(-4.19780531827186,0.469433339720774,
1.47110518233911));
#59045=CARTESIAN_POINT('Ctrl Pts',(-4.17129077586617,-0.0159206597535222,
1.46583367300764));
#59046=CARTESIAN_POINT('Ctrl Pts',(-4.14477623346049,-0.501274659227791,
1.46056216367617));
#59047=CARTESIAN_POINT('Ctrl Pts',(-4.1182616910548,-0.983750275402204,
1.19027455387084));
#59048=CARTESIAN_POINT('Ctrl Pts',(-4.09174714864911,-1.24172722383962,
0.779124717811985));
#59049=CARTESIAN_POINT('Ctrl Pts',(-4.07688311438036,-1.38634892401639,
0.548634401997345));
#59050=CARTESIAN_POINT('Ctrl Pts',(-4.06201908011162,-1.46041707087967,
0.273875090335108));
#59051=CARTESIAN_POINT('Ctrl Pts',(-4.04715504584288,-1.46122237770127,
-0.000480703445675848));
#59052=CARTESIAN_POINT('Origin',(-17.3,0.,0.));
#59053=CARTESIAN_POINT('',(-3.47584495415716,-1.46423846103291,-0.0012628549216627));
#59054=CARTESIAN_POINT('',(-3.54715504584288,-1.46465674957962,-0.0011499352553702));
#59055=CARTESIAN_POINT('',(-17.3,-1.4635,-1.79227059055215E-16));
#59056=CARTESIAN_POINT('Ctrl Pts',(-3.47584495415716,-1.46423846103291,
-0.0012628549216627));
#59057=CARTESIAN_POINT('Ctrl Pts',(-3.49750741714361,-1.46061129198041,
0.396491821226815));
#59058=CARTESIAN_POINT('Ctrl Pts',(-3.51916988013006,-1.29269684904186,
0.796941553735221));
#59059=CARTESIAN_POINT('Ctrl Pts',(-3.54083234311651,-1.00366072506953,
1.06845075102716));
#59060=CARTESIAN_POINT('Ctrl Pts',(-3.56734688552219,-0.649884676121027,
1.40077409439001));
#59061=CARTESIAN_POINT('Ctrl Pts',(-3.59386142792788,-0.114651306021696,
1.53992637284989));
#59062=CARTESIAN_POINT('Ctrl Pts',(-3.62037597033356,0.356185361221739,
1.42198939759372));
#59063=CARTESIAN_POINT('Ctrl Pts',(-3.64689051273925,0.827022028465174,
1.30405242233755));
#59064=CARTESIAN_POINT('Ctrl Pts',(-3.67340505514494,1.23346199285271,0.929026193365342));
#59065=CARTESIAN_POINT('Ctrl Pts',(-3.69991959755062,1.38881117598024,0.46917520809393));
#59066=CARTESIAN_POINT('Ctrl Pts',(-3.72643413995631,1.54416035910777,0.00932422282251724));
#59067=CARTESIAN_POINT('Ctrl Pts',(-3.752948682362,1.44841876097529,-0.535351518748095));
#59068=CARTESIAN_POINT('Ctrl Pts',(-3.77946322476768,1.14556431435133,-0.914660734973559));
#59069=CARTESIAN_POINT('Ctrl Pts',(-3.80597776717337,0.84270986772736,-1.29396995119905));
#59070=CARTESIAN_POINT('Ctrl Pts',(-3.83249230957905,0.332742572611882,
-1.50791264207935));
#59071=CARTESIAN_POINT('Ctrl Pts',(-3.85900685198474,-0.150089262462492,
-1.45821640085108));
#59072=CARTESIAN_POINT('Ctrl Pts',(-3.88552139439043,-0.632921097536866,
-1.4085201596228));
#59073=CARTESIAN_POINT('Ctrl Pts',(-3.91203593679612,-1.08861747257013,
-1.09518498628594));
#59074=CARTESIAN_POINT('Ctrl Pts',(-3.93855047920181,-1.30785887613792,
-0.662138217085276));
#59075=CARTESIAN_POINT('Ctrl Pts',(-3.95098197085359,-1.41065143565023,
-0.459101814880751));
#59076=CARTESIAN_POINT('Ctrl Pts',(-3.96341346250538,-1.46146514572316,
-0.229749742597532));
#59077=CARTESIAN_POINT('Ctrl Pts',(-3.97584495415716,-1.46111494020071,
-0.00025097937605606));
#59078=CARTESIAN_POINT('Ctrl Pts',(-4.04715504584288,-1.46122237770127,
-0.000480703445675848));
#59079=CARTESIAN_POINT('Ctrl Pts',(-4.03550453770593,-1.46185358141812,
-0.215522215734277));
#59080=CARTESIAN_POINT('Ctrl Pts',(-4.02385402956899,-1.41747570995839,
-0.430315826540335));
#59081=CARTESIAN_POINT('Ctrl Pts',(-4.01220352143205,-1.32678415700106,
-0.623350322901187));
#59082=CARTESIAN_POINT('Ctrl Pts',(-3.98568897902636,-1.12038586102462,
-1.06266346524309));
#59083=CARTESIAN_POINT('Ctrl Pts',(-3.95917443662068,-0.674110988371246,
-1.3892776876145));
#59084=CARTESIAN_POINT('Ctrl Pts',(-3.93265989421499,-0.192951378833284,
-1.45316605717873));
#59085=CARTESIAN_POINT('Ctrl Pts',(-3.9061453518093,0.288208230704705,-1.51705442674297));
#59086=CARTESIAN_POINT('Ctrl Pts',(-3.87963080940361,0.804252577127286,
-1.3182169435));
#59087=CARTESIAN_POINT('Ctrl Pts',(-3.85311626699793,1.11814191997438,-0.947987590175135));
#59088=CARTESIAN_POINT('Ctrl Pts',(-3.82660172459224,1.43203126282145,-0.57775823685029));
#59089=CARTESIAN_POINT('Ctrl Pts',(-3.80008718218656,1.54376560209305,-0.0361370134435621));
#59090=CARTESIAN_POINT('Ctrl Pts',(-3.77357263978087,1.40202090146358,0.42808786036197));
#59091=CARTESIAN_POINT('Ctrl Pts',(-3.74705809737518,1.26027620083411,0.892312734167503));
#59092=CARTESIAN_POINT('Ctrl Pts',(-3.7205435549695,0.865052460303565,1.27914125837184));
#59093=CARTESIAN_POINT('Ctrl Pts',(-3.69402901256381,0.397891699522902,
1.4108876708586));
#59094=CARTESIAN_POINT('Ctrl Pts',(-3.66751447015812,-0.069269061257761,
1.54263408334537));
#59095=CARTESIAN_POINT('Ctrl Pts',(-3.64099992775244,-0.608366842288541,
1.41929838411456));
#59096=CARTESIAN_POINT('Ctrl Pts',(-3.61448538534675,-0.971772541566861,
1.09753357661018));
#59097=CARTESIAN_POINT('Ctrl Pts',(-3.59204193884546,-1.27938020249592,
0.825173181596368));
#59098=CARTESIAN_POINT('Ctrl Pts',(-3.56959849234417,-1.46110604285371,
0.41064008787777));
#59099=CARTESIAN_POINT('Ctrl Pts',(-3.54715504584288,-1.46465674957962,
-0.0011499352553702));
#59100=CARTESIAN_POINT('Origin',(-17.3,0.,0.));
#59101=CARTESIAN_POINT('',(-2.97584495415716,-1.46529038421007,0.000858184953542052));
#59102=CARTESIAN_POINT('',(-3.04715504584288,-1.46493873305747,0.00104194039951338));
#59103=CARTESIAN_POINT('',(-17.3,-1.4635,-1.79227059055215E-16));
#59104=CARTESIAN_POINT('Ctrl Pts',(-2.97584495415716,-1.46529038421007,
0.000858184953542052));
#59105=CARTESIAN_POINT('Ctrl Pts',(-2.97857228697047,-1.46563784872126,
0.0508424879856784));
#59106=CARTESIAN_POINT('Ctrl Pts',(-2.98129961978378,-1.46330283124409,
0.10079394579702));
#59107=CARTESIAN_POINT('Ctrl Pts',(-2.98402695259709,-1.45817844302379,
0.150457591094951));
#59108=CARTESIAN_POINT('Ctrl Pts',(-3.01054149500277,-1.40836024404669,
0.633276857906377));
#59109=CARTESIAN_POINT('Ctrl Pts',(-3.03705603740846,-1.09490997556484,
1.08889407252482));
#59110=CARTESIAN_POINT('Ctrl Pts',(-3.06357057981415,-0.66180784161105,
1.30802608506082));
#59111=CARTESIAN_POINT('Ctrl Pts',(-3.09008512221983,-0.228705707657263,
1.52715809759682));
#59112=CARTESIAN_POINT('Ctrl Pts',(-3.11659966462552,0.324048291768454,
1.50980490805039));
#59113=CARTESIAN_POINT('Ctrl Pts',(-3.1431142070312,0.74255220914835,1.26393752816612));
#59114=CARTESIAN_POINT('Ctrl Pts',(-3.16962874943689,1.16105612652827,1.01807014828184));
#59115=CARTESIAN_POINT('Ctrl Pts',(-3.19614329184258,1.44530996186235,0.543688578059681));
#59116=CARTESIAN_POINT('Ctrl Pts',(-3.22265783424827,1.46474459678038,0.0586951839612338));
#59117=CARTESIAN_POINT('Ctrl Pts',(-3.24917237665395,1.48417923169841,-0.426298210137186));
#59118=CARTESIAN_POINT('Ctrl Pts',(-3.27568691905964,1.23879466620043,-0.921903428111893));
#59119=CARTESIAN_POINT('Ctrl Pts',(-3.30220146146532,0.841305813494467,
-1.20046923600649));
#59120=CARTESIAN_POINT('Ctrl Pts',(-3.32871600387101,0.443816960788507,
-1.47903504390108));
#59121=CARTESIAN_POINT('Ctrl Pts',(-3.3552305462767,-0.105776179125424,
-1.54056144171556));
#59122=CARTESIAN_POINT('Ctrl Pts',(-3.38174508868239,-0.555023567511395,
-1.35678690217903));
#59123=CARTESIAN_POINT('Ctrl Pts',(-3.40825963108808,-1.00427095589739,
-1.17301236264248));
#59124=CARTESIAN_POINT('Ctrl Pts',(-3.43477417349376,-1.35317259275541,
-0.743936885754905));
#59125=CARTESIAN_POINT('Ctrl Pts',(-3.46128871589945,-1.44146404728557,
-0.266651943178191));
#59126=CARTESIAN_POINT('Ctrl Pts',(-3.46614079531868,-1.45762111094013,
-0.179310271896277));
#59127=CARTESIAN_POINT('Ctrl Pts',(-3.47099287473792,-1.46505089461079,
-0.0903541682802729));
#59128=CARTESIAN_POINT('Ctrl Pts',(-3.47584495415716,-1.46423846103291,
-0.0012628549216627));
#59129=CARTESIAN_POINT('Ctrl Pts',(-3.54715504584288,-1.46465674957962,
-0.0011499352553702));
#59130=CARTESIAN_POINT('Ctrl Pts',(-3.54308394993848,-1.46530082479368,
-0.075845979668695));
#59131=CARTESIAN_POINT('Ctrl Pts',(-3.53901285403409,-1.46008229464905,
-0.150451767153425));
#59132=CARTESIAN_POINT('Ctrl Pts',(-3.53494175812969,-1.44868904639678,
-0.224102367635917));
#59133=CARTESIAN_POINT('Ctrl Pts',(-3.508427215724,-1.3744862344225,-0.703779588599594));
#59134=CARTESIAN_POINT('Ctrl Pts',(-3.48191267331832,-1.03836699294809,
-1.14294011474894));
#59135=CARTESIAN_POINT('Ctrl Pts',(-3.45539813091263,-0.594724289002558,
-1.33986000925486));
#59136=CARTESIAN_POINT('Ctrl Pts',(-3.42888358850694,-0.151081585057076,
-1.53677990376077));
#59137=CARTESIAN_POINT('Ctrl Pts',(-3.40236904610126,0.400084581359495,
-1.49145916662331));
#59138=CARTESIAN_POINT('Ctrl Pts',(-3.37585450369557,0.805601617729781,
-1.22471541912446));
#59139=CARTESIAN_POINT('Ctrl Pts',(-3.34933996128989,1.21111865410007,-0.957971671625605));
#59140=CARTESIAN_POINT('Ctrl Pts',(-3.32282541888421,1.47098656042407,-0.469804913765352));
#59141=CARTESIAN_POINT('Ctrl Pts',(-3.29631087647852,1.46583764767282,0.0155504017651938));
#59142=CARTESIAN_POINT('Ctrl Pts',(-3.26979633407283,1.46068873492156,0.500905717295823));
#59143=CARTESIAN_POINT('Ctrl Pts',(-3.24328179166714,1.19052300309495,0.983449590496744));
#59144=CARTESIAN_POINT('Ctrl Pts',(-3.21676724926145,0.779438342998958,
1.24153038375752));
#59145=CARTESIAN_POINT('Ctrl Pts',(-3.19025270685576,0.368353682903008,
1.49961117701827));
#59146=CARTESIAN_POINT('Ctrl Pts',(-3.16373816445008,-0.183649905462294,
1.53322889033894));
#59147=CARTESIAN_POINT('Ctrl Pts',(-3.13722362204439,-0.623015168294578,
1.32694156781861));
#59148=CARTESIAN_POINT('Ctrl Pts',(-3.11070907963871,-1.06238043112686,
1.12065424529827));
#59149=CARTESIAN_POINT('Ctrl Pts',(-3.08419453723302,-1.38910736842613,
0.674461886936952));
#59150=CARTESIAN_POINT('Ctrl Pts',(-3.05767999482733,-1.45311727289601,
0.193318430423119));
#59151=CARTESIAN_POINT('Ctrl Pts',(-3.05417167849918,-1.46158685119682,
0.129655123742453));
#59152=CARTESIAN_POINT('Ctrl Pts',(-3.05066336217103,-1.46545685722587,
0.0653799035508948));
#59153=CARTESIAN_POINT('Ctrl Pts',(-3.04715504584288,-1.46493873305747,
0.00104194039951338));
#59154=CARTESIAN_POINT('Origin',(-17.3,0.,0.));
#59155=CARTESIAN_POINT('',(-2.47584495415716,-1.46155994553451,0.000838156444187416));
#59156=CARTESIAN_POINT('',(-2.54715504584288,-1.46134104288809,0.000637616632206692));
#59157=CARTESIAN_POINT('',(-17.3,-1.4635,-1.79227059055215E-16));
#59158=CARTESIAN_POINT('Ctrl Pts',(-2.47584495415716,-1.46155994553451,
0.000838156444187416));
#59159=CARTESIAN_POINT('Ctrl Pts',(-2.48615169920302,-1.46254670497474,
0.190967096739963));
#59160=CARTESIAN_POINT('Ctrl Pts',(-2.49645844424887,-1.42812769578372,
0.38075266272535));
#59161=CARTESIAN_POINT('Ctrl Pts',(-2.50676518929473,-1.35664666452184,
0.555366262980827));
#59162=CARTESIAN_POINT('Ctrl Pts',(-2.53327973170041,-1.1727586546639,1.00456721711192));
#59163=CARTESIAN_POINT('Ctrl Pts',(-2.5597942741061,-0.743595061800773,
1.35336046190046));
#59164=CARTESIAN_POINT('Ctrl Pts',(-2.58630881651179,-0.266287832759806,
1.44153135537509));
#59165=CARTESIAN_POINT('Ctrl Pts',(-2.61282335891747,0.211019396281106,
1.5297022488497));
#59166=CARTESIAN_POINT('Ctrl Pts',(-2.63933790132316,0.736470261499846,
1.35725079101045));
#59167=CARTESIAN_POINT('Ctrl Pts',(-2.66585244372885,1.06870423335387,1.00339081121795));
#59168=CARTESIAN_POINT('Ctrl Pts',(-2.69236698613453,1.40093820520792,0.649530831425438));
#59169=CARTESIAN_POINT('Ctrl Pts',(-2.71888152854022,1.53995528369721,0.114262329679646));
#59170=CARTESIAN_POINT('Ctrl Pts',(-2.7453960709459,1.42189938274908,-0.35654453263864));
#59171=CARTESIAN_POINT('Ctrl Pts',(-2.77191061335159,1.30384348180092,-0.82735139495698));
#59172=CARTESIAN_POINT('Ctrl Pts',(-2.79842515575728,0.928714601415265,
-1.2336966178478));
#59173=CARTESIAN_POINT('Ctrl Pts',(-2.82493969816297,0.468824390893206,
-1.38892964145764));
#59174=CARTESIAN_POINT('Ctrl Pts',(-2.85145424056866,0.00893418037119946,
-1.54416266506747));
#59175=CARTESIAN_POINT('Ctrl Pts',(-2.87796878297434,-0.535717360287188,
-1.44828348939639));
#59176=CARTESIAN_POINT('Ctrl Pts',(-2.90448332538003,-0.914950065880211,
-1.14533324205864));
#59177=CARTESIAN_POINT('Ctrl Pts',(-2.92827053497241,-1.2551742234086,-0.873544993963514));
#59178=CARTESIAN_POINT('Ctrl Pts',(-2.95205774456478,-1.46225987355395,
-0.435094144278848));
#59179=CARTESIAN_POINT('Ctrl Pts',(-2.97584495415716,-1.46529038421007,
0.000858184953542052));
#59180=CARTESIAN_POINT('Ctrl Pts',(-3.04715504584288,-1.46493873305747,
0.00104194039951338));
#59181=CARTESIAN_POINT('Ctrl Pts',(-3.02414881976534,-1.46154106858268,
-0.420862354190906));
#59182=CARTESIAN_POINT('Ctrl Pts',(-3.00114259368781,-1.2694430210697,-0.845464750254815));
#59183=CARTESIAN_POINT('Ctrl Pts',(-2.97813636761028,-0.948269993348118,
-1.11790243046778));
#59184=CARTESIAN_POINT('Ctrl Pts',(-2.95162182520459,-0.578119937689832,
-1.4318852801785));
#59185=CARTESIAN_POINT('Ctrl Pts',(-2.9251072827989,-0.036526954732755,
-1.5437564249336));
#59186=CARTESIAN_POINT('Ctrl Pts',(-2.89859274039322,0.427733707804147,
-1.40212898819544));
#59187=CARTESIAN_POINT('Ctrl Pts',(-2.87207819798753,0.89199437034105,-1.26050155145728));
#59188=CARTESIAN_POINT('Ctrl Pts',(-2.84556365558184,1.27892271245777,-0.865375533225857));
#59189=CARTESIAN_POINT('Ctrl Pts',(-2.81904911317616,1.41078712169197,-0.398248065403867));
#59190=CARTESIAN_POINT('Ctrl Pts',(-2.79253457077047,1.54265153092617,0.068879402418151));
#59191=CARTESIAN_POINT('Ctrl Pts',(-2.76602002836478,1.41945200727779,0.608008319830747));
#59192=CARTESIAN_POINT('Ctrl Pts',(-2.7395054859591,1.09777900331638,0.971495282648806));
#59193=CARTESIAN_POINT('Ctrl Pts',(-2.71299094355341,0.776105999355004,
1.33498224546682));
#59194=CARTESIAN_POINT('Ctrl Pts',(-2.68647640114773,0.255959515080636,
1.52282725369035));
#59195=CARTESIAN_POINT('Ctrl Pts',(-2.65996185874204,-0.223736433597789,
1.44874560658848));
#59196=CARTESIAN_POINT('Ctrl Pts',(-2.63344731633635,-0.703432382276295,
1.37466395948659));
#59197=CARTESIAN_POINT('Ctrl Pts',(-2.60693277393067,-1.14267779535884,
1.03865565705922));
#59198=CARTESIAN_POINT('Ctrl Pts',(-2.58041823152498,-1.33970974406678,
0.59506270760455));
#59199=CARTESIAN_POINT('Ctrl Pts',(-2.56933050296428,-1.42210365196957,
0.409563062174604));
#59200=CARTESIAN_POINT('Ctrl Pts',(-2.55824277440358,-1.46214153647667,
0.205250020725279));
#59201=CARTESIAN_POINT('Ctrl Pts',(-2.54715504584288,-1.46134104288809,
0.000637616632206692));
#59202=CARTESIAN_POINT('Origin',(-17.3,0.,0.));
#59203=CARTESIAN_POINT('',(-1.97584495415716,-1.46221851409551,-0.00117471765568408));
#59204=CARTESIAN_POINT('',(-2.04715504584289,-1.46259601224811,-0.00127585584471357));
#59205=CARTESIAN_POINT('',(-17.3,-1.4635,-1.79227059055215E-16));
#59206=CARTESIAN_POINT('Ctrl Pts',(-1.97584495415716,-1.46221851409551,
-0.00117471765568408));
#59207=CARTESIAN_POINT('Ctrl Pts',(-1.99373111143557,-1.45974902951182,
0.328398847612615));
#59208=CARTESIAN_POINT('Ctrl Pts',(-2.01161726871397,-1.3495306267837,0.659468494052664));
#59209=CARTESIAN_POINT('Ctrl Pts',(-2.02950342599237,-1.14510209648561,
0.91523933882229));
#59210=CARTESIAN_POINT('Ctrl Pts',(-2.05601796839806,-0.842056067584495,
1.29439550994524));
#59211=CARTESIAN_POINT('Ctrl Pts',(-2.08253251080374,-0.331980757629562,
1.50808054568027));
#59212=CARTESIAN_POINT('Ctrl Pts',(-2.10904705320943,0.150825910019734,
1.45814039194405));
#59213=CARTESIAN_POINT('Ctrl Pts',(-2.13556159561512,0.633632577669058,
1.40820023820784));
#59214=CARTESIAN_POINT('Ctrl Pts',(-2.16207613802081,1.08917060301271,1.09463489500037));
#59215=CARTESIAN_POINT('Ctrl Pts',(-2.1885906804265,1.3081932105853,0.661477424025895));
#59216=CARTESIAN_POINT('Ctrl Pts',(-2.21510522283218,1.52721581815786,0.228319953051469));
#59217=CARTESIAN_POINT('Ctrl Pts',(-2.24161976523787,1.50972300795938,-0.324429645689988));
#59218=CARTESIAN_POINT('Ctrl Pts',(-2.26813430764355,1.26374992525915,-0.742871445701784));
#59219=CARTESIAN_POINT('Ctrl Pts',(-2.29464885004924,1.01777684255889,-1.16131324571363));
#59220=CARTESIAN_POINT('Ctrl Pts',(-2.32116339245492,0.543323487356945,
-1.4454472469958));
#59221=CARTESIAN_POINT('Ctrl Pts',(-2.34767793486061,0.0583251997158712,
-1.46475937594014));
#59222=CARTESIAN_POINT('Ctrl Pts',(-2.3741924772663,-0.426673087925147,
-1.48407150488447));
#59223=CARTESIAN_POINT('Ctrl Pts',(-2.40070701967198,-0.922216308005284,
-1.23856176149093));
#59224=CARTESIAN_POINT('Ctrl Pts',(-2.42722156207767,-1.20068170461892,
-0.841002558057389));
#59225=CARTESIAN_POINT('Ctrl Pts',(-2.4434293594375,-1.37090190495213,-0.597982749938599));
#59226=CARTESIAN_POINT('Ctrl Pts',(-2.45963715679733,-1.46000822411528,
-0.298147733169239));
#59227=CARTESIAN_POINT('Ctrl Pts',(-2.47584495415716,-1.46155994553451,
0.000838156444187416));
#59228=CARTESIAN_POINT('Ctrl Pts',(-2.54715504584288,-1.46134104288809,
0.000637616632206692));
#59229=CARTESIAN_POINT('Ctrl Pts',(-2.53172823199789,-1.46022728315745,
-0.284048056455808));
#59230=CARTESIAN_POINT('Ctrl Pts',(-2.5163014181529,-1.38005734937291,-0.569313244852052));
#59231=CARTESIAN_POINT('Ctrl Pts',(-2.50087460430791,-1.22491886837172,
-0.805292239031575));
#59232=CARTESIAN_POINT('Ctrl Pts',(-2.47436006190223,-0.958277559635383,
-1.21087663973118));
#59233=CARTESIAN_POINT('Ctrl Pts',(-2.44784551949654,-0.47017645782932,
-1.47086784464852));
#59234=CARTESIAN_POINT('Ctrl Pts',(-2.42133097709086,0.0151801427879505,
-1.46584152880958));
#59235=CARTESIAN_POINT('Ctrl Pts',(-2.39481643468517,0.500536743405221,
-1.46081521297064));
#59236=CARTESIAN_POINT('Ctrl Pts',(-2.36830189227948,0.983148842833728,
-1.19077137637541));
#59237=CARTESIAN_POINT('Ctrl Pts',(-2.3417873498738,1.2413334644567,-0.779751918463746));
#59238=CARTESIAN_POINT('Ctrl Pts',(-2.31527280746811,1.49951808607968,-0.368732460552062));
#59239=CARTESIAN_POINT('Ctrl Pts',(-2.28875826506243,1.53327522989713,0.183262618676012));
#59240=CARTESIAN_POINT('Ctrl Pts',(-2.26224372265674,1.32709889398495,0.622679973952962));
#59241=CARTESIAN_POINT('Ctrl Pts',(-2.23572918025105,1.12092255807279,1.06209732922989));
#59242=CARTESIAN_POINT('Ctrl Pts',(-2.20921463784537,0.674812742430977,
1.38893696055564));
#59243=CARTESIAN_POINT('Ctrl Pts',(-2.18270009543968,0.193685469657787,
1.45306839587207));
#59244=CARTESIAN_POINT('Ctrl Pts',(-2.156185553034,-0.28744180311543,1.51719983118851));
#59245=CARTESIAN_POINT('Ctrl Pts',(-2.12967101062831,-0.803586533020062,
1.31862307049558));
#59246=CARTESIAN_POINT('Ctrl Pts',(-2.10315646822262,-1.11766286959625,
0.948552336073166));
#59247=CARTESIAN_POINT('Ctrl Pts',(-2.08448932742938,-1.33878330626034,
0.688009936463793));
#59248=CARTESIAN_POINT('Ctrl Pts',(-2.06582218663613,-1.45974572493651,
0.342464156450928));
#59249=CARTESIAN_POINT('Ctrl Pts',(-2.04715504584289,-1.46259601224811,
-0.00127585584471357));
#59250=CARTESIAN_POINT('Origin',(-17.3,0.,0.));
#59251=CARTESIAN_POINT('',(-1.47584495415717,-1.46581513481851,-0.000356810360598175));
#59252=CARTESIAN_POINT('',(-1.54715504584288,-1.46591291273786,-9.23842247488784E-5));
#59253=CARTESIAN_POINT('',(-17.3,-1.4635,-1.79227059055215E-16));
#59254=CARTESIAN_POINT('Ctrl Pts',(-1.47584495415717,-1.46581513481851,
-0.000356810360598175));
#59255=CARTESIAN_POINT('Ctrl Pts',(-1.50131052366812,-1.46429011704063,
0.465912677307333));
#59256=CARTESIAN_POINT('Ctrl Pts',(-1.52677609317907,-1.22259768826152,
0.933541855018993));
#59257=CARTESIAN_POINT('Ctrl Pts',(-1.55224166269002,-0.840699239369595,
1.20089411587294));
#59258=CARTESIAN_POINT('Ctrl Pts',(-1.5787562050957,-0.443069702223083,
1.47925910019502));
#59259=CARTESIAN_POINT('Ctrl Pts',(-1.60527074750139,0.106554431146246,
1.54050780744101));
#59260=CARTESIAN_POINT('Ctrl Pts',(-1.63178528990707,0.555708917962632,
1.35650633016601));
#59261=CARTESIAN_POINT('Ctrl Pts',(-1.65829983231276,1.00486340477899,1.17250485289101));
#59262=CARTESIAN_POINT('Ctrl Pts',(-1.68481437471845,1.35354824504234,0.743253191095036));
#59263=CARTESIAN_POINT('Ctrl Pts',(-1.71132891712413,1.44159857415386,0.265923710694476));
#59264=CARTESIAN_POINT('Ctrl Pts',(-1.73784345952982,1.52964890326539,-0.211405769706084));
#59265=CARTESIAN_POINT('Ctrl Pts',(-1.7643580019355,1.35706472122508,-0.736813068711231));
#59266=CARTESIAN_POINT('Ctrl Pts',(-1.79087254434119,1.00312083194446,-1.06895765030956));
#59267=CARTESIAN_POINT('Ctrl Pts',(-1.81738708674688,0.649176942663795,
-1.40110223190793));
#59268=CARTESIAN_POINT('Ctrl Pts',(-1.84390162915257,0.11387334614275,-1.53998409609945));
#59269=CARTESIAN_POINT('Ctrl Pts',(-1.87041617155826,-0.356903680568287,
-1.4218092757004));
#59270=CARTESIAN_POINT('Ctrl Pts',(-1.89693071396394,-0.827680707279217,
-1.30363445530139));
#59271=CARTESIAN_POINT('Ctrl Pts',(-1.92344525636963,-1.2339311641802,-0.92840295031193));
#59272=CARTESIAN_POINT('Ctrl Pts',(-1.94995979877531,-1.38904801870709,
-0.468473544561806));
#59273=CARTESIAN_POINT('Ctrl Pts',(-1.95858818390259,-1.43952627852816,
-0.318802922928734));
#59274=CARTESIAN_POINT('Ctrl Pts',(-1.96721656902988,-1.46340980765971,
-0.160162900787707));
#59275=CARTESIAN_POINT('Ctrl Pts',(-1.97584495415716,-1.46221851409551,
-0.00117471765568408));
#59276=CARTESIAN_POINT('Ctrl Pts',(-2.04715504584289,-1.46259601224811,
-0.00127585584471357));
#59277=CARTESIAN_POINT('Ctrl Pts',(-2.03930764423044,-1.46379423266615,
-0.145779288728592));
#59278=CARTESIAN_POINT('Ctrl Pts',(-2.031460242618,-1.44411917499234,-0.289963598662981));
#59279=CARTESIAN_POINT('Ctrl Pts',(-2.02361284100556,-1.40223698554355,
-0.427379528058853));
#59280=CARTESIAN_POINT('Ctrl Pts',(-1.99709829859987,-1.26072682166689,
-0.891675949616525));
#59281=CARTESIAN_POINT('Ctrl Pts',(-1.97058375619419,-0.865698550665846,
-1.27870408457996));
#59282=CARTESIAN_POINT('Ctrl Pts',(-1.9440692137885,-0.398604405731616,
-1.41068648231822));
#59283=CARTESIAN_POINT('Ctrl Pts',(-1.91755467138282,0.0684897392025882,
-1.54266888005647));
#59284=CARTESIAN_POINT('Ctrl Pts',(-1.89104012897713,0.607649758069999,
-1.41960554056952));
#59285=CARTESIAN_POINT('Ctrl Pts',(-1.86452558657144,0.971217961473909,
-1.09802436035208));
#59286=CARTESIAN_POINT('Ctrl Pts',(-1.83801104416575,1.33478616487784,-0.776443180134614));
#59287=CARTESIAN_POINT('Ctrl Pts',(-1.81149650176006,1.52276255281831,-0.256344159186644));
#59288=CARTESIAN_POINT('Ctrl Pts',(-1.78498195935438,1.44880207486443,0.22337048598841));
#59289=CARTESIAN_POINT('Ctrl Pts',(-1.75846741694869,1.37484159691055,0.703085131163465));
#59290=CARTESIAN_POINT('Ctrl Pts',(-1.73195287454301,1.03894425306233,1.14241540056557));
#59291=CARTESIAN_POINT('Ctrl Pts',(-1.70543833213732,0.595401087256812,
1.33955939206657));
#59292=CARTESIAN_POINT('Ctrl Pts',(-1.67892378973163,0.151857921451289,
1.53670338356758));
#59293=CARTESIAN_POINT('Ctrl Pts',(-1.65240924732594,-0.399331066311595,
1.49166109716746));
#59294=CARTESIAN_POINT('Ctrl Pts',(-1.62589470492026,-0.804982807087559,
1.22512224200014));
#59295=CARTESIAN_POINT('Ctrl Pts',(-1.59964815189446,-1.20653452015798,
0.961277364402592));
#59296=CARTESIAN_POINT('Ctrl Pts',(-1.57340159886867,-1.46547608429131,
0.480390737597124));
#59297=CARTESIAN_POINT('Ctrl Pts',(-1.54715504584288,-1.46591291273786,
-9.23842247488784E-5));
#59298=CARTESIAN_POINT('Origin',(-17.3,0.,0.));
#59299=CARTESIAN_POINT('',(-0.975844954157165,-1.4632995300711,0.00135195255092181));
#59300=CARTESIAN_POINT('',(-1.04715504584289,-1.46287428079508,0.00132175412439906));
#59301=CARTESIAN_POINT('',(-17.3,-1.4635,-1.79227059055215E-16));
#59302=CARTESIAN_POINT('Ctrl Pts',(-0.975844954157165,-1.4632995300711,
0.00135195255092181));
#59303=CARTESIAN_POINT('Ctrl Pts',(-0.982375393494976,-1.4643975106379,
0.121457105082137));
#59304=CARTESIAN_POINT('Ctrl Pts',(-0.988905832832787,-1.4508550804661,
0.241318079550921));
#59305=CARTESIAN_POINT('Ctrl Pts',(-0.995436272170598,-1.42171992921314,
0.357261097571569));
#59306=CARTESIAN_POINT('Ctrl Pts',(-1.02195081457628,-1.30342693797136,
0.828006771626319));
#59307=CARTESIAN_POINT('Ctrl Pts',(-1.04846535698197,-0.928091181909397,
1.23416574829629));
#59308=CARTESIAN_POINT('Ctrl Pts',(-1.07497989938765,-0.468122219837597,
1.38916720728875));
#59309=CARTESIAN_POINT('Ctrl Pts',(-1.10149444179334,-0.00815325776574491,
1.54416866628123));
#59310=CARTESIAN_POINT('Ctrl Pts',(-1.12800898419903,0.536448910315971,
1.44801260759614));
#59311=CARTESIAN_POINT('Ctrl Pts',(-1.15452352660471,0.915528317071882,
1.14487040370153));
#59312=CARTESIAN_POINT('Ctrl Pts',(-1.1810380690104,1.29460772382779,0.841728199806911));
#59313=CARTESIAN_POINT('Ctrl Pts',(-1.20755261141609,1.5081643692579,0.331599850702771));
#59314=CARTESIAN_POINT('Ctrl Pts',(-1.23406715382178,1.45810237232685,-0.15119396951098));
#59315=CARTESIAN_POINT('Ctrl Pts',(-1.26058169622746,1.4080403753958,-0.633987789724676));
#59316=CARTESIAN_POINT('Ctrl Pts',(-1.28709623863315,1.09435973610365,-1.08944708104799));
#59317=CARTESIAN_POINT('Ctrl Pts',(-1.31361078103884,0.661146898645242,
-1.30836038425853));
#59318=CARTESIAN_POINT('Ctrl Pts',(-1.34012532344452,0.227934061186759,
-1.52727368746911));
#59319=CARTESIAN_POINT('Ctrl Pts',(-1.36663986585021,-0.324810974438033,
-1.50964100256683));
#59320=CARTESIAN_POINT('Ctrl Pts',(-1.3931544082559,-0.743190600300525,
-1.26356217237913));
#59321=CARTESIAN_POINT('Ctrl Pts',(-1.41966895066158,-1.16157022616292,
-1.01748334219149));
#59322=CARTESIAN_POINT('Ctrl Pts',(-1.44618349306727,-1.44558444226309,
-0.542958366718559));
#59323=CARTESIAN_POINT('Ctrl Pts',(-1.47269803547295,-1.46477407985142,
-0.0579552482830333));
#59324=CARTESIAN_POINT('Ctrl Pts',(-1.47374700836769,-1.4655332635998,-0.0387674713522122));
#59325=CARTESIAN_POINT('Ctrl Pts',(-1.47479598126243,-1.46587795306069,
-0.0195632943937738));
#59326=CARTESIAN_POINT('Ctrl Pts',(-1.47584495415717,-1.46581513481851,
-0.000356810360598175));
#59327=CARTESIAN_POINT('Ctrl Pts',(-1.54715504584288,-1.46591291273786,
-9.23842247488784E-5));
#59328=CARTESIAN_POINT('Ctrl Pts',(-1.54688705646299,-1.46591737295725,
-0.0049983379223528));
#59329=CARTESIAN_POINT('Ctrl Pts',(-1.54661906708309,-1.46589488315485,
-0.00990424955315265));
#59330=CARTESIAN_POINT('Ctrl Pts',(-1.5463510777032,-1.46584531996366,-0.0148098876518666));
#59331=CARTESIAN_POINT('Ctrl Pts',(-1.51983653529752,-1.46094159827471,
-0.500167738202059));
#59332=CARTESIAN_POINT('Ctrl Pts',(-1.49332199289183,-1.19101966110771,
-0.982848015367965));
#59333=CARTESIAN_POINT('Ctrl Pts',(-1.46680745048614,-0.780065437455982,
-1.24113645682674));
#59334=CARTESIAN_POINT('Ctrl Pts',(-1.44029290808046,-0.369111213804236,
-1.49942489828552));
#59335=CARTESIAN_POINT('Ctrl Pts',(-1.41377836567477,0.182875296332269,
-1.53332150403716));
#59336=CARTESIAN_POINT('Ctrl Pts',(-1.38726382326908,0.622344727124077,
-1.32725615280541));
#59337=CARTESIAN_POINT('Ctrl Pts',(-1.36074928086339,1.06181415791586,-1.12119080157368));
#59338=CARTESIAN_POINT('Ctrl Pts',(-1.33423473845771,1.38876650936299,-0.675163493358575));
#59339=CARTESIAN_POINT('Ctrl Pts',(-1.30772019605202,1.45301945035473,-0.194052463649122));
#59340=CARTESIAN_POINT('Ctrl Pts',(-1.28120565364634,1.51727239134647,0.287058566060359));
#59341=CARTESIAN_POINT('Ctrl Pts',(-1.25469111124065,1.31882592188284,0.803253317264156));
#59342=CARTESIAN_POINT('Ctrl Pts',(-1.22817656883496,0.948834572316278,
1.1174231749986));
#59343=CARTESIAN_POINT('Ctrl Pts',(-1.20166202642928,0.578843222749738,
1.43159303273303));
#59344=CARTESIAN_POINT('Ctrl Pts',(-1.17514748402359,0.0373069930802804,
1.54373799699806));
#59345=CARTESIAN_POINT('Ctrl Pts',(-1.1486329416179,-0.427025233810471,
1.40234501189082));
#59346=CARTESIAN_POINT('Ctrl Pts',(-1.12211839921221,-0.89135746070125,
1.26095202678357));
#59347=CARTESIAN_POINT('Ctrl Pts',(-1.09560385680653,-1.27848568481334,
0.866021092304002));
#59348=CARTESIAN_POINT('Ctrl Pts',(-1.06908931440084,-1.41058591850998,
0.398960495781479));
#59349=CARTESIAN_POINT('Ctrl Pts',(-1.06177789154819,-1.44701274619994,
0.270167870710371));
#59350=CARTESIAN_POINT('Ctrl Pts',(-1.05446646869554,-1.46404753918599,
0.135890589201196));
#59351=CARTESIAN_POINT('Ctrl Pts',(-1.04715504584289,-1.46287428079508,
0.00132175412439906));
#59352=CARTESIAN_POINT('Origin',(-17.3,0.,0.));
#59353=CARTESIAN_POINT('',(-0.47584495415717,-1.4610556053668,-0.000134560743048767));
#59354=CARTESIAN_POINT('',(-0.547155045842891,-1.46121426462895,-0.000470658046818673));
#59355=CARTESIAN_POINT('',(-17.3,-1.4635,-1.79227059055215E-16));
#59356=CARTESIAN_POINT('Ctrl Pts',(-0.47584495415717,-1.4610556053668,-0.000134560743048767));
#59357=CARTESIAN_POINT('Ctrl Pts',(-0.489954805727525,-1.46067797988535,
0.260281498090399));
#59358=CARTESIAN_POINT('Ctrl Pts',(-0.504064657297881,-1.39440376469311,
0.520857511314463));
#59359=CARTESIAN_POINT('Ctrl Pts',(-0.518174508868237,-1.26341397229026,
0.743430076950993));
#59360=CARTESIAN_POINT('Ctrl Pts',(-0.544689051273926,-1.01726436624661,
1.16167754755594));
#59361=CARTESIAN_POINT('Ctrl Pts',(-0.571203593679616,-0.542590552750608,
1.44572691447813));
#59362=CARTESIAN_POINT('Ctrl Pts',(-0.597718136085304,-0.0575643430575941,
1.46483074051128));
#59363=CARTESIAN_POINT('Ctrl Pts',(-0.624232678490992,0.42746186663542,
1.48393456654444));
#59364=CARTESIAN_POINT('Ctrl Pts',(-0.650747220896674,0.922840472525375,
1.23809285168862));
#59365=CARTESIAN_POINT('Ctrl Pts',(-0.677261763302362,1.20109540462185,
0.840373701153215));
#59366=CARTESIAN_POINT('Ctrl Pts',(-0.703776305708048,1.47935033671831,
0.442654550617832));
#59367=CARTESIAN_POINT('Ctrl Pts',(-0.730290848113738,1.54048159502121,
-0.106942035597157));
#59368=CARTESIAN_POINT('Ctrl Pts',(-0.756805390519424,1.35637172984761,
-0.556039857846719));
#59369=CARTESIAN_POINT('Ctrl Pts',(-0.783319932925108,1.17226186467403,
-1.00513768009626));
#59370=CARTESIAN_POINT('Ctrl Pts',(-0.809834475330794,0.742910876024013,
-1.35373673838046));
#59371=CARTESIAN_POINT('Ctrl Pts',(-0.836349017736478,0.265556504920355,
-1.44167185463886));
#59372=CARTESIAN_POINT('Ctrl Pts',(-0.862863560142165,-0.211797866183358,
-1.52960697089727));
#59373=CARTESIAN_POINT('Ctrl Pts',(-0.889378102547852,-0.737155619740722,
-1.35687814512982));
#59374=CARTESIAN_POINT('Ctrl Pts',(-0.91589264495354,-1.06920938330862,
-1.00284754652629));
#59375=CARTESIAN_POINT('Ctrl Pts',(-0.935876748021415,-1.31947946278746,
-0.736013449847445));
#59376=CARTESIAN_POINT('Ctrl Pts',(-0.95586085108929,-1.45993954834883,
-0.366187446103257));
#59377=CARTESIAN_POINT('Ctrl Pts',(-0.975844954157165,-1.4632995300711,
0.00135195255092181));
#59378=CARTESIAN_POINT('Ctrl Pts',(-1.04715504584289,-1.46287428079508,
0.00132175412439906));
#59379=CARTESIAN_POINT('Ctrl Pts',(-1.02795192628985,-1.45979277099851,
-0.352117170168635));
#59380=CARTESIAN_POINT('Ctrl Pts',(-1.00874880673681,-1.33110732839389,
-0.707567307740881));
#59381=CARTESIAN_POINT('Ctrl Pts',(-0.989545687183776,-1.09826933307926,
-0.970940151577963));
#59382=CARTESIAN_POINT('Ctrl Pts',(-0.963031144778092,-0.776780270670734,
-1.33458994384934));
#59383=CARTESIAN_POINT('Ctrl Pts',(-0.936516602372409,-0.256729902572511,
-1.52269926982669));
#59384=CARTESIAN_POINT('Ctrl Pts',(-0.910002059966724,0.223003927681576,
-1.44885926067856));
#59385=CARTESIAN_POINT('Ctrl Pts',(-0.883487517561038,0.70273775793569,
-1.37501925153043));
#59386=CARTESIAN_POINT('Ctrl Pts',(-0.856972975155351,1.14215505034566,
-1.0392299072568));
#59387=CARTESIAN_POINT('Ctrl Pts',(-0.830458432749665,1.33941008664533,
-0.59573789159776));
#59388=CARTESIAN_POINT('Ctrl Pts',(-0.803943890343978,1.53666512294502,
-0.152245875938697));
#59389=CARTESIAN_POINT('Ctrl Pts',(-0.777429347938291,1.49175790313437,
0.398948811105779));
#59390=CARTESIAN_POINT('Ctrl Pts',(-0.750914805532604,1.22532338885631,
0.8046704059668));
#59391=CARTESIAN_POINT('Ctrl Pts',(-0.724400263126918,0.958888874578265,
1.2103920008278));
#59392=CARTESIAN_POINT('Ctrl Pts',(-0.697885720721231,0.470927065832829,
1.47064050350535));
#59393=CARTESIAN_POINT('Ctrl Pts',(-0.671371178315545,-0.0144355535737682,
1.4658545555427));
#59394=CARTESIAN_POINT('Ctrl Pts',(-0.64485663590986,-0.499798172980338,
1.46106860758005));
#59395=CARTESIAN_POINT('Ctrl Pts',(-0.618342093504176,-0.98256160304807,
1.19124820897721));
#59396=CARTESIAN_POINT('Ctrl Pts',(-0.591827551098492,-1.24094710973327,
0.780368395977307));
#59397=CARTESIAN_POINT('Ctrl Pts',(-0.576936716013292,-1.38605902264452,
0.549614138875445));
#59398=CARTESIAN_POINT('Ctrl Pts',(-0.562045880928091,-1.46040081110129,
0.274368907965358));
#59399=CARTESIAN_POINT('Ctrl Pts',(-0.547155045842891,-1.46121426462895,
-0.000470658046818673));
#59400=CARTESIAN_POINT('Origin',(-35.5608671147362,0.,0.));
#59401=CARTESIAN_POINT('',(-0.310867114736255,-1.17578287613307,-0.000108287608020487));
#59402=CARTESIAN_POINT('',(-0.212132885263923,-1.17696636327651,-4.59991182728825E-5));
#59403=CARTESIAN_POINT('',(-35.5608671147362,-1.17775,1.38253677383905E-12));
#59404=CARTESIAN_POINT('',(-0.2,-0.20806946958181,-1.15922480922725));
#59405=CARTESIAN_POINT('Ctrl Pts',(-0.310867114736255,-1.17578287613307,
-0.000108287608020629));
#59406=CARTESIAN_POINT('Ctrl Pts',(-0.298462423900919,-1.17605004458734,
-0.184351563818547));
#59407=CARTESIAN_POINT('Ctrl Pts',(-0.261506718988835,-1.05473749252561,
-0.732947532879346));
#59408=CARTESIAN_POINT('Ctrl Pts',(-0.224551014076752,-0.563910892482186,
-1.09543997095558));
#59409=CARTESIAN_POINT('Ctrl Pts',(-0.200000000000004,-0.207979487136961,
-1.16121778488277));
#59410=CARTESIAN_POINT('',(-0.2,-1.1640875192389,-0.178872328917063));
#59411=CARTESIAN_POINT('Origin',(-0.2,0.,0.));
#59412=CARTESIAN_POINT('Ctrl Pts',(-0.212132885263923,-1.17696636327651,
-4.59991182729606E-5));
#59413=CARTESIAN_POINT('Ctrl Pts',(-0.208088590175949,-1.17739142535704,
-0.059880676848224));
#59414=CARTESIAN_POINT('Ctrl Pts',(-0.204044295087974,-1.17317818858489,
-0.119710943859588));
#59415=CARTESIAN_POINT('Ctrl Pts',(-0.2,-1.1640875192389,-0.178872328917063));
#59416=CARTESIAN_POINT('Origin',(-35.5608671147362,0.,0.));
#59417=CARTESIAN_POINT('',(-0.81086711473626,-1.17758867204732,0.00108798231488299));
#59418=CARTESIAN_POINT('',(-0.712132885263918,-1.17591055699811,-0.000378761538900874));
#59419=CARTESIAN_POINT('',(-35.5608671147362,-1.17775,1.38253677383905E-12));
#59420=CARTESIAN_POINT('Ctrl Pts',(-0.81086711473626,-1.17758867204732,
0.00108798231488304));
#59421=CARTESIAN_POINT('Ctrl Pts',(-0.790883011668376,-1.17488473048725,
-0.294688940654132));
#59422=CARTESIAN_POINT('Ctrl Pts',(-0.744384366194804,-0.911876732317324,
-0.987178885589815));
#59423=CARTESIAN_POINT('Ctrl Pts',(-0.671371178315547,0.252336971202078,
-1.36995284217421));
#59424=CARTESIAN_POINT('Ctrl Pts',(-0.591827551098487,1.28889616535859,
-0.528348726914579));
#59425=CARTESIAN_POINT('Ctrl Pts',(-0.512283923881428,1.14131022863273,
0.798513000617958));
#59426=CARTESIAN_POINT('Ctrl Pts',(-0.432740296664372,-0.0546559205033708,
1.39203554179653));
#59427=CARTESIAN_POINT('Ctrl Pts',(-0.365601360282643,-1.02192204925182,
0.813214204481599));
#59428=CARTESIAN_POINT('Ctrl Pts',(-0.324976966306605,-1.17547898244608,
0.209461246584642));
#59429=CARTESIAN_POINT('Ctrl Pts',(-0.310867114736255,-1.17578287613307,
-0.000108287608020629));
#59430=CARTESIAN_POINT('Ctrl Pts',(-0.712132885263918,-1.17591055699811,
-0.000378761538900839));
#59431=CARTESIAN_POINT('Ctrl Pts',(-0.700509177943399,-1.17642155446286,
-0.173028232716761));
#59432=CARTESIAN_POINT('Ctrl Pts',(-0.662370928217192,-1.05979880462431,
-0.738851338425022));
#59433=CARTESIAN_POINT('Ctrl Pts',(-0.597718136085294,-0.184831240778329,
-1.38079239774389));
#59434=CARTESIAN_POINT('Ctrl Pts',(-0.518174508868238,1.06175884240671,
-0.901671642965467));
#59435=CARTESIAN_POINT('Ctrl Pts',(-0.438630881651178,1.33236304935347,
0.405021101276792));
#59436=CARTESIAN_POINT('Ctrl Pts',(-0.35908725443412,0.380047119706207,
1.34111457344272));
#59437=CARTESIAN_POINT('Ctrl Pts',(-0.283587922305033,-0.857321546120441,
1.05741628964119));
#59438=CARTESIAN_POINT('Ctrl Pts',(-0.234603132581635,-1.17460470324253,
0.332397597978653));
#59439=CARTESIAN_POINT('Ctrl Pts',(-0.212132885263923,-1.17696636327651,
-4.59991182729606E-5));
#59440=CARTESIAN_POINT('Origin',(-35.5608671147362,0.,0.));
#59441=CARTESIAN_POINT('',(-1.31086711473626,-1.17961310217458,-0.000287142740902327));
#59442=CARTESIAN_POINT('',(-1.21213288526391,-1.17724645316462,0.00106368016567451));
#59443=CARTESIAN_POINT('',(-35.5608671147362,-1.17775,1.38253677383905E-12));
#59444=CARTESIAN_POINT('Ctrl Pts',(-1.31086711473626,-1.17961310217458,
-0.000287142740902635));
#59445=CARTESIAN_POINT('Ctrl Pts',(-1.30981814184151,-1.17966365508524,
-0.0157435394407337));
#59446=CARTESIAN_POINT('Ctrl Pts',(-1.28225462654108,-1.17237480984895,
-0.421837399635015));
#59447=CARTESIAN_POINT('Ctrl Pts',(-1.22817656883496,-0.70621222470226,
-1.20069203698611));
#59448=CARTESIAN_POINT('Ctrl Pts',(-1.14863294161791,0.628250636330202,
-1.24326168777629));
#59449=CARTESIAN_POINT('Ctrl Pts',(-1.06908931440084,1.38555307485394,-0.143670610859339));
#59450=CARTESIAN_POINT('Ctrl Pts',(-0.989545687183782,0.869974654993682,
1.08790505669946));
#59451=CARTESIAN_POINT('Ctrl Pts',(-0.910002059966723,-0.444829315197323,
1.32004950107908));
#59452=CARTESIAN_POINT('Ctrl Pts',(-0.85044253581755,-1.12332549722415,
0.585834040613157));
#59453=CARTESIAN_POINT('Ctrl Pts',(-0.817397554074062,-1.17847227068925,
0.0977424704552608));
#59454=CARTESIAN_POINT('Ctrl Pts',(-0.81086711473626,-1.17758867204732,
0.00108798231488304));
#59455=CARTESIAN_POINT('Ctrl Pts',(-1.21213288526391,-1.17724645316462,
0.00106368016567453));
#59456=CARTESIAN_POINT('Ctrl Pts',(-1.19292976571085,-1.17476661157779,
-0.283365901718006));
#59457=CARTESIAN_POINT('Ctrl Pts',(-1.14721210375209,-0.928218299771867,
-0.964372467620693));
#59458=CARTESIAN_POINT('Ctrl Pts',(-1.07497989938766,0.211906852253127,
-1.3767713178738));
#59459=CARTESIAN_POINT('Ctrl Pts',(-0.995436272170595,1.27276858673064,
-0.566093011994411));
#59460=CARTESIAN_POINT('Ctrl Pts',(-0.915892644953538,1.16435148089155,
0.76462692514249));
#59461=CARTESIAN_POINT('Ctrl Pts',(-0.836349017736476,-0.0137086904440423,
1.39293100582981));
#59462=CARTESIAN_POINT('Ctrl Pts',(-0.768429097839939,-1.00890275949954,
0.836708964814963));
#59463=CARTESIAN_POINT('Ctrl Pts',(-0.727023720349086,-1.17525593117465,
0.220798074040274));
#59464=CARTESIAN_POINT('Ctrl Pts',(-0.712132885263918,-1.17591055699811,
-0.000378761538900839));
#59465=CARTESIAN_POINT('Origin',(-35.5608671147362,0.,0.));
#59466=CARTESIAN_POINT('',(-1.81086711473626,-1.17671872564126,-0.000945352728389693));
#59467=CARTESIAN_POINT('',(-1.71213288526391,-1.17969178884661,-7.43461005511814E-5));
#59468=CARTESIAN_POINT('',(-35.5608671147362,-1.17775,1.38253677383905E-12));
#59469=CARTESIAN_POINT('Ctrl Pts',(-1.81086711473626,-1.17671872564126,
-0.000945352728389855));
#59470=CARTESIAN_POINT('Ctrl Pts',(-1.80223872960897,-1.17767741781437,
-0.128890916571168));
#59471=CARTESIAN_POINT('Ctrl Pts',(-1.76709580207599,-1.09939444640547,
-0.648864838733412));
#59472=CARTESIAN_POINT('Ctrl Pts',(-1.70543833213732,-0.339145526056245,
-1.35106551741206));
#59473=CARTESIAN_POINT('Ctrl Pts',(-1.62589470492026,0.9532093987185,-1.01577043941121));
#59474=CARTESIAN_POINT('Ctrl Pts',(-1.5463510777032,1.36987018532208,0.25269238205091));
#59475=CARTESIAN_POINT('Ctrl Pts',(-1.46680745048614,0.528058971205146,
1.28901177668085));
#59476=CARTESIAN_POINT('Ctrl Pts',(-1.38831279616383,-0.78137054082941,
1.14309230194811));
#59477=CARTESIAN_POINT('Ctrl Pts',(-1.3363326842472,-1.17838584581094,0.374942709736548));
#59478=CARTESIAN_POINT('Ctrl Pts',(-1.31086711473626,-1.17961310217458,
-0.000287142740902635));
#59479=CARTESIAN_POINT('Ctrl Pts',(-1.71213288526391,-1.17969178884661,
-7.43461005513196E-5));
#59480=CARTESIAN_POINT('Ctrl Pts',(-1.71186489588399,-1.17969537820321,
-0.00402240689185183));
#59481=CARTESIAN_POINT('Ctrl Pts',(-1.68508236409837,-1.17788662184485,
-0.398583404005852));
#59482=CARTESIAN_POINT('Ctrl Pts',(-1.63178528990707,-0.74125237059894,
-1.17938226616436));
#59483=CARTESIAN_POINT('Ctrl Pts',(-1.55224166269001,0.591379222800219,
-1.26121703368907));
#59484=CARTESIAN_POINT('Ctrl Pts',(-1.47269803547295,1.3807228481852,-0.18439709057274));
#59485=CARTESIAN_POINT('Ctrl Pts',(-1.3931544082559,0.901624120319131,1.06182436804775));
#59486=CARTESIAN_POINT('Ctrl Pts',(-1.31361078103883,-0.405777918272958,
1.33256997446379));
#59487=CARTESIAN_POINT('Ctrl Pts',(-1.25327027337484,-1.11476781233784,
0.609290130836548));
#59488=CARTESIAN_POINT('Ctrl Pts',(-1.21944430811653,-1.17819063155183,
0.109357800774495));
#59489=CARTESIAN_POINT('Ctrl Pts',(-1.21213288526391,-1.17724645316462,
0.00106368016567453));
#59490=CARTESIAN_POINT('Origin',(-35.5608671147362,0.,0.));
#59491=CARTESIAN_POINT('',(-2.31086711473625,-1.17618874332304,0.000674505468416633));
#59492=CARTESIAN_POINT('',(-2.21213288526391,-1.1770225168604,-0.00102674357284102));
#59493=CARTESIAN_POINT('',(-35.5608671147362,-1.17775,1.38253677383905E-12));
#59494=CARTESIAN_POINT('Ctrl Pts',(-2.31086711473625,-1.17618874332304,
0.000674505468416693));
#59495=CARTESIAN_POINT('Ctrl Pts',(-2.29465931737641,-1.17493999723399,
-0.239934057218548));
#59496=CARTESIAN_POINT('Ctrl Pts',(-2.25193697761089,-0.985923408261569,
-0.875958445349159));
#59497=CARTESIAN_POINT('Ctrl Pts',(-2.18270009543968,0.0554231623812737,
-1.39187858910792));
#59498=CARTESIAN_POINT('Ctrl Pts',(-2.10315646822262,1.2008705947473,-0.7059090229788));
#59499=CARTESIAN_POINT('Ctrl Pts',(-2.02361284100557,1.24310255349976,0.628564854542996));
#59500=CARTESIAN_POINT('Ctrl Pts',(-1.9440692137885,0.143321393236571,1.38558893987825));
#59501=CARTESIAN_POINT('Ctrl Pts',(-1.87315397169873,-0.954546644775816,
0.925660834446937));
#59502=CARTESIAN_POINT('Ctrl Pts',(-1.82875327201465,-1.17473141066438,
0.264278607978505));
#59503=CARTESIAN_POINT('Ctrl Pts',(-1.81086711473626,-1.17671872564126,
-0.000945352728389855));
#59504=CARTESIAN_POINT('Ctrl Pts',(-2.21213288526391,-1.1770225168604,-0.00102674357284116));
#59505=CARTESIAN_POINT('Ctrl Pts',(-2.20428548365143,-1.17798678341153,
-0.117315720736906));
#59506=CARTESIAN_POINT('Ctrl Pts',(-2.16992353963328,-1.1086556584985,-0.625393540296511));
#59507=CARTESIAN_POINT('Ctrl Pts',(-2.10904705320943,-0.378771384950898,
-1.34049615412855));
#59508=CARTESIAN_POINT('Ctrl Pts',(-2.02950342599237,0.922893894627693,
-1.04339089670334));
#59509=CARTESIAN_POINT('Ctrl Pts',(-1.94995979877531,1.37671526305346,0.21225643214144));
#59510=CARTESIAN_POINT('Ctrl Pts',(-1.87041617155825,0.56577621956083,1.2729080716121));
#59511=CARTESIAN_POINT('Ctrl Pts',(-1.79114053372112,-0.76044669356272,
1.1645312469487));
#59512=CARTESIAN_POINT('Ctrl Pts',(-1.73837943828967,-1.17934025163867,
0.386593912679761));
#59513=CARTESIAN_POINT('Ctrl Pts',(-1.71213288526391,-1.17969178884661,
-7.43461005513196E-5));
#59514=CARTESIAN_POINT('Origin',(-35.5608671147362,0.,0.));
#59515=CARTESIAN_POINT('',(-2.81086711473625,-1.1791908097051,0.000690623389146067));
#59516=CARTESIAN_POINT('',(-2.71213288526391,-1.1760125816614,0.000513121278469739));
#59517=CARTESIAN_POINT('',(-35.5608671147362,-1.17775,1.38253677383905E-12));
#59518=CARTESIAN_POINT('Ctrl Pts',(-2.81086711473625,-1.1791908097051,0.000690623389146068));
#59519=CARTESIAN_POINT('Ctrl Pts',(-2.78707990514387,-1.17675200961973,
-0.350141529500257));
#59520=CARTESIAN_POINT('Ctrl Pts',(-2.7367781531458,-0.824340564457964,
-1.09628254632819));
#59521=CARTESIAN_POINT('Ctrl Pts',(-2.65996185874204,0.445497494323327,
-1.31982185031089));
#59522=CARTESIAN_POINT('Ctrl Pts',(-2.58041823152498,1.35115114421937,-0.338804249505638));
#59523=CARTESIAN_POINT('Ctrl Pts',(-2.50087460430792,1.01552962555056,0.953465947825067));
#59524=CARTESIAN_POINT('Ctrl Pts',(-2.42133097709085,-0.253038375497675,
1.36980630546842));
#59525=CARTESIAN_POINT('Ctrl Pts',(-2.35799514723364,-1.07802819152289,
0.699314027852116));
#59526=CARTESIAN_POINT('Ctrl Pts',(-2.3211738597821,-1.17698283688684,0.153680559061323));
#59527=CARTESIAN_POINT('Ctrl Pts',(-2.31086711473625,-1.17618874332304,
0.000674505468416693));
#59528=CARTESIAN_POINT('Ctrl Pts',(-2.71213288526391,-1.1760125816614,0.000513121278469617));
#59529=CARTESIAN_POINT('Ctrl Pts',(-2.69670607141889,-1.17511628475514,
-0.228587358038304));
#59530=CARTESIAN_POINT('Ctrl Pts',(-2.65476471516818,-0.999712830335691,
-0.852717840732116));
#59531=CARTESIAN_POINT('Ctrl Pts',(-2.58630881651179,0.0144248373372911,
-1.3929068982755));
#59532=CARTESIAN_POINT('Ctrl Pts',(-2.50676518929473,1.17956949077493,-0.740954465306795));
#59533=CARTESIAN_POINT('Ctrl Pts',(-2.42722156207767,1.26106756278956,0.591697815993344));
#59534=CARTESIAN_POINT('Ctrl Pts',(-2.34767793486061,0.184048426393107,
1.38076930720073));
#59535=CARTESIAN_POINT('Ctrl Pts',(-2.27598170925602,-0.939117811692954,
0.948652692700248));
#59536=CARTESIAN_POINT('Ctrl Pts',(-2.23080002605712,-1.17472875131086,
0.275597649649284));
#59537=CARTESIAN_POINT('Ctrl Pts',(-2.21213288526391,-1.1770225168604,-0.00102674357284116));
#59538=CARTESIAN_POINT('Origin',(-35.5608671147362,0.,0.));
#59539=CARTESIAN_POINT('',(-3.31086711473625,-1.17834427569628,-0.00101628109532418));
#59540=CARTESIAN_POINT('',(-3.21213288526392,-1.17890781883051,0.000838500381393336));
#59541=CARTESIAN_POINT('',(-35.5608671147362,-1.17775,1.38253677383905E-12));
#59542=CARTESIAN_POINT('Ctrl Pts',(-3.31086711473625,-1.17834427569628,
-0.00101628109532408));
#59543=CARTESIAN_POINT('Ctrl Pts',(-3.30601503531701,-1.17899808071603,
-0.072712416598091));
#59544=CARTESIAN_POINT('Ctrl Pts',(-3.27464841349208,-1.14034568634848,
-0.535493912102965));
#59545=CARTESIAN_POINT('Ctrl Pts',(-3.21676724926146,-0.527407731806677,
-1.28927840998041));
#59546=CARTESIAN_POINT('Ctrl Pts',(-3.13722362204439,0.799445675505238,
-1.14073850900496));
#59547=CARTESIAN_POINT('Ctrl Pts',(-3.05767999482733,1.39186454536937,0.0557747376017607));
#59548=CARTESIAN_POINT('Ctrl Pts',(-2.97813636761027,0.705605670279753,
1.20104886331929));
#59549=CARTESIAN_POINT('Ctrl Pts',(-2.89859274039321,-0.62887883157946,
1.24294374337767));
#59550=CARTESIAN_POINT('Ctrl Pts',(-2.84283632276854,-1.15932309657661,
0.47191381349839));
#59551=CARTESIAN_POINT('Ctrl Pts',(-2.81359444754955,-1.17947043138465,
0.0409154357539586));
#59552=CARTESIAN_POINT('Ctrl Pts',(-2.81086711473625,-1.1791908097051,0.000690623389146068));
#59553=CARTESIAN_POINT('Ctrl Pts',(-3.21213288526392,-1.17890781883051,
0.000838500381393362));
#59554=CARTESIAN_POINT('Ctrl Pts',(-3.18912665918635,-1.17617355211756,
-0.338688512228519));
#59555=CARTESIAN_POINT('Ctrl Pts',(-3.13960589070309,-0.843417985641057,
-1.07419213998031));
#59556=CARTESIAN_POINT('Ctrl Pts',(-3.06357057981415,0.406451325412254,
-1.33236444837786));
#59557=CARTESIAN_POINT('Ctrl Pts',(-2.98402695259708,1.34059178648789,-0.378432775049564));
#59558=CARTESIAN_POINT('Ctrl Pts',(-2.90448332538003,1.04315774690456,0.923157417945318));
#59559=CARTESIAN_POINT('Ctrl Pts',(-2.82493969816297,-0.212604170117943,
1.37666160332707));
#59560=CARTESIAN_POINT('Ctrl Pts',(-2.76082288479093,-1.06738626099137,
0.722781401633066));
#59561=CARTESIAN_POINT('Ctrl Pts',(-2.72322061382458,-1.17665677798775,
0.165174726280128));
#59562=CARTESIAN_POINT('Ctrl Pts',(-2.71213288526391,-1.1760125816614,0.000513121278469617));
#59563=CARTESIAN_POINT('Origin',(-35.5608671147362,0.,0.));
#59564=CARTESIAN_POINT('',(-3.81086711473625,-1.17583062577477,-0.000201975373600133));
#59565=CARTESIAN_POINT('',(-3.71213288526391,-1.17868089293979,-0.000925409118186643));
#59566=CARTESIAN_POINT('',(-35.5608671147362,-1.17775,1.38253677383905E-12));
#59567=CARTESIAN_POINT('Ctrl Pts',(-3.81086711473625,-1.17583062577477,
-0.000201975373600293));
#59568=CARTESIAN_POINT('Ctrl Pts',(-3.79843562308445,-1.17611245328021,
-0.184890850251831));
#59569=CARTESIAN_POINT('Ctrl Pts',(-3.75948958902697,-1.04800296746839,
-0.763124087068342));
#59570=CARTESIAN_POINT('Ctrl Pts',(-3.69402901256381,-0.142621398653279,
-1.3856611673339));
#59571=CARTESIAN_POINT('Ctrl Pts',(-3.61448538534675,1.08856544484988,-0.869150738531468));
#59572=CARTESIAN_POINT('Ctrl Pts',(-3.53494175812969,1.31970927922097,0.445830856210143));
#59573=CARTESIAN_POINT('Ctrl Pts',(-3.45539813091263,0.338462949072693,
1.35123668027329));
#59574=CARTESIAN_POINT('Ctrl Pts',(-3.38070658311482,-0.874900453070544,
1.03578123328469));
#59575=CARTESIAN_POINT('Ctrl Pts',(-3.33252957772269,-1.17542531542853,
0.319076352887373));
#59576=CARTESIAN_POINT('Ctrl Pts',(-3.31086711473625,-1.17834427569628,
-0.00101628109532408));
#59577=CARTESIAN_POINT('Ctrl Pts',(-3.71213288526391,-1.17868089293979,
-0.000925409118186669));
#59578=CARTESIAN_POINT('Ctrl Pts',(-3.70806178935948,-1.17919921175325,
-0.0610369679214061));
#59579=CARTESIAN_POINT('Ctrl Pts',(-3.67747615104936,-1.14764809049271,
-0.512101957958643));
#59580=CARTESIAN_POINT('Ctrl Pts',(-3.62037597033357,-0.565133098256669,
-1.27319373407426));
#59581=CARTESIAN_POINT('Ctrl Pts',(-3.5408323431165,0.765517983049464,-1.16377829540639));
#59582=CARTESIAN_POINT('Ctrl Pts',(-3.46128871589945,1.39290321025801,0.0147766736470439));
#59583=CARTESIAN_POINT('Ctrl Pts',(-3.38174508868238,0.740656492133029,
1.17975661214186));
#59584=CARTESIAN_POINT('Ctrl Pts',(-3.30220146146532,-0.592016332323219,
1.2609180645441));
#59585=CARTESIAN_POINT('Ctrl Pts',(-3.24566406032584,-1.15267305353486,
0.495261131766334));
#59586=CARTESIAN_POINT('Ctrl Pts',(-3.21564120159203,-1.17932477867964,
0.0526144047891755));
#59587=CARTESIAN_POINT('Ctrl Pts',(-3.21213288526392,-1.17890781883051,
0.000838500381393362));
#59588=CARTESIAN_POINT('Origin',(-35.5608671147362,0.,0.));
#59589=CARTESIAN_POINT('',(-4.31086711473625,-1.17760067476461,0.00108813158859299));
#59590=CARTESIAN_POINT('',(-4.21213288526391,-1.17591708598406,-0.000386845562409671));
#59591=CARTESIAN_POINT('',(-35.5608671147362,-1.17775,1.38253677383905E-12));
#59592=CARTESIAN_POINT('Ctrl Pts',(-4.31086711473625,-1.17760067476461,
0.00108813158859295));
#59593=CARTESIAN_POINT('Ctrl Pts',(-4.29085621085191,-1.1748911418629,-0.295079604829545));
#59594=CARTESIAN_POINT('Ctrl Pts',(-4.24433076456189,-0.911310100265462,
-0.987967233608653));
#59595=CARTESIAN_POINT('Ctrl Pts',(-4.17129077586617,0.253730346700255,
-1.36967829988445));
#59596=CARTESIAN_POINT('Ctrl Pts',(-4.09174714864911,1.28941158768824,-0.527082053902699));
#59597=CARTESIAN_POINT('Ctrl Pts',(-4.01220352143205,1.14053653923849,0.799733791128557));
#59598=CARTESIAN_POINT('Ctrl Pts',(-3.93265989421499,-0.0561263093121601,
1.39185041272904));
#59599=CARTESIAN_POINT('Ctrl Pts',(-3.86554775864972,-1.02226475660902,
0.812599585797225));
#59600=CARTESIAN_POINT('Ctrl Pts',(-3.82495016549014,-1.17551135668189,
0.209023342990697));
#59601=CARTESIAN_POINT('Ctrl Pts',(-3.81086711473625,-1.17583062577477,
-0.000201975373600293));
#59602=CARTESIAN_POINT('Ctrl Pts',(-4.21213288526391,-1.17591708598406,
-0.000386845562409758));
#59603=CARTESIAN_POINT('Ctrl Pts',(-4.20048237712693,-1.17642504647458,
-0.173441263805405));
#59604=CARTESIAN_POINT('Ctrl Pts',(-4.16231732658427,-1.05943529231218,
-0.739684098294869));
#59605=CARTESIAN_POINT('Ctrl Pts',(-4.09763773363592,-0.183350861145989,
-1.38086210931729));
#59606=CARTESIAN_POINT('Ctrl Pts',(-4.01809410641886,1.06250748323233,-0.900819377736997));
#59607=CARTESIAN_POINT('Ctrl Pts',(-3.9385504792018,1.3322617396258,0.406787856702201));
#59608=CARTESIAN_POINT('Ctrl Pts',(-3.85900685198474,0.378094140562434,
1.34068733271538));
#59609=CARTESIAN_POINT('Ctrl Pts',(-3.78353432067212,-0.856808474456836,
1.05816423047969));
#59610=CARTESIAN_POINT('Ctrl Pts',(-3.73457633176517,-1.17582346564415,
0.330462154765891));
#59611=CARTESIAN_POINT('Ctrl Pts',(-3.71213288526391,-1.17868089293979,
-0.000925409118186669));
#59612=CARTESIAN_POINT('Origin',(-35.5608671147362,0.,0.));
#59613=CARTESIAN_POINT('',(-4.81086711473624,-1.17960887409498,-0.000294231637304944));
#59614=CARTESIAN_POINT('',(-4.71213288526391,-1.17725794698973,0.0010650668865906));
#59615=CARTESIAN_POINT('',(-35.5608671147362,-1.17775,1.38253677383905E-12));
#59616=CARTESIAN_POINT('Ctrl Pts',(-4.81086711473624,-1.17960887409498,
-0.000294231637304968));
#59617=CARTESIAN_POINT('Ctrl Pts',(-4.80979134102505,-1.17966188515311,
-0.0161456849046697));
#59618=CARTESIAN_POINT('Ctrl Pts',(-4.78220102490816,-1.17217941461582,
-0.422635941839761));
#59619=CARTESIAN_POINT('Ctrl Pts',(-4.72809616638559,-0.704998830211815,
-1.20140517037799));
#59620=CARTESIAN_POINT('Ctrl Pts',(-4.64855253916853,0.629506665960787,
-1.24262588558339));
#59621=CARTESIAN_POINT('Ctrl Pts',(-4.56900891195147,1.38569714811699,-0.142271387535955));
#59622=CARTESIAN_POINT('Ctrl Pts',(-4.48946528473441,0.868875748162881,
1.08878495042198));
#59623=CARTESIAN_POINT('Ctrl Pts',(-4.40992165751735,-0.446164189652799,
1.31959662392811));
#59624=CARTESIAN_POINT('Ctrl Pts',(-4.35038893418463,-1.12361025449941,
0.585032693523647));
#59625=CARTESIAN_POINT('Ctrl Pts',(-4.3173707532576,-1.1784812857883,0.0973440483868324));
#59626=CARTESIAN_POINT('Ctrl Pts',(-4.31086711473625,-1.17760067476461,
0.00108813158859295));
#59627=CARTESIAN_POINT('Ctrl Pts',(-4.71213288526391,-1.17725794698973,
0.00106506688659067));
#59628=CARTESIAN_POINT('Ctrl Pts',(-4.69290296489438,-1.17476961504499,
-0.283754674824574));
#59629=CARTESIAN_POINT('Ctrl Pts',(-4.64715850211917,-0.927667344013,-0.965158191565359));
#59630=CARTESIAN_POINT('Ctrl Pts',(-4.57489949693828,0.213299609668962,
-1.37655402354802));
#59631=CARTESIAN_POINT('Ctrl Pts',(-4.49535586972123,1.27333644141125,-0.564811482005513));
#59632=CARTESIAN_POINT('Ctrl Pts',(-4.41581224250416,1.1635848947598,0.765811919414912));
#59633=CARTESIAN_POINT('Ctrl Pts',(-4.33626861528711,-0.0151285090234098,
1.39289943335687));
#59634=CARTESIAN_POINT('Ctrl Pts',(-4.26837549620702,-1.0093367994606,0.835934120578));
#59635=CARTESIAN_POINT('Ctrl Pts',(-4.22699691953262,-1.17526901621324,
0.220400674850707));
#59636=CARTESIAN_POINT('Ctrl Pts',(-4.21213288526391,-1.17591708598406,
-0.000386845562409758));
#59637=CARTESIAN_POINT('Origin',(-35.5608671147362,0.,0.));
#59638=CARTESIAN_POINT('',(-5.31086711473625,-1.17670885667242,-0.000942008607549203));
#59639=CARTESIAN_POINT('',(-5.21213288526391,-1.17969057793969,-8.17602703367948E-5));
#59640=CARTESIAN_POINT('',(-35.5608671147362,-1.17775,1.38253677383905E-12));
#59641=CARTESIAN_POINT('Ctrl Pts',(-5.31086711473625,-1.17670885667242,
-0.00094200860754937));
#59642=CARTESIAN_POINT('Ctrl Pts',(-5.3022119287925,-1.1776665848779,-0.129287698859234));
#59643=CARTESIAN_POINT('Ctrl Pts',(-5.26704220044306,-1.09906906098629,
-0.64967040496034));
#59644=CARTESIAN_POINT('Ctrl Pts',(-5.20535792968794,-0.337780283452094,
-1.35140749373458));
#59645=CARTESIAN_POINT('Ctrl Pts',(-5.12581430247089,0.954235217191234,
-1.01480682116499));
#59646=CARTESIAN_POINT('Ctrl Pts',(-5.04627067525382,1.36961416599977,0.254076308033152));
#59647=CARTESIAN_POINT('Ctrl Pts',(-4.96672704803676,0.526756342369506,
1.2895446831283));
#59648=CARTESIAN_POINT('Ctrl Pts',(-4.88825919453091,-0.782078078757634,
1.14235246346663));
#59649=CARTESIAN_POINT('Ctrl Pts',(-4.83630588343073,-1.17835532417835,
0.374544313813887));
#59650=CARTESIAN_POINT('Ctrl Pts',(-4.81086711473624,-1.17960887409498,
-0.000294231637304968));
#59651=CARTESIAN_POINT('Ctrl Pts',(-5.21213288526391,-1.17969057793969,
-8.17602703368457E-5));
#59652=CARTESIAN_POINT('Ctrl Pts',(-5.21183809506752,-1.17969490898888,
-0.0044246668410752));
#59653=CARTESIAN_POINT('Ctrl Pts',(-5.18502876246545,-1.17770326595971,
-0.399380889169589));
#59654=CARTESIAN_POINT('Ctrl Pts',(-5.13170488745769,-0.740060404085762,
-1.1801306290134));
#59655=CARTESIAN_POINT('Ctrl Pts',(-5.05216126024064,0.592653251738383,
-1.26061882678114));
#59656=CARTESIAN_POINT('Ctrl Pts',(-4.97261763302358,1.38090837817934,-0.183002060931766));
#59657=CARTESIAN_POINT('Ctrl Pts',(-4.89307400580652,0.900550968384048,
1.06273498887245));
#59658=CARTESIAN_POINT('Ctrl Pts',(-4.81353037858945,-0.407124362038215,
1.33215894587174));
#59659=CARTESIAN_POINT('Ctrl Pts',(-4.75321667174192,-1.1150679509245,0.608485500857434));
#59660=CARTESIAN_POINT('Ctrl Pts',(-4.71941750730007,-1.17820056959916,
0.108959646111801));
#59661=CARTESIAN_POINT('Ctrl Pts',(-4.71213288526391,-1.17725794698973,
0.00106506688659067));
#59662=CARTESIAN_POINT('Origin',(-35.5608671147362,0.,0.));
#59663=CARTESIAN_POINT('',(-5.81086711473624,-1.17619564711525,0.000679704233106716));
#59664=CARTESIAN_POINT('',(-5.71213288526391,-1.17701161509376,-0.0010244818722574));
#59665=CARTESIAN_POINT('',(-35.5608671147362,-1.17775,1.38253677383905E-12));
#59666=CARTESIAN_POINT('Ctrl Pts',(-5.81086711473624,-1.17619564711525,
0.000679704233106926));
#59667=CARTESIAN_POINT('Ctrl Pts',(-5.79463251655995,-1.17493475376919,
-0.240323181193375));
#59668=CARTESIAN_POINT('Ctrl Pts',(-5.75188337597797,-0.985441160761987,
-0.876754842997505));
#59669=CARTESIAN_POINT('Ctrl Pts',(-5.68261969299031,0.0568294419673366,
-1.39182188103819));
#59670=CARTESIAN_POINT('Ctrl Pts',(-5.60307606577323,1.20158320893396,-0.704695342697066));
#59671=CARTESIAN_POINT('Ctrl Pts',(-5.52353243855619,1.24246683775691,0.629820522915297));
#59672=CARTESIAN_POINT('Ctrl Pts',(-5.44398881133912,0.141921367341324,
1.38573304048903));
#59673=CARTESIAN_POINT('Ctrl Pts',(-5.37310037006582,-0.955066676424592,
0.924870157254964));
#59674=CARTESIAN_POINT('Ctrl Pts',(-5.32872647119819,-1.17473265309615,
0.26389013335399));
#59675=CARTESIAN_POINT('Ctrl Pts',(-5.31086711473625,-1.17670885667242,
-0.00094200860754937));
#59676=CARTESIAN_POINT('Ctrl Pts',(-5.71213288526391,-1.17701161509376,
-0.00102448187225759));
#59677=CARTESIAN_POINT('Ctrl Pts',(-5.70425868283498,-1.17797639299272,
-0.11771334838427));
#59678=CARTESIAN_POINT('Ctrl Pts',(-5.66986993800036,-1.10834486446487,
-0.626198871419997));
#59679=CARTESIAN_POINT('Ctrl Pts',(-5.60896665076006,-0.377416799240644,
-1.34087816854557));
#59680=CARTESIAN_POINT('Ctrl Pts',(-5.52942302354299,0.923947631924043,
-1.0424579016407));
#59681=CARTESIAN_POINT('Ctrl Pts',(-5.44987939632593,1.37650010191426,0.213647309042655));
#59682=CARTESIAN_POINT('Ctrl Pts',(-5.37033576910888,0.564489829717927,
1.27347906750608));
#59683=CARTESIAN_POINT('Ctrl Pts',(-5.2910869320882,-0.761174594165626,
1.16379940679085));
#59684=CARTESIAN_POINT('Ctrl Pts',(-5.23835263747321,-1.17930535808438,
0.386192734438204));
#59685=CARTESIAN_POINT('Ctrl Pts',(-5.21213288526391,-1.17969057793969,
-8.17602703368457E-5));
#59686=CARTESIAN_POINT('Origin',(-35.5608671147362,0.,0.));
#59687=CARTESIAN_POINT('',(-6.31086711473623,-1.17919972158703,0.000685029099866681));
#59688=CARTESIAN_POINT('',(-6.2121328852639,-1.17601780156144,0.000518948208354519));
#59689=CARTESIAN_POINT('',(-35.5608671147362,-1.17775,1.38253677383905E-12));
#59690=CARTESIAN_POINT('Ctrl Pts',(-6.31086711473623,-1.17919972158703,
0.000685029099866626));
#59691=CARTESIAN_POINT('Ctrl Pts',(-6.2870531043274,-1.1767738351423,-0.350535422240098));
#59692=CARTESIAN_POINT('Ctrl Pts',(-6.23672455151288,-0.823675614850911,
-1.09703732904515));
#59693=CARTESIAN_POINT('Ctrl Pts',(-6.15988145629266,0.446830771117568,
-1.31937106076852));
#59694=CARTESIAN_POINT('Ctrl Pts',(-6.08033782907561,1.35149277113303,-0.337438918303999));
#59695=CARTESIAN_POINT('Ctrl Pts',(-6.00079420185854,1.01456575685592,0.954491518572258));
#59696=CARTESIAN_POINT('Ctrl Pts',(-5.92125057464148,-0.254422253155312,
1.36954994473014));
#59697=CARTESIAN_POINT('Ctrl Pts',(-5.85794154560071,-1.07838539397748,
0.698508541121604));
#59698=CARTESIAN_POINT('Ctrl Pts',(-5.82114705896563,-1.1769940600563,0.153285650768014));
#59699=CARTESIAN_POINT('Ctrl Pts',(-5.81086711473624,-1.17619564711525,
0.000679704233106926));
#59700=CARTESIAN_POINT('Ctrl Pts',(-6.2121328852639,-1.17601780156144,0.000518948208354537));
#59701=CARTESIAN_POINT('Ctrl Pts',(-6.19667927060242,-1.17510951974459,
-0.22897699947036));
#59702=CARTESIAN_POINT('Ctrl Pts',(-6.15471111353526,-0.999248015551786,
-0.85351639676874));
#59703=CARTESIAN_POINT('Ctrl Pts',(-6.08622841406241,0.0158321768580185,
-1.39289161294304));
#59704=CARTESIAN_POINT('Ctrl Pts',(-6.00668478684535,1.18031752451205,-0.739762289225985));
#59705=CARTESIAN_POINT('Ctrl Pts',(-5.92714115962829,1.26046908724875,0.592971654736946));
#59706=CARTESIAN_POINT('Ctrl Pts',(-5.84759753241124,0.182653249041503,
1.38095455893587));
#59707=CARTESIAN_POINT('Ctrl Pts',(-5.77592810762311,-0.939656131499914,
0.947865308820643));
#59708=CARTESIAN_POINT('Ctrl Pts',(-5.73077322524066,-1.17472772816033,
0.275209227245314));
#59709=CARTESIAN_POINT('Ctrl Pts',(-5.71213288526391,-1.17701161509376,
-0.00102448187225759));
#59710=CARTESIAN_POINT('Origin',(-35.5608671147362,0.,0.));
#59711=CARTESIAN_POINT('',(-6.81086711473623,-1.17833240675485,-0.00101876322115038));
#59712=CARTESIAN_POINT('',(-6.7121328852639,-1.17891820058549,0.000833935244456217));
#59713=CARTESIAN_POINT('',(-35.5608671147362,-1.17775,1.38253677383905E-12));
#59714=CARTESIAN_POINT('Ctrl Pts',(-6.81086711473623,-1.17833240675485,
-0.00101876322115052));
#59715=CARTESIAN_POINT('Ctrl Pts',(-6.80598823450053,-1.17899064958735,
-0.0731127916092454));
#59716=CARTESIAN_POINT('Ctrl Pts',(-6.77459481185915,-1.14008822124925,
-0.536297066982777));
#59717=CARTESIAN_POINT('Ctrl Pts',(-6.71668684681209,-0.526104818498686,
-1.28981062717108));
#59718=CARTESIAN_POINT('Ctrl Pts',(-6.63714321959501,0.800597831774603,
-1.13993019337537));
#59719=CARTESIAN_POINT('Ctrl Pts',(-6.55759959237797,1.39180748198953,0.0571810028673485));
#59720=CARTESIAN_POINT('Ctrl Pts',(-6.47805596516089,0.704391810220957,
1.2017611708258));
#59721=CARTESIAN_POINT('Ctrl Pts',(-6.39851233794385,-0.630134339685656,
1.24230771065784));
#59722=CARTESIAN_POINT('Ctrl Pts',(-6.34278272113561,-1.15954471322248,
0.471113104676609));
#59723=CARTESIAN_POINT('Ctrl Pts',(-6.31356764673308,-1.17947481947488,
0.0405137706896489));
#59724=CARTESIAN_POINT('Ctrl Pts',(-6.31086711473623,-1.17919972158703,
0.000685029099866626));
#59725=CARTESIAN_POINT('Ctrl Pts',(-6.71213288526389,-1.17891820058549,
0.000833935244456199));
#59726=CARTESIAN_POINT('Ctrl Pts',(-6.68909985836987,-1.1761915925298,-0.339080789692708));
#59727=CARTESIAN_POINT('Ctrl Pts',(-6.63955228907016,-0.842772870908722,
-1.07495319818965));
#59728=CARTESIAN_POINT('Ctrl Pts',(-6.56349017736478,0.407797294762003,
-1.33195310338462));
#59729=CARTESIAN_POINT('Ctrl Pts',(-6.4839465501477,1.34097345813645,-0.377078092448702));
#59730=CARTESIAN_POINT('Ctrl Pts',(-6.40440292293066,1.04222448684345,0.924210918705832));
#59731=CARTESIAN_POINT('Ctrl Pts',(-6.32485929571359,-0.213994994785076,
1.37644609245625));
#59732=CARTESIAN_POINT('Ctrl Pts',(-6.26076928315801,-1.06775896809028,
0.721976263731495));
#59733=CARTESIAN_POINT('Ctrl Pts',(-6.22319381300811,-1.17666790445113,
0.164780718057665));
#59734=CARTESIAN_POINT('Ctrl Pts',(-6.2121328852639,-1.17601780156144,0.000518948208354537));
#59735=CARTESIAN_POINT('Origin',(-35.5608671147362,0.,0.));
#59736=CARTESIAN_POINT('',(-7.31086711473623,-1.17582863156191,-0.000195490556475402));
#59737=CARTESIAN_POINT('',(-7.2121328852639,-1.17866970590259,-0.0009291108299532));
#59738=CARTESIAN_POINT('',(-35.5608671147362,-1.17775,1.38253677383905E-12));
#59739=CARTESIAN_POINT('Ctrl Pts',(-7.31086711473623,-1.17582863156191,
-0.000195490556475393));
#59740=CARTESIAN_POINT('Ctrl Pts',(-7.29840882226798,-1.17610197282125,
-0.185283315322087));
#59741=CARTESIAN_POINT('Ctrl Pts',(-7.25943598739405,-1.04760233522402,
-0.763928060988009));
#59742=CARTESIAN_POINT('Ctrl Pts',(-7.19394861011444,-0.141221299809534,
-1.38580455999072));
#59743=CARTESIAN_POINT('Ctrl Pts',(-7.11440498289737,1.08944305027853,-0.868050444508131));
#59744=CARTESIAN_POINT('Ctrl Pts',(-7.03486135568032,1.3192581529162,0.447164019097165));
#59745=CARTESIAN_POINT('Ctrl Pts',(-6.95531772846325,0.337097531626415,
1.35157796230272));
#59746=CARTESIAN_POINT('Ctrl Pts',(-6.8806529814819,-0.875511261087105,
1.03501036576305));
#59747=CARTESIAN_POINT('Ctrl Pts',(-6.83250277690622,-1.17541339278816,
0.318686162360974));
#59748=CARTESIAN_POINT('Ctrl Pts',(-6.81086711473623,-1.17833240675485,
-0.00101876322115052));
#59749=CARTESIAN_POINT('Ctrl Pts',(-7.2121328852639,-1.17866970590259,-0.000929110829953382));
#59750=CARTESIAN_POINT('Ctrl Pts',(-7.20803498854302,-1.17919281713394,
-0.0614378874008591));
#59751=CARTESIAN_POINT('Ctrl Pts',(-7.17742254941645,-1.14740386673235,
-0.512904288824735));
#59752=CARTESIAN_POINT('Ctrl Pts',(-7.12029556788419,-0.563846417115518,
-1.27376407593289));
#59753=CARTESIAN_POINT('Ctrl Pts',(-7.04075194066713,0.766693435271625,
-1.16300424743101));
#59754=CARTESIAN_POINT('Ctrl Pts',(-6.96120831345008,1.39288756943087,0.0161840092713161));
#59755=CARTESIAN_POINT('Ctrl Pts',(-6.88166468623301,0.73946412716746,1.1805043447034));
#59756=CARTESIAN_POINT('Ctrl Pts',(-6.80212105901595,-0.593290019902356,
1.26031926729517));
#59757=CARTESIAN_POINT('Ctrl Pts',(-6.74561045869291,-1.15290745544743,
0.494459474393185));
#59758=CARTESIAN_POINT('Ctrl Pts',(-6.71561440077556,-1.1793303360935,0.0522131305606883));
#59759=CARTESIAN_POINT('Ctrl Pts',(-6.71213288526389,-1.17891820058549,
0.000833935244456199));
#59760=CARTESIAN_POINT('Origin',(-35.5608671147362,0.,0.));
#59761=CARTESIAN_POINT('',(-7.81086711473624,-1.17761266659143,0.00108828304854199));
#59762=CARTESIAN_POINT('',(-7.7121328852639,-1.17591322103504,-0.000380663888920052));
#59763=CARTESIAN_POINT('',(-35.5608671147362,-1.17775,1.38253677383905E-12));
#59764=CARTESIAN_POINT('Ctrl Pts',(-7.81086711473624,-1.17761266659143,
0.00108828304854196));
#59765=CARTESIAN_POINT('Ctrl Pts',(-7.79082941003544,-1.17489672111447,
-0.295468412184884));
#59766=CARTESIAN_POINT('Ctrl Pts',(-7.74427716292896,-0.91073905944592,
-0.988747856234089));
#59767=CARTESIAN_POINT('Ctrl Pts',(-7.6712103734168,0.255114094679148,-1.36942124005254));
#59768=CARTESIAN_POINT('Ctrl Pts',(-7.59166674619974,1.28994347575683,-0.525779006202587));
#59769=CARTESIAN_POINT('Ctrl Pts',(-7.51212311898267,1.13972793260945,0.800885743187348));
#59770=CARTESIAN_POINT('Ctrl Pts',(-7.43257949176562,-0.0575325601190364,
1.39179299413997));
#59771=CARTESIAN_POINT('Ctrl Pts',(-7.36549415701681,-1.0226996709703,0.811798018593268));
#59772=CARTESIAN_POINT('Ctrl Pts',(-7.32492336467368,-1.17552023030474,
0.208632543615389));
#59773=CARTESIAN_POINT('Ctrl Pts',(-7.31086711473623,-1.17582863156191,
-0.000195490556475393));
#59774=CARTESIAN_POINT('Ctrl Pts',(-7.7121328852639,-1.17591322103504,-0.00038066388892));
#59775=CARTESIAN_POINT('Ctrl Pts',(-7.70045557631047,-1.17641412149157,
-0.173834599103264));
#59776=CARTESIAN_POINT('Ctrl Pts',(-7.66226372495135,-1.05905068433182,
-0.740488825604028));
#59777=CARTESIAN_POINT('Ctrl Pts',(-7.59755733118654,-0.181955590322025,
-1.38104665612053));
#59778=CARTESIAN_POINT('Ctrl Pts',(-7.51801370396949,1.06341709890332,-0.899745395648787));
#59779=CARTESIAN_POINT('Ctrl Pts',(-7.43847007675242,1.3318500546647,0.408133722106875));
#59780=CARTESIAN_POINT('Ctrl Pts',(-7.35892644953538,0.376739361598168,
1.34106866216976));
#59781=CARTESIAN_POINT('Ctrl Pts',(-7.28348071903918,-0.857438750290286,
1.0573987684494));
#59782=CARTESIAN_POINT('Ctrl Pts',(-7.2345495309487,-1.17580814058615,0.330070886875712));
#59783=CARTESIAN_POINT('Ctrl Pts',(-7.2121328852639,-1.17866970590259,-0.000929110829953382));
#59784=CARTESIAN_POINT('Origin',(-35.5608671147362,0.,0.));
#59785=CARTESIAN_POINT('',(-8.31086711473624,-1.17960456788227,-0.000301336879507475));
#59786=CARTESIAN_POINT('',(-8.21213288526389,-1.17726943853211,0.00106644700324871));
#59787=CARTESIAN_POINT('',(-35.5608671147362,-1.17775,1.38253677383905E-12));
#59788=CARTESIAN_POINT('Ctrl Pts',(-8.31086711473624,-1.17960456788227,
-0.000301336879507583));
#59789=CARTESIAN_POINT('Ctrl Pts',(-8.30976454020858,-1.1796600868532,-0.0165478569140431));
#59790=CARTESIAN_POINT('Ctrl Pts',(-8.28214742327524,-1.17198360631363,
-0.423434528327187));
#59791=CARTESIAN_POINT('Ctrl Pts',(-8.2280157639362,-0.703784610462002,
-1.20211686457176));
#59792=CARTESIAN_POINT('Ctrl Pts',(-8.14847213671916,0.630761852593739,
-1.24198921868246));
#59793=CARTESIAN_POINT('Ctrl Pts',(-8.06892850950209,1.38584018711583,-0.140871252517076));
#59794=CARTESIAN_POINT('Ctrl Pts',(-7.98938488228504,0.867775232498749,
1.08966227789749));
#59795=CARTESIAN_POINT('Ctrl Pts',(-7.90984125506796,-0.447497238546542,
1.31914516089179));
#59796=CARTESIAN_POINT('Ctrl Pts',(-7.85033533255171,-1.12389613593606,
0.584228134995474));
#59797=CARTESIAN_POINT('Ctrl Pts',(-7.81734395244113,-1.17849054848121,
0.0969450497794044));
#59798=CARTESIAN_POINT('Ctrl Pts',(-7.81086711473624,-1.17761266659143,
0.00108828304854196));
#59799=CARTESIAN_POINT('Ctrl Pts',(-8.21213288526389,-1.17726943853211,
0.00106644700324865));
#59800=CARTESIAN_POINT('Ctrl Pts',(-8.19287616407791,-1.17477250782038,
-0.284143183611619));
#59801=CARTESIAN_POINT('Ctrl Pts',(-8.14710490048626,-0.927115044542352,
-0.965942824430619));
#59802=CARTESIAN_POINT('Ctrl Pts',(-8.0748190944889,0.214690325287459,-1.37633781008121));
#59803=CARTESIAN_POINT('Ctrl Pts',(-7.99527546727185,1.27390645824667,-0.563524656841738));
#59804=CARTESIAN_POINT('Ctrl Pts',(-7.91573184005478,1.16281054989956,0.766987176081464));
#59805=CARTESIAN_POINT('Ctrl Pts',(-7.83618821283773,-0.016535840652032,
1.39288343704887));
#59806=CARTESIAN_POINT('Ctrl Pts',(-7.7683218945741,-1.00978864286737,0.835134152043033));
#59807=CARTESIAN_POINT('Ctrl Pts',(-7.72697011871615,-1.17527677499773,
0.220010570106118));
#59808=CARTESIAN_POINT('Ctrl Pts',(-7.7121328852639,-1.17591322103504,-0.00038066388892));
#59809=CARTESIAN_POINT('Origin',(-35.5608671147362,0.,0.));
#59810=CARTESIAN_POINT('',(-8.81086711473623,-1.17669902819161,-0.000938630091047622));
#59811=CARTESIAN_POINT('',(-8.71213288526389,-1.17968925837541,-8.9173716636276E-5));
#59812=CARTESIAN_POINT('',(-35.5608671147362,-1.17775,1.38253677383905E-12));
#59813=CARTESIAN_POINT('Ctrl Pts',(-8.81086711473623,-1.17669902819161,
-0.000938630091047495));
#59814=CARTESIAN_POINT('Ctrl Pts',(-8.80218512797603,-1.17765573995214,
-0.129684452328276));
#59815=CARTESIAN_POINT('Ctrl Pts',(-8.76698859881015,-1.09874317011466,
-0.65047597720531));
#59816=CARTESIAN_POINT('Ctrl Pts',(-8.70527752723856,-0.336414693769986,
-1.35174808593414));
#59817=CARTESIAN_POINT('Ctrl Pts',(-8.62573390002151,0.955260057255724,
-1.01384217559874));
#59818=CARTESIAN_POINT('Ctrl Pts',(-8.54619027280444,1.36935675665274,0.255459991036712));
#59819=CARTESIAN_POINT('Ctrl Pts',(-8.46664664558739,0.525453160360428,
1.29007624204083));
#59820=CARTESIAN_POINT('Ctrl Pts',(-8.38820559289798,-0.782784891184577,
1.14161242002925));
#59821=CARTESIAN_POINT('Ctrl Pts',(-8.33627908261427,-1.1783249751922,0.374145954339654));
#59822=CARTESIAN_POINT('Ctrl Pts',(-8.31086711473624,-1.17960456788227,
-0.000301336879507583));
#59823=CARTESIAN_POINT('Ctrl Pts',(-8.71213288526389,-1.17968925837541,
-8.91737166363286E-5));
#59824=CARTESIAN_POINT('Ctrl Pts',(-8.71181129425105,-1.17969439827978,
-0.00482692941936411));
#59825=CARTESIAN_POINT('Ctrl Pts',(-8.68497516083253,-1.17751950125305,
-0.400178411758024));
#59826=CARTESIAN_POINT('Ctrl Pts',(-8.63162448500833,-0.738867661530245,
-1.1808777591165));
#59827=CARTESIAN_POINT('Ctrl Pts',(-8.55208085779126,0.59392663665258,-1.26001938616266));
#59828=CARTESIAN_POINT('Ctrl Pts',(-8.47253723057421,1.38109257254281,-0.181606743537313));
#59829=CARTESIAN_POINT('Ctrl Pts',(-8.39299360335714,0.899476756568682,
1.06364433323544));
#59830=CARTESIAN_POINT('Ctrl Pts',(-8.3134499761401,-0.408470123411764,
1.33174692096928));
#59831=CARTESIAN_POINT('Ctrl Pts',(-8.25316307010899,-1.11536792071274,
0.607680449651806));
#59832=CARTESIAN_POINT('Ctrl Pts',(-8.2193907064836,-1.17821052692035,0.108561408848025));
#59833=CARTESIAN_POINT('Ctrl Pts',(-8.21213288526389,-1.17726943853211,
0.00106644700324865));
#59834=CARTESIAN_POINT('Origin',(-35.5608671147362,0.,0.));
#59835=CARTESIAN_POINT('',(-9.31086711473623,-1.17620260599838,0.000684878377940163));
#59836=CARTESIAN_POINT('',(-9.21213288526389,-1.17700074425756,-0.00102218139484231));
#59837=CARTESIAN_POINT('',(-35.5608671147362,-1.17775,1.38253677383905E-12));
#59838=CARTESIAN_POINT('Ctrl Pts',(-9.31086711473623,-1.17620260599838,
0.000684878377940155));
#59839=CARTESIAN_POINT('Ctrl Pts',(-9.29460571574348,-1.17492956671425,
-0.240712289578281));
#59840=CARTESIAN_POINT('Ctrl Pts',(-9.25182977434505,-0.984958310030366,
-0.877551160602252));
#59841=CARTESIAN_POINT('Ctrl Pts',(-9.18253929054092,0.0582356635878705,
-1.3917637520418));
#59842=CARTESIAN_POINT('Ctrl Pts',(-9.10299566332388,1.20229459640314,-0.703480943217913));
#59843=CARTESIAN_POINT('Ctrl Pts',(-9.02345203610679,1.24182985382652,0.631075548691406));
#59844=CARTESIAN_POINT('Ctrl Pts',(-8.94390840888976,0.140521196236644,
1.38587572582076));
#59845=CARTESIAN_POINT('Ctrl Pts',(-8.87304676843288,-0.955586084668702,
0.92407937504744));
#59846=CARTESIAN_POINT('Ctrl Pts',(-8.82869967038171,-1.17473396925088,
0.263501653288927));
#59847=CARTESIAN_POINT('Ctrl Pts',(-8.81086711473623,-1.17669902819161,
-0.000938630091047495));
#59848=CARTESIAN_POINT('Ctrl Pts',(-9.21213288526389,-1.17700074425756,
-0.0010221813948424));
#59849=CARTESIAN_POINT('Ctrl Pts',(-9.20423188201851,-1.17796598494008,
-0.118110947805483));
#59850=CARTESIAN_POINT('Ctrl Pts',(-9.16981633636744,-1.10803357457856,
-0.627004213361478));
#59851=CARTESIAN_POINT('Ctrl Pts',(-9.10888624831068,-0.37606182780791,
-1.34125881353932));
#59852=CARTESIAN_POINT('Ctrl Pts',(-9.02934262109362,0.925000425181733,
-1.04152384353156));
#59853=CARTESIAN_POINT('Ctrl Pts',(-8.94979899387657,1.37628353717109,0.215037970003031));
#59854=CARTESIAN_POINT('Ctrl Pts',(-8.87025536665949,0.563202860613652,
1.27404875928191));
#59855=CARTESIAN_POINT('Ctrl Pts',(-8.79103333045528,-0.761901787005847,
1.16306729225316));
#59856=CARTESIAN_POINT('Ctrl Pts',(-8.73832583665674,-1.17927062333932,
0.385791649689134));
#59857=CARTESIAN_POINT('Ctrl Pts',(-8.71213288526389,-1.17968925837541,
-8.91737166363286E-5));
#59858=CARTESIAN_POINT('Origin',(-35.5608671147362,0.,0.));
#59859=CARTESIAN_POINT('',(-9.81086711473622,-1.17920857465814,0.00067940234225231));
#59860=CARTESIAN_POINT('',(-9.71213288526389,-1.17602308153073,0.000524756514563435));
#59861=CARTESIAN_POINT('',(-35.5608671147362,-1.17775,1.38253677383905E-12));
#59862=CARTESIAN_POINT('Ctrl Pts',(-9.81086711473622,-1.17920857465814,
0.000679402342252224));
#59863=CARTESIAN_POINT('Ctrl Pts',(-9.78702630351093,-1.17679579427288,
-0.350929376268994));
#59864=CARTESIAN_POINT('Ctrl Pts',(-9.73667094987996,-0.823009981098092,
-1.0977918872868));
#59865=CARTESIAN_POINT('Ctrl Pts',(-9.65980105384327,0.448163591769547,
-1.31891892435554));
#59866=CARTESIAN_POINT('Ctrl Pts',(-9.58025742662623,1.35183301838504,-0.33607324263468));
#59867=CARTESIAN_POINT('Ctrl Pts',(-9.50071379940917,1.0136008524543,0.955516114942553));
#59868=CARTESIAN_POINT('Ctrl Pts',(-9.42117017219209,-0.255805871095256,
1.36929218588443));
#59869=CARTESIAN_POINT('Ctrl Pts',(-9.35788794396779,-1.07874206960061,
0.697703046197374));
#59870=CARTESIAN_POINT('Ctrl Pts',(-9.32112025814917,-1.17700528320692,
0.152890711568344));
#59871=CARTESIAN_POINT('Ctrl Pts',(-9.31086711473623,-1.17620260599838,
0.000684878377940155));
#59872=CARTESIAN_POINT('Ctrl Pts',(-9.71213288526389,-1.17602308153073,
0.000524756514563435));
#59873=CARTESIAN_POINT('Ctrl Pts',(-9.69665246978596,-1.17510280305878,
-0.229366621244868));
#59874=CARTESIAN_POINT('Ctrl Pts',(-9.65465751190234,-0.99878260724446,
-0.854314884247616));
#59875=CARTESIAN_POINT('Ctrl Pts',(-9.58614801161304,0.0172395002259546,
-1.39287490567643));
#59876=CARTESIAN_POINT('Ctrl Pts',(-9.50660438439598,1.18106435331442,-0.738569357989597));
#59877=CARTESIAN_POINT('Ctrl Pts',(-9.42706075717891,1.25986932500286,0.59424488819676));
#59878=CARTESIAN_POINT('Ctrl Pts',(-9.34751712996187,0.181257885165623,
1.3811384008478));
#59879=CARTESIAN_POINT('Ctrl Pts',(-9.27587450599017,-0.940193819229214,
0.947077805540203));
#59880=CARTESIAN_POINT('Ctrl Pts',(-9.23074642442419,-1.17472678680111,
0.274820806024488));
#59881=CARTESIAN_POINT('Ctrl Pts',(-9.21213288526389,-1.17700074425756,
-0.0010221813948424));
#59882=CARTESIAN_POINT('Origin',(-35.5608671147362,0.,0.));
#59883=CARTESIAN_POINT('',(-10.3108671147362,-1.17832052192974,-0.00102120244541717));
#59884=CARTESIAN_POINT('',(-10.2121328852639,-1.17892853960487,0.000829332411371141));
#59885=CARTESIAN_POINT('',(-35.5608671147362,-1.17775,1.38253677383905E-12));
#59886=CARTESIAN_POINT('Ctrl Pts',(-10.3108671147362,-1.17832052192974,
-0.0010212024454173));
#59887=CARTESIAN_POINT('Ctrl Pts',(-10.3059614336841,-1.17898318451254,
-0.073513146495671));
#59888=CARTESIAN_POINT('Ctrl Pts',(-10.2745412102262,-1.13983029700994,
-0.537100248604522));
#59889=CARTESIAN_POINT('Ctrl Pts',(-10.2166064443627,-0.524801368121128,
-1.29034152766978));
#59890=CARTESIAN_POINT('Ctrl Pts',(-10.1370628171456,0.801749170760637,
-1.13912071405783));
#59891=CARTESIAN_POINT('Ctrl Pts',(-10.0575191899286,1.39174899779504,0.0585872097601163));
#59892=CARTESIAN_POINT('Ctrl Pts',(-9.97797556271153,0.703177231089948,
1.20247225152501));
#59893=CARTESIAN_POINT('Ctrl Pts',(-9.89843193549446,-0.63138920452485,
1.24167040973862));
#59894=CARTESIAN_POINT('Ctrl Pts',(-9.84272911950269,-1.15976589559383,
0.470312429397423));
#59895=CARTESIAN_POINT('Ctrl Pts',(-9.81354084591662,-1.17947916637948,
0.0401120938638806));
#59896=CARTESIAN_POINT('Ctrl Pts',(-9.81086711473622,-1.17920857465814,
0.000679402342252224));
#59897=CARTESIAN_POINT('Ctrl Pts',(-10.2121328852639,-1.17892853960487,
0.000829332411371106));
#59898=CARTESIAN_POINT('Ctrl Pts',(-10.1890730575534,-1.17620975931657,
-0.339473117241695));
#59899=CARTESIAN_POINT('Ctrl Pts',(-10.1394986874372,-0.842127078826765,
-1.07571404946627));
#59900=CARTESIAN_POINT('Ctrl Pts',(-10.0634097749154,0.40914284781568,-1.33154039867832));
#59901=CARTESIAN_POINT('Ctrl Pts',(-9.98386614769835,1.34135376086346,-0.375723024911412));
#59902=CARTESIAN_POINT('Ctrl Pts',(-9.90432252048127,1.04129016283722,0.9252634759946));
#59903=CARTESIAN_POINT('Ctrl Pts',(-9.82477889326422,-0.215385600998657,
1.3762291764505));
#59904=CARTESIAN_POINT('Ctrl Pts',(-9.76071568152509,-1.06813113821466,
0.721171110256381));
#59905=CARTESIAN_POINT('Ctrl Pts',(-9.72316701219165,-1.17667903740497,
0.164386679045683));
#59906=CARTESIAN_POINT('Ctrl Pts',(-9.71213288526389,-1.17602308153073,
0.000524756514563435));
#59907=CARTESIAN_POINT('Origin',(-35.5608671147362,0.,0.));
#59908=CARTESIAN_POINT('',(-10.8108671147362,-1.17582670261709,-0.000188998789078225));
#59909=CARTESIAN_POINT('',(-10.7121328852639,-1.17865848830409,-0.000932771918738112));
#59910=CARTESIAN_POINT('',(-35.5608671147362,-1.17775,1.38253677383905E-12));
#59911=CARTESIAN_POINT('Ctrl Pts',(-10.8108671147362,-1.17582670261709,
-0.000188998789078139));
#59912=CARTESIAN_POINT('Ctrl Pts',(-10.7983820214515,-1.176091511301,-0.185675751126754));
#59913=CARTESIAN_POINT('Ctrl Pts',(-10.7593823857611,-1.04720114782861,
-0.764732004625058));
#59914=CARTESIAN_POINT('Ctrl Pts',(-10.6938682076651,-0.139821056801252,
-1.38594653796095));
#59915=CARTESIAN_POINT('Ctrl Pts',(-10.614324580448,1.09031954355872,-0.866949264343001));
#59916=CARTESIAN_POINT('Ctrl Pts',(-10.534780953231,1.31880567985816,0.4484967255007));
#59917=CARTESIAN_POINT('Ctrl Pts',(-10.4552373260139,0.335731770057017,
1.35191786458549));
#59918=CARTESIAN_POINT('Ctrl Pts',(-10.380599379849,-0.876121404964598,
1.03423932121344));
#59919=CARTESIAN_POINT('Ctrl Pts',(-10.3324759760898,-1.175401582903,0.318296003784583));
#59920=CARTESIAN_POINT('Ctrl Pts',(-10.3108671147362,-1.17832052192974,
-0.0010212024454173));
#59921=CARTESIAN_POINT('Ctrl Pts',(-10.7121328852639,-1.17865848830409,
-0.00093277191873813));
#59922=CARTESIAN_POINT('Ctrl Pts',(-10.7080081877265,-1.17918638551096,
-0.0618387895771099));
#59923=CARTESIAN_POINT('Ctrl Pts',(-10.6773689477835,-1.14715919296215,
-0.513706649318993));
#59924=CARTESIAN_POINT('Ctrl Pts',(-10.6202151654348,-0.562559160376593,
-1.27433311748048));
#59925=CARTESIAN_POINT('Ctrl Pts',(-10.5406715382178,0.767868104821389,
-1.1622290122128));
#59926=CARTESIAN_POINT('Ctrl Pts',(-10.4611279110007,1.39287050668653,0.0175913283742381));
#59927=CARTESIAN_POINT('Ctrl Pts',(-10.3815842837836,0.73827100732634,1.18125087215736));
#59928=CARTESIAN_POINT('Ctrl Pts',(-10.3020406565666,-0.594563101826563,
1.25971918346015));
#59929=CARTESIAN_POINT('Ctrl Pts',(-10.24555685706,-1.15314141439117,0.493657848568567));
#59930=CARTESIAN_POINT('Ctrl Pts',(-10.2155875999591,-1.17933585445271,
0.0518118414046211));
#59931=CARTESIAN_POINT('Ctrl Pts',(-10.2121328852639,-1.17892853960487,
0.000829332411371106));
#59932=CARTESIAN_POINT('Origin',(-35.5608671147362,0.,0.));
#59933=CARTESIAN_POINT('',(-11.3108671147362,-1.17762466953345,0.00108839146631162));
#59934=CARTESIAN_POINT('',(-11.2121328852639,-1.17590941904104,-0.000374468625826685));
#59935=CARTESIAN_POINT('',(-35.5608671147362,-1.17775,1.38253677383905E-12));
#59936=CARTESIAN_POINT('Ctrl Pts',(-11.3108671147362,-1.17762466953345,
0.00108839146631154));
#59937=CARTESIAN_POINT('Ctrl Pts',(-11.290802609219,-1.17490239677762,-0.295857233741433));
#59938=CARTESIAN_POINT('Ctrl Pts',(-11.244223561296,-0.910167371062506,
-0.989528333638478));
#59939=CARTESIAN_POINT('Ctrl Pts',(-11.1711299709674,0.256497582227027,
-1.36916278225881));
#59940=CARTESIAN_POINT('Ctrl Pts',(-11.0915863437504,1.2904740469978,-0.52447542176553));
#59941=CARTESIAN_POINT('Ctrl Pts',(-11.0120427165333,1.13891816249902,0.802036877668863));
#59942=CARTESIAN_POINT('Ctrl Pts',(-10.9324990893162,-0.0589387521943207,
1.39173415475109));
#59943=CARTESIAN_POINT('Ctrl Pts',(-10.8654405553839,-1.02313400954157,
0.810996401841933));
#59944=CARTESIAN_POINT('Ctrl Pts',(-10.8248965638572,-1.17552913816377,
0.208241718963453));
#59945=CARTESIAN_POINT('Ctrl Pts',(-10.8108671147362,-1.17582670261709,
-0.000188998789078139));
#59946=CARTESIAN_POINT('Ctrl Pts',(-11.2121328852639,-1.17590941904104,
-0.000374468625826806));
#59947=CARTESIAN_POINT('Ctrl Pts',(-11.200428775494,-1.17640320837023,-0.174227904069011));
#59948=CARTESIAN_POINT('Ctrl Pts',(-11.1622101233184,-1.05866553135645,
-0.74129353109382));
#59949=CARTESIAN_POINT('Ctrl Pts',(-11.0974769287372,-0.18056013375031,
-1.38122979309427));
#59950=CARTESIAN_POINT('Ctrl Pts',(-11.0179333015201,1.06432562899421,-0.898670495063273));
#59951=CARTESIAN_POINT('Ctrl Pts',(-10.938389674303,1.33143701009596,0.409479170871799));
#59952=CARTESIAN_POINT('Ctrl Pts',(-10.858846047086,0.375384198042811,1.34144862260576));
#59953=CARTESIAN_POINT('Ctrl Pts',(-10.7834271174063,-0.858068354441969,
1.0566331129145));
#59954=CARTESIAN_POINT('Ctrl Pts',(-10.7345227301322,-1.17579293599113,
0.329679660768861));
#59955=CARTESIAN_POINT('Ctrl Pts',(-10.7121328852639,-1.17865848830409,
-0.00093277191873813));
#59956=CARTESIAN_POINT('Origin',(-35.5608671147362,0.,0.));
#59957=CARTESIAN_POINT('',(-11.8108671147362,-1.17960016821189,-0.000308426038616608));
#59958=CARTESIAN_POINT('',(-11.7121328852639,-1.17728095270416,0.00106778596620033));
#59959=CARTESIAN_POINT('',(-35.5608671147362,-1.17775,1.38253677383905E-12));
#59960=CARTESIAN_POINT('Ctrl Pts',(-11.8108671147362,-1.17960016821189,
-0.000308426038616535));
#59961=CARTESIAN_POINT('Ctrl Pts',(-11.8097377393921,-1.17965824466903,
-0.0169500240275318));
#59962=CARTESIAN_POINT('Ctrl Pts',(-11.7820938216423,-1.17178738065343,
-0.424233150976045));
#59963=CARTESIAN_POINT('Ctrl Pts',(-11.7279353614868,-0.702569672259767,
-1.20282733159494));
#59964=CARTESIAN_POINT('Ctrl Pts',(-11.6483917342698,0.632016395318918,
-1.2413512839076));
#59965=CARTESIAN_POINT('Ctrl Pts',(-11.5688481070527,1.38598181139171,-0.139470973691));
#59966=CARTESIAN_POINT('Ctrl Pts',(-11.4893044798357,0.866673830973786,
1.09053849300069));
#59967=CARTESIAN_POINT('Ctrl Pts',(-11.4097608526186,-0.448829830616605,
1.31869235121755));
#59968=CARTESIAN_POINT('Ctrl Pts',(-11.3502817309188,-1.12418153891304,
0.583423595664754));
#59969=CARTESIAN_POINT('Ctrl Pts',(-11.3173171516247,-1.17849978502934,
0.0965460260839821));
#59970=CARTESIAN_POINT('Ctrl Pts',(-11.3108671147362,-1.17762466953345,
0.00108839146631154));
#59971=CARTESIAN_POINT('Ctrl Pts',(-11.7121328852639,-1.17728095270416,
0.00106778596620021));
#59972=CARTESIAN_POINT('Ctrl Pts',(-11.6928493632614,-1.17477548883292,
-0.284531699071451));
#59973=CARTESIAN_POINT('Ctrl Pts',(-11.6470512988533,-0.926562106106686,
-0.966727326674524));
#59974=CARTESIAN_POINT('Ctrl Pts',(-11.5747386920395,0.216080821741205,
-1.37612019159185));
#59975=CARTESIAN_POINT('Ctrl Pts',(-11.4951950648225,1.27447517462567,-0.562237256408714));
#59976=CARTESIAN_POINT('Ctrl Pts',(-11.4156514376054,1.16203501799428,0.768161649775757));
#59977=CARTESIAN_POINT('Ctrl Pts',(-11.3361078103884,-0.0179431554001853,
1.39286601882789));
#59978=CARTESIAN_POINT('Ctrl Pts',(-11.2682682929412,-1.010239900524,0.834334123584145));
#59979=CARTESIAN_POINT('Ctrl Pts',(-11.2269433178997,-1.17528457582444,
0.219620442970041));
#59980=CARTESIAN_POINT('Ctrl Pts',(-11.2121328852639,-1.17590941904104,
-0.000374468625826806));
#59981=CARTESIAN_POINT('Origin',(-35.5608671147362,0.,0.));
#59982=CARTESIAN_POINT('',(-12.3108671147362,-1.17668924014875,-0.000935216629109687));
#59983=CARTESIAN_POINT('',(-12.2121328852639,-1.17968782784267,-9.65820520404392E-5));
#59984=CARTESIAN_POINT('',(-35.5608671147362,-1.17775,1.38253677383905E-12));
#59985=CARTESIAN_POINT('Ctrl Pts',(-12.3108671147362,-1.17668924014875,
-0.000935216629109649));
#59986=CARTESIAN_POINT('Ctrl Pts',(-12.3021583271596,-1.17764488283097,
-0.130081176142648));
#59987=CARTESIAN_POINT('Ctrl Pts',(-12.2669349971772,-1.09841677303328,
-0.651281554432957));
#59988=CARTESIAN_POINT('Ctrl Pts',(-12.2051971247892,-0.335048760661853,
-1.35208729821336));
#59989=CARTESIAN_POINT('Ctrl Pts',(-12.1256534975721,0.956283922151258,
-1.01287649506048));
#59990=CARTESIAN_POINT('Ctrl Pts',(-12.0461098703551,1.36909794940973,0.256843413256152));
#59991=CARTESIAN_POINT('Ctrl Pts',(-11.966566243138,0.524149441947044,1.29060648399021));
#59992=CARTESIAN_POINT('Ctrl Pts',(-11.8881519912651,-0.783491007014861,
1.14087211442108));
#59993=CARTESIAN_POINT('Ctrl Pts',(-11.8362522817978,-1.17829477353105,
0.373747681458496));
#59994=CARTESIAN_POINT('Ctrl Pts',(-11.8108671147362,-1.17960016821189,
-0.000308426038616535));
#59995=CARTESIAN_POINT('Ctrl Pts',(-12.2121328852639,-1.17968782784267,
-9.65820520404728E-5));
#59996=CARTESIAN_POINT('Ctrl Pts',(-12.2117844934346,-1.17969384319053,
-0.00522919056453987));
#59997=CARTESIAN_POINT('Ctrl Pts',(-12.1849215591996,-1.17733532698894,
-0.400975971111822));
#59998=CARTESIAN_POINT('Ctrl Pts',(-12.1315440825589,-0.737674164708033,
-1.18162368373076));
#59999=CARTESIAN_POINT('Ctrl Pts',(-12.0520004553419,0.595199415261899,
-1.25941865926429));
#60000=CARTESIAN_POINT('Ctrl Pts',(-11.9724568281248,1.3812753570299,-0.180211240751194));
#60001=CARTESIAN_POINT('Ctrl Pts',(-11.8929132009078,0.898401626530242,
1.06455259178631));
#60002=CARTESIAN_POINT('Ctrl Pts',(-11.8133695736907,-0.409815467802085,
1.33133353656448));
#60003=CARTESIAN_POINT('Ctrl Pts',(-11.7531094684761,-1.11566740233522,
0.606875413125733));
#60004=CARTESIAN_POINT('Ctrl Pts',(-11.7193639056671,-1.17822046263239,
0.108163144542644));
#60005=CARTESIAN_POINT('Ctrl Pts',(-11.7121328852639,-1.17728095270416,
0.00106778596620021));
#60006=CARTESIAN_POINT('Origin',(-35.5608671147362,0.,0.));
#60007=CARTESIAN_POINT('',(-12.8108671147362,-1.17620961977275,0.000690027712506509));
#60008=CARTESIAN_POINT('',(-12.7121328852639,-1.17698990462219,-0.00101984215893941));
#60009=CARTESIAN_POINT('',(-35.5608671147362,-1.17775,1.38253677383905E-12));
#60010=CARTESIAN_POINT('Ctrl Pts',(-12.8108671147362,-1.17620961977275,
0.000690027712506418));
#60011=CARTESIAN_POINT('Ctrl Pts',(-12.794578914927,-1.17492443634169,-0.24110138251064));
#60012=CARTESIAN_POINT('Ctrl Pts',(-12.7517761727121,-0.984474855720211,
-0.878347397724903));
#60013=CARTESIAN_POINT('Ctrl Pts',(-12.6824588880915,0.0596418257590296,
-1.39170420227544));
#60014=CARTESIAN_POINT('Ctrl Pts',(-12.6029152608745,1.2030047565203,-0.702265825596333));
#60015=CARTESIAN_POINT('Ctrl Pts',(-12.5233716336574,1.24119160218488,0.632329930239507));
#60016=CARTESIAN_POINT('Ctrl Pts',(-12.4438280064404,0.139120881682115,
1.38601699639326));
#60017=CARTESIAN_POINT('Ctrl Pts',(-12.3729931668,-0.956104870347375,0.923288487221614));
#60018=CARTESIAN_POINT('Ctrl Pts',(-12.3286728695652,-1.17473535860622,
0.263113168064762));
#60019=CARTESIAN_POINT('Ctrl Pts',(-12.3108671147362,-1.17668924014875,
-0.000935216629109649));
#60020=CARTESIAN_POINT('Ctrl Pts',(-12.7121328852639,-1.17698990462219,
-0.00101984215893938));
#60021=CARTESIAN_POINT('Ctrl Pts',(-12.704205081202,-1.17795555935218,-0.11850851884417));
#60022=CARTESIAN_POINT('Ctrl Pts',(-12.6697627347345,-1.10772178842638,
-0.62780956583934));
#60023=CARTESIAN_POINT('Ctrl Pts',(-12.6088058458613,-0.374706472475756,
-1.34163808932065));
#60024=CARTESIAN_POINT('Ctrl Pts',(-12.5292622186442,0.926052274160795,
-1.04058872219181));
#60025=CARTESIAN_POINT('Ctrl Pts',(-12.4497185914272,1.37606556746074,0.216428411443782));
#60026=CARTESIAN_POINT('Ctrl Pts',(-12.3701749642101,0.561915316568623,
1.27461715045607));
#60027=CARTESIAN_POINT('Ctrl Pts',(-12.2909797288224,-0.762628277933677,
1.1623348962687));
#60028=CARTESIAN_POINT('Ctrl Pts',(-12.2382990358403,-1.17923604199531,
0.385390665053393));
#60029=CARTESIAN_POINT('Ctrl Pts',(-12.2121328852639,-1.17968782784267,
-9.65820520404728E-5));
#60030=CARTESIAN_POINT('Origin',(-35.5608671147362,0.,0.));
#60031=CARTESIAN_POINT('',(-13.3108671147362,-1.1792173683553,0.000673743327001118));
#60032=CARTESIAN_POINT('',(-13.2121328852639,-1.17602842142206,0.000530545984581826));
#60033=CARTESIAN_POINT('',(-35.5608671147362,-1.17775,1.38253677383905E-12));
#60034=CARTESIAN_POINT('Ctrl Pts',(-13.3108671147362,-1.1792173683553,0.000673743327001138));
#60035=CARTESIAN_POINT('Ctrl Pts',(-13.2869995026945,-1.17681788725409,
-0.351323391984844));
#60036=CARTESIAN_POINT('Ctrl Pts',(-13.236617348247,-0.822343662973783,
-1.09854622043971));
#60037=CARTESIAN_POINT('Ctrl Pts',(-13.1597206513939,0.449495954917602,
-1.3184654415356));
#60038=CARTESIAN_POINT('Ctrl Pts',(-13.0801770241768,1.35217188563002,-0.334707223887899));
#60039=CARTESIAN_POINT('Ctrl Pts',(-13.0006333969598,1.01263491332703,0.956539735882493));
#60040=CARTESIAN_POINT('Ctrl Pts',(-12.9210897697427,-0.25718922789799,
1.36903302920864));
#60041=CARTESIAN_POINT('Ctrl Pts',(-12.8578343423349,-1.07909821874922,
0.696897543302798));
#60042=CARTESIAN_POINT('Ctrl Pts',(-12.8210934573327,-1.17701650612111,
0.152495741468027));
#60043=CARTESIAN_POINT('Ctrl Pts',(-12.8108671147362,-1.17620961977275,
0.000690027712506418));
#60044=CARTESIAN_POINT('Ctrl Pts',(-13.2121328852639,-1.17602842142206,
0.000530545984581809));
#60045=CARTESIAN_POINT('Ctrl Pts',(-13.1966256689695,-1.17509613497152,
-0.229756223488072));
#60046=CARTESIAN_POINT('Ctrl Pts',(-13.1546039102694,-0.998316605074535,
-0.855113302780238));
#60047=CARTESIAN_POINT('Ctrl Pts',(-13.0860676091637,0.0186468059951288,
-1.39285677650551));
#60048=CARTESIAN_POINT('Ctrl Pts',(-13.0065239819466,1.18180997643742,-0.737375672791089));
#60049=CARTESIAN_POINT('Ctrl Pts',(-12.9269803547296,1.25926827663031,0.595517515026806));
#60050=CARTESIAN_POINT('Ctrl Pts',(-12.8474367275125,0.179862336254169,
1.38132083283659));
#60051=CARTESIAN_POINT('Ctrl Pts',(-12.7758209043573,-0.940730875292218,
0.946290183190409));
#60052=CARTESIAN_POINT('Ctrl Pts',(-12.7307196236077,-1.17472592689814,
0.274432385832564));
#60053=CARTESIAN_POINT('Ctrl Pts',(-12.7121328852639,-1.17698990462219,
-0.00101984215893938));
#60054=CARTESIAN_POINT('Origin',(-35.5608671147362,0.,0.));
#60055=CARTESIAN_POINT('',(-13.8108671147362,-1.1783086217086,-0.00102359871729984));
#60056=CARTESIAN_POINT('',(-13.7121328852639,-1.17893883534851,0.000824692032647192));
#60057=CARTESIAN_POINT('',(-35.5608671147362,-1.17775,1.38253677383905E-12));
#60058=CARTESIAN_POINT('Ctrl Pts',(-13.8108671147362,-1.1783086217086,-0.0010235987173));
#60059=CARTESIAN_POINT('Ctrl Pts',(-13.8059346328676,-1.17897568560547,
-0.0739134811648439));
#60060=CARTESIAN_POINT('Ctrl Pts',(-13.7744876085933,-1.13957191331326,
-0.537903456860039));
#60061=CARTESIAN_POINT('Ctrl Pts',(-13.7165260419133,-0.523497382004637,
-1.29087111093451));
#60062=CARTESIAN_POINT('Ctrl Pts',(-13.6369824146963,0.802899691287971,
-1.13831007187878));
#60063=CARTESIAN_POINT('Ctrl Pts',(-13.5574387874792,1.39168909284562,0.05999335684464));
#60064=CARTESIAN_POINT('Ctrl Pts',(-13.4778951602621,0.701961934126549,
1.20318210469084));
#60065=CARTESIAN_POINT('Ctrl Pts',(-13.3983515330451,-0.632643424815839,
1.24103184127092));
#60066=CARTESIAN_POINT('Ctrl Pts',(-13.3426755178698,-1.15998664398442,
0.469511787720473));
#60067=CARTESIAN_POINT('Ctrl Pts',(-13.3135140451002,-1.17948347203477,
0.0397104053879535));
#60068=CARTESIAN_POINT('Ctrl Pts',(-13.3108671147362,-1.1792173683553,0.000673743327001138));
#60069=CARTESIAN_POINT('Ctrl Pts',(-13.7121328852639,-1.17893883534851,
0.000824692032647123));
#60070=CARTESIAN_POINT('Ctrl Pts',(-13.6890462567369,-1.17622805273099,
-0.339865495247411));
#60071=CARTESIAN_POINT('Ctrl Pts',(-13.6394450858043,-0.841480609154534,
-1.07647469321775));
#60072=CARTESIAN_POINT('Ctrl Pts',(-13.563329372466,0.410487983199367,-1.33112633468056));
#60073=CARTESIAN_POINT('Ctrl Pts',(-13.483785745249,1.34173269428113,-0.374367573820533));
#60074=CARTESIAN_POINT('Ctrl Pts',(-13.4042421180319,1.04035477583892,0.92631508873616));
#60075=CARTESIAN_POINT('Ctrl Pts',(-13.3246984908148,-0.216775987337669,
1.37601085553309));
#60076=CARTESIAN_POINT('Ctrl Pts',(-13.2606620798922,-1.06850277171503,
0.720365941468082));
#60077=CARTESIAN_POINT('Ctrl Pts',(-13.2231402113752,-1.17669017662013,
0.163992609232004));
#60078=CARTESIAN_POINT('Ctrl Pts',(-13.2121328852639,-1.17602842142206,
0.000530545984581809));
#60079=CARTESIAN_POINT('Origin',(-35.5608671147362,0.,0.));
#60080=CARTESIAN_POINT('',(-14.3108671147362,-1.17582483899281,-0.0001825003029064));
#60081=CARTESIAN_POINT('',(-14.2121328852639,-1.17864724066233,-0.000936392280242448));
#60082=CARTESIAN_POINT('',(-35.5608671147362,-1.17775,1.38253677383905E-12));
#60083=CARTESIAN_POINT('Ctrl Pts',(-14.3108671147362,-1.17582483899281,
-0.00018250030290639));
#60084=CARTESIAN_POINT('Ctrl Pts',(-14.2983552206351,-1.17608106896736,
-0.186068157712449));
#60085=CARTESIAN_POINT('Ctrl Pts',(-14.2593287841282,-1.04679940493409,
-0.765535917678041));
#60086=CARTESIAN_POINT('Ctrl Pts',(-14.1937878052157,-0.138420671057853,
-1.38608710109966));
#60087=CARTESIAN_POINT('Ctrl Pts',(-14.1142441779986,1.09119492379563,-0.865847199160223));
#60088=CARTESIAN_POINT('Ctrl Pts',(-14.0347005507816,1.31835186050876,0.449828974060237));
#60089=CARTESIAN_POINT('Ctrl Pts',(-13.9551569235645,0.334365665758747,
1.3522563867746));
#60090=CARTESIAN_POINT('Ctrl Pts',(-13.880545778216,-0.876730884968787,
1.03346810019051));
#60091=CARTESIAN_POINT('Ctrl Pts',(-13.8324491752733,-1.1753898855048,0.317905876834171));
#60092=CARTESIAN_POINT('Ctrl Pts',(-13.8108671147362,-1.1783086217086,-0.0010235987173));
#60093=CARTESIAN_POINT('Ctrl Pts',(-14.2121328852639,-1.17864724066233,
-0.00093639228024244));
#60094=CARTESIAN_POINT('Ctrl Pts',(-14.2079813869101,-1.1791799169808,-0.062239674349538));
#60095=CARTESIAN_POINT('Ctrl Pts',(-14.1773153461506,-1.14691406887258,
-0.514509039350729));
#60096=CARTESIAN_POINT('Ctrl Pts',(-14.1201347629855,-0.561271329354032,
-1.27490085813617));
#60097=CARTESIAN_POINT('Ctrl Pts',(-14.0405911357683,0.769041990499703,
-1.16145259054315));
#60098=CARTESIAN_POINT('Ctrl Pts',(-13.9610475085513,1.39285202204237,0.0189986295192388));
#60099=CARTESIAN_POINT('Ctrl Pts',(-13.8815038813343,0.737077133827655,
1.18199619374158));
#60100=CARTESIAN_POINT('Ctrl Pts',(-13.8019602541172,-0.595835576796184,
1.25911781365174));
#60101=CARTESIAN_POINT('Ctrl Pts',(-13.7455032554271,-1.15337493066883,
0.492856254368816));
#60102=CARTESIAN_POINT('Ctrl Pts',(-13.7155607991426,-1.17934133367546,
0.0514105374266761));
#60103=CARTESIAN_POINT('Ctrl Pts',(-13.7121328852639,-1.17893883534851,
0.000824692032647123));
#60104=CARTESIAN_POINT('Origin',(-35.5608671147362,0.,0.));
#60105=CARTESIAN_POINT('',(-14.8108671147362,-1.17763668317489,0.00108845679832357));
#60106=CARTESIAN_POINT('',(-14.7121328852639,-1.17590568010642,-0.000368259996795101));
#60107=CARTESIAN_POINT('',(-35.5608671147362,-1.17775,1.38253677383905E-12));
#60108=CARTESIAN_POINT('Ctrl Pts',(-14.8108671147362,-1.17763668317489,
0.00108845679832346));
#60109=CARTESIAN_POINT('Ctrl Pts',(-14.7907758084025,-1.1749081691312,-0.296246069770847));
#60110=CARTESIAN_POINT('Ctrl Pts',(-14.7441699596631,-0.90959503482556,
-0.990308665309722));
#60111=CARTESIAN_POINT('Ctrl Pts',(-14.6710495685181,0.25788080793157,-1.36890292676711));
#60112=CARTESIAN_POINT('Ctrl Pts',(-14.591505941301,1.2910033008695,-0.523171301922277));
#60113=CARTESIAN_POINT('Ctrl Pts',(-14.5119623140839,1.13810722973384,0.803187193397973));
#60114=CARTESIAN_POINT('Ctrl Pts',(-14.4324186868668,-0.0603448841024907,
1.39167389462245));
#60115=CARTESIAN_POINT('Ctrl Pts',(-14.365386953751,-1.02356777266643,0.810194735888077));
#60116=CARTESIAN_POINT('Ctrl Pts',(-14.3248697630407,-1.17553807999456,
0.207850868947047));
#60117=CARTESIAN_POINT('Ctrl Pts',(-14.3108671147362,-1.17582483899281,
-0.00018250030290639));
#60118=CARTESIAN_POINT('Ctrl Pts',(-14.7121328852639,-1.17590568010642,
-0.000368259996795066));
#60119=CARTESIAN_POINT('Ctrl Pts',(-14.7004019746775,-1.17639230734852,
-0.174621178730114));
#60120=CARTESIAN_POINT('Ctrl Pts',(-14.6621565216855,-1.05827983303723,
-0.742098214484146));
#60121=CARTESIAN_POINT('Ctrl Pts',(-14.5973965262878,-0.179164492855332,
-1.38141152005153));
#60122=CARTESIAN_POINT('Ctrl Pts',(-14.5178528990707,1.06523307257745,-0.897594677077771));
#60123=CARTESIAN_POINT('Ctrl Pts',(-14.4383092718537,1.33102260634132,0.410824201623429));
#60124=CARTESIAN_POINT('Ctrl Pts',(-14.3587656446366,0.37402865127972,1.34182721363559));
#60125=CARTESIAN_POINT('Ctrl Pts',(-14.2833735157734,-0.858697287164189,
1.05586726445034));
#60126=CARTESIAN_POINT('Ctrl Pts',(-14.2344959293158,-1.17577785159837,
0.329288476095253));
#60127=CARTESIAN_POINT('Ctrl Pts',(-14.2121328852639,-1.17864724066233,
-0.00093639228024244));
#60128=CARTESIAN_POINT('Origin',(-35.5608671147362,0.,0.));
#60129=CARTESIAN_POINT('',(-15.3108671147362,-1.17959567567971,-0.000315498773397984));
#60130=CARTESIAN_POINT('',(-15.2121328852639,-1.17729248913048,0.00106908369163515));
#60131=CARTESIAN_POINT('',(-35.5608671147362,-1.17775,1.38253677383905E-12));
#60132=CARTESIAN_POINT('Ctrl Pts',(-15.3108671147362,-1.17959567567971,
-0.000315498773397779));
#60133=CARTESIAN_POINT('Ctrl Pts',(-15.3097109385756,-1.17965635862726,
-0.017352186126931));
#60134=CARTESIAN_POINT('Ctrl Pts',(-15.2820402200094,-1.17159073736189,
-0.425031809757892));
#60135=CARTESIAN_POINT('Ctrl Pts',(-15.2278549590375,-0.70135401684535,
-1.20353657072225));
#60136=CARTESIAN_POINT('Ctrl Pts',(-15.1483113318204,0.633270292855629,
-1.24071208191002));
#60137=CARTESIAN_POINT('Ctrl Pts',(-15.0687677046033,1.38612202080006,-0.138070552487189));
#60138=CARTESIAN_POINT('Ctrl Pts',(-14.9892240773863,0.865571544712346,
1.09141359483712));
#60139=CARTESIAN_POINT('Ctrl Pts',(-14.9096804501692,-0.45016196450262,
1.31823819536764));
#60140=CARTESIAN_POINT('Ctrl Pts',(-14.8502281292859,-1.12446646376063,
0.582619075676667));
#60141=CARTESIAN_POINT('Ctrl Pts',(-14.8172903508082,-1.17850899528528,
0.0961469773735007));
#60142=CARTESIAN_POINT('Ctrl Pts',(-14.8108671147362,-1.17763668317489,
0.00108845679832346));
#60143=CARTESIAN_POINT('Ctrl Pts',(-15.2121328852639,-1.17729248913048,
0.00106908369163521));
#60144=CARTESIAN_POINT('Ctrl Pts',(-15.192822562445,-1.17477855836446,-0.284920221449956));
#60145=CARTESIAN_POINT('Ctrl Pts',(-15.1469976972204,-0.92600852840609,
-0.967511697806338));
#60146=CARTESIAN_POINT('Ctrl Pts',(-15.0746582895901,0.217471097610649,
-1.37590116830213));
#60147=CARTESIAN_POINT('Ctrl Pts',(-14.9951146623731,1.27504258996775,-0.560949282020663));
#60148=CARTESIAN_POINT('Ctrl Pts',(-14.915571035156,1.16125829983559,0.76933533929888));
#60149=CARTESIAN_POINT('Ctrl Pts',(-14.836027407939,-0.0193504518311904,
1.39284717871167));
#60150=CARTESIAN_POINT('Ctrl Pts',(-14.7682146913082,-1.0106905727704,0.833534035568003));
#60151=CARTESIAN_POINT('Ctrl Pts',(-14.7269165170832,-1.17529241842247,
0.219230293332935));
#60152=CARTESIAN_POINT('Ctrl Pts',(-14.7121328852639,-1.17590568010642,
-0.000368259996795066));
#60153=CARTESIAN_POINT('Origin',(-35.5608671147362,0.,0.));
#60154=CARTESIAN_POINT('',(-15.8108671147362,-1.1766794928373,-0.000931768368600377));
#60155=CARTESIAN_POINT('',(-15.7121328852639,-1.17968628694626,-0.000103984866668544));
#60156=CARTESIAN_POINT('',(-35.5608671147362,-1.17775,1.38253677383905E-12));
#60157=CARTESIAN_POINT('Ctrl Pts',(-15.8108671147362,-1.1766794928373,-0.000931768368600226));
#60158=CARTESIAN_POINT('Ctrl Pts',(-15.8021315263431,-1.17763401370504,
-0.130477870265945));
#60159=CARTESIAN_POINT('Ctrl Pts',(-15.7668813955443,-1.0980898693991,-0.652087136442379));
#60160=CARTESIAN_POINT('Ctrl Pts',(-15.7051167223398,-0.333682485522065,
-1.352425130226));
#60161=CARTESIAN_POINT('Ctrl Pts',(-15.6255730951227,0.957306810832643,
-1.011909780536));
#60162=CARTESIAN_POINT('Ctrl Pts',(-15.5460294679057,1.36883774453492,0.258226573279226));
#60163=CARTESIAN_POINT('Ctrl Pts',(-15.4664858406886,0.52284518846023,1.29113540843514));
#60164=CARTESIAN_POINT('Ctrl Pts',(-15.3880983896322,-0.78419642644012,
1.14013154729383));
#60165=CARTESIAN_POINT('Ctrl Pts',(-15.3362254809813,-1.17826471897844,
0.373349494719946));
#60166=CARTESIAN_POINT('Ctrl Pts',(-15.3108671147362,-1.17959567567971,
-0.000315498773397779));
#60167=CARTESIAN_POINT('Ctrl Pts',(-15.7121328852639,-1.17968628694626,
-0.000103984866668646));
#60168=CARTESIAN_POINT('Ctrl Pts',(-15.7117576926181,-1.17969324372913,
-0.0056314501573956));
#60169=CARTESIAN_POINT('Ctrl Pts',(-15.6848679575667,-1.17715074290506,
-0.401773567217293));
#60170=CARTESIAN_POINT('Ctrl Pts',(-15.6314636801096,-0.736479914837584,
-1.1823684020947));
#60171=CARTESIAN_POINT('Ctrl Pts',(-15.5519200528925,0.596471586267007,
-1.2588166466993));
#60172=CARTESIAN_POINT('Ctrl Pts',(-15.4723764256754,1.38145673145398,-0.178815553998048));
#60173=CARTESIAN_POINT('Ctrl Pts',(-15.3928327984584,0.897325579366346,
1.06545976359786));
#60174=CARTESIAN_POINT('Ctrl Pts',(-15.3132891712414,-0.41116039383583,
1.3309187930794));
#60175=CARTESIAN_POINT('Ctrl Pts',(-15.2530558668431,-1.11596639612747,
0.606070391443501));
#60176=CARTESIAN_POINT('Ctrl Pts',(-15.2193371048507,-1.17823037657205,
0.107764853257028));
#60177=CARTESIAN_POINT('Ctrl Pts',(-15.2121328852639,-1.17729248913048,
0.00106908369163521));
#60178=CARTESIAN_POINT('Origin',(-35.5608671147362,0.,0.));
#60179=CARTESIAN_POINT('',(-16.3108671147362,-1.17621668823985,0.000695152040889676));
#60180=CARTESIAN_POINT('',(-16.2121328852639,-1.17697909652625,-0.00101746427987839));
#60181=CARTESIAN_POINT('',(-35.5608671147362,-1.17775,1.38253677383905E-12));
#60182=CARTESIAN_POINT('Ctrl Pts',(-16.3108671147362,-1.17621668823985,
0.000695152040889723));
#60183=CARTESIAN_POINT('Ctrl Pts',(-16.2945521141105,-1.17491936293083,
-0.24149046014261));
#60184=CARTESIAN_POINT('Ctrl Pts',(-16.2517225710792,-0.983990797500948,
-0.879143553958332));
#60185=CARTESIAN_POINT('Ctrl Pts',(-16.1823784856422,0.061047927045359,
-1.39164323179989));
#60186=CARTESIAN_POINT('Ctrl Pts',(-16.1028348584251,1.20371368856048,-0.701049991072757));
#60187=CARTESIAN_POINT('Ctrl Pts',(-16.0232912312081,1.24055208348352,0.633583666279101));
#60188=CARTESIAN_POINT('Ctrl Pts',(-15.943747603991,0.13772042510721,1.3861568520623));
#60189=CARTESIAN_POINT('Ctrl Pts',(-15.872939565167,-0.956623033777217,
0.922497494227833));
#60190=CARTESIAN_POINT('Ctrl Pts',(-15.8286460687488,-1.17473682087889,
0.262724677481997));
#60191=CARTESIAN_POINT('Ctrl Pts',(-15.8108671147362,-1.1766794928373,-0.000931768368600226));
#60192=CARTESIAN_POINT('Ctrl Pts',(-16.2121328852639,-1.17697909652625,
-0.00101746427987831));
#60193=CARTESIAN_POINT('Ctrl Pts',(-16.2041782803856,-1.17794511640517,
-0.118906061450257));
#60194=CARTESIAN_POINT('Ctrl Pts',(-16.1697091331016,-1.10740950566883,
-0.628614928672698));
#60195=CARTESIAN_POINT('Ctrl Pts',(-16.1087254434119,-0.373350734627734,
-1.34201599550232));
#60196=CARTESIAN_POINT('Ctrl Pts',(-16.0291818161949,0.927103177787362,
-1.0396525385761));
#60197=CARTESIAN_POINT('Ctrl Pts',(-15.9496381889778,1.37584619300581,0.217818631945427));
#60198=CARTESIAN_POINT('Ctrl Pts',(-15.8700945617608,0.560627198897243,
1.27518424044833));
#60199=CARTESIAN_POINT('Ctrl Pts',(-15.7909261271894,-0.763354067122768,
1.16160221950801));
#60200=CARTESIAN_POINT('Ctrl Pts',(-15.7382722350238,-1.17920161385159,
0.384989780054453));
#60201=CARTESIAN_POINT('Ctrl Pts',(-15.7121328852639,-1.17968628694626,
-0.000103984866668646));
#60202=CARTESIAN_POINT('Origin',(-35.5608671147362,0.,0.));
#60203=CARTESIAN_POINT('',(-16.8108671147362,-1.17922610211458,0.000668052266892519));
#60204=CARTESIAN_POINT('',(-16.7121328852639,-1.17603382108715,0.000536316405655574));
#60205=CARTESIAN_POINT('',(-35.5608671147362,-1.17775,1.38253677383905E-12));
#60206=CARTESIAN_POINT('Ctrl Pts',(-16.8108671147362,-1.17922610211458,
0.000668052266892499));
#60207=CARTESIAN_POINT('Ctrl Pts',(-16.786972701878,-1.17684011432817,-0.351717469786626));
#60208=CARTESIAN_POINT('Ctrl Pts',(-16.7365637466141,-0.821676660253239,
-1.09930032789078));
#60209=CARTESIAN_POINT('Ctrl Pts',(-16.6596402489445,0.450827859201633,
-1.31801061277163));
#60210=CARTESIAN_POINT('Ctrl Pts',(-16.5800966217275,1.35250937252205,-0.333340863458119));
#60211=CARTESIAN_POINT('Ctrl Pts',(-16.5005529945104,1.01166794046017,0.957562380347131));
#60212=CARTESIAN_POINT('Ctrl Pts',(-16.4210093672934,-0.258572322151341,
1.36877247496735));
#60213=CARTESIAN_POINT('Ctrl Pts',(-16.3577807407019,-1.07945384177108,
0.696092032679032));
#60214=CARTESIAN_POINT('Ctrl Pts',(-16.3210666565162,-1.17702772858213,
0.152100740472336));
#60215=CARTESIAN_POINT('Ctrl Pts',(-16.3108671147362,-1.17621668823985,
0.000695152040889723));
#60216=CARTESIAN_POINT('Ctrl Pts',(-16.7121328852639,-1.17603382108715,
0.000536316405655504));
#60217=CARTESIAN_POINT('Ctrl Pts',(-16.696598868153,-1.1750895157582,-0.230145806328667));
#60218=CARTESIAN_POINT('Ctrl Pts',(-16.6545503086365,-0.997850008706123,
-0.855911651981158));
#60219=CARTESIAN_POINT('Ctrl Pts',(-16.5859872067143,0.0200540927288029,
-1.39283722544883));
#60220=CARTESIAN_POINT('Ctrl Pts',(-16.5064435794972,1.18255439311996,-0.736181234849029));
#60221=CARTESIAN_POINT('Ctrl Pts',(-16.4268999522802,1.25866594274463,0.596789533927942));
#60222=CARTESIAN_POINT('Ctrl Pts',(-16.3473563250631,0.17846660373185,1.38150185471594));
#60223=CARTESIAN_POINT('Ctrl Pts',(-16.2757673027243,-0.941267299997083,
0.945502442243397));
#60224=CARTESIAN_POINT('Ctrl Pts',(-16.2306928227913,-1.17472514816837,
0.274043966445028));
#60225=CARTESIAN_POINT('Ctrl Pts',(-16.2121328852639,-1.17697909652625,
-0.00101746427987831));
#60226=CARTESIAN_POINT('Origin',(-35.5608671147362,0.,0.));
#60227=CARTESIAN_POINT('',(-17.3108671147362,-1.17829670657796,-0.00102595198748888));
#60228=CARTESIAN_POINT('',(-17.2121328852639,-1.17894908727537,0.000820014261101384));
#60229=CARTESIAN_POINT('',(-35.5608671147362,-1.17775,1.38253677383905E-12));
#60230=CARTESIAN_POINT('Ctrl Pts',(-17.3108671147362,-1.17829670657796,
-0.00102595198748913));
#60231=CARTESIAN_POINT('Ctrl Pts',(-17.3059078320511,-1.17896815298064,
-0.0743137955243832));
#60232=CARTESIAN_POINT('Ctrl Pts',(-17.2744340069604,-1.13931306984172,
-0.538706691640527));
#60233=CARTESIAN_POINT('Ctrl Pts',(-17.2164456394639,-0.522192861480347,
-1.29139937642464));
#60234=CARTESIAN_POINT('Ctrl Pts',(-17.1369020122469,0.804049392182112,
-1.13749826766574));
#60235=CARTESIAN_POINT('Ctrl Pts',(-17.0573583850298,1.39162776720246,0.0613994426854746));
#60236=CARTESIAN_POINT('Ctrl Pts',(-16.9778147578128,0.700745920571368,
1.20389072959865));
#60237=CARTESIAN_POINT('Ctrl Pts',(-16.8982711305957,-0.63389699927829,
1.24039200590658));
#60238=CARTESIAN_POINT('Ctrl Pts',(-16.8426219162368,-1.16020695868756,
0.468711179705086));
#60239=CARTESIAN_POINT('Ctrl Pts',(-16.8134872442837,-1.17948773637762,
0.0393087053733596));
#60240=CARTESIAN_POINT('Ctrl Pts',(-16.8108671147362,-1.17922610211458,
0.000668052266892499));
#60241=CARTESIAN_POINT('Ctrl Pts',(-17.2121328852639,-1.17894908727537,
0.000820014261101471));
#60242=CARTESIAN_POINT('Ctrl Pts',(-17.1890194559205,-1.17624647302594,
-0.340257924082543));
#60243=CARTESIAN_POINT('Ctrl Pts',(-17.1393914841714,-0.84083346165202,
-1.07723512885116));
#60244=CARTESIAN_POINT('Ctrl Pts',(-17.0632489700166,0.411832699539931,
-1.33071091181399));
#60245=CARTESIAN_POINT('Ctrl Pts',(-16.9837053427996,1.34211025800256,-0.373011740559811));
#60246=CARTESIAN_POINT('Ctrl Pts',(-16.9041617155825,1.03941832680352,0.927365755856943));
#60247=CARTESIAN_POINT('Ctrl Pts',(-16.8246180883655,-0.218166152382787,
1.37579112992694));
#60248=CARTESIAN_POINT('Ctrl Pts',(-16.7606084782593,-1.06887386894006,
0.719560757628652));
#60249=CARTESIAN_POINT('Ctrl Pts',(-16.7231134105587,-1.17670132186795,
0.163598508604886));
#60250=CARTESIAN_POINT('Ctrl Pts',(-16.7121328852639,-1.17603382108715,
0.000536316405655504));
#60251=CARTESIAN_POINT('Origin',(-35.5608671147362,0.,0.));
#60252=CARTESIAN_POINT('',(-17.8108671147362,-1.17582304073982,-0.000175995329426161));
#60253=CARTESIAN_POINT('',(-17.7121328852639,-1.17863596349438,-0.000939971812119189));
#60254=CARTESIAN_POINT('',(-35.5608671147362,-1.17775,1.38253677383905E-12));
#60255=CARTESIAN_POINT('Ctrl Pts',(-17.8108671147362,-1.17582304073982,
-0.000175995329426085));
#60256=CARTESIAN_POINT('Ctrl Pts',(-17.7983284198186,-1.17607064606856,
-0.186460535126324));
#60257=CARTESIAN_POINT('Ctrl Pts',(-17.7592751824953,-1.0463971061925,-0.766339799844726));
#60258=CARTESIAN_POINT('Ctrl Pts',(-17.6937074027663,-0.137020144008901,
-1.38622624926336));
#60259=CARTESIAN_POINT('Ctrl Pts',(-17.6141637755493,1.09206919009568,-0.864744250084811));
#60260=CARTESIAN_POINT('Ctrl Pts',(-17.5346201483322,1.31789669533126,0.451160763415784));
#60261=CARTESIAN_POINT('Ctrl Pts',(-17.4550765211151,0.332999220126171,
1.35259352852449));
#60262=CARTESIAN_POINT('Ctrl Pts',(-17.3804921765831,-0.877339701365798,
1.0326967032482));
#60263=CARTESIAN_POINT('Ctrl Pts',(-17.3324223744568,-1.17537830032499,
0.317515781186765));
#60264=CARTESIAN_POINT('Ctrl Pts',(-17.3108671147362,-1.17829670657796,
-0.00102595198748913));
#60265=CARTESIAN_POINT('Ctrl Pts',(-17.7121328852639,-1.17863596349438,
-0.000939971812119285));
#60266=CARTESIAN_POINT('Ctrl Pts',(-17.7079545860936,-1.17917341164053,
-0.062640541617889));
#60267=CARTESIAN_POINT('Ctrl Pts',(-17.6772617445177,-1.14666849415385,
-0.515311458828749));
#60268=CARTESIAN_POINT('Ctrl Pts',(-17.6200543605361,-0.559982925362541,
-1.27546729732031));
#60269=CARTESIAN_POINT('Ctrl Pts',(-17.540510733319,0.770215091108087,-1.16067498321473));
#60270=CARTESIAN_POINT('Ctrl Pts',(-17.460967106102,1.39283211551731,0.0204059112696104));
#60271=CARTESIAN_POINT('Ctrl Pts',(-17.3814234788849,0.735882507890194,
1.18274030869519));
#60272=CARTESIAN_POINT('Ctrl Pts',(-17.3018798516679,-0.597107443512156,
1.25851515848381));
#60273=CARTESIAN_POINT('Ctrl Pts',(-17.2454496537941,-1.15360800458277,
0.492054691869927));
#60274=CARTESIAN_POINT('Ctrl Pts',(-17.2155339983262,-1.17934677368052,
0.0510092187330667));
#60275=CARTESIAN_POINT('Ctrl Pts',(-17.2121328852639,-1.17894908727537,
0.000820014261101471));
#60276=CARTESIAN_POINT('Origin',(-35.5608671147362,0.,0.));
#60277=CARTESIAN_POINT('',(-18.3108671147362,-1.17764870709862,0.00108847900253356));
#60278=CARTESIAN_POINT('',(-18.2121328852639,-1.17590200433377,-0.000362038225872191));
#60279=CARTESIAN_POINT('',(-35.5608671147362,-1.17775,1.38253677383905E-12));
#60280=CARTESIAN_POINT('Ctrl Pts',(-18.3108671147362,-1.17764870709862,
0.00108847900253358));
#60281=CARTESIAN_POINT('Ctrl Pts',(-18.290749007586,-1.17491403845395,-0.296634920545634));
#60282=CARTESIAN_POINT('Ctrl Pts',(-18.2441163580302,-0.909022050445814,
-0.991088850735009));
#60283=CARTESIAN_POINT('Ctrl Pts',(-18.1709691660687,0.259263770380752,
-1.36864167384269));
#60284=CARTESIAN_POINT('Ctrl Pts',(-18.0914255388516,1.29153123683166,-0.521866648004122));
#60285=CARTESIAN_POINT('Ctrl Pts',(-18.0118819116345,1.13729513514176,0.804336689200407));
#60286=CARTESIAN_POINT('Ctrl Pts',(-17.9323382844175,-0.0617509544081363,
1.39161221381557));
#60287=CARTESIAN_POINT('Ctrl Pts',(-17.865333352118,-1.02400096068858,0.809393021075806));
#60288=CARTESIAN_POINT('Ctrl Pts',(-17.8248429622243,-1.17554705553286,
0.207459993479165));
#60289=CARTESIAN_POINT('Ctrl Pts',(-17.8108671147362,-1.17582304073982,
-0.000175995329426085));
#60290=CARTESIAN_POINT('Ctrl Pts',(-18.2121328852639,-1.17590200433377,
-0.00036203822587207));
#60291=CARTESIAN_POINT('Ctrl Pts',(-18.2003751738611,-1.17638141866479,
-0.175014423114699));
#60292=CARTESIAN_POINT('Ctrl Pts',(-18.1621029200526,-1.05789358902536,
-0.742902875494098));
#60293=CARTESIAN_POINT('Ctrl Pts',(-18.0973161238384,-0.177768669061831,
-1.38159183680678));
#60294=CARTESIAN_POINT('Ctrl Pts',(-18.0177724966214,1.06613942872675,-0.896517942790525));
#60295=CARTESIAN_POINT('Ctrl Pts',(-17.9382288694043,1.33060684382376,0.412168812988731));
#60296=CARTESIAN_POINT('Ctrl Pts',(-17.8586852421873,0.372672722692757,
1.34220443487269));
#60297=CARTESIAN_POINT('Ctrl Pts',(-17.7833199141404,-0.85932554870962,
1.05510122363174));
#60298=CARTESIAN_POINT('Ctrl Pts',(-17.7344691284993,-1.17576288714689,
0.328897332505749));
#60299=CARTESIAN_POINT('Ctrl Pts',(-17.7121328852639,-1.17863596349438,
-0.000939971812119285));
#60300=CARTESIAN_POINT('Origin',(-35.5608671147362,0.,0.));
#60301=CARTESIAN_POINT('',(-18.8108671147362,-1.17959109088123,-0.000322554745341552));
#60302=CARTESIAN_POINT('',(-18.7121328852639,-1.17730404743425,0.00107034009675953));
#60303=CARTESIAN_POINT('',(-35.5608671147362,-1.17775,1.38253677383905E-12));
#60304=CARTESIAN_POINT('Ctrl Pts',(-18.8108671147362,-1.17959109088123,
-0.000322554745341669));
#60305=CARTESIAN_POINT('Ctrl Pts',(-18.8096841377592,-1.17965442875519,
-0.0177543430943377));
#60306=CARTESIAN_POINT('Ctrl Pts',(-18.7819866183765,-1.17139367616527,
-0.425830504643864));
#60307=CARTESIAN_POINT('Ctrl Pts',(-18.7277745565881,-0.700137645459773,
-1.20424458122967));
#60308=CARTESIAN_POINT('Ctrl Pts',(-18.648230929371,0.63452354392386,-1.24007161334226));
#60309=CARTESIAN_POINT('Ctrl Pts',(-18.5686873021539,1.38626081519776,-0.136669990335221));
#60310=CARTESIAN_POINT('Ctrl Pts',(-18.4891436749369,0.864468374839663,
1.09228758251344));
#60311=CARTESIAN_POINT('Ctrl Pts',(-18.4096000477198,-0.451493638844702,
1.31778269380568));
#60312=CARTESIAN_POINT('Ctrl Pts',(-18.3501745276529,-1.12475091080895,
0.581814575175766));
#60313=CARTESIAN_POINT('Ctrl Pts',(-18.3172635499917,-1.17851817910214,
0.0957479037213191));
#60314=CARTESIAN_POINT('Ctrl Pts',(-18.3108671147362,-1.17764870709862,
0.00108847900253358));
#60315=CARTESIAN_POINT('Ctrl Pts',(-18.7121328852639,-1.17730404743425,
0.00107034009675942));
#60316=CARTESIAN_POINT('Ctrl Pts',(-18.6927957616285,-1.1747817166967,-0.285308750994182));
#60317=CARTESIAN_POINT('Ctrl Pts',(-18.6469440955875,-0.925454311140779,
-0.968295937334803));
#60318=CARTESIAN_POINT('Ctrl Pts',(-18.5745778871408,0.21886115147667,-1.37568074043561));
#60319=CARTESIAN_POINT('Ctrl Pts',(-18.4950342599237,1.27560870369364,-0.55966073499237));
#60320=CARTESIAN_POINT('Ctrl Pts',(-18.4154906327066,1.16048039621642,0.770508243452683));
#60321=CARTESIAN_POINT('Ctrl Pts',(-18.3359470054896,-0.0207577285084573,
1.39282691671949));
#60322=CARTESIAN_POINT('Ctrl Pts',(-18.2681610896753,-1.01114065994669,
0.832733888360385));
#60323=CARTESIAN_POINT('Ctrl Pts',(-18.2268897162668,-1.17530030252116,
0.21884012108592));
#60324=CARTESIAN_POINT('Ctrl Pts',(-18.2121328852639,-1.17590200433377,
-0.00036203822587207));
#60325=CARTESIAN_POINT('Origin',(-35.5608671147362,0.,0.));
#60326=CARTESIAN_POINT('',(-19.3108671147362,-1.17666978654916,-0.000928285457528838));
#60327=CARTESIAN_POINT('',(-19.2121328852639,-1.17968463629076,-0.000111381752591205));
#60328=CARTESIAN_POINT('',(-35.5608671147362,-1.17775,1.38253677383905E-12));
#60329=CARTESIAN_POINT('Ctrl Pts',(-19.3108671147362,-1.17666978654916,
-0.000928285457529009));
#60330=CARTESIAN_POINT('Ctrl Pts',(-19.3021047255266,-1.17762313276549,
-0.130874534662354));
#60331=CARTESIAN_POINT('Ctrl Pts',(-19.2668277939114,-1.09776245886893,
-0.652892723031988));
#60332=CARTESIAN_POINT('Ctrl Pts',(-19.2050363198904,-0.332315869745427,
-1.35276158162712));
#60333=CARTESIAN_POINT('Ctrl Pts',(-19.1254926926734,0.958328722255644,
-1.0109420330122));
#60334=CARTESIAN_POINT('Ctrl Pts',(-19.0459490654563,1.36857614229396,0.25960946969393));
#60335=CARTESIAN_POINT('Ctrl Pts',(-18.9664054382392,0.521540401231442,
1.29166301483565));
#60336=CARTESIAN_POINT('Ctrl Pts',(-18.8880447879992,-0.78490114965271,
1.13939071929856));
#60337=CARTESIAN_POINT('Ctrl Pts',(-18.8361986801649,-1.1782348113175,0.372951393674192));
#60338=CARTESIAN_POINT('Ctrl Pts',(-18.8108671147362,-1.17959109088123,
-0.000322554745341669));
#60339=CARTESIAN_POINT('Ctrl Pts',(-19.2121328852639,-1.17968463629076,
-0.000111381752591032));
#60340=CARTESIAN_POINT('Ctrl Pts',(-19.2117308918017,-1.17969259990424,
-0.00603370807851372));
#60341=CARTESIAN_POINT('Ctrl Pts',(-19.1848143559338,-1.17696574873875,
-0.402571200060254));
#60342=CARTESIAN_POINT('Ctrl Pts',(-19.1313832776602,-0.735284913137964,
-1.18311191344811));
#60343=CARTESIAN_POINT('Ctrl Pts',(-19.0518396504431,0.597743148369296,
-1.25821334908223));
#60344=CARTESIAN_POINT('Ctrl Pts',(-18.9722960232261,1.38163669562993,-0.177419684702549));
#60345=CARTESIAN_POINT('Ctrl Pts',(-18.892752396009,0.896248616175358,1.06636584774406));
#60346=CARTESIAN_POINT('Ctrl Pts',(-18.813208768792,-0.412504900140071,
1.33050269093737));
#60347=CARTESIAN_POINT('Ctrl Pts',(-18.7530022652102,-1.1162649024249,0.605265384768711));
#60348=CARTESIAN_POINT('Ctrl Pts',(-18.7193103040342,-1.17824026857666,
0.107366535052814));
#60349=CARTESIAN_POINT('Ctrl Pts',(-18.7121328852639,-1.17730404743425,
0.00107034009675942));
#60350=CARTESIAN_POINT('Origin',(-35.5608671147362,0.,0.));
#60351=CARTESIAN_POINT('',(-19.8108671147362,-1.17622381119946,0.000700251168187343));
#60352=CARTESIAN_POINT('',(-19.7121328852639,-1.17696832030681,-0.00101504787385631));
#60353=CARTESIAN_POINT('',(-35.5608671147362,-1.17775,1.38253677383905E-12));
#60354=CARTESIAN_POINT('Ctrl Pts',(-19.8108671147362,-1.17622381119946,
0.000700251168187383));
#60355=CARTESIAN_POINT('Ctrl Pts',(-19.7945253132941,-1.17491434676118,
-0.2418795226269));
#60356=CARTESIAN_POINT('Ctrl Pts',(-19.7516689694463,-0.983506135042355,
-0.879939628894577));
#60357=CARTESIAN_POINT('Ctrl Pts',(-19.6822980831928,0.0624539660114313,
-1.3915808406774));
#60358=CARTESIAN_POINT('Ctrl Pts',(-19.6027544559757,1.20442139179994,-0.699833440888375));
#60359=CARTESIAN_POINT('Ctrl Pts',(-19.5232108287587,1.23991129837533,0.634836755530266));
#60360=CARTESIAN_POINT('Ctrl Pts',(-19.4436672015416,0.13631982794163,1.38629529268513));
#60361=CARTESIAN_POINT('Ctrl Pts',(-19.3728859635341,-0.95714057527515,
0.921706396515711));
#60362=CARTESIAN_POINT('Ctrl Pts',(-19.3286192679323,-1.17473835578566,
0.262336181341884));
#60363=CARTESIAN_POINT('Ctrl Pts',(-19.3108671147362,-1.17666978654916,
-0.000928285457529009));
#60364=CARTESIAN_POINT('Ctrl Pts',(-19.7121328852639,-1.17696832030681,
-0.00101504787385635));
#60365=CARTESIAN_POINT('Ctrl Pts',(-19.7041514795691,-1.17793465627579,
-0.119303575573876));
#60366=CARTESIAN_POINT('Ctrl Pts',(-19.6696555314687,-1.10709672596639,
-0.629420301679817));
#60367=CARTESIAN_POINT('Ctrl Pts',(-19.6086450409626,-0.371994615647838,
-1.3423925316986));
#60368=CARTESIAN_POINT('Ctrl Pts',(-19.5291014137455,0.928153134988703,
-1.03871529364008));
#60369=CARTESIAN_POINT('Ctrl Pts',(-19.4495577865284,1.37562541403019,0.219208630088832));
#60370=CARTESIAN_POINT('Ctrl Pts',(-19.3700141593114,0.55933850891441,1.27575002867982));
#60371=CARTESIAN_POINT('Ctrl Pts',(-19.2908725255565,-0.764079154747326,
1.16086926264095));
#60372=CARTESIAN_POINT('Ctrl Pts',(-19.2382454342073,-1.17916733870663,
0.384588994216886));
#60373=CARTESIAN_POINT('Ctrl Pts',(-19.2121328852639,-1.17968463629076,
-0.000111381752591032));
#60374=CARTESIAN_POINT('Origin',(-35.5608671147362,0.,0.));
#60375=CARTESIAN_POINT('',(-20.3108671147362,-1.17923477537134,0.000662329376658134));
#60376=CARTESIAN_POINT('',(-20.2121328852639,-1.17603928037595,0.000542067565237406));
#60377=CARTESIAN_POINT('',(-35.5608671147362,-1.17775,1.38253677383905E-12));
#60378=CARTESIAN_POINT('Ctrl Pts',(-20.3108671147362,-1.17923477537134,
0.000662329376658151));
#60379=CARTESIAN_POINT('Ctrl Pts',(-20.2869459010615,-1.17686247573691,
-0.35211161007433));
#60380=CARTESIAN_POINT('Ctrl Pts',(-20.2365101449812,-0.821008972712208,
-1.10005420902622));
#60381=CARTESIAN_POINT('Ctrl Pts',(-20.1595598464952,0.452159303261918,
-1.31755443852794));
#60382=CARTESIAN_POINT('Ctrl Pts',(-20.0800162192781,1.35284547871658,-0.331974162740232));
#60383=CARTESIAN_POINT('Ctrl Pts',(-20.0004725920611,1.01069993484086,0.958584047292498));
#60384=CARTESIAN_POINT('Ctrl Pts',(-19.920928964844,-0.259955152443364,
1.36851052342652));
#60385=CARTESIAN_POINT('Ctrl Pts',(-19.857727139069,-1.07980893901382,0.695286514566635));
#60386=CARTESIAN_POINT('Ctrl Pts',(-19.8210398556998,-1.17703895037361,
0.151705708587368));
#60387=CARTESIAN_POINT('Ctrl Pts',(-19.8108671147362,-1.17622381119946,
0.000700251168187383));
#60388=CARTESIAN_POINT('Ctrl Pts',(-20.2121328852639,-1.17603928037595,
0.000542067565237423));
#60389=CARTESIAN_POINT('Ctrl Pts',(-20.1965720673366,-1.17508294569432,
-0.230535369896458));
#60390=CARTESIAN_POINT('Ctrl Pts',(-20.1544967070036,-0.997382817803285,
-0.856709931464427));
#60391=CARTESIAN_POINT('Ctrl Pts',(-20.0859068042649,0.0214613589905084,
-1.39281625252631));
#60392=CARTESIAN_POINT('Ctrl Pts',(-20.0063631770478,1.1832976026021,-0.734986045382691));
#60393=CARTESIAN_POINT('Ctrl Pts',(-19.9268195498308,1.25806232396071,0.598060943601679));
#60394=CARTESIAN_POINT('Ctrl Pts',(-19.8472759226137,0.177070689023417,
1.38168146630109));
#60395=CARTESIAN_POINT('Ctrl Pts',(-19.7757137010914,-0.941803093652268,
0.94471458317044));
#60396=CARTESIAN_POINT('Ctrl Pts',(-19.7306660219748,-1.17472445032866,
0.27365554763835));
#60397=CARTESIAN_POINT('Ctrl Pts',(-19.7121328852639,-1.17696832030681,
-0.00101504787385635));
#60398=CARTESIAN_POINT('Origin',(-35.5608671147362,0.,0.));
#60399=CARTESIAN_POINT('',(-20.8108671147362,-1.17828477702325,-0.00102826220839124));
#60400=CARTESIAN_POINT('',(-20.7121328852639,-1.17895929484358,0.00081529925158268));
#60401=CARTESIAN_POINT('',(-35.5608671147362,-1.17775,1.38253677383905E-12));
#60402=CARTESIAN_POINT('Ctrl Pts',(-20.8108671147362,-1.17828477702325,
-0.00102826220839125));
#60403=CARTESIAN_POINT('Ctrl Pts',(-20.8058810312347,-1.17896058675312,
-0.0747140894821463));
#60404=CARTESIAN_POINT('Ctrl Pts',(-20.7743804053275,-1.13905376627765,
-0.539509952836493));
#60405=CARTESIAN_POINT('Ctrl Pts',(-20.7163652370146,-0.520887807880025,
-1.29192632360089));
#60406=CARTESIAN_POINT('Ctrl Pts',(-20.6368216097975,0.80519827226939,-1.13668530224745));
#60407=CARTESIAN_POINT('Ctrl Pts',(-20.5572779825804,1.39156502092812,0.06280546584721));
#60408=CARTESIAN_POINT('Ctrl Pts',(-20.4777343553634,0.699529191665802,
1.20459812552501));
#60409=CARTESIAN_POINT('Ctrl Pts',(-20.3981907281463,-0.635149926632454,
1.23975090429883));
#60410=CARTESIAN_POINT('Ctrl Pts',(-20.3425683146039,-1.16042683999627,
0.467910605410006));
#60411=CARTESIAN_POINT('Ctrl Pts',(-20.3134604434672,-1.17949195934555,
0.0389069939316387));
#60412=CARTESIAN_POINT('Ctrl Pts',(-20.3108671147362,-1.17923477537134,
0.000662329376658151));
#60413=CARTESIAN_POINT('Ctrl Pts',(-20.7121328852639,-1.17895929484358,
0.000815299251582628));
#60414=CARTESIAN_POINT('Ctrl Pts',(-20.688992655104,-1.17626502045395,-0.340650404120654));
#60415=CARTESIAN_POINT('Ctrl Pts',(-20.6393378825385,-0.84018563607975,
-1.07799535577281));
#60416=CARTESIAN_POINT('Ctrl Pts',(-20.5631685675673,0.413176995464697,
-1.3302941305027));
#60417=CARTESIAN_POINT('Ctrl Pts',(-20.4836249403502,1.34248645164237,-0.371655526513227));
#60418=CARTESIAN_POINT('Ctrl Pts',(-20.4040813131332,1.03848081668687,0.928415476284475));
#60419=CARTESIAN_POINT('Ctrl Pts',(-20.3245376859161,-0.219556094714919,
1.37556999985631));
#60420=CARTESIAN_POINT('Ctrl Pts',(-20.2605548766263,-1.06924443023848,
0.718755558999398));
#60421=CARTESIAN_POINT('Ctrl Pts',(-20.2230866097423,-1.17671247292024,
0.163204377153041));
#60422=CARTESIAN_POINT('Ctrl Pts',(-20.2121328852639,-1.17603928037595,
0.000542067565237423));
#60423=CARTESIAN_POINT('Origin',(-35.5608671147362,0.,0.));
#60424=CARTESIAN_POINT('',(-21.3108671147362,-1.17582130790704,-0.000169484100476859));
#60425=CARTESIAN_POINT('',(-21.2121328852639,-1.17862465731635,-0.000943510414042614));
#60426=CARTESIAN_POINT('',(-35.5608671147362,-1.17775,1.38253677383905E-12));
#60427=CARTESIAN_POINT('Ctrl Pts',(-21.3108671147362,-1.17582130790704,
-0.000169484100476808));
#60428=CARTESIAN_POINT('Ctrl Pts',(-21.2983016190021,-1.17606024285316,
-0.186852883416342));
#60429=CARTESIAN_POINT('Ctrl Pts',(-21.2592215808624,-1.04599425125585,
-0.767143650822197));
#60430=CARTESIAN_POINT('Ctrl Pts',(-21.1936270003169,-0.135619477084131,
-1.38636398230999));
#60431=CARTESIAN_POINT('Ctrl Pts',(-21.1140833730999,1.09294234156633,-0.863640418242735));
#60432=CARTESIAN_POINT('Ctrl Pts',(-21.0345397458828,1.31744018479035,0.452492092207748));
#60433=CARTESIAN_POINT('Ctrl Pts',(-20.9549961186657,0.331632434554235,
1.352929289491));
#60434=CARTESIAN_POINT('Ctrl Pts',(-20.8804385749502,-0.877947854422183,
1.03192513093976));
#60435=CARTESIAN_POINT('Ctrl Pts',(-20.8323955736404,-1.17536682709477,
0.317125716520315));
#60436=CARTESIAN_POINT('Ctrl Pts',(-20.8108671147362,-1.17828477702325,
-0.00102826220839125));
#60437=CARTESIAN_POINT('Ctrl Pts',(-21.2121328852639,-1.17862465731635,
-0.00094351041404258));
#60438=CARTESIAN_POINT('Ctrl Pts',(-21.2079277852772,-1.17916686958785,
-0.0630413912822054));
#60439=CARTESIAN_POINT('Ctrl Pts',(-21.1772081428848,-1.14642246849581,
-0.516113907661345));
#60440=CARTESIAN_POINT('Ctrl Pts',(-21.1199739580867,-0.558693949717291,
-1.27603243445472));
#60441=CARTESIAN_POINT('Ctrl Pts',(-21.0404303308696,0.771387405449101,
-1.15989619102127));
#60442=CARTESIAN_POINT('Ctrl Pts',(-20.9608867036526,1.39281078713163,0.0218131721888098));
#60443=CARTESIAN_POINT('Ctrl Pts',(-20.8813430764355,0.734687130733419,
1.18348321625862));
#60444=CARTESIAN_POINT('Ctrl Pts',(-20.8017994492184,-0.598378700676205,
1.25791121857157));
#60445=CARTESIAN_POINT('Ctrl Pts',(-20.7453960521612,-1.15384063643505,
0.491253161147155));
#60446=CARTESIAN_POINT('Ctrl Pts',(-20.7155071975097,-1.17935217438729,
0.050607885430154));
#60447=CARTESIAN_POINT('Ctrl Pts',(-20.7121328852639,-1.17895929484358,
0.000815299251582628));
#60448=CARTESIAN_POINT('Origin',(-35.5608671147362,0.,0.));
#60449=CARTESIAN_POINT('',(-21.8108671147362,-1.17766074088617,0.00108845803827099));
#60450=CARTESIAN_POINT('',(-21.7121328852638,-1.17589839182392,-0.00035580353738629));
#60451=CARTESIAN_POINT('',(-35.5608671147362,-1.17775,1.38253677383905E-12));
#60452=CARTESIAN_POINT('Ctrl Pts',(-21.8108671147362,-1.17766074088617,
0.00108845803827095));
#60453=CARTESIAN_POINT('Ctrl Pts',(-21.7907222067696,-1.17492000502449,
-0.297023786339216));
#60454=CARTESIAN_POINT('Ctrl Pts',(-21.7440627563973,-0.908448417634372,
-0.991868889400734));
#60455=CARTESIAN_POINT('Ctrl Pts',(-21.6708887636193,0.260646468162729,
-1.36837902375229));
#60456=CARTESIAN_POINT('Ctrl Pts',(-21.5913451364022,1.29205785434534,-0.520561461342927));
#60457=CARTESIAN_POINT('Ctrl Pts',(-21.5118015091852,1.13648187955178,0.805485363902682));
#60458=CARTESIAN_POINT('Ctrl Pts',(-21.4322578819681,-0.0631569616758272,
1.3915491123934));
#60459=CARTESIAN_POINT('Ctrl Pts',(-21.3652797504851,-1.02443357395186,
0.808591257748514));
#60460=CARTESIAN_POINT('Ctrl Pts',(-21.3248161614078,-1.17555606451471,
0.207069092473432));
#60461=CARTESIAN_POINT('Ctrl Pts',(-21.3108671147362,-1.17582130790704,
-0.000169484100476808));
#60462=CARTESIAN_POINT('Ctrl Pts',(-21.7121328852638,-1.17589839182392,
-0.000355803537386394));
#60463=CARTESIAN_POINT('Ctrl Pts',(-21.7003483730446,-1.17637054255772,
-0.175407637251437));
#60464=CARTESIAN_POINT('Ctrl Pts',(-21.6620493184196,-1.05750679897208,
-0.743707513842047));
#60465=CARTESIAN_POINT('Ctrl Pts',(-21.5972357213891,-0.176372663794721,
-1.38177074317598));
#60466=CARTESIAN_POINT('Ctrl Pts',(-21.517692094172,1.06704469651685,-0.895440293300685));
#60467=CARTESIAN_POINT('Ctrl Pts',(-21.4381484669549,1.33018972296772,0.413513003595081));
#60468=CARTESIAN_POINT('Ctrl Pts',(-21.3586048397379,0.371316413666049,
1.34258028593203));
#60469=CARTESIAN_POINT('Ctrl Pts',(-21.2832663125075,-0.859953139331574,
1.05433499103261));
#60470=CARTESIAN_POINT('Ctrl Pts',(-21.2344423276828,-1.17574804237543,
0.328506229651944));
#60471=CARTESIAN_POINT('Ctrl Pts',(-21.2121328852639,-1.17862465731635,
-0.00094351041404258));
#60472=CARTESIAN_POINT('Origin',(-35.5608671147362,0.,0.));
#60473=CARTESIAN_POINT('',(-22.3108671147362,-1.17958641441151,-0.000329593618060359));
#60474=CARTESIAN_POINT('',(-22.2121328852638,-1.17731562723721,0.00107155510022959));
#60475=CARTESIAN_POINT('',(-35.5608671147362,-1.17775,1.38253677383905E-12));
#60476=CARTESIAN_POINT('Ctrl Pts',(-22.3108671147362,-1.17958641441151,
-0.000329593618060599));
#60477=CARTESIAN_POINT('Ctrl Pts',(-22.3096573369427,-1.17965245508073,
-0.0181564948118189));
#60478=CARTESIAN_POINT('Ctrl Pts',(-22.2819330167435,-1.17119619678948,
-0.426629235604552));
#60479=CARTESIAN_POINT('Ctrl Pts',(-22.2276941541387,-0.69892055934474,
-1.20495136239444));
#60480=CARTESIAN_POINT('Ctrl Pts',(-22.1481505269216,0.635776147244211,
-1.23942987885813));
#60481=CARTESIAN_POINT('Ctrl Pts',(-22.0686068997046,1.38639819444309,-0.135269288664905));
#60482=CARTESIAN_POINT('Ctrl Pts',(-21.9890632724875,0.863364322481949,
1.09316045513743));
#60483=CARTESIAN_POINT('Ctrl Pts',(-21.9095196452704,-0.4528248522834,1.31732584699667));
#60484=CARTESIAN_POINT('Ctrl Pts',(-21.85012092602,-1.12503488038791,0.581010094305927));
#60485=CARTESIAN_POINT('Ctrl Pts',(-21.8172367491753,-1.1785273363336,0.095348805201107));
#60486=CARTESIAN_POINT('Ctrl Pts',(-21.8108671147362,-1.17766074088617,
0.00108845803827095));
#60487=CARTESIAN_POINT('Ctrl Pts',(-22.2121328852638,-1.17731562723721,
0.00107155510022956));
#60488=CARTESIAN_POINT('Ctrl Pts',(-22.192768960812,-1.17478496411128,-0.285697287951891));
#60489=CARTESIAN_POINT('Ctrl Pts',(-22.1468904939546,-0.92489945401143,
-0.969080044767785));
#60490=CARTESIAN_POINT('Ctrl Pts',(-22.0744974846914,0.220250981920178,
-1.37545890821731));
#60491=CARTESIAN_POINT('Ctrl Pts',(-21.9949538574744,1.27617351522542,-0.558371616639268));
#60492=CARTESIAN_POINT('Ctrl Pts',(-21.9154102302573,1.15970130793088,0.771680361039824));
#60493=CARTESIAN_POINT('Ctrl Pts',(-21.8358666030402,-0.0221649839953902,
1.39280523287201));
#60494=CARTESIAN_POINT('Ctrl Pts',(-21.7681074880424,-1.01159016239307,
0.831933682326423));
#60495=CARTESIAN_POINT('Ctrl Pts',(-21.7268629154503,-1.17530822785005,
0.218449926120964));
#60496=CARTESIAN_POINT('Ctrl Pts',(-21.7121328852638,-1.17589839182392,
-0.000355803537386394));
#60497=CARTESIAN_POINT('Origin',(-35.5608671147362,0.,0.));
#60498=CARTESIAN_POINT('',(-22.8108671147362,-1.17666012157462,-0.000924768044772844));
#60499=CARTESIAN_POINT('',(-22.7121328852638,-1.17968287648054,-0.000118772304556619));
#60500=CARTESIAN_POINT('',(-35.5608671147362,-1.17775,1.38253677383905E-12));
#60501=CARTESIAN_POINT('Ctrl Pts',(-22.8108671147362,-1.17666012157462,
-0.000924768044772949));
#60502=CARTESIAN_POINT('Ctrl Pts',(-22.8020779247101,-1.17761224020395,
-0.131271169296472));
#60503=CARTESIAN_POINT('Ctrl Pts',(-22.7667741922784,-1.09743454109949,
-0.653698313999505));
#60504=CARTESIAN_POINT('Ctrl Pts',(-22.7049559174411,-0.330948914727013,
-1.35309665207331));
#60505=CARTESIAN_POINT('Ctrl Pts',(-22.625412290224,0.959349655377068,-1.00997325347698));
#60506=CARTESIAN_POINT('Ctrl Pts',(-22.5458686630069,1.36831314295389,0.260992101088554));
#60507=CARTESIAN_POINT('Ctrl Pts',(-22.4663250357899,0.520235081592649,
1.29218930265316));
#60508=CARTESIAN_POINT('Ctrl Pts',(-22.3879911863663,-0.785605176845554,
1.13864963108566));
#60509=CARTESIAN_POINT('Ctrl Pts',(-22.3361718793484,-1.17820505033083,
0.372553377872414));
#60510=CARTESIAN_POINT('Ctrl Pts',(-22.3108671147362,-1.17958641441151,
-0.000329593618060599));
#60511=CARTESIAN_POINT('Ctrl Pts',(-22.7121328852638,-1.17968287648054,
-0.000118772304556725));
#60512=CARTESIAN_POINT('Ctrl Pts',(-22.7117040909852,-1.17969191172516,
-0.00643596420863167));
#60513=CARTESIAN_POINT('Ctrl Pts',(-22.6847607543009,-1.17678034422692,
-0.403368869626029));
#60514=CARTESIAN_POINT('Ctrl Pts',(-22.6313028752108,-0.734089160829106,
-1.18385421703197));
#60515=CARTESIAN_POINT('Ctrl Pts',(-22.5517592479938,0.59901410027068,-1.25760876702895));
#60516=CARTESIAN_POINT('Ctrl Pts',(-22.4722156207767,1.38181524937403,-0.176023634289684));
#60517=CARTESIAN_POINT('Ctrl Pts',(-22.3926719935596,0.89517073805671,1.06727084329994));
#60518=CARTESIAN_POINT('Ctrl Pts',(-22.3131283663426,-0.413848985342271,
1.33008523056319));
#60519=CARTESIAN_POINT('Ctrl Pts',(-22.2529486635773,-1.11656292156274,
0.604460393264336));
#60520=CARTESIAN_POINT('Ctrl Pts',(-22.2192835032177,-1.17825013848407,
0.106968189992137));
#60521=CARTESIAN_POINT('Ctrl Pts',(-22.2121328852638,-1.17731562723721,
0.00107155510022956));
#60522=CARTESIAN_POINT('Origin',(-35.5608671147362,0.,0.));
#60523=CARTESIAN_POINT('',(-23.3108671147362,-1.17623098844965,0.000705324900118179));
#60524=CARTESIAN_POINT('',(-23.2121328852638,-1.17695757629942,-0.00101259305823678));
#60525=CARTESIAN_POINT('',(-35.5608671147362,-1.17775,1.38253677383905E-12));
#60526=CARTESIAN_POINT('Ctrl Pts',(-23.3108671147362,-1.17623098844965,
0.000705324900118123));
#60527=CARTESIAN_POINT('Ctrl Pts',(-23.2944985124776,-1.17490938811235,
-0.242268570117102));
#60528=CARTESIAN_POINT('Ctrl Pts',(-23.2516153678133,-0.983020868014358,
-0.880735622124971));
#60529=CARTESIAN_POINT('Ctrl Pts',(-23.1822176807434,0.063859941221911,
-1.39151702897166));
#60530=CARTESIAN_POINT('Ctrl Pts',(-23.1026740535264,1.20512786551627,-0.698616176285083));
#60531=CARTESIAN_POINT('Ctrl Pts',(-23.0231304263093,1.23926924751441,0.636089196713827));
#60532=CARTESIAN_POINT('Ctrl Pts',(-22.9435867990922,0.134919091615136,
1.38643231812041));
#60533=CARTESIAN_POINT('Ctrl Pts',(-22.8728323619012,-0.957657495158324,
0.920915194534099));
#60534=CARTESIAN_POINT('Ctrl Pts',(-22.8285924671158,-1.17473996304328,
0.261947679446613));
#60535=CARTESIAN_POINT('Ctrl Pts',(-22.8108671147362,-1.17666012157462,
-0.000924768044772949));
#60536=CARTESIAN_POINT('Ctrl Pts',(-23.2121328852638,-1.17695757629942,
-0.00101259305823675));
#60537=CARTESIAN_POINT('Ctrl Pts',(-23.2041246787526,-1.17792417914125,
-0.119701061165631));
#60538=CARTESIAN_POINT('Ctrl Pts',(-23.1696019298358,-1.10678344897941,
-0.630225684678308));
#60539=CARTESIAN_POINT('Ctrl Pts',(-23.1085646385132,-0.370638116920458,
-1.34276769752508));
#60540=CARTESIAN_POINT('Ctrl Pts',(-23.0290210112962,0.929202144692953,
-1.03777698834055));
#60541=CARTESIAN_POINT('Ctrl Pts',(-22.949477384079,1.37540323075928,0.220598404455005));
#60542=CARTESIAN_POINT('Ctrl Pts',(-22.869933756862,0.558049247935703,1.27631451457294));
#60543=CARTESIAN_POINT('Ctrl Pts',(-22.7908189239236,-0.764803540982205,
1.16013602633681));
#60544=CARTESIAN_POINT('Ctrl Pts',(-22.7382186333909,-1.17913321635846,
0.384188307066044));
#60545=CARTESIAN_POINT('Ctrl Pts',(-22.7121328852638,-1.17968287648054,
-0.000118772304556725));
#60546=CARTESIAN_POINT('Origin',(-35.5608671147362,0.,0.));
#60547=CARTESIAN_POINT('',(-23.8108671147362,-1.17924338756027,0.000656574873420682));
#60548=CARTESIAN_POINT('',(-23.7121328852638,-1.17604479913671,0.000547799251428352));
#60549=CARTESIAN_POINT('',(-35.5608671147362,-1.17775,1.38253677383905E-12));
#60550=CARTESIAN_POINT('Ctrl Pts',(-23.8108671147362,-1.17924338756027,
0.000656574873420736));
#60551=CARTESIAN_POINT('Ctrl Pts',(-23.7869191002451,-1.17688497172179,
-0.352505813248667));
#60552=CARTESIAN_POINT('Ctrl Pts',(-23.7364565433482,-0.82034060012706,
-1.10080786323156));
#60553=CARTESIAN_POINT('Ctrl Pts',(-23.6594794440458,0.453490285739293,
-1.31709691927021));
#60554=CARTESIAN_POINT('Ctrl Pts',(-23.5799358168287,1.35318020387053,-0.330607123129397));
#60555=CARTESIAN_POINT('Ctrl Pts',(-23.5003921896117,1.00973089745727,0.959604735675643));
#60556=CARTESIAN_POINT('Ctrl Pts',(-23.4208485623946,-0.261337717362417,
1.36824717485357));
#60557=CARTESIAN_POINT('Ctrl Pts',(-23.3576735374361,-1.08016351082504,
0.694480989205406));
#60558=CARTESIAN_POINT('Ctrl Pts',(-23.3210130548833,-1.17705017127962,
0.151310645819719));
#60559=CARTESIAN_POINT('Ctrl Pts',(-23.3108671147362,-1.17623098844965,
0.000705324900118123));
#60560=CARTESIAN_POINT('Ctrl Pts',(-23.7121328852638,-1.17604479913671,
0.000547799251428352));
#60561=CARTESIAN_POINT('Ctrl Pts',(-23.6965452665201,-1.17507642505556,
-0.23092491432183));
#60562=CARTESIAN_POINT('Ctrl Pts',(-23.6544431053707,-0.996915032030405,
-0.857508140843176));
#60563=CARTESIAN_POINT('Ctrl Pts',(-23.5858264018155,0.0228686033435479,
-1.39279385775939));
#60564=CARTESIAN_POINT('Ctrl Pts',(-23.5062827745985,1.18403960412511,-0.733790105612224));
#60565=CARTESIAN_POINT('Ctrl Pts',(-23.4267391473814,1.25745742089477,0.599331742750071));
#60566=CARTESIAN_POINT('Ctrl Pts',(-23.3471955201644,0.175674593553903,
1.38185966740868));
#60567=CARTESIAN_POINT('Ctrl Pts',(-23.2756600994585,-0.942338256566478,
0.943926606442159));
#60568=CARTESIAN_POINT('Ctrl Pts',(-23.2306392211583,-1.17472383309582,
0.273267129189906));
#60569=CARTESIAN_POINT('Ctrl Pts',(-23.2121328852638,-1.17695757629942,
-0.00101259305823675));
#60570=CARTESIAN_POINT('Origin',(-35.5608671147362,0.,0.));
#60571=CARTESIAN_POINT('',(-24.3108671147362,-1.17827283352878,-0.00103052933429097));
#60572=CARTESIAN_POINT('',(-24.2121328852638,-1.17896945751039,0.000810547160777966));
#60573=CARTESIAN_POINT('',(-35.5608671147362,-1.17775,1.38253677383905E-12));
#60574=CARTESIAN_POINT('Ctrl Pts',(-24.3108671147362,-1.17827283352878,
-0.00103052933429112));
#60575=CARTESIAN_POINT('Ctrl Pts',(-24.3058542304182,-1.17895298703858,
-0.0751143629464088));
#60576=CARTESIAN_POINT('Ctrl Pts',(-24.2743268036945,-1.13879400230303,
-0.540313240337936));
#60577=CARTESIAN_POINT('Ctrl Pts',(-24.2162848345652,-0.519582222535895,
-1.29245195192535));
#60578=CARTESIAN_POINT('Ctrl Pts',(-24.1367412073481,0.806346330376981,
-1.13587117645381));
#60579=CARTESIAN_POINT('Ctrl Pts',(-24.057197580131,1.39150085408669,0.0642114248945288));
#60580=CARTESIAN_POINT('Ctrl Pts',(-23.977653952914,0.698311748651915,1.20530429174781));
#60581=CARTESIAN_POINT('Ctrl Pts',(-23.8981103256969,-0.636402205599313,
1.2391085371021));
#60582=CARTESIAN_POINT('Ctrl Pts',(-23.842514712971,-1.1606462882032,0.467110064893475));
#60583=CARTESIAN_POINT('Ctrl Pts',(-23.8134336426507,-1.17949614087667,
0.038505271174667));
#60584=CARTESIAN_POINT('Ctrl Pts',(-23.8108671147362,-1.17924338756027,
0.000656574873420736));
#60585=CARTESIAN_POINT('Ctrl Pts',(-24.2121328852638,-1.17896945751039,
0.000810547160777922));
#60586=CARTESIAN_POINT('Ctrl Pts',(-24.1889658542875,-1.17628369526718,
-0.341042935736306));
#60587=CARTESIAN_POINT('Ctrl Pts',(-24.1392842809056,-0.83953713219871,
-1.07875537338835));
#60588=CARTESIAN_POINT('Ctrl Pts',(-24.0630881651179,0.4145208696013,-1.32987599117216));
#60589=CARTESIAN_POINT('Ctrl Pts',(-23.9835445379008,1.34286127481651,-0.370298933065331));
#60590=CARTESIAN_POINT('Ctrl Pts',(-23.9040009106838,1.03754224644608,0.929464248947089));
#60591=CARTESIAN_POINT('Ctrl Pts',(-23.8244572834667,-0.220945812915096,
1.37534746554696));
#60592=CARTESIAN_POINT('Ctrl Pts',(-23.7605012749934,-1.06961445595894,
0.71795034584099));
#60593=CARTESIAN_POINT('Ctrl Pts',(-23.7230598089258,-1.17672362954916,
0.162810214865867));
#60594=CARTESIAN_POINT('Ctrl Pts',(-23.7121328852638,-1.17604479913671,
0.000547799251428352));
#60595=CARTESIAN_POINT('Origin',(-35.5608671147362,0.,0.));
#60596=CARTESIAN_POINT('',(-24.8108671147362,-1.17581964054164,-0.000162966847959915));
#60597=CARTESIAN_POINT('',(-24.7121328852638,-1.17861332264333,-0.000947007987461695));
#60598=CARTESIAN_POINT('',(-35.5608671147362,-1.17775,1.38253677383905E-12));
#60599=CARTESIAN_POINT('Ctrl Pts',(-24.8108671147362,-1.17581964054164,
-0.000162966847959863));
#60600=CARTESIAN_POINT('Ctrl Pts',(-24.7982748181856,-1.17604985957002,
-0.187245202631063));
#60601=CARTESIAN_POINT('Ctrl Pts',(-24.7591679792295,-1.04559083977625,
-0.767947470306765));
#60602=CARTESIAN_POINT('Ctrl Pts',(-24.6935465978676,-0.134218671713418,
-1.38650030009895));
#60603=CARTESIAN_POINT('Ctrl Pts',(-24.6140029706505,1.09381437731624,-0.862535704760827));
#60604=CARTESIAN_POINT('Ctrl Pts',(-24.5344593434334,1.31698232935204,0.453822959077054));
#60605=CARTESIAN_POINT('Ctrl Pts',(-24.4549157162164,0.330265310438215,
1.35326366933134));
#60606=CARTESIAN_POINT('Ctrl Pts',(-24.3803849733173,-0.878555344404979,
1.03115338381769));
#60607=CARTESIAN_POINT('Ctrl Pts',(-24.3323687728239,-1.17535546554516,
0.31673568251358));
#60608=CARTESIAN_POINT('Ctrl Pts',(-24.3108671147362,-1.17827283352878,
-0.00103052933429112));
#60609=CARTESIAN_POINT('Ctrl Pts',(-24.7121328852638,-1.17861332264333,
-0.000947007987461626));
#60610=CARTESIAN_POINT('Ctrl Pts',(-24.7079009844607,-1.17916029092104,
-0.063442223242721));
#60611=CARTESIAN_POINT('Ctrl Pts',(-24.6771545412518,-1.14617599158811,
-0.516916385756128));
#60612=CARTESIAN_POINT('Ctrl Pts',(-24.6198935556373,-0.557404403734147,
-1.27659626896248));
#60613=CARTESIAN_POINT('Ctrl Pts',(-24.5403499284203,0.772558932325985,
-1.15911621475782));
#60614=CARTESIAN_POINT('Ctrl Pts',(-24.4608063012032,1.39278803690711,0.0232204108402372));
#60615=CARTESIAN_POINT('Ctrl Pts',(-24.3812626739862,0.733491003577628,
1.18422491567347));
#60616=CARTESIAN_POINT('Ctrl Pts',(-24.3017190467691,-0.599649346990552,
1.25730599453155));
#60617=CARTESIAN_POINT('Ctrl Pts',(-24.2453424505283,-1.15407282652745,
0.490451662275239));
#60618=CARTESIAN_POINT('Ctrl Pts',(-24.2154803966932,-1.17935753571579,
0.0502065376244371));
#60619=CARTESIAN_POINT('Ctrl Pts',(-24.2121328852638,-1.17896945751039,
0.000810547160777922));
#60620=CARTESIAN_POINT('Origin',(-35.5608671147362,0.,0.));
#60621=CARTESIAN_POINT('',(-25.3108671147362,-1.17767278411775,0.00108839386667727));
#60622=CARTESIAN_POINT('',(-25.2121328852638,-1.17589484267592,-0.000349556156004835));
#60623=CARTESIAN_POINT('',(-35.5608671147362,-1.17775,1.38253677383905E-12));
#60624=CARTESIAN_POINT('Ctrl Pts',(-25.3108671147362,-1.17767278411775,
0.00108839386667732));
#60625=CARTESIAN_POINT('Ctrl Pts',(-25.2906954059531,-1.17492606912136,
-0.2974126674257));
#60626=CARTESIAN_POINT('Ctrl Pts',(-25.2440091547643,-0.907874136102811,
-0.992648780792579));
#60627=CARTESIAN_POINT('Ctrl Pts',(-25.1708083611699,0.262028899865992,
-1.36811497676401));
#60628=CARTESIAN_POINT('Ctrl Pts',(-25.0912647339529,1.29258315287295,-0.519255743271084));
#60629=CARTESIAN_POINT('Ctrl Pts',(-25.0117211067357,1.13566746379413,0.806633216332175));
#60630=CARTESIAN_POINT('Ctrl Pts',(-24.9321774795188,-0.0645629044702633,
1.39148459042037));
#60631=CARTESIAN_POINT('Ctrl Pts',(-24.8652261488522,-1.0248656128002,0.807789446248808));
#60632=CARTESIAN_POINT('Ctrl Pts',(-24.8247893605913,-1.17556510667638,
0.206678165844237));
#60633=CARTESIAN_POINT('Ctrl Pts',(-24.8108671147362,-1.17581964054164,
-0.000162966847959863));
#60634=CARTESIAN_POINT('Ctrl Pts',(-25.2121328852638,-1.17589484267592,
-0.00034955615600487));
#60635=CARTESIAN_POINT('Ctrl Pts',(-25.2003215722281,-1.17635967926637,
-0.175800821169687));
#60636=CARTESIAN_POINT('Ctrl Pts',(-25.1619957167867,-1.05711946252861,
-0.744512129245651));
#60637=CARTESIAN_POINT('Ctrl Pts',(-25.0971553189397,-0.174976478479087,
-1.38194823897649));
#60638=CARTESIAN_POINT('Ctrl Pts',(-25.0176116917226,1.06794887502363,-0.894361729708357));
#60639=CARTESIAN_POINT('Ctrl Pts',(-24.9380680645055,1.32977124419901,0.414856772070276));
#60640=CARTESIAN_POINT('Ctrl Pts',(-24.8585244372885,0.369959725584168,
1.34295476642992));
#60641=CARTESIAN_POINT('Ctrl Pts',(-24.7832127108746,-0.860580059283745,
1.0535685672263));
#60642=CARTESIAN_POINT('Ctrl Pts',(-24.7344155268664,-1.17573331702244,
0.328115167186435));
#60643=CARTESIAN_POINT('Ctrl Pts',(-24.7121328852638,-1.17861332264333,
-0.000947007987461626));
#60644=CARTESIAN_POINT('Origin',(-35.5608671147362,0.,0.));
#60645=CARTESIAN_POINT('',(-25.8108671147362,-1.17958164686523,-0.000336615057284358));
#60646=CARTESIAN_POINT('',(-25.7121328852638,-1.17732722815968,0.00107272862214718));
#60647=CARTESIAN_POINT('',(-35.5608671147362,-1.17775,1.38253677383905E-12));
#60648=CARTESIAN_POINT('Ctrl Pts',(-25.8108671147362,-1.17958164686523,
-0.000336615057284393));
#60649=CARTESIAN_POINT('Ctrl Pts',(-25.8096305361263,-1.17965043763247,
-0.0185586411613626));
#60650=CARTESIAN_POINT('Ctrl Pts',(-25.7818794151106,-1.17099829896009,
-0.427428002609933));
#60651=CARTESIAN_POINT('Ctrl Pts',(-25.7276137516893,-0.697702759742729,
-1.20565691349503));
#60652=CARTESIAN_POINT('Ctrl Pts',(-25.6480701244723,0.637028101537958,
-1.23878687911276));
#60653=CARTESIAN_POINT('Ctrl Pts',(-25.5685264972552,1.38653415839583,-0.133868448906134));
#60654=CARTESIAN_POINT('Ctrl Pts',(-25.4889828700381,0.862259388766268,
1.09403221181801));
#60655=CARTESIAN_POINT('Ctrl Pts',(-25.4094392428211,-0.454155603459752,
1.31686765540699));
#60656=CARTESIAN_POINT('Ctrl Pts',(-25.3500673243871,-1.12531837282715,
0.580205633210485));
#60657=CARTESIAN_POINT('Ctrl Pts',(-25.3172099483588,-1.17853646683388,
0.0949496818871333));
#60658=CARTESIAN_POINT('Ctrl Pts',(-25.3108671147362,-1.17767278411775,
0.00108839386667732));
#60659=CARTESIAN_POINT('Ctrl Pts',(-25.7121328852638,-1.17732722815968,
0.00107272862214714));
#60660=CARTESIAN_POINT('Ctrl Pts',(-25.6927421599956,-1.17478830088982,
-0.286085832571626));
#60661=CARTESIAN_POINT('Ctrl Pts',(-25.6468368923217,-0.924343956719117,
-0.969864019612402));
#60662=CARTESIAN_POINT('Ctrl Pts',(-25.574417082242,0.221640587522368,-1.3752356718737));
#60663=CARTESIAN_POINT('Ctrl Pts',(-25.494873455025,1.27673702398653,-0.557081928277323));
#60664=CARTESIAN_POINT('Ctrl Pts',(-25.4153298278079,1.1589210357743,0.772851690863756));
#60665=CARTESIAN_POINT('Ctrl Pts',(-25.3357862005909,-0.0235722168554084,
1.39278212719136));
#60666=CARTESIAN_POINT('Ctrl Pts',(-25.2680538864095,-1.01203908044992,
0.831133417830471));
#60667=CARTESIAN_POINT('Ctrl Pts',(-25.2268361146338,-1.17531619413885,
0.218059708330772));
#60668=CARTESIAN_POINT('Ctrl Pts',(-25.2121328852638,-1.17589484267592,
-0.00034955615600487));
#60669=CARTESIAN_POINT('Origin',(-35.5608671147362,0.,0.));
#60670=CARTESIAN_POINT('',(-26.3108671147362,-1.17665049820237,-0.000921216280392121));
#60671=CARTESIAN_POINT('',(-26.2121328852638,-1.1796810081197,-0.000126156119591159));
#60672=CARTESIAN_POINT('',(-35.5608671147362,-1.17775,1.38253677383905E-12));
#60673=CARTESIAN_POINT('Ctrl Pts',(-26.3108671147362,-1.17665049820237,
-0.00092121628039208));
#60674=CARTESIAN_POINT('Ctrl Pts',(-26.3020511238937,-1.17760133621249,
-0.131667774133514));
#60675=CARTESIAN_POINT('Ctrl Pts',(-26.2667205906455,-1.09710611574738,
-0.65450390914198));
#60676=CARTESIAN_POINT('Ctrl Pts',(-26.2048755149917,-0.329581621862289,
-1.35343034122248));
#60677=CARTESIAN_POINT('Ctrl Pts',(-26.1253318877746,0.960369609154678,
-1.00900344291933));
#60678=CARTESIAN_POINT('Ctrl Pts',(-26.0457882605576,1.36804874678321,0.262374466051626));
#60679=CARTESIAN_POINT('Ctrl Pts',(-25.9662446333405,0.518929230876408,
1.2927142713504));
#60680=CARTESIAN_POINT('Ctrl Pts',(-25.8879375847333,-0.786308508212076,
1.13790828330489));
#60681=CARTESIAN_POINT('Ctrl Pts',(-25.8361450785319,-1.17817543580043,
0.372155446866836));
#60682=CARTESIAN_POINT('Ctrl Pts',(-25.8108671147362,-1.17958164686523,
-0.000336615057284393));
#60683=CARTESIAN_POINT('Ctrl Pts',(-26.2121328852638,-1.1796810081197,-0.000126156119591359));
#60684=CARTESIAN_POINT('Ctrl Pts',(-26.2116772901687,-1.17969117920181,
-0.00683821842843334));
#60685=CARTESIAN_POINT('Ctrl Pts',(-26.1847071526679,-1.17659452910613,
-0.40416657589943));
#60686=CARTESIAN_POINT('Ctrl Pts',(-26.1312224727615,-0.732892659131677,
-1.1845953120885));
#60687=CARTESIAN_POINT('Ctrl Pts',(-26.0516788455444,0.600284440673691,
-1.25700290115665));
#60688=CARTESIAN_POINT('Ctrl Pts',(-25.9721352183273,1.38199239250399,-0.174627404184641));
#60689=CARTESIAN_POINT('Ctrl Pts',(-25.8925915911103,0.894091946110794,
1.06817474934159));
#60690=CARTESIAN_POINT('Ctrl Pts',(-25.8130479638932,-0.415192648070296,
1.32966641238302));
#60691=CARTESIAN_POINT('Ctrl Pts',(-25.7528950619444,-1.116860453876,0.603655417092753));
#60692=CARTESIAN_POINT('Ctrl Pts',(-25.7192567024013,-1.17825998613265,
0.106569818137628));
#60693=CARTESIAN_POINT('Ctrl Pts',(-25.7121328852638,-1.17732722815968,
0.00107272862214714));
#60694=CARTESIAN_POINT('Origin',(-35.5608671147362,0.,0.));
#60695=CARTESIAN_POINT('',(-26.8108671147362,-1.17623821978682,0.000710373043126506));
#60696=CARTESIAN_POINT('',(-26.7121328852638,-1.17694686483815,-0.00101009995142842));
#60697=CARTESIAN_POINT('',(-35.5608671147362,-1.17775,1.38253677383905E-12));
#60698=CARTESIAN_POINT('Ctrl Pts',(-26.8108671147362,-1.17623821978682,
0.000710373043126492));
#60699=CARTESIAN_POINT('Ctrl Pts',(-26.7944717116611,-1.17490448726406,
-0.242657602767575));
#60700=CARTESIAN_POINT('Ctrl Pts',(-26.7515617661804,-0.98253499608713,
-0.881531533240058));
#60701=CARTESIAN_POINT('Ctrl Pts',(-26.6821372782941,0.065265851241496,
-1.39145179674781));
#60702=CARTESIAN_POINT('Ctrl Pts',(-26.6025936510769,1.20583310898822,-0.697398198505544));
#60703=CARTESIAN_POINT('Ctrl Pts',(-26.52305002386,1.23862593155623,0.637340988551213));
#60704=CARTESIAN_POINT('Ctrl Pts',(-26.4435063966428,0.133518217557687,
1.38656792822826));
#60705=CARTESIAN_POINT('Ctrl Pts',(-26.3727787602683,-0.958173793744215,
0.920123888731101));
#60706=CARTESIAN_POINT('Ctrl Pts',(-26.3285656662994,-1.17474164236858,
0.261559171599099));
#60707=CARTESIAN_POINT('Ctrl Pts',(-26.3108671147362,-1.17665049820237,
-0.00092121628039208));
#60708=CARTESIAN_POINT('Ctrl Pts',(-26.7121328852638,-1.17694686483815,
-0.00101009995142851));
#60709=CARTESIAN_POINT('Ctrl Pts',(-26.7040978779362,-1.1779136851793,-0.120098518176512));
#60710=CARTESIAN_POINT('Ctrl Pts',(-26.6695483282028,-1.10646967436812,
-0.631031077485085));
#60711=CARTESIAN_POINT('Ctrl Pts',(-26.6084842360638,-0.369281239830358,
-1.34314149259879));
#60712=CARTESIAN_POINT('Ctrl Pts',(-26.5289406088467,0.930250205829247,
-1.03683762363535));
#60713=CARTESIAN_POINT('Ctrl Pts',(-26.4493969816297,1.37517964341989,0.221987953625214));
#60714=CARTESIAN_POINT('Ctrl Pts',(-26.3698533544126,0.556759417277243,
1.27687769755144));
#60715=CARTESIAN_POINT('Ctrl Pts',(-26.2907653222907,-0.765527226002879,
1.15940251126422));
#60716=CARTESIAN_POINT('Ctrl Pts',(-26.2381918325744,-1.17909924660449,
0.383787718128221));
#60717=CARTESIAN_POINT('Ctrl Pts',(-26.2121328852638,-1.1796810081197,-0.000126156119591359));
#60718=CARTESIAN_POINT('Origin',(-35.5608671147362,0.,0.));
#60719=CARTESIAN_POINT('',(-27.3108671147362,-1.17925193811534,0.00065078897648006));
#60720=CARTESIAN_POINT('',(-27.2121328852638,-1.17605037721591,0.000553511253033878));
#60721=CARTESIAN_POINT('',(-35.5608671147362,-1.17775,1.38253677383905E-12));
#60722=CARTESIAN_POINT('Ctrl Pts',(-27.3108671147362,-1.17925193811534,
0.000650788976480016));
#60723=CARTESIAN_POINT('Ctrl Pts',(-27.2868922994286,-1.1769076025239,-0.352900079711213));
#60724=CARTESIAN_POINT('Ctrl Pts',(-27.2364029417154,-0.819671542274753,
-1.10156128989161));
#60725=CARTESIAN_POINT('Ctrl Pts',(-27.1593990415964,0.454820805275012,
-1.3166380554655));
#60726=CARTESIAN_POINT('Ctrl Pts',(-27.0798554143794,1.35351354764217,-0.329239746021173));
#60727=CARTESIAN_POINT('Ctrl Pts',(-27.0003117871623,1.00876082929865,0.960624444454579));
#60728=CARTESIAN_POINT('Ctrl Pts',(-26.9207681599452,-0.262720015497096,
1.36798242951735));
#60729=CARTESIAN_POINT('Ctrl Pts',(-26.8576199358032,-1.08051755755227,
0.69367545683447));
#60730=CARTESIAN_POINT('Ctrl Pts',(-26.8209862540668,-1.17706139108464,
0.150915552176598));
#60731=CARTESIAN_POINT('Ctrl Pts',(-26.8108671147362,-1.17623821978682,
0.000710373043126492));
#60732=CARTESIAN_POINT('Ctrl Pts',(-27.2121328852638,-1.17605037721591,
0.000553511253033739));
#60733=CARTESIAN_POINT('Ctrl Pts',(-27.1965184657036,-1.17506995411779,
-0.231314439735884));
#60734=CARTESIAN_POINT('Ctrl Pts',(-27.1543895037377,-0.996446651052049,
-0.858306279729821));
#60735=CARTESIAN_POINT('Ctrl Pts',(-27.0857459993661,0.0242758243513772,
-1.39277004117091));
#60736=CARTESIAN_POINT('Ctrl Pts',(-27.0062023721491,1.18478039693156,-0.732593416758471));
#60737=CARTESIAN_POINT('Ctrl Pts',(-26.926658744932,1.2568512341643,0.60060193007585));
#60738=CARTESIAN_POINT('Ctrl Pts',(-26.847115117715,0.174278318748489,1.38203645785679));
#60739=CARTESIAN_POINT('Ctrl Pts',(-26.7756064978256,-0.94287278904871,
0.943138512528417));
#60740=CARTESIAN_POINT('Ctrl Pts',(-26.7306124203419,-1.17472329618662,
0.272878710877991));
#60741=CARTESIAN_POINT('Ctrl Pts',(-26.7121328852638,-1.17694686483815,
-0.00101009995142851));
#60742=CARTESIAN_POINT('Origin',(-35.5608671147362,0.,0.));
#60743=CARTESIAN_POINT('',(-27.8108671147362,-1.17826087657773,-0.00103275332089385));
#60744=CARTESIAN_POINT('',(-27.7121328852638,-1.17897957473222,0.000805758147836705));
#60745=CARTESIAN_POINT('',(-35.5608671147362,-1.17775,1.38253677383905E-12));
#60746=CARTESIAN_POINT('Ctrl Pts',(-27.8108671147362,-1.17826087657773,
-0.00103275332089375));
#60747=CARTESIAN_POINT('Ctrl Pts',(-27.8058274296017,-1.17894535395326,
-0.0755146158255072));
#60748=CARTESIAN_POINT('Ctrl Pts',(-27.7742732020616,-1.13853377759971,
-0.541116554034106));
#60749=CARTESIAN_POINT('Ctrl Pts',(-27.7162044321158,-0.51827610678078,
-1.2929762608614));
#60750=CARTESIAN_POINT('Ctrl Pts',(-27.6366608048988,0.807493565332879,
-1.13505589111593));
#60751=CARTESIAN_POINT('Ctrl Pts',(-27.5571171776817,1.39143526674366,0.0656173183921381));
#60752=CARTESIAN_POINT('Ctrl Pts',(-27.4775735504646,0.697093592772551,
1.20600922754614));
#60753=CARTESIAN_POINT('Ctrl Pts',(-27.3980299232476,-0.637653834900464,
1.23846490497216));
#60754=CARTESIAN_POINT('Ctrl Pts',(-27.3424611113381,-1.16086530360064,
0.466309558213219));
#60755=CARTESIAN_POINT('Ctrl Pts',(-27.3134068418343,-1.17950028090973,
0.0381035372145209));
#60756=CARTESIAN_POINT('Ctrl Pts',(-27.3108671147362,-1.17925193811534,
0.000650788976480016));
#60757=CARTESIAN_POINT('Ctrl Pts',(-27.7121328852638,-1.17897957473222,
0.00080575814783667));
#60758=CARTESIAN_POINT('Ctrl Pts',(-27.6889390534711,-1.17630249771759,
-0.341435519304642));
#60759=CARTESIAN_POINT('Ctrl Pts',(-27.6392306792727,-0.83888794977059,
-1.07951518110267));
#60760=CARTESIAN_POINT('Ctrl Pts',(-27.5630077626685,0.415864320577861,
-1.32945649424924));
#60761=CARTESIAN_POINT('Ctrl Pts',(-27.4834641354515,1.34323472714235,-0.368941961600966));
#60762=CARTESIAN_POINT('Ctrl Pts',(-27.4039205082344,1.03660261703927,0.930512072774181));
#60763=CARTESIAN_POINT('Ctrl Pts',(-27.3243768810174,-0.222335305564666,
1.37512352722605));
#60764=CARTESIAN_POINT('Ctrl Pts',(-27.2604476733605,-1.06998394645003,
0.717145118413367));
#60765=CARTESIAN_POINT('Ctrl Pts',(-27.2230330081093,-1.17673479152724,
0.162416021733489));
#60766=CARTESIAN_POINT('Ctrl Pts',(-27.2121328852638,-1.17605037721591,
0.000553511253033739));
#60767=CARTESIAN_POINT('Origin',(-35.5608671147362,0.,0.));
#60768=CARTESIAN_POINT('',(-28.3108671147362,-1.17581803868898,-0.000156443803798287));
#60769=CARTESIAN_POINT('',(-28.2121328852638,-1.17860195998943,-0.000950464435633125));
#60770=CARTESIAN_POINT('',(-35.5608671147362,-1.17775,1.38253677383905E-12));
#60771=CARTESIAN_POINT('Ctrl Pts',(-28.3108671147362,-1.17581803868898,
-0.00015644380379834));
#60772=CARTESIAN_POINT('Ctrl Pts',(-28.2982480173692,-1.17603949646834,
-0.187637492819666));
#60773=CARTESIAN_POINT('Ctrl Pts',(-28.2591143775965,-1.04518687140584,
-0.768751257994004));
#60774=CARTESIAN_POINT('Ctrl Pts',(-28.1934661954182,-0.132817729326718,
-1.38663520249108));
#60775=CARTESIAN_POINT('Ctrl Pts',(-28.1139225682011,1.09468529645522,-0.861430110766812));
#60776=CARTESIAN_POINT('Ctrl Pts',(-28.0343789409841,1.31652312948372,0.455153362665139));
#60777=CARTESIAN_POINT('Ctrl Pts',(-27.954835313767,0.32889784917371,1.35359666770419));
#60778=CARTESIAN_POINT('Ctrl Pts',(-27.8803313716844,-0.879162171581557,
1.03038146243381));
#60779=CARTESIAN_POINT('Ctrl Pts',(-27.8323419720074,-1.17534421540685,
0.316345678846432));
#60780=CARTESIAN_POINT('Ctrl Pts',(-27.8108671147362,-1.17826087657773,
-0.00103275332089375));
#60781=CARTESIAN_POINT('Ctrl Pts',(-28.2121328852638,-1.17860195998943,
-0.00095046443563316));
#60782=CARTESIAN_POINT('Ctrl Pts',(-28.2078741836442,-1.17915367573901,
-0.063843037399876));
#60783=CARTESIAN_POINT('Ctrl Pts',(-28.1771009396189,-1.14592906312012,
-0.517718893020072));
#60784=CARTESIAN_POINT('Ctrl Pts',(-28.1198131531879,-0.556114288729563,
-1.27715880026799));
#60785=CARTESIAN_POINT('Ctrl Pts',(-28.0402695259709,0.773729670542738,
-1.15833505522063));
#60786=CARTESIAN_POINT('Ctrl Pts',(-27.9607258987538,1.39276386486699,0.0246276257872868));
#60787=CARTESIAN_POINT('Ctrl Pts',(-27.8811822715368,0.732294127643924,
1.18496540618255));
#60788=CARTESIAN_POINT('Ctrl Pts',(-27.8016386443197,-0.600919381158034,
1.25669948698159));
#60789=CARTESIAN_POINT('Ctrl Pts',(-27.7452888488954,-1.15430457516135,
0.48965019532849));
#60790=CARTESIAN_POINT('Ctrl Pts',(-27.7154535958768,-1.17936285758663,
0.0498051754229093));
#60791=CARTESIAN_POINT('Ctrl Pts',(-27.7121328852638,-1.17897957473222,
0.00080575814783667));
#60792=CARTESIAN_POINT('Origin',(-35.5608671147362,0.,0.));
#60793=CARTESIAN_POINT('',(-28.8108671147362,-1.17768483637225,0.00108828645020804));
#60794=CARTESIAN_POINT('',(-28.7121328852638,-1.17589135698706,-0.000343296306542437));
#60795=CARTESIAN_POINT('',(-35.5608671147362,-1.17775,1.38253677383905E-12));
#60796=CARTESIAN_POINT('Ctrl Pts',(-28.8108671147362,-1.17768483637225,
0.00108828645020802));
#60797=CARTESIAN_POINT('Ctrl Pts',(-28.7906686051367,-1.17493223102293,
-0.29780156408021));
#60798=CARTESIAN_POINT('Ctrl Pts',(-28.7439555531314,-0.907299205563009,
-0.993428524395512));
#60799=CARTESIAN_POINT('Ctrl Pts',(-28.6707279587205,0.26341106407934,-1.3678495331474));
#60800=CARTESIAN_POINT('Ctrl Pts',(-28.5911843315035,1.29310713187823,-0.517949495121513));
#60801=CARTESIAN_POINT('Ctrl Pts',(-28.5116407042864,1.13485188870017,0.807780245317151));
#60802=CARTESIAN_POINT('Ctrl Pts',(-28.4320970770694,-0.0659687813562216,
1.39141864796234));
#60803=CARTESIAN_POINT('Ctrl Pts',(-28.3651725472193,-1.02529707757759,
0.806987586918573));
#60804=CARTESIAN_POINT('Ctrl Pts',(-28.3247625597749,-1.17557418175436,
0.206287213506804));
#60805=CARTESIAN_POINT('Ctrl Pts',(-28.3108671147362,-1.17581803868898,
-0.00015644380379834));
#60806=CARTESIAN_POINT('Ctrl Pts',(-28.7121328852638,-1.17589135698706,
-0.000343296306542576));
#60807=CARTESIAN_POINT('Ctrl Pts',(-28.7002947714117,-1.17634882903018,
-0.176193974899314));
#60808=CARTESIAN_POINT('Ctrl Pts',(-28.6619421151538,-1.05673157934627,
-0.745316721421754));
#60809=CARTESIAN_POINT('Ctrl Pts',(-28.5970749164903,-0.173580114540252,
-1.38212432402709));
#60810=CARTESIAN_POINT('Ctrl Pts',(-28.5175312892732,1.06885196332402,-0.893282253114629));
#60811=CARTESIAN_POINT('Ctrl Pts',(-28.4379876620562,1.32935140794485,0.416200117042506));
#60812=CARTESIAN_POINT('Ctrl Pts',(-28.3584440348391,0.36860265983214,1.34332787598405));
#60813=CARTESIAN_POINT('Ctrl Pts',(-28.2831591092417,-0.861206308820253,
1.0528019527854));
#60814=CARTESIAN_POINT('Ctrl Pts',(-28.2343887260499,-1.17571871082606,
0.327724144762794));
#60815=CARTESIAN_POINT('Ctrl Pts',(-28.2121328852638,-1.17860195998943,
-0.00095046443563316));
#60816=CARTESIAN_POINT('Origin',(-35.5608671147362,0.,0.));
#60817=CARTESIAN_POINT('',(-29.3108671147362,-1.17957678883665,-0.00034361873145996));
#60818=CARTESIAN_POINT('',(-29.2121328852639,-1.17733884982054,0.0010738605839565));
#60819=CARTESIAN_POINT('',(-35.5608671147362,-1.17775,1.38253677383905E-12));
#60820=CARTESIAN_POINT('Ctrl Pts',(-29.3108671147362,-1.17957678883665,
-0.000343618731460009));
#60821=CARTESIAN_POINT('Ctrl Pts',(-29.3096037353098,-1.1796483764396,-0.0189607820253154));
#60822=CARTESIAN_POINT('Ctrl Pts',(-29.2818258134777,-1.17079998240224,
-0.428226805629651));
#60823=CARTESIAN_POINT('Ctrl Pts',(-29.2275333492399,-0.696484247896873,
-1.20636123381121));
#60824=CARTESIAN_POINT('Ctrl Pts',(-29.1479897220229,0.638279405527112,
-1.23814261476251));
#60825=CARTESIAN_POINT('Ctrl Pts',(-29.0684460948058,1.38666870691719,-0.132467472488888));
#60826=CARTESIAN_POINT('Ctrl Pts',(-28.9889024675888,0.86115357482053,1.0949028516653));
#60827=CARTESIAN_POINT('Ctrl Pts',(-28.9093588403717,-0.455485891015299,
1.31640811950435));
#60828=CARTESIAN_POINT('Ctrl Pts',(-28.8500137227542,-1.12560138845616,
0.579401192032053));
#60829=CARTESIAN_POINT('Ctrl Pts',(-28.8171831475423,-1.17854557045775,
0.0945505338539331));
#60830=CARTESIAN_POINT('Ctrl Pts',(-28.8108671147362,-1.17768483637225,
0.00108828645020802));
#60831=CARTESIAN_POINT('Ctrl Pts',(-29.2121328852639,-1.17733884982054,
0.0010738605839564));
#60832=CARTESIAN_POINT('Ctrl Pts',(-29.1927153591791,-1.17479172731383,
-0.286474385102847));
#60833=CARTESIAN_POINT('Ctrl Pts',(-29.1467832906887,-0.923787818965214,
-0.970647861375066));
#60834=CARTESIAN_POINT('Ctrl Pts',(-29.0743366797926,0.223029966864688,
-1.37501103163265));
#60835=CARTESIAN_POINT('Ctrl Pts',(-28.9947930525756,1.27729922940169,-0.555791671223127));
#60836=CARTESIAN_POINT('Ctrl Pts',(-28.9152494253585,1.15813958054323,0.774022231728725));
#60837=CARTESIAN_POINT('Ctrl Pts',(-28.8357057981415,-0.0249794256519103,
1.39275759970113));
#60838=CARTESIAN_POINT('Ctrl Pts',(-28.7680002847766,-1.01248741445764,
0.830333095236203));
#60839=CARTESIAN_POINT('Ctrl Pts',(-28.7268093138174,-1.17532420111746,
0.217669467608967));
#60840=CARTESIAN_POINT('Ctrl Pts',(-28.7121328852638,-1.17589135698706,
-0.000343296306542576));
#60841=CARTESIAN_POINT('Origin',(-35.5608671147362,0.,0.));
#60842=CARTESIAN_POINT('',(-29.8108671147362,-1.17664091671953,-0.000917630315069691));
#60843=CARTESIAN_POINT('',(-29.7121328852638,-1.17967903181214,-0.00013353279709416));
#60844=CARTESIAN_POINT('',(-35.5608671147362,-1.17775,1.38253677383905E-12));
#60845=CARTESIAN_POINT('Ctrl Pts',(-29.8108671147362,-1.17664091671953,
-0.000917630315069879));
#60846=CARTESIAN_POINT('Ctrl Pts',(-29.8020243230772,-1.17759042098373,
-0.13206434913897));
#60847=CARTESIAN_POINT('Ctrl Pts',(-29.7666669890126,-1.09677718246914,
-0.655309508255734));
#60848=CARTESIAN_POINT('Ctrl Pts',(-29.7047951125423,-0.328213992546994,
-1.35376264873402));
#60849=CARTESIAN_POINT('Ctrl Pts',(-29.6252514853253,0.96138858254731,-1.00803260232924));
#60850=CARTESIAN_POINT('Ctrl Pts',(-29.5457078581082,1.3677829540518,0.263756563172021));
#60851=CARTESIAN_POINT('Ctrl Pts',(-29.4661642308912,0.517622850415724,
1.29323792039148));
#60852=CARTESIAN_POINT('Ctrl Pts',(-29.3878839831004,-0.787011143946497,
1.13716667660531));
#60853=CARTESIAN_POINT('Ctrl Pts',(-29.3361182777155,-1.17814596750797,
0.371757600210271));
#60854=CARTESIAN_POINT('Ctrl Pts',(-29.3108671147362,-1.17957678883665,
-0.000343618731460009));
#60855=CARTESIAN_POINT('Ctrl Pts',(-29.7121328852638,-1.17967903181214,
-0.000133532797094274));
#60856=CARTESIAN_POINT('Ctrl Pts',(-29.7116504893523,-1.17969040234477,
-0.00724047061861174));
#60857=CARTESIAN_POINT('Ctrl Pts',(-29.684653551035,-1.17640830311254,-0.404964318864758));
#60858=CARTESIAN_POINT('Ctrl Pts',(-29.6311420703121,-0.731695409267114,
-1.18533519786117));
#60859=CARTESIAN_POINT('Ctrl Pts',(-29.551598443095,0.601554168281548,-1.25639575208381));
#60860=CARTESIAN_POINT('Ctrl Pts',(-29.4720548158779,1.38216812483898,-0.173230995812698));
#60861=CARTESIAN_POINT('Ctrl Pts',(-29.3925111886609,0.893012241438832,
1.06907756494632));
#60862=CARTESIAN_POINT('Ctrl Pts',(-29.3129675614438,-0.416535886952527,
1.3292462368244));
#60863=CARTESIAN_POINT('Ctrl Pts',(-29.2528414603115,-1.11715749969954,
0.602850456415611));
#60864=CARTESIAN_POINT('Ctrl Pts',(-29.2192299015848,-1.1782698113613,0.106171419552341));
#60865=CARTESIAN_POINT('Ctrl Pts',(-29.2121328852639,-1.17733884982054,
0.0010738605839564));
#60866=CARTESIAN_POINT('Origin',(-35.5608671147362,0.,0.));
#60867=CARTESIAN_POINT('',(-30.3108671147362,-1.17624550500564,0.000715395404373505));
#60868=CARTESIAN_POINT('',(-30.2121328852638,-1.17693618625551,-0.00100756867321319));
#60869=CARTESIAN_POINT('',(-35.5608671147362,-1.17775,1.38253677383905E-12));
#60870=CARTESIAN_POINT('Ctrl Pts',(-30.3108671147362,-1.17624550500564,
0.000715395404373449));
#60871=CARTESIAN_POINT('Ctrl Pts',(-30.2944449108447,-1.17489964449614,
-0.24304662073349));
#60872=CARTESIAN_POINT('Ctrl Pts',(-30.2515081645475,-0.982048518931031,
-0.882327361829687));
#60873=CARTESIAN_POINT('Ctrl Pts',(-30.1820568758447,0.0666716946350309,
-1.39138514407244));
#60874=CARTESIAN_POINT('Ctrl Pts',(-30.1025132486276,1.2065371214959,-0.696179508793066));
#60875=CARTESIAN_POINT('Ctrl Pts',(-30.0229696214105,1.23798135115748,0.638592129764595));
#60876=CARTESIAN_POINT('Ctrl Pts',(-29.9434259941935,0.132117207199287,
1.38670212287024));
#60877=CARTESIAN_POINT('Ctrl Pts',(-29.8727251586353,-0.958689471350472,
0.919332479554083));
#60878=CARTESIAN_POINT('Ctrl Pts',(-29.8285388654829,-1.17474339347833,
0.261170657603315));
#60879=CARTESIAN_POINT('Ctrl Pts',(-29.8108671147362,-1.17664091671953,
-0.000917630315069879));
#60880=CARTESIAN_POINT('Ctrl Pts',(-30.2121328852638,-1.17693618625551,
-0.00100756867321311));
#60881=CARTESIAN_POINT('Ctrl Pts',(-30.2040710771197,-1.17790317456817,
-0.12049594655812));
#60882=CARTESIAN_POINT('Ctrl Pts',(-30.1694947265699,-1.10615540179254,
-0.631836479916431));
#60883=CARTESIAN_POINT('Ctrl Pts',(-30.1084038336144,-0.367923985762689,
-1.34351391653814));
#60884=CARTESIAN_POINT('Ctrl Pts',(-30.0288602063974,0.931297317327677,
-1.03589720048344));
#60885=CARTESIAN_POINT('Ctrl Pts',(-29.9493165791803,1.37495465224026,0.223377276180953));
#60886=CARTESIAN_POINT('Ctrl Pts',(-29.8697729519633,0.555469018255743,
1.2774395770404));
#60887=CARTESIAN_POINT('Ctrl Pts',(-29.7907117206578,-0.766250209985431,
1.15866871809116));
#60888=CARTESIAN_POINT('Ctrl Pts',(-29.738165031758,-1.17906542924158,0.383387226930625));
#60889=CARTESIAN_POINT('Ctrl Pts',(-29.7121328852638,-1.17967903181214,
-0.000133532797094274));
#60890=CARTESIAN_POINT('Origin',(-35.5608671147362,0.,0.));
#60891=CARTESIAN_POINT('',(-30.8108671147362,-1.17926042646981,0.000644971907101031));
#60892=CARTESIAN_POINT('',(-30.7121328852638,-1.17605601445831,0.000559203359190574));
#60893=CARTESIAN_POINT('',(-35.5608671147362,-1.17775,1.38253677383905E-12));
#60894=CARTESIAN_POINT('Ctrl Pts',(-30.8108671147362,-1.17926042646981,
0.000644971907101054));
#60895=CARTESIAN_POINT('Ctrl Pts',(-30.7868654986121,-1.1769303683839,-0.353294409864568));
#60896=CARTESIAN_POINT('Ctrl Pts',(-30.7363493400824,-0.819001798932681,
-1.10231448839058));
#60897=CARTESIAN_POINT('Ctrl Pts',(-30.659318639147,0.456150860510873,-1.31617784758222));
#60898=CARTESIAN_POINT('Ctrl Pts',(-30.57977501193,1.35384550969123,-0.327872032811375));
#60899=CARTESIAN_POINT('Ctrl Pts',(-30.5002313847129,1.00778973135526,0.961643172588391));
#60900=CARTESIAN_POINT('Ctrl Pts',(-30.4206877574958,-0.264102045436351,
1.3677162876881));
#60901=CARTESIAN_POINT('Ctrl Pts',(-30.3575663341703,-1.080871079543,0.692869917692197));
#60902=CARTESIAN_POINT('Ctrl Pts',(-30.3209594532504,-1.1770726095736,0.150520427665763));
#60903=CARTESIAN_POINT('Ctrl Pts',(-30.3108671147362,-1.17624550500564,
0.000715395404373449));
#60904=CARTESIAN_POINT('Ctrl Pts',(-30.7121328852638,-1.17605601445831,
0.000559203359190626));
#60905=CARTESIAN_POINT('Ctrl Pts',(-30.6964916648872,-1.17506353315699,
-0.231703946270628));
#60906=CARTESIAN_POINT('Ctrl Pts',(-30.6543359021048,-0.995977674532915,
-0.859104347736037));
#60907=CARTESIAN_POINT('Ctrl Pts',(-30.5856655969168,0.0256830205774446,
-1.39274480278519));
#60908=CARTESIAN_POINT('Ctrl Pts',(-30.5061219696997,1.18551998026519,-0.731395980043076));
#60909=CARTESIAN_POINT('Ctrl Pts',(-30.4265783424827,1.25624376438813,0.601871504282349));
#60910=CARTESIAN_POINT('Ctrl Pts',(-30.3470347152656,0.172881866032571,
1.38221183746495));
#60911=CARTESIAN_POINT('Ctrl Pts',(-30.2755528961927,-0.943406691408323,
0.942350301898318));
#60912=CARTESIAN_POINT('Ctrl Pts',(-30.2305856195254,-1.17472283931786,
0.272490292481629));
#60913=CARTESIAN_POINT('Ctrl Pts',(-30.2121328852638,-1.17693618625551,
-0.00100756867321311));
#60914=CARTESIAN_POINT('Origin',(-35.5608671147362,0.,0.));
#60915=CARTESIAN_POINT('',(-31.3108671147362,-1.17824890665216,-0.00103493412604925));
#60916=CARTESIAN_POINT('',(-31.2121328852638,-1.17898964596467,0.000800932373318346));
#60917=CARTESIAN_POINT('',(-35.5608671147362,-1.17775,1.38253677383905E-12));
#60918=CARTESIAN_POINT('Ctrl Pts',(-31.3108671147362,-1.17824890665216,
-0.00103493412604934));
#60919=CARTESIAN_POINT('Ctrl Pts',(-31.3058006287853,-1.17893768761402,
-0.0759148480283834));
#60920=CARTESIAN_POINT('Ctrl Pts',(-31.2742196004287,-1.13827309184918,
-0.541919893813802));
#60921=CARTESIAN_POINT('Ctrl Pts',(-31.2161240296664,-0.516969461947962,
-1.29349924987385));
#60922=CARTESIAN_POINT('Ctrl Pts',(-31.1365804024493,0.808639975965988,
-1.13423944706605));
#60923=CARTESIAN_POINT('Ctrl Pts',(-31.0570367752323,1.39136825896598,0.067023144904906));
#60924=CARTESIAN_POINT('Ctrl Pts',(-30.9774931480152,0.695874725271205,
1.20671293220041));
#60925=CARTESIAN_POINT('Ctrl Pts',(-30.8979495207982,-0.638904813258247,
1.23782000856604));
#60926=CARTESIAN_POINT('Ctrl Pts',(-30.8424075097052,-1.16108388648063,
0.465509085426306));
#60927=CARTESIAN_POINT('Ctrl Pts',(-30.8133800410178,-1.17950437938413,
0.0377017921632874));
#60928=CARTESIAN_POINT('Ctrl Pts',(-30.8108671147362,-1.17926042646981,
0.000644971907101054));
#60929=CARTESIAN_POINT('Ctrl Pts',(-31.2121328852638,-1.17898964596467,
0.000800932373318424));
#60930=CARTESIAN_POINT('Ctrl Pts',(-31.1889122526546,-1.17632142805659,
-0.341828155202142));
#60931=CARTESIAN_POINT('Ctrl Pts',(-31.1391770776397,-0.838238088557327,
-1.08027477832003));
#60932=CARTESIAN_POINT('Ctrl Pts',(-31.0629273602191,0.417207347022933,
-1.32903564016216));
#60933=CARTESIAN_POINT('Ctrl Pts',(-30.9833837330021,1.34360680823865,-0.367584613505395));
#60934=CARTESIAN_POINT('Ctrl Pts',(-30.903840105785,1.03566192942565,0.931558946696078));
#60935=CARTESIAN_POINT('Ctrl Pts',(-30.824296478568,-0.223724571245162,
1.3748981851222));
#60936=CARTESIAN_POINT('Ctrl Pts',(-30.7603940717276,-1.07035290206037,
0.716339876975727));
#60937=CARTESIAN_POINT('Ctrl Pts',(-30.7230062072929,-1.17674595862744,
0.162021797746519));
#60938=CARTESIAN_POINT('Ctrl Pts',(-30.7121328852638,-1.17605601445831,
0.000559203359190626));
#60939=CARTESIAN_POINT('Origin',(-35.5608671147362,0.,0.));
#60940=CARTESIAN_POINT('',(-31.8108671147362,-1.17581650239264,-0.000149915200615911));
#60941=CARTESIAN_POINT('',(-31.7121328852638,-1.17859056986776,-0.000953879663846968));
#60942=CARTESIAN_POINT('',(-35.5608671147362,-1.17775,1.38253677383905E-12));
#60943=CARTESIAN_POINT('Ctrl Pts',(-31.8108671147362,-1.17581650239264,
-0.000149915200616038));
#60944=CARTESIAN_POINT('Ctrl Pts',(-31.7982212165527,-1.1760291537976,-0.188029754032307));
#60945=CARTESIAN_POINT('Ctrl Pts',(-31.7590607759636,-1.0447823457967,-0.769555013578587));
#60946=CARTESIAN_POINT('Ctrl Pts',(-31.6933857929688,-0.131416651354211,
-1.38676868934885));
#60947=CARTESIAN_POINT('Ctrl Pts',(-31.6138421657517,1.09555509809422,-0.860323637389223));
#60948=CARTESIAN_POINT('Ctrl Pts',(-31.5342985385347,1.31606258565414,0.45648330161381));
#60949=CARTESIAN_POINT('Ctrl Pts',(-31.4547549113176,0.327530052156675,
1.35392828426963));
#60950=CARTESIAN_POINT('Ctrl Pts',(-31.3802777700514,-0.879768336219877,
1.02960936733916));
#60951=CARTESIAN_POINT('Ctrl Pts',(-31.332315171191,-1.17533307641041,0.315955705199351));
#60952=CARTESIAN_POINT('Ctrl Pts',(-31.3108671147362,-1.17824890665216,
-0.00103493412604934));
#60953=CARTESIAN_POINT('Ctrl Pts',(-31.7121328852638,-1.17859056986776,
-0.00095387966384702));
#60954=CARTESIAN_POINT('Ctrl Pts',(-31.7078473828277,-1.17914702414124,
-0.0642438336544744));
#60955=CARTESIAN_POINT('Ctrl Pts',(-31.677047337986,-1.14568168278089,-0.51852142935964));
#60956=CARTESIAN_POINT('Ctrl Pts',(-31.6197327507386,-0.554823606020508,
-1.27772002779702));
#60957=CARTESIAN_POINT('Ctrl Pts',(-31.5401891235215,0.774899618904291,
-1.1575527132071));
#60958=CARTESIAN_POINT('Ctrl Pts',(-31.4606454963045,1.39273827103593,0.0260348155934577));
#60959=CARTESIAN_POINT('Ctrl Pts',(-31.3811018690874,0.73109650415408,1.18570468702998));
#60960=CARTESIAN_POINT('Ctrl Pts',(-31.3015582418703,-0.602188801882199,
1.25609169654084));
#60961=CARTESIAN_POINT('Ctrl Pts',(-31.2452352472625,-1.154535882638,0.488848760380386));
#60962=CARTESIAN_POINT('Ctrl Pts',(-31.2154267950603,-1.17936813992108,
0.0494037989323538));
#60963=CARTESIAN_POINT('Ctrl Pts',(-31.2121328852638,-1.17898964596467,
0.000800932373318424));
#60964=CARTESIAN_POINT('Origin',(-35.5608671147362,0.,0.));
#60965=CARTESIAN_POINT('',(-32.3108671147362,-1.1776968972288,0.00108813574317774));
#60966=CARTESIAN_POINT('',(-32.2121328852638,-1.17588793485307,-0.000337024215327775));
#60967=CARTESIAN_POINT('',(-35.5608671147362,-1.17775,1.38253677383905E-12));
#60968=CARTESIAN_POINT('Ctrl Pts',(-32.3108671147362,-1.1776968972288,0.00108813574317767));
#60969=CARTESIAN_POINT('Ctrl Pts',(-32.2906418043202,-1.17493849100873,
-0.298190476586958));
#60970=CARTESIAN_POINT('Ctrl Pts',(-32.2439019514985,-0.906723625724865,
-0.994208119680003));
#60971=CARTESIAN_POINT('Ctrl Pts',(-32.1706475562712,0.264792959390405,
-1.3675826931817));
#60972=CARTESIAN_POINT('Ctrl Pts',(-32.0911039290541,1.29362979082703,-0.516642718223328));
#60973=CARTESIAN_POINT('Ctrl Pts',(-32.011560301837,1.1340351551021,0.808926449684369));
#60974=CARTESIAN_POINT('Ctrl Pts',(-31.93201667462,-0.0673745908983318,
1.39135128508784));
#60975=CARTESIAN_POINT('Ctrl Pts',(-31.8651189455863,-1.02572796862834,
0.806185680098539));
#60976=CARTESIAN_POINT('Ctrl Pts',(-31.8247357589584,-1.17558328948551,
0.20589623537659));
#60977=CARTESIAN_POINT('Ctrl Pts',(-31.8108671147362,-1.17581650239264,
-0.000149915200616038));
#60978=CARTESIAN_POINT('Ctrl Pts',(-32.2121328852638,-1.17588793485307,
-0.000337024215328035));
#60979=CARTESIAN_POINT('Ctrl Pts',(-32.2002679705952,-1.17633799208892,
-0.176587098471389));
#60980=CARTESIAN_POINT('Ctrl Pts',(-32.1618885135209,-1.05634314907566,
-0.746121290085078));
#60981=CARTESIAN_POINT('Ctrl Pts',(-32.096994514041,-0.172183573404041,
-1.38229899814921));
#60982=CARTESIAN_POINT('Ctrl Pts',(-32.0174508868238,1.06975396049637,-0.892201864620813));
#60983=CARTESIAN_POINT('Ctrl Pts',(-31.9379072596068,1.3289302146337,0.417543037140155));
#60984=CARTESIAN_POINT('Ctrl Pts',(-31.8583636323897,0.367245217795309,
1.34369961421373));
#60985=CARTESIAN_POINT('Ctrl Pts',(-31.7831055076088,-0.861831888195839,
1.05203514828171));
#60986=CARTESIAN_POINT('Ctrl Pts',(-31.7343619252334,-1.17570422352421,
0.327333162035316));
#60987=CARTESIAN_POINT('Ctrl Pts',(-31.7121328852638,-1.17859056986776,
-0.00095387966384702));
#60988=CARTESIAN_POINT('Origin',(-35.5608671147362,0.,0.));
#60989=CARTESIAN_POINT('',(-32.8108671147362,-1.17957184097153,-0.000350604622900076));
#60990=CARTESIAN_POINT('',(-32.7121328852638,-1.1773504918584,0.00107495084775092));
#60991=CARTESIAN_POINT('',(-35.5608671147362,-1.17775,1.38253677383905E-12));
#60992=CARTESIAN_POINT('Ctrl Pts',(-32.8108671147362,-1.17957184097153,
-0.000350604622899962));
#60993=CARTESIAN_POINT('Ctrl Pts',(-32.8095769344933,-1.17964627158723,
-0.0193629176176901));
#60994=CARTESIAN_POINT('Ctrl Pts',(-32.7817722118448,-1.17060124696026,
-0.429025645350123));
#60995=CARTESIAN_POINT('Ctrl Pts',(-32.7274529467905,-0.69526502492905,
-1.20706432189118));
#60996=CARTESIAN_POINT('Ctrl Pts',(-32.6479093195736,0.639530057869942,
-1.23749708685117));
#60997=CARTESIAN_POINT('Ctrl Pts',(-32.5683656923564,1.38680183990368,-0.131066360639972));
#60998=CARTESIAN_POINT('Ctrl Pts',(-32.4888220651394,0.860046881755779,
1.09577237368332));
#60999=CARTESIAN_POINT('Ctrl Pts',(-32.4092784379223,-0.456815713582613,
1.31594723981434));
#61000=CARTESIAN_POINT('Ctrl Pts',(-32.3499601211213,-1.1258839276056,0.578596770904729));
#61001=CARTESIAN_POINT('Ctrl Pts',(-32.3171563467259,-1.1785546470622,0.094151361166444));
#61002=CARTESIAN_POINT('Ctrl Pts',(-32.3108671147362,-1.1776968972288,0.00108813574317767));
#61003=CARTESIAN_POINT('Ctrl Pts',(-32.7121328852638,-1.1773504918584,0.00107495084775085));
#61004=CARTESIAN_POINT('Ctrl Pts',(-32.6926885583627,-1.17479524368154,
-0.28686294584429));
#61005=CARTESIAN_POINT('Ctrl Pts',(-32.6467296890558,-0.923231040420216,
-0.971431569472807));
#61006=CARTESIAN_POINT('Ctrl Pts',(-32.5742562773433,0.224419118509842,
-1.37478498777756));
#61007=CARTESIAN_POINT('Ctrl Pts',(-32.4947126501262,1.27786013090699,-0.554500846765326));
#61008=CARTESIAN_POINT('Ctrl Pts',(-32.4151690229092,1.15735694303011,0.775191982424803));
#61009=CARTESIAN_POINT('Ctrl Pts',(-32.3356253956921,-0.0263866089456238,
1.39273165043428));
#61010=CARTESIAN_POINT('Ctrl Pts',(-32.2679466831437,-1.01293516475784,
0.82953271490403));
#61011=CARTESIAN_POINT('Ctrl Pts',(-32.2267825130009,-1.17533224851651,
0.217279203848309));
#61012=CARTESIAN_POINT('Ctrl Pts',(-32.2121328852638,-1.17588793485307,
-0.000337024215328035));
#61013=CARTESIAN_POINT('Origin',(-35.5608671147362,0.,0.));
#61014=CARTESIAN_POINT('',(-33.3108671147362,-1.17663137595576,-0.000914001560779414));
#61015=CARTESIAN_POINT('',(-33.2121328852639,-1.179676948955,-0.000140904201940406));
#61016=CARTESIAN_POINT('',(-35.5608671147362,-1.17775,1.38253677383905E-12));
#61017=CARTESIAN_POINT('Ctrl Pts',(-33.3108671147362,-1.17663137595576,
-0.000914001560779511));
#61018=CARTESIAN_POINT('Ctrl Pts',(-33.3019975222608,-1.1775794950042,-0.132460896041139));
#61019=CARTESIAN_POINT('Ctrl Pts',(-33.2666133873797,-1.09644774808449,
-0.656115154141397));
#61020=CARTESIAN_POINT('Ctrl Pts',(-33.204714710093,-0.326846022470247,
-1.35409354000658));
#61021=CARTESIAN_POINT('Ctrl Pts',(-33.1251710828758,0.962406571507915,
-1.00706075074908));
#61022=CARTESIAN_POINT('Ctrl Pts',(-33.0456274556588,1.36751576661517,0.26513840054929));
#61023=CARTESIAN_POINT('Ctrl Pts',(-32.9660838284418,0.516315940709615,
1.29376024423113));
#61024=CARTESIAN_POINT('Ctrl Pts',(-32.8878303814675,-0.787713083824443,
1.1364248141512));
#61025=CARTESIAN_POINT('Ctrl Pts',(-32.836091476899,-1.17811664522137,0.371359837535488));
#61026=CARTESIAN_POINT('Ctrl Pts',(-32.8108671147362,-1.17957184097153,
-0.000350604622899962));
#61027=CARTESIAN_POINT('Ctrl Pts',(-33.2121328852639,-1.179676948955,-0.000140904201940543));
#61028=CARTESIAN_POINT('Ctrl Pts',(-33.2116236885358,-1.17968958197449,
-0.0076427229676073));
#61029=CARTESIAN_POINT('Ctrl Pts',(-33.1845999494021,-1.17622166758078,
-0.405762103065146));
#61030=CARTESIAN_POINT('Ctrl Pts',(-33.1310616678627,-0.730497410775578,
-1.1860738687982));
#61031=CARTESIAN_POINT('Ctrl Pts',(-33.0515180406456,0.602823280911789,
-1.25578732295739));
#61032=CARTESIAN_POINT('Ctrl Pts',(-32.9719744134286,1.38234244666654,-0.171834409267923));
#61033=CARTESIAN_POINT('Ctrl Pts',(-32.8924307862115,0.891931624897046,
1.06997928849094));
#61034=CARTESIAN_POINT('Ctrl Pts',(-32.8128871589945,-0.417878700488076,
1.32882470468588));
#61035=CARTESIAN_POINT('Ctrl Pts',(-32.7527878586786,-1.11745405938805,
0.602045511337059));
#61036=CARTESIAN_POINT('Ctrl Pts',(-32.7192031007684,-1.17827961403218,
0.105772994234821));
#61037=CARTESIAN_POINT('Ctrl Pts',(-32.7121328852638,-1.1773504918584,0.00107495084775085));
#61038=CARTESIAN_POINT('Origin',(-35.5608671147362,0.,0.));
#61039=CARTESIAN_POINT('',(-33.8108671147362,-1.17625258863493,0.000721924261463078));
#61040=CARTESIAN_POINT('',(-33.7121328852638,-1.17692552717653,-0.001004960261487));
#61041=CARTESIAN_POINT('',(-35.5608671147362,-1.17775,1.38253677383905E-12));
#61042=CARTESIAN_POINT('Ctrl Pts',(-33.8108671147362,-1.17625258863493,
0.000721924261462958));
#61043=CARTESIAN_POINT('Ctrl Pts',(-33.7944181100282,-1.17489470568404,
-0.243434697208882));
#61044=CARTESIAN_POINT('Ctrl Pts',(-33.7514545629146,-0.981561844828172,
-0.883125560569472));
#61045=CARTESIAN_POINT('Ctrl Pts',(-33.6819764733953,0.0680777368036397,
-1.39131546907066));
#61046=CARTESIAN_POINT('Ctrl Pts',(-33.6024328461782,1.20723976173548,-0.694960952389941));
#61047=CARTESIAN_POINT('Ctrl Pts',(-33.5228892189612,1.23733558104474,0.639843063744817));
#61048=CARTESIAN_POINT('Ctrl Pts',(-33.4433455917441,0.130716022946506,
1.38683466763195));
#61049=CARTESIAN_POINT('Ctrl Pts',(-33.3726715570025,-0.95920451437908,
0.918541050994175));
#61050=CARTESIAN_POINT('Ctrl Pts',(-33.3285120646665,-1.17474521115347,
0.260782166896676));
#61051=CARTESIAN_POINT('Ctrl Pts',(-33.3108671147362,-1.17663137595576,
-0.000914001560779511));
#61052=CARTESIAN_POINT('Ctrl Pts',(-33.7121328852638,-1.17692552717653,
-0.00100496026148728));
#61053=CARTESIAN_POINT('Ctrl Pts',(-33.7040442763033,-1.17789265561524,
-0.12089336944156));
#61054=CARTESIAN_POINT('Ctrl Pts',(-33.669441124937,-1.10584072736996,-0.632642166838988));
#61055=CARTESIAN_POINT('Ctrl Pts',(-33.6083234311651,-0.366566277470248,
-1.34388474473925));
#61056=CARTESIAN_POINT('Ctrl Pts',(-33.528779803948,0.932343436689741,-1.03495583798244));
#61057=CARTESIAN_POINT('Ctrl Pts',(-33.4492361767309,1.37472827927823,0.224766432947515));
#61058=CARTESIAN_POINT('Ctrl Pts',(-33.3696925495139,0.554178040687849,
1.2780001196717));
#61059=CARTESIAN_POINT('Ctrl Pts',(-33.2906581190248,-0.76697248715969,
1.15793466444302));
#61060=CARTESIAN_POINT('Ctrl Pts',(-33.2381382309415,-1.1790317640579,0.38298683302465));
#61061=CARTESIAN_POINT('Ctrl Pts',(-33.2121328852639,-1.179676948955,-0.000140904201940543));
#61062=CARTESIAN_POINT('Origin',(-35.5608671147362,0.,0.));
#61063=CARTESIAN_POINT('',(-34.3108671147362,-1.17925499677644,0.000722179416794065));
#61064=CARTESIAN_POINT('',(-34.2121328852638,-1.17605840265479,0.000574308414346136));
#61065=CARTESIAN_POINT('',(-35.5608671147362,-1.17775,1.38253677383905E-12));
#61066=CARTESIAN_POINT('Ctrl Pts',(-34.3108671147362,-1.17925499677644,
0.000722179416794018));
#61067=CARTESIAN_POINT('Ctrl Pts',(-34.2868386977957,-1.17693533461402,
-0.353580965932757));
#61068=CARTESIAN_POINT('Ctrl Pts',(-34.2362957384495,-0.818353920066329,
-1.10320287134604));
#61069=CARTESIAN_POINT('Ctrl Pts',(-34.1592382366976,0.457492926185055,
-1.31564139210814));
#61070=CARTESIAN_POINT('Ctrl Pts',(-34.0796946094806,1.3541695165413,-0.326543447000047));
#61071=CARTESIAN_POINT('Ctrl Pts',(-34.0001509822635,1.00682106773482,0.962681709799215));
#61072=CARTESIAN_POINT('Ctrl Pts',(-33.9206073550465,-0.265485630343504,
1.36743779586005));
#61073=CARTESIAN_POINT('Ctrl Pts',(-33.8575127325373,-1.0812236919471,0.692066684536782));
#61074=CARTESIAN_POINT('Ctrl Pts',(-33.8209326524339,-1.17708350954923,
0.150127175290172));
#61075=CARTESIAN_POINT('Ctrl Pts',(-33.8108671147362,-1.17625258863493,
0.000721924261462958));
#61076=CARTESIAN_POINT('Ctrl Pts',(-34.2121328852638,-1.17605840265479,
0.000574308414346206));
#61077=CARTESIAN_POINT('Ctrl Pts',(-34.1964648640707,-1.17505531307848,
-0.232088160436699));
#61078=CARTESIAN_POINT('Ctrl Pts',(-34.1542823004719,-0.995513626366357,
-0.85991809699752));
#61079=CARTESIAN_POINT('Ctrl Pts',(-34.0855851944674,0.0270938664892442,
-1.39270766067608));
#61080=CARTESIAN_POINT('Ctrl Pts',(-34.0060415672503,1.18625641663401,-0.730203319351427));
#61081=CARTESIAN_POINT('Ctrl Pts',(-33.9264979400333,1.25563603260232,0.603143373819632));
#61082=CARTESIAN_POINT('Ctrl Pts',(-33.8469543128163,0.171484699201278,
1.3823842729852));
#61083=CARTESIAN_POINT('Ctrl Pts',(-33.7754992945597,-0.943939764166423,
0.941562544723186));
#61084=CARTESIAN_POINT('Ctrl Pts',(-33.7305588187089,-1.17472239876083,
0.272102054697359));
#61085=CARTESIAN_POINT('Ctrl Pts',(-33.7121328852638,-1.17692552717653,
-0.00100496026148728));
#61086=CARTESIAN_POINT('Origin',(-0.2,3.28582941601228E-17,0.));
#61087=CARTESIAN_POINT('',(-0.2,1.38699088616441,0.466999498604503));
#61088=CARTESIAN_POINT('Ctrl Pts',(-0.2,-0.207979487136895,-1.16121778488279));
#61089=CARTESIAN_POINT('Ctrl Pts',(-0.199999999999999,-0.17996785785622,
-1.16987676038429));
#61090=CARTESIAN_POINT('Ctrl Pts',(-0.200000000000005,-0.151667340461406,
-1.17740349654605));
#61091=CARTESIAN_POINT('Ctrl Pts',(-0.200000000000004,-0.123132736344806,
-1.18376041834314));
#61092=CARTESIAN_POINT('Ctrl Pts',(-0.200000000000001,-0.0760735798974293,
-1.1942442286722));
#61093=CARTESIAN_POINT('Ctrl Pts',(-0.199999999999998,-0.0283788177258679,
-1.20154929893047));
#61094=CARTESIAN_POINT('Ctrl Pts',(-0.199999999999998,0.0196878622471927,
-1.20583213317713));
#61095=CARTESIAN_POINT('Ctrl Pts',(-0.199999999999998,0.0380691674922849,
-1.20746994306219));
#61096=CARTESIAN_POINT('Ctrl Pts',(-0.200000000000004,0.0565050987880124,
-1.2086652918681));
#61097=CARTESIAN_POINT('Ctrl Pts',(-0.200000000000004,0.0749816324965036,
-1.20942512509166));
#61098=CARTESIAN_POINT('Ctrl Pts',(-0.200000000000004,0.0864312154600023,
-1.20989598037592));
#61099=CARTESIAN_POINT('Ctrl Pts',(-0.200000000000005,0.09789848461842,
-1.21019959627083));
#61100=CARTESIAN_POINT('Ctrl Pts',(-0.200000000000005,0.109373451700485,
-1.21033736826952));
#61101=CARTESIAN_POINT('Ctrl Pts',(-0.200000000000004,0.159816976356299,
-1.2109430088054));
#61102=CARTESIAN_POINT('Ctrl Pts',(-0.199999999999996,0.21028424266955,
-1.20834757047201));
#61103=CARTESIAN_POINT('Ctrl Pts',(-0.199999999999995,0.260486404812435,
-1.20272430978437));
#61104=CARTESIAN_POINT('Ctrl Pts',(-0.199999999999995,0.296855798949691,
-1.19865048954325));
#61105=CARTESIAN_POINT('Ctrl Pts',(-0.199999999999997,0.333086695276272,
-1.19298646331018));
#61106=CARTESIAN_POINT('Ctrl Pts',(-0.199999999999996,0.369073996782841,
-1.18578183454027));
#61107=CARTESIAN_POINT('Ctrl Pts',(-0.199999999999995,0.384213139928643,
-1.18275099027872));
#61108=CARTESIAN_POINT('Ctrl Pts',(-0.199999999999998,0.399309200131859,
-1.17944734014573));
#61109=CARTESIAN_POINT('Ctrl Pts',(-0.199999999999998,0.414354411325149,
-1.17587387674941));
#61110=CARTESIAN_POINT('Ctrl Pts',(-0.199999999999997,0.427366804737433,
-1.17278323807642));
#61111=CARTESIAN_POINT('Ctrl Pts',(-0.199999999999993,0.440344323191234,
-1.16948974515456));
#61112=CARTESIAN_POINT('Ctrl Pts',(-0.199999999999993,0.453257211519439,
-1.16600226357088));
#61113=CARTESIAN_POINT('Ctrl Pts',(-0.199999999999993,0.503975772807244,
-1.15230431746102));
#61114=CARTESIAN_POINT('Ctrl Pts',(-0.199999999999988,0.5537718606903,-1.1356014144362));
#61115=CARTESIAN_POINT('Ctrl Pts',(-0.199999999999992,0.602349869633212,
-1.11606206524489));
#61116=CARTESIAN_POINT('Ctrl Pts',(-0.199999999999996,0.651837272735973,
-1.09615693387296));
#61117=CARTESIAN_POINT('Ctrl Pts',(-0.2,0.700061744369224,-1.07330810109062));
#61118=CARTESIAN_POINT('Ctrl Pts',(-0.2,0.746713474323926,-1.04764073086544));
#61119=CARTESIAN_POINT('Ctrl Pts',(-0.2,0.773395470711291,-1.03296053186132));
#61120=CARTESIAN_POINT('Ctrl Pts',(-0.199999999999994,0.799562953931442,
-1.01735738288161));
#61121=CARTESIAN_POINT('Ctrl Pts',(-0.199999999999993,0.825155999701759,
-1.00084728202755));
#61122=CARTESIAN_POINT('Ctrl Pts',(-0.199999999999992,0.84136793032273,
-0.990388948463293));
#61123=CARTESIAN_POINT('Ctrl Pts',(-0.199999999999994,0.857349325029275,
-0.979566585249447));
#61124=CARTESIAN_POINT('Ctrl Pts',(-0.199999999999994,0.873084385111579,
-0.968383188012168));
#61125=CARTESIAN_POINT('Ctrl Pts',(-0.199999999999993,0.880884272467831,
-0.962839565156282));
#61126=CARTESIAN_POINT('Ctrl Pts',(-0.199999999999998,0.888622356506473,
-0.95720800218513));
#61127=CARTESIAN_POINT('Ctrl Pts',(-0.199999999999998,0.89628698404453,
-0.951496475501582));
#61128=CARTESIAN_POINT('Ctrl Pts',(-0.199999999999999,0.940230294863368,
-0.918750801813058));
#61129=CARTESIAN_POINT('Ctrl Pts',(-0.2,0.981849241670539,-0.883317934714933));
#61130=CARTESIAN_POINT('Ctrl Pts',(-0.199999999999999,1.02082692352098,
-0.845344163653151));
#61131=CARTESIAN_POINT('Ctrl Pts',(-0.199999999999999,1.02628931308357,
-0.840022463622452));
#61132=CARTESIAN_POINT('Ctrl Pts',(-0.199999999999995,1.03169981019787,
-0.8346507797186));
#61133=CARTESIAN_POINT('Ctrl Pts',(-0.199999999999996,1.03705751954036,
-0.829229435958842));
#61134=CARTESIAN_POINT('Ctrl Pts',(-0.199999999999998,1.07393371359335,
-0.791915257131079));
#61135=CARTESIAN_POINT('Ctrl Pts',(-0.200000000000001,1.10831166419257,
-0.752252087056621));
#61136=CARTESIAN_POINT('Ctrl Pts',(-0.200000000000003,1.14017701794897,
-0.710537394505997));
#61137=CARTESIAN_POINT('Ctrl Pts',(-0.200000000000005,1.15714800209,-0.688320808079979));
#61138=CARTESIAN_POINT('Ctrl Pts',(-0.200000000000006,1.17340579040207,
-0.665521567859066));
#61139=CARTESIAN_POINT('Ctrl Pts',(-0.200000000000005,1.18894441677493,
-0.642180190235135));
#61140=CARTESIAN_POINT('Ctrl Pts',(-0.200000000000005,1.19826943417516,
-0.628172597333051));
#61141=CARTESIAN_POINT('Ctrl Pts',(-0.199999999999999,1.20733539801163,
-0.613969703735576));
#61142=CARTESIAN_POINT('Ctrl Pts',(-0.199999999999999,1.21614051436765,
-0.599579836608104));
#61143=CARTESIAN_POINT('Ctrl Pts',(-0.199999999999999,1.22219283654289,
-0.589688756423258));
#61144=CARTESIAN_POINT('Ctrl Pts',(-0.199999999999997,1.22812251980414,
-0.579707981684439));
#61145=CARTESIAN_POINT('Ctrl Pts',(-0.199999999999997,1.23391867616795,
-0.569658683741284));
#61146=CARTESIAN_POINT('Ctrl Pts',(-0.199999999999996,1.2613223359756,-0.522146586956005));
#61147=CARTESIAN_POINT('Ctrl Pts',(-0.199999999999998,1.28580053533619,
-0.473016095229739));
#61148=CARTESIAN_POINT('Ctrl Pts',(-0.199999999999998,1.30735107827001,
-0.422603250496398));
#61149=CARTESIAN_POINT('Ctrl Pts',(-0.199999999999998,1.32936794320409,
-0.371099546072548));
#61150=CARTESIAN_POINT('Ctrl Pts',(-0.200000000000001,1.34832961329657,
-0.318256565595133));
#61151=CARTESIAN_POINT('Ctrl Pts',(-0.200000000000001,1.36419558884076,
-0.264393162206011));
#61152=CARTESIAN_POINT('Ctrl Pts',(-0.200000000000001,1.37307857615403,
-0.234236306888627));
#61153=CARTESIAN_POINT('Ctrl Pts',(-0.200000000000008,1.38099045666224,
-0.203758954279961));
#61154=CARTESIAN_POINT('Ctrl Pts',(-0.200000000000009,1.38791810504401,
-0.173013380822985));
#61155=CARTESIAN_POINT('Ctrl Pts',(-0.200000000000009,1.39266339253719,
-0.151953336034936));
#61156=CARTESIAN_POINT('Ctrl Pts',(-0.200000000000011,1.3969467919497,-0.130767392506577));
#61157=CARTESIAN_POINT('Ctrl Pts',(-0.200000000000013,1.40076280465425,
-0.109471897823214));
#61158=CARTESIAN_POINT('Ctrl Pts',(-0.200000000000014,1.40337099863038,
-0.0949167101830787));
#61159=CARTESIAN_POINT('Ctrl Pts',(-0.199999999999992,1.40576157137632,
-0.0803042164079611));
#61160=CARTESIAN_POINT('Ctrl Pts',(-0.199999999999993,1.40792789131239,
-0.0656738373046273));
#61161=CARTESIAN_POINT('Ctrl Pts',(-0.199999999999995,1.41645918627998,
-0.00805719557944552));
#61162=CARTESIAN_POINT('Ctrl Pts',(-0.200000000000006,1.42153315207724,
0.0499141617019763));
#61163=CARTESIAN_POINT('Ctrl Pts',(-0.200000000000005,1.42311910879787,
0.107898749183097));
#61164=CARTESIAN_POINT('Ctrl Pts',(-0.200000000000003,1.42476833679356,
0.168196614660305));
#61165=CARTESIAN_POINT('Ctrl Pts',(-0.199999999999996,1.42264651610737,
0.22850989730486));
#61166=CARTESIAN_POINT('Ctrl Pts',(-0.199999999999997,1.41666493374304,
0.28847860395704));
#61167=CARTESIAN_POINT('Ctrl Pts',(-0.199999999999998,1.41105131042735,
0.344758315473251));
#61168=CARTESIAN_POINT('Ctrl Pts',(-0.199999999999995,1.40203806422657,
0.400735686869312));
#61169=CARTESIAN_POINT('Ctrl Pts',(-0.199999999999995,1.38950159942899,
0.456116958127017));
#61170=CARTESIAN_POINT('Ctrl Pts',(-0.199999999999995,1.38867986533664,
0.459747062738241));
#61171=CARTESIAN_POINT('Ctrl Pts',(-0.2,1.38784297517085,0.463374604186691));
#61172=CARTESIAN_POINT('Ctrl Pts',(-0.2,1.38699088616441,0.466999498604503));
#61173=CARTESIAN_POINT('',(-0.2,-1.79227059055215E-16,1.4635));
#61174=CARTESIAN_POINT('Origin',(-0.2,0.,0.));
#61175=CARTESIAN_POINT('',(-0.2,0.501864481801965,1.37604662611724));
#61176=CARTESIAN_POINT('Origin',(-0.2,0.,0.));
#61177=CARTESIAN_POINT('Ctrl Pts',(-0.2,0.50202173509711,1.37727613462792));
#61178=CARTESIAN_POINT('Ctrl Pts',(-0.2,0.467209610033743,1.38655883583692));
#61179=CARTESIAN_POINT('Ctrl Pts',(-0.199999999999991,0.432087726974528,
1.39445148143947));
#61180=CARTESIAN_POINT('Ctrl Pts',(-0.199999999999991,0.396707563583374,
1.40089474981437));
#61181=CARTESIAN_POINT('Ctrl Pts',(-0.19999999999999,0.33987401238208,1.41124500792484));
#61182=CARTESIAN_POINT('Ctrl Pts',(-0.200000000000006,0.282373290930486,
1.417857743763));
#61183=CARTESIAN_POINT('Ctrl Pts',(-0.200000000000005,0.224536309947567,
1.42084361738228));
#61184=CARTESIAN_POINT('Ctrl Pts',(-0.200000000000004,0.194463123061523,
1.42239616618141));
#61185=CARTESIAN_POINT('Ctrl Pts',(-0.2,0.164299125551568,1.42296729002729));
#61186=CARTESIAN_POINT('Ctrl Pts',(-0.199999999999999,0.134092360305547,
1.42256735698774));
#61187=CARTESIAN_POINT('Ctrl Pts',(-0.199999999999998,0.121186218285078,
1.42239648160386));
#61188=CARTESIAN_POINT('Ctrl Pts',(-0.199999999999994,0.108271378161479,
1.42204813448602));
#61189=CARTESIAN_POINT('Ctrl Pts',(-0.199999999999994,0.0953682127448282,
1.42152399163123));
#61190=CARTESIAN_POINT('Ctrl Pts',(-0.199999999999996,0.0378376022185237,
1.41918702566471));
#61191=CARTESIAN_POINT('Ctrl Pts',(-0.200000000000007,-0.0195396042662414,
1.41335923195479));
#61192=CARTESIAN_POINT('Ctrl Pts',(-0.200000000000003,-0.0764338051951725,
1.40414978072417));
#61193=CARTESIAN_POINT('Ctrl Pts',(-0.2,-0.114252001240382,1.39802815802059));
#61194=CARTESIAN_POINT('Ctrl Pts',(-0.199999999999994,-0.15185661385594,
1.39041128430496));
#61195=CARTESIAN_POINT('Ctrl Pts',(-0.199999999999992,-0.189145373564116,
1.38131971234083));
#61196=CARTESIAN_POINT('Ctrl Pts',(-0.199999999999991,-0.204522753083807,
1.37757047118567));
#61197=CARTESIAN_POINT('Ctrl Pts',(-0.199999999999998,-0.219846350113962,
1.37357033828829));
#61198=CARTESIAN_POINT('Ctrl Pts',(-0.199999999999998,-0.235108670748314,
1.36932034708906));
#61199=CARTESIAN_POINT('Ctrl Pts',(-0.199999999999998,-0.248545656240996,
1.36557864414255));
#61200=CARTESIAN_POINT('Ctrl Pts',(-0.199999999999987,-0.261938666183503,
1.3616420272537));
#61201=CARTESIAN_POINT('Ctrl Pts',(-0.199999999999987,-0.275257297963859,
1.35751930035212));
#61202=CARTESIAN_POINT('Ctrl Pts',(-0.199999999999989,-0.329002504954751,
1.34088269575589));
#61203=CARTESIAN_POINT('Ctrl Pts',(-0.2,-0.381618224871022,1.32119875338036));
#61204=CARTESIAN_POINT('Ctrl Pts',(-0.200000000000001,-0.432796645025925,
1.29856457497461));
#61205=CARTESIAN_POINT('Ctrl Pts',(-0.200000000000002,-0.482685261313613,
1.27650082548696));
#61206=CARTESIAN_POINT('Ctrl Pts',(-0.200000000000003,-0.531208941724398,
1.25163303504481));
#61207=CARTESIAN_POINT('Ctrl Pts',(-0.200000000000002,-0.57805281350073,
1.22401270646073));
#61208=CARTESIAN_POINT('Ctrl Pts',(-0.200000000000002,-0.605369225972023,
1.20790626052479));
#61209=CARTESIAN_POINT('Ctrl Pts',(-0.199999999999991,-0.632113797838164,
1.19086314281957));
#61210=CARTESIAN_POINT('Ctrl Pts',(-0.199999999999989,-0.658217585593046,
1.17288853171812));
#61211=CARTESIAN_POINT('Ctrl Pts',(-0.199999999999988,-0.675175610796268,
1.16121153254318));
#61212=CARTESIAN_POINT('Ctrl Pts',(-0.199999999999995,-0.691863102147501,
1.14914134267626));
#61213=CARTESIAN_POINT('Ctrl Pts',(-0.199999999999995,-0.708259846095076,
1.13667865309989));
#61214=CARTESIAN_POINT('Ctrl Pts',(-0.199999999999994,-0.718423561459792,
1.12895350779433));
#61215=CARTESIAN_POINT('Ctrl Pts',(-0.200000000000005,-0.72847844599448,
1.12107500079026));
#61216=CARTESIAN_POINT('Ctrl Pts',(-0.200000000000005,-0.738398879101225,
1.11306041296684));
#61217=CARTESIAN_POINT('Ctrl Pts',(-0.200000000000004,-0.779407630315877,
1.07992998059534));
#61218=CARTESIAN_POINT('Ctrl Pts',(-0.199999999999987,-0.818192292478104,
1.04442585590619));
#61219=CARTESIAN_POINT('Ctrl Pts',(-0.199999999999988,-0.854466407805115,
1.00660336811821));
#61220=CARTESIAN_POINT('Ctrl Pts',(-0.199999999999988,-0.860634784543826,
1.00017169220363));
#61221=CARTESIAN_POINT('Ctrl Pts',(-0.199999999999995,-0.866730468954246,
0.993672901300179));
#61222=CARTESIAN_POINT('Ctrl Pts',(-0.199999999999996,-0.872751928881112,
0.987107177684735));
#61223=CARTESIAN_POINT('Ctrl Pts',(-0.2,-0.908388068815388,0.94824998219203));
#61224=CARTESIAN_POINT('Ctrl Pts',(-0.200000000000001,-0.941428229725658,
0.907049875606388));
#61225=CARTESIAN_POINT('Ctrl Pts',(-0.2,-0.971787759829015,0.863805062866217));
#61226=CARTESIAN_POINT('Ctrl Pts',(-0.199999999999999,-0.986409690306514,
0.842977248889962));
#61227=CARTESIAN_POINT('Ctrl Pts',(-0.2,-1.00040912668513,0.821674881056962));
#61228=CARTESIAN_POINT('Ctrl Pts',(-0.2,-1.01377269674601,0.799930439499796));
#61229=CARTESIAN_POINT('Ctrl Pts',(-0.2,-1.02415577823187,0.783035679527426));
#61230=CARTESIAN_POINT('Ctrl Pts',(-0.200000000000001,-1.03415494874593,
0.765874035875678));
#61231=CARTESIAN_POINT('Ctrl Pts',(-0.2,-1.04376284041761,0.748460746768354));
#61232=CARTESIAN_POINT('Ctrl Pts',(-0.2,-1.04834541507807,0.740155314094317));
#61233=CARTESIAN_POINT('Ctrl Pts',(-0.199999999999998,-1.05283734842709,
0.731795409508619));
#61234=CARTESIAN_POINT('Ctrl Pts',(-0.199999999999997,-1.05723350309492,
0.72339177859167));
#61235=CARTESIAN_POINT('Ctrl Pts',(-0.199999999999995,-1.08157589449212,
0.676859186270714));
#61236=CARTESIAN_POINT('Ctrl Pts',(-0.199999999999994,-1.10302971579605,
0.628908125843251));
#61237=CARTESIAN_POINT('Ctrl Pts',(-0.199999999999993,-1.12153136716694,
0.579842458254082));
#61238=CARTESIAN_POINT('Ctrl Pts',(-0.199999999999993,-1.13995375954158,
0.530986982473522));
#61239=CARTESIAN_POINT('Ctrl Pts',(-0.199999999999998,-1.15544931532854,
0.481025232927459));
#61240=CARTESIAN_POINT('Ctrl Pts',(-0.2,-1.16790446064798,0.430251413185659));
#61241=CARTESIAN_POINT('Ctrl Pts',(-0.200000000000002,-1.17443020194359,
0.403649008819676));
#61242=CARTESIAN_POINT('Ctrl Pts',(-0.2,-1.18012045949723,0.376823695199568));
#61243=CARTESIAN_POINT('Ctrl Pts',(-0.200000000000001,-1.18495316181998,
0.349818803045841));
#61244=CARTESIAN_POINT('Ctrl Pts',(-0.200000000000001,-1.18825456893228,
0.33137070981168));
#61245=CARTESIAN_POINT('Ctrl Pts',(-0.199999999999997,-1.19115569092218,
0.312838829634385));
#61246=CARTESIAN_POINT('Ctrl Pts',(-0.199999999999997,-1.19364840917177,
0.294237378020598));
#61247=CARTESIAN_POINT('Ctrl Pts',(-0.199999999999996,-1.19498882449599,
0.284234775119132));
#61248=CARTESIAN_POINT('Ctrl Pts',(-0.199999999999996,-1.19621114658957,
0.274210923601008));
#61249=CARTESIAN_POINT('Ctrl Pts',(-0.199999999999996,-1.19731245520782,
0.264185232341623));
#61250=CARTESIAN_POINT('Ctrl Pts',(-0.199999999999996,-1.20281983502613,
0.214049158954717));
#61251=CARTESIAN_POINT('Ctrl Pts',(-0.200000000000007,-1.20531936750276,
0.163767737011937));
#61252=CARTESIAN_POINT('Ctrl Pts',(-0.200000000000006,-1.2047212293548,
0.113609796366066));
#61253=CARTESIAN_POINT('Ctrl Pts',(-0.200000000000005,-1.20413275350728,
0.0642621051471473));
#61254=CARTESIAN_POINT('Ctrl Pts',(-0.200000000000007,-1.20054580644529,
0.0150329753455555));
#61255=CARTESIAN_POINT('Ctrl Pts',(-0.200000000000009,-1.19382633959115,
-0.0338080607322077));
#61256=CARTESIAN_POINT('Ctrl Pts',(-0.200000000000011,-1.18710687273702,
-0.0826490968099709));
#61257=CARTESIAN_POINT('Ctrl Pts',(-0.200000000000001,-1.17725493947779,
-0.131102982562808));
#61258=CARTESIAN_POINT('Ctrl Pts',(-0.2,-1.1640875192389,-0.178872328917063));
#61259=CARTESIAN_POINT('Ctrl Pts',(-34.8014778394209,-0.510216505387977,
1.0614961988296));
#61260=CARTESIAN_POINT('Ctrl Pts',(-34.7749632970153,-0.863898086752264,
0.891496362124812));
#61261=CARTESIAN_POINT('Ctrl Pts',(-34.7219342122039,-1.38177714701916,
0.173082322994189));
#61262=CARTESIAN_POINT('Ctrl Pts',(-34.6423905849868,-0.891720964097157,
-1.07138127409762));
#61263=CARTESIAN_POINT('Ctrl Pts',(-34.5628469577698,0.41872224072349,-1.32812088037402));
#61264=CARTESIAN_POINT('Ctrl Pts',(-34.4833033305527,1.34388692616717,-0.366485362373245));
#61265=CARTESIAN_POINT('Ctrl Pts',(-34.4037597033356,1.03476789300364,0.932740929113639));
#61266=CARTESIAN_POINT('Ctrl Pts',(-34.3242160761186,-0.225138742279001,
1.37459976780186));
#61267=CARTESIAN_POINT('Ctrl Pts',(-34.2446724489015,-1.27812685049181,
0.55389298243285));
#61268=CARTESIAN_POINT('Ctrl Pts',(-34.1651288216845,-1.1569721580061,-0.775796455775922));
#61269=CARTESIAN_POINT('Ctrl Pts',(-34.0855851944674,0.0270938664892442,
-1.39270766067608));
#61270=CARTESIAN_POINT('Ctrl Pts',(-34.0060415672503,1.18625641663401,-0.730203319351427));
#61271=CARTESIAN_POINT('Ctrl Pts',(-33.9264979400333,1.25563603260232,0.603143373819632));
#61272=CARTESIAN_POINT('Ctrl Pts',(-33.8469543128163,0.171484699201278,
1.3823842729852));
#61273=CARTESIAN_POINT('Ctrl Pts',(-33.7674106855991,-1.07020426635795,
0.891662136491004));
#61274=CARTESIAN_POINT('Ctrl Pts',(-33.6878670583821,-1.32871925846032,
-0.418214763006971));
#61275=CARTESIAN_POINT('Ctrl Pts',(-33.6083234311651,-0.366566277470248,
-1.34388474473925));
#61276=CARTESIAN_POINT('Ctrl Pts',(-33.528779803948,0.932343436689741,-1.03495583798244));
#61277=CARTESIAN_POINT('Ctrl Pts',(-33.4492361767309,1.37472827927823,0.224766432947515));
#61278=CARTESIAN_POINT('Ctrl Pts',(-33.3696925495139,0.554178040687849,
1.2780001196717));
#61279=CARTESIAN_POINT('Ctrl Pts',(-33.2901489222968,-0.775484290456672,
1.15716111629985));
#61280=CARTESIAN_POINT('Ctrl Pts',(-33.2106052950798,-1.39272494414946,
-0.0267384097234227));
#61281=CARTESIAN_POINT('Ctrl Pts',(-33.1310616678627,-0.730497410775578,
-1.1860738687982));
#61282=CARTESIAN_POINT('Ctrl Pts',(-33.0515180406456,0.602823280911789,
-1.25578732295739));
#61283=CARTESIAN_POINT('Ctrl Pts',(-32.9719744134286,1.38234244666654,-0.171834409267923));
#61284=CARTESIAN_POINT('Ctrl Pts',(-32.8924307862115,0.891931624897046,
1.06997928849094));
#61285=CARTESIAN_POINT('Ctrl Pts',(-32.8128871589945,-0.417878700488076,
1.32882470468588));
#61286=CARTESIAN_POINT('Ctrl Pts',(-32.7333435317774,-1.34379233452526,
0.366905798459168));
#61287=CARTESIAN_POINT('Ctrl Pts',(-32.6537999045604,-1.03519118905535,
-0.932082027005969));
#61288=CARTESIAN_POINT('Ctrl Pts',(-32.5742562773433,0.224419118509842,
-1.37478498777756));
#61289=CARTESIAN_POINT('Ctrl Pts',(-32.4947126501262,1.27786013090699,-0.554500846765326));
#61290=CARTESIAN_POINT('Ctrl Pts',(-32.4151690229092,1.15735694303011,0.775191982424803));
#61291=CARTESIAN_POINT('Ctrl Pts',(-32.3356253956921,-0.0263866089456238,
1.39273165043428));
#61292=CARTESIAN_POINT('Ctrl Pts',(-32.2560817684751,-1.18588931814518,
0.730796981615063));
#61293=CARTESIAN_POINT('Ctrl Pts',(-32.1765381412579,-1.25593954855088,
-0.602506061058643));
#61294=CARTESIAN_POINT('Ctrl Pts',(-32.096994514041,-0.172183573404041,
-1.38229899814921));
#61295=CARTESIAN_POINT('Ctrl Pts',(-32.0174508868238,1.06975396049637,-0.892201864620813));
#61296=CARTESIAN_POINT('Ctrl Pts',(-31.9379072596068,1.3289302146337,0.417543037140155));
#61297=CARTESIAN_POINT('Ctrl Pts',(-31.8583636323897,0.367245217795309,
1.34369961421373));
#61298=CARTESIAN_POINT('Ctrl Pts',(-31.7788200051727,-0.931820516628637,
1.03542659228985));
#61299=CARTESIAN_POINT('Ctrl Pts',(-31.6992763779556,-1.37484163028206,
-0.224071852035116));
#61300=CARTESIAN_POINT('Ctrl Pts',(-31.6197327507386,-0.554823606020508,
-1.27772002779702));
#61301=CARTESIAN_POINT('Ctrl Pts',(-31.5401891235215,0.774899618904291,
-1.1575527132071));
#61302=CARTESIAN_POINT('Ctrl Pts',(-31.4606454963045,1.39273827103593,0.0260348155934577));
#61303=CARTESIAN_POINT('Ctrl Pts',(-31.3811018690874,0.73109650415408,1.18570468702998));
#61304=CARTESIAN_POINT('Ctrl Pts',(-31.3015582418703,-0.602188801882199,
1.25609169654084));
#61305=CARTESIAN_POINT('Ctrl Pts',(-31.2220146146532,-1.38225546190224,
0.172532725222116));
#61306=CARTESIAN_POINT('Ctrl Pts',(-31.1424709874362,-0.892472047174996,
-1.06952856354678));
#61307=CARTESIAN_POINT('Ctrl Pts',(-31.0629273602191,0.417207347022933,
-1.32903564016216));
#61308=CARTESIAN_POINT('Ctrl Pts',(-30.9833837330021,1.34360680823865,-0.367584613505395));
#61309=CARTESIAN_POINT('Ctrl Pts',(-30.903840105785,1.03566192942565,0.931558946696078));
#61310=CARTESIAN_POINT('Ctrl Pts',(-30.824296478568,-0.223724571245162,
1.3748981851222));
#61311=CARTESIAN_POINT('Ctrl Pts',(-30.7447528513509,-1.27757984317515,
0.555146329848009));
#61312=CARTESIAN_POINT('Ctrl Pts',(-30.6652092241338,-1.15774840952399,
-0.774607205928161));
#61313=CARTESIAN_POINT('Ctrl Pts',(-30.5856655969168,0.0256830205774446,
-1.39274480278519));
#61314=CARTESIAN_POINT('Ctrl Pts',(-30.5061219696997,1.18551998026519,-0.731395980043076));
#61315=CARTESIAN_POINT('Ctrl Pts',(-30.4265783424827,1.25624376438813,0.601871504282349));
#61316=CARTESIAN_POINT('Ctrl Pts',(-30.3470347152656,0.172881866032571,
1.38221183746495));
#61317=CARTESIAN_POINT('Ctrl Pts',(-30.2674910880486,-1.0693030983587,0.892742172786554));
#61318=CARTESIAN_POINT('Ctrl Pts',(-30.1879474608315,-1.3291409808946,-0.416871630286474));
#61319=CARTESIAN_POINT('Ctrl Pts',(-30.1084038336144,-0.367923985762689,
-1.34351391653814));
#61320=CARTESIAN_POINT('Ctrl Pts',(-30.0288602063974,0.931297317327677,
-1.03589720048344));
#61321=CARTESIAN_POINT('Ctrl Pts',(-29.9493165791803,1.37495465224026,0.223377276180953));
#61322=CARTESIAN_POINT('Ctrl Pts',(-29.8697729519633,0.555469018255743,
1.2774395770404));
#61323=CARTESIAN_POINT('Ctrl Pts',(-29.7902293247462,-0.774314743530089,
1.15794403197352));
#61324=CARTESIAN_POINT('Ctrl Pts',(-29.7106856975291,-1.39275124567373,
-0.02533122392278));
#61325=CARTESIAN_POINT('Ctrl Pts',(-29.6311420703121,-0.731695409267114,
-1.18533519786117));
#61326=CARTESIAN_POINT('Ctrl Pts',(-29.551598443095,0.601554168281548,-1.25639575208381));
#61327=CARTESIAN_POINT('Ctrl Pts',(-29.4720548158779,1.38216812483898,-0.173230995812698));
#61328=CARTESIAN_POINT('Ctrl Pts',(-29.3925111886609,0.893012241438832,
1.06907756494632));
#61329=CARTESIAN_POINT('Ctrl Pts',(-29.3129675614438,-0.416535886952527,
1.3292462368244));
#61330=CARTESIAN_POINT('Ctrl Pts',(-29.2334239342268,-1.34342093911796,
0.368263334545493));
#61331=CARTESIAN_POINT('Ctrl Pts',(-29.1538803070097,-1.03613240544832,
-0.93103562854009));
#61332=CARTESIAN_POINT('Ctrl Pts',(-29.0743366797926,0.223029966864688,
-1.37501103163265));
#61333=CARTESIAN_POINT('Ctrl Pts',(-28.9947930525756,1.27729922940169,-0.555791671223127));
#61334=CARTESIAN_POINT('Ctrl Pts',(-28.9152494253585,1.15813958054323,0.774022231728725));
#61335=CARTESIAN_POINT('Ctrl Pts',(-28.8357057981415,-0.0249794256519103,
1.39275759970113));
#61336=CARTESIAN_POINT('Ctrl Pts',(-28.7561621709244,-1.18515033982969,
0.7319947918071));
#61337=CARTESIAN_POINT('Ctrl Pts',(-28.6766185437074,-1.2565476596182,-0.601236793900022));
#61338=CARTESIAN_POINT('Ctrl Pts',(-28.5970749164903,-0.173580114540252,
-1.38212432402709));
#61339=CARTESIAN_POINT('Ctrl Pts',(-28.5175312892732,1.06885196332402,-0.893282253114629));
#61340=CARTESIAN_POINT('Ctrl Pts',(-28.4379876620562,1.32935140794485,0.416200117042506));
#61341=CARTESIAN_POINT('Ctrl Pts',(-28.3584440348391,0.36860265983214,1.34332787598405));
#61342=CARTESIAN_POINT('Ctrl Pts',(-28.278900407622,-0.930773880350019,
1.03636754430526));
#61343=CARTESIAN_POINT('Ctrl Pts',(-28.199356780405,-1.37506732329578,-0.222682643318531));
#61344=CARTESIAN_POINT('Ctrl Pts',(-28.1198131531879,-0.556114288729563,
-1.27715880026799));
#61345=CARTESIAN_POINT('Ctrl Pts',(-28.0402695259709,0.773729670542738,
-1.15833505522063));
#61346=CARTESIAN_POINT('Ctrl Pts',(-27.9607258987538,1.39276386486699,0.0246276257872868));
#61347=CARTESIAN_POINT('Ctrl Pts',(-27.8811822715368,0.732294127643924,
1.18496540618255));
#61348=CARTESIAN_POINT('Ctrl Pts',(-27.8016386443197,-0.600919381158034,
1.25669948698159));
#61349=CARTESIAN_POINT('Ctrl Pts',(-27.7220950171026,-1.3820804350321,0.173929222192942));
#61350=CARTESIAN_POINT('Ctrl Pts',(-27.6425513898856,-0.893552207796699,
-1.06862629350621));
#61351=CARTESIAN_POINT('Ctrl Pts',(-27.5630077626685,0.415864320577861,
-1.32945649424924));
#61352=CARTESIAN_POINT('Ctrl Pts',(-27.4834641354515,1.34323472714235,-0.368941961600966));
#61353=CARTESIAN_POINT('Ctrl Pts',(-27.4039205082344,1.03660261703927,0.930512072774181));
#61354=CARTESIAN_POINT('Ctrl Pts',(-27.3243768810174,-0.222335305564666,
1.37512352722605));
#61355=CARTESIAN_POINT('Ctrl Pts',(-27.2448332538003,-1.27701828964825,
0.556436870754451));
#61356=CARTESIAN_POINT('Ctrl Pts',(-27.1652896265832,-1.15853045599325,
-0.773437059990814));
#61357=CARTESIAN_POINT('Ctrl Pts',(-27.0857459993661,0.0242758243513772,
-1.39277004117091));
#61358=CARTESIAN_POINT('Ctrl Pts',(-27.0062023721491,1.18478039693156,-0.732593416758471));
#61359=CARTESIAN_POINT('Ctrl Pts',(-26.926658744932,1.2568512341643,0.60060193007585));
#61360=CARTESIAN_POINT('Ctrl Pts',(-26.847115117715,0.174278318748489,1.38203645785679));
#61361=CARTESIAN_POINT('Ctrl Pts',(-26.7675714904979,-1.06840055550726,
0.893822105467825));
#61362=CARTESIAN_POINT('Ctrl Pts',(-26.6880278632809,-1.32956149573086,
-0.415528497579976));
#61363=CARTESIAN_POINT('Ctrl Pts',(-26.6084842360638,-0.369281239830358,
-1.34314149259879));
#61364=CARTESIAN_POINT('Ctrl Pts',(-26.5289406088467,0.930250205829247,
-1.03683762363535));
#61365=CARTESIAN_POINT('Ctrl Pts',(-26.4493969816297,1.37517964341989,0.221987953625214));
#61366=CARTESIAN_POINT('Ctrl Pts',(-26.3698533544126,0.556759417277243,
1.27687769755144));
#61367=CARTESIAN_POINT('Ctrl Pts',(-26.2903097271956,-0.773144400091584,
1.15872578284863));
#61368=CARTESIAN_POINT('Ctrl Pts',(-26.2107660999785,-1.39277612861249,
-0.0239240213665873));
#61369=CARTESIAN_POINT('Ctrl Pts',(-26.1312224727615,-0.732892659131677,
-1.1845953120885));
#61370=CARTESIAN_POINT('Ctrl Pts',(-26.0516788455444,0.600284440673691,
-1.25700290115665));
#61371=CARTESIAN_POINT('Ctrl Pts',(-25.9721352183273,1.38199239250399,-0.174627404184641));
#61372=CARTESIAN_POINT('Ctrl Pts',(-25.8925915911103,0.894091946110794,
1.06817474934159));
#61373=CARTESIAN_POINT('Ctrl Pts',(-25.8130479638932,-0.415192648070296,
1.32966641238302));
#61374=CARTESIAN_POINT('Ctrl Pts',(-25.7335043366761,-1.34304817235933,
0.369620494498651));
#61375=CARTESIAN_POINT('Ctrl Pts',(-25.6539607094591,-1.03707256407851,
-0.929988279531947));
#61376=CARTESIAN_POINT('Ctrl Pts',(-25.574417082242,0.221640587522368,-1.3752356718737));
#61377=CARTESIAN_POINT('Ctrl Pts',(-25.494873455025,1.27673702398653,-0.557081928277323));
#61378=CARTESIAN_POINT('Ctrl Pts',(-25.4153298278079,1.1589210357743,0.772851690863756));
#61379=CARTESIAN_POINT('Ctrl Pts',(-25.3357862005909,-0.0235722168554084,
1.39278212719136));
#61380=CARTESIAN_POINT('Ctrl Pts',(-25.2562425733738,-1.18441015166521,
0.733191854744411));
#61381=CARTESIAN_POINT('Ctrl Pts',(-25.1766989461567,-1.25715448794894,
-0.599966912971858));
#61382=CARTESIAN_POINT('Ctrl Pts',(-25.0971553189397,-0.174976478479087,
-1.38194823897649));
#61383=CARTESIAN_POINT('Ctrl Pts',(-25.0176116917226,1.06794887502363,-0.894361729708357));
#61384=CARTESIAN_POINT('Ctrl Pts',(-24.9380680645055,1.32977124419901,0.414856772070276));
#61385=CARTESIAN_POINT('Ctrl Pts',(-24.8585244372885,0.369959725584168,
1.34295476642992));
#61386=CARTESIAN_POINT('Ctrl Pts',(-24.7789808100714,-0.929726293898997,
1.03730743835374));
#61387=CARTESIAN_POINT('Ctrl Pts',(-24.6994371828544,-1.37529161258391,
-0.221293207278282));
#61388=CARTESIAN_POINT('Ctrl Pts',(-24.6198935556373,-0.557404403734147,
-1.27659626896248));
#61389=CARTESIAN_POINT('Ctrl Pts',(-24.5403499284203,0.772558932325985,
-1.15911621475782));
#61390=CARTESIAN_POINT('Ctrl Pts',(-24.4608063012032,1.39278803690711,0.0232204108402372));
#61391=CARTESIAN_POINT('Ctrl Pts',(-24.3812626739862,0.733491003577628,
1.18422491567347));
#61392=CARTESIAN_POINT('Ctrl Pts',(-24.3017190467691,-0.599649346990552,
1.25730599453155));
#61393=CARTESIAN_POINT('Ctrl Pts',(-24.222175419552,-1.38190399727711,0.175325541609601));
#61394=CARTESIAN_POINT('Ctrl Pts',(-24.142631792335,-0.894631456243355,
-1.06772293256774));
#61395=CARTESIAN_POINT('Ctrl Pts',(-24.0630881651179,0.4145208696013,-1.32987599117216));
#61396=CARTESIAN_POINT('Ctrl Pts',(-23.9835445379008,1.34286127481651,-0.370298933065331));
#61397=CARTESIAN_POINT('Ctrl Pts',(-23.9040009106838,1.03754224644608,0.929464248947089));
#61398=CARTESIAN_POINT('Ctrl Pts',(-23.8244572834667,-0.220945812915096,
1.37534746554696));
#61399=CARTESIAN_POINT('Ctrl Pts',(-23.7449136562496,-1.27645543248829,
0.557726843627128));
#61400=CARTESIAN_POINT('Ctrl Pts',(-23.6653700290326,-1.15931131978672,
-0.772266124496938));
#61401=CARTESIAN_POINT('Ctrl Pts',(-23.5858264018155,0.0228686033435479,
-1.39279385775939));
#61402=CARTESIAN_POINT('Ctrl Pts',(-23.5062827745985,1.18403960412511,-0.733790105612224));
#61403=CARTESIAN_POINT('Ctrl Pts',(-23.4267391473814,1.25745742089477,0.599331742750071));
#61404=CARTESIAN_POINT('Ctrl Pts',(-23.3471955201644,0.175674593553903,
1.38185966740868));
#61405=CARTESIAN_POINT('Ctrl Pts',(-23.2676518929473,-1.06749692198837,
0.894901125698542));
#61406=CARTESIAN_POINT('Ctrl Pts',(-23.1881082657303,-1.32998065329578,
-0.41418494068481));
#61407=CARTESIAN_POINT('Ctrl Pts',(-23.1085646385132,-0.370638116920458,
-1.34276769752508));
#61408=CARTESIAN_POINT('Ctrl Pts',(-23.0290210112962,0.929202144692953,
-1.03777698834055));
#61409=CARTESIAN_POINT('Ctrl Pts',(-22.949477384079,1.37540323075928,0.220598404455005));
#61410=CARTESIAN_POINT('Ctrl Pts',(-22.869933756862,0.558049247935703,1.27631451457294));
#61411=CARTESIAN_POINT('Ctrl Pts',(-22.7903901296449,-0.771973267395321,
1.15950635084856));
#61412=CARTESIAN_POINT('Ctrl Pts',(-22.7108465024279,-1.39279958974781,
-0.0225167943877718));
#61413=CARTESIAN_POINT('Ctrl Pts',(-22.6313028752108,-0.734089160829106,
-1.18385421703197));
#61414=CARTESIAN_POINT('Ctrl Pts',(-22.5517592479938,0.59901410027068,-1.25760876702895));
#61415=CARTESIAN_POINT('Ctrl Pts',(-22.4722156207767,1.38181524937403,-0.176023634289684));
#61416=CARTESIAN_POINT('Ctrl Pts',(-22.3926719935596,0.89517073805671,1.06727084329994));
#61417=CARTESIAN_POINT('Ctrl Pts',(-22.3131283663426,-0.413848985342271,
1.33008523056319));
#61418=CARTESIAN_POINT('Ctrl Pts',(-22.2335847391255,-1.3426740345616,0.370977277127896));
#61419=CARTESIAN_POINT('Ctrl Pts',(-22.1540411119085,-1.03801166402214,
-0.92893998115333));
#61420=CARTESIAN_POINT('Ctrl Pts',(-22.0744974846914,0.220250981920178,
-1.37545890821731));
#61421=CARTESIAN_POINT('Ctrl Pts',(-21.9949538574744,1.27617351522542,-0.558371616639268));
#61422=CARTESIAN_POINT('Ctrl Pts',(-21.9154102302573,1.15970130793088,0.771680361039824));
#61423=CARTESIAN_POINT('Ctrl Pts',(-21.8358666030402,-0.0221649839953902,
1.39280523287201));
#61424=CARTESIAN_POINT('Ctrl Pts',(-21.7563229758232,-1.18366875440587,
0.734388169209185));
#61425=CARTESIAN_POINT('Ctrl Pts',(-21.6767793486061,-1.25776003292443,
-0.598696419572632));
#61426=CARTESIAN_POINT('Ctrl Pts',(-21.5972357213891,-0.176372663794721,
-1.38177074317598));
#61427=CARTESIAN_POINT('Ctrl Pts',(-21.517692094172,1.06704469651685,-0.895440293300685));
#61428=CARTESIAN_POINT('Ctrl Pts',(-21.4381484669549,1.33018972296772,0.413513003595081));
#61429=CARTESIAN_POINT('Ctrl Pts',(-21.3586048397379,0.371316413666049,
1.34258028593203));
#61430=CARTESIAN_POINT('Ctrl Pts',(-21.2790612125208,-0.92867775834492,
1.03824627347591));
#61431=CARTESIAN_POINT('Ctrl Pts',(-21.1995175853038,-1.37551449791751,
-0.219903545332743));
#61432=CARTESIAN_POINT('Ctrl Pts',(-21.1199739580867,-0.558693949717291,
-1.27603243445472));
#61433=CARTESIAN_POINT('Ctrl Pts',(-21.0404303308696,0.771387405449101,
-1.15989619102127));
#61434=CARTESIAN_POINT('Ctrl Pts',(-20.9608867036526,1.39281078713163,0.0218131721888098));
#61435=CARTESIAN_POINT('Ctrl Pts',(-20.8813430764355,0.734687130733419,
1.18348321625862));
#61436=CARTESIAN_POINT('Ctrl Pts',(-20.8017994492184,-0.598378700676205,
1.25791121857157));
#61437=CARTESIAN_POINT('Ctrl Pts',(-20.7222558220014,-1.38172614881739,
0.17672168204673));
#61438=CARTESIAN_POINT('Ctrl Pts',(-20.6427121947843,-0.895709791413247,
-1.06681848165356));
#61439=CARTESIAN_POINT('Ctrl Pts',(-20.5631685675673,0.413176995464697,
-1.3302941305027));
#61440=CARTESIAN_POINT('Ctrl Pts',(-20.4836249403502,1.34248645164237,-0.371655526513227));
#61441=CARTESIAN_POINT('Ctrl Pts',(-20.4040813131332,1.03848081668687,0.928415476284475));
#61442=CARTESIAN_POINT('Ctrl Pts',(-20.3245376859161,-0.219556094714919,
1.37556999985631));
#61443=CARTESIAN_POINT('Ctrl Pts',(-20.244994058699,-1.27589127226986,0.559016247149181));
#61444=CARTESIAN_POINT('Ctrl Pts',(-20.165450431482,-1.16009100010727,-0.771094400641886));
#61445=CARTESIAN_POINT('Ctrl Pts',(-20.0859068042649,0.0214613589905084,
-1.39281625252631));
#61446=CARTESIAN_POINT('Ctrl Pts',(-20.0063631770478,1.1832976026021,-0.734986045382691));
#61447=CARTESIAN_POINT('Ctrl Pts',(-19.9268195498308,1.25806232396071,0.598060943601679));
#61448=CARTESIAN_POINT('Ctrl Pts',(-19.8472759226137,0.177070689023417,
1.38168146630109));
#61449=CARTESIAN_POINT('Ctrl Pts',(-19.7677322953967,-1.06659219872449,
0.895979232377189));
#61450=CARTESIAN_POINT('Ctrl Pts',(-19.6881886681796,-1.33039845316146,
-0.412840960972545));
#61451=CARTESIAN_POINT('Ctrl Pts',(-19.6086450409626,-0.371994615647838,
-1.3423925316986));
#61452=CARTESIAN_POINT('Ctrl Pts',(-19.5291014137455,0.928153134988703,
-1.03871529364008));
#61453=CARTESIAN_POINT('Ctrl Pts',(-19.4495577865284,1.37562541403019,0.219208630088832));
#61454=CARTESIAN_POINT('Ctrl Pts',(-19.3700141593114,0.55933850891441,1.27575002867982));
#61455=CARTESIAN_POINT('Ctrl Pts',(-19.2904705320943,-0.77080134663684,
1.16028573517647));
#61456=CARTESIAN_POINT('Ctrl Pts',(-19.2109269048773,-1.39282162905571,
-0.0211095444228931));
#61457=CARTESIAN_POINT('Ctrl Pts',(-19.1313832776602,-0.735284913137964,
-1.18311191344811));
#61458=CARTESIAN_POINT('Ctrl Pts',(-19.0518396504431,0.597743148369296,
-1.25821334908223));
#61459=CARTESIAN_POINT('Ctrl Pts',(-18.9722960232261,1.38163669562993,-0.177419684702549));
#61460=CARTESIAN_POINT('Ctrl Pts',(-18.892752396009,0.896248616175358,1.06636584774406));
#61461=CARTESIAN_POINT('Ctrl Pts',(-18.813208768792,-0.412504900140071,
1.33050269093737));
#61462=CARTESIAN_POINT('Ctrl Pts',(-18.7336651415749,-1.3422985261067,0.372333681048236));
#61463=CARTESIAN_POINT('Ctrl Pts',(-18.6541215143579,-1.03894970432056,
-0.927890734474365));
#61464=CARTESIAN_POINT('Ctrl Pts',(-18.5745778871408,0.21886115147667,-1.37568074043561));
#61465=CARTESIAN_POINT('Ctrl Pts',(-18.4950342599237,1.27560870369364,-0.55966073499237));
#61466=CARTESIAN_POINT('Ctrl Pts',(-18.4154906327066,1.16048039621642,0.770508243452683));
#61467=CARTESIAN_POINT('Ctrl Pts',(-18.3359470054896,-0.0207577285084573,
1.39282691671949));
#61468=CARTESIAN_POINT('Ctrl Pts',(-18.2564033782725,-1.18292614880853,
0.735583733980142));
#61469=CARTESIAN_POINT('Ctrl Pts',(-18.1768597510555,-1.25836429392647,
-0.597425314999374));
#61470=CARTESIAN_POINT('Ctrl Pts',(-18.0973161238384,-0.177768669061831,
-1.38159183680678));
#61471=CARTESIAN_POINT('Ctrl Pts',(-18.0177724966214,1.06613942872675,-0.896517942790525));
#61472=CARTESIAN_POINT('Ctrl Pts',(-17.9382288694043,1.33060684382376,0.412168812988731));
#61473=CARTESIAN_POINT('Ctrl Pts',(-17.8586852421873,0.372672722692757,
1.34220443487269));
#61474=CARTESIAN_POINT('Ctrl Pts',(-17.7791416149702,-0.927628274758204,
1.03918404871335));
#61475=CARTESIAN_POINT('Ctrl Pts',(-17.6995979877531,-1.37573597906903,
-0.218513658900598));
#61476=CARTESIAN_POINT('Ctrl Pts',(-17.6200543605361,-0.559982925362541,
-1.27546729732031));
#61477=CARTESIAN_POINT('Ctrl Pts',(-17.540510733319,0.770215091108087,-1.16067498321473));
#61478=CARTESIAN_POINT('Ctrl Pts',(-17.460967106102,1.39283211551731,0.0204059112696104));
#61479=CARTESIAN_POINT('Ctrl Pts',(-17.3814234788849,0.735882507890194,
1.18274030869519));
#61480=CARTESIAN_POINT('Ctrl Pts',(-17.3018798516679,-0.597107443512156,
1.25851515848381));
#61481=CARTESIAN_POINT('Ctrl Pts',(-17.2223362244507,-1.38154688983449,
0.178117642079035));
#61482=CARTESIAN_POINT('Ctrl Pts',(-17.1427925972337,-0.896787212205539,
-1.06591294168697));
#61483=CARTESIAN_POINT('Ctrl Pts',(-17.0632489700166,0.411832699539931,
-1.33071091181399));
#61484=CARTESIAN_POINT('Ctrl Pts',(-16.9837053427996,1.34211025800256,-0.373011740559811));
#61485=CARTESIAN_POINT('Ctrl Pts',(-16.9041617155825,1.03941832680352,0.927365755856943));
#61486=CARTESIAN_POINT('Ctrl Pts',(-16.8246180883655,-0.218166152382787,
1.37579112992694));
#61487=CARTESIAN_POINT('Ctrl Pts',(-16.7450744611484,-1.27532580956886,
0.56030508000436));
#61488=CARTESIAN_POINT('Ctrl Pts',(-16.6655308339313,-1.16086949615897,
-0.76992188962178));
#61489=CARTESIAN_POINT('Ctrl Pts',(-16.5859872067143,0.0200540927288029,
-1.39283722544883));
#61490=CARTESIAN_POINT('Ctrl Pts',(-16.5064435794972,1.18255439311996,-0.736181234849029));
#61491=CARTESIAN_POINT('Ctrl Pts',(-16.4268999522802,1.25866594274463,0.596789533927942));
#61492=CARTESIAN_POINT('Ctrl Pts',(-16.3473563250631,0.17846660373185,1.38150185471594));
#61493=CARTESIAN_POINT('Ctrl Pts',(-16.267812697846,-1.0656863866392,0.897056424403193));
#61494=CARTESIAN_POINT('Ctrl Pts',(-16.188269070629,-1.33081489490141,-0.411496559815159));
#61495=CARTESIAN_POINT('Ctrl Pts',(-16.1087254434119,-0.373350734627734,
-1.34201599550232));
#61496=CARTESIAN_POINT('Ctrl Pts',(-16.0291818161949,0.927103177787362,
-1.0396525385761));
#61497=CARTESIAN_POINT('Ctrl Pts',(-15.9496381889778,1.37584619300581,0.217818631945427));
#61498=CARTESIAN_POINT('Ctrl Pts',(-15.8700945617608,0.560627198897243,
1.27518424044833));
#61499=CARTESIAN_POINT('Ctrl Pts',(-15.7905509345437,-0.769628639012477,
1.16106393503672));
#61500=CARTESIAN_POINT('Ctrl Pts',(-15.7110073073266,-1.39284224651372,
-0.019702272908519));
#61501=CARTESIAN_POINT('Ctrl Pts',(-15.6314636801096,-0.736479914837584,
-1.1823684020947));
#61502=CARTESIAN_POINT('Ctrl Pts',(-15.5519200528925,0.596471586267007,
-1.2588166466993));
#61503=CARTESIAN_POINT('Ctrl Pts',(-15.4723764256754,1.38145673145398,-0.178815553998048));
#61504=CARTESIAN_POINT('Ctrl Pts',(-15.3928327984584,0.897325579366346,
1.06545976359786));
#61505=CARTESIAN_POINT('Ctrl Pts',(-15.3132891712414,-0.41116039383583,
1.3309187930794));
#61506=CARTESIAN_POINT('Ctrl Pts',(-15.2337455440242,-1.34192164737798,
0.373689704874937));
#61507=CARTESIAN_POINT('Ctrl Pts',(-15.1542019168072,-1.03988668401616,
-0.926840540566187));
#61508=CARTESIAN_POINT('Ctrl Pts',(-15.0746582895901,0.217471097610649,
-1.37590116830213));
#61509=CARTESIAN_POINT('Ctrl Pts',(-14.9951146623731,1.27504258996775,-0.560949282020663));
#61510=CARTESIAN_POINT('Ctrl Pts',(-14.915571035156,1.16125829983559,0.76933533929888));
#61511=CARTESIAN_POINT('Ctrl Pts',(-14.836027407939,-0.0193504518311904,
1.39284717871167));
#61512=CARTESIAN_POINT('Ctrl Pts',(-14.7564837807219,-1.18218233563127,
0.736778547836819));
#61513=CARTESIAN_POINT('Ctrl Pts',(-14.6769401535049,-1.25896727033822,
-0.596153600549652));
#61514=CARTESIAN_POINT('Ctrl Pts',(-14.5973965262878,-0.179164492855332,
-1.38141152005153));
#61515=CARTESIAN_POINT('Ctrl Pts',(-14.5178528990707,1.06523307257745,-0.897594677077771));
#61516=CARTESIAN_POINT('Ctrl Pts',(-14.4383092718537,1.33102260634132,0.410824201623429));
#61517=CARTESIAN_POINT('Ctrl Pts',(-14.3587656446366,0.37402865127972,1.34182721363559));
#61518=CARTESIAN_POINT('Ctrl Pts',(-14.2792220174196,-0.926577844210213,
1.04012076310873));
#61519=CARTESIAN_POINT('Ctrl Pts',(-14.1996783902025,-1.3759560558124,-0.217123549400712));
#61520=CARTESIAN_POINT('Ctrl Pts',(-14.1201347629855,-0.561271329354032,
-1.27490085813617));
#61521=CARTESIAN_POINT('Ctrl Pts',(-14.0405911357683,0.769041990499703,
-1.16145259054315));
#61522=CARTESIAN_POINT('Ctrl Pts',(-13.9610475085513,1.39285202204237,0.0189986295192388));
#61523=CARTESIAN_POINT('Ctrl Pts',(-13.8815038813343,0.737077133827655,
1.18199619374158));
#61524=CARTESIAN_POINT('Ctrl Pts',(-13.8019602541172,-0.595835576796184,
1.25911781365174));
#61525=CARTESIAN_POINT('Ctrl Pts',(-13.7224166269001,-1.38136622051142,
0.179513420281436));
#61526=CARTESIAN_POINT('Ctrl Pts',(-13.6428729996831,-0.897863717520344,
-1.0650063135924));
#61527=CARTESIAN_POINT('Ctrl Pts',(-13.563329372466,0.410487983199367,-1.33112633468056));
#61528=CARTESIAN_POINT('Ctrl Pts',(-13.483785745249,1.34173269428113,-0.374367573820533));
#61529=CARTESIAN_POINT('Ctrl Pts',(-13.4042421180319,1.04035477583892,0.92631508873616));
#61530=CARTESIAN_POINT('Ctrl Pts',(-13.3246984908148,-0.216775987337669,
1.37601085553309));
#61531=CARTESIAN_POINT('Ctrl Pts',(-13.2451548635978,-1.27475904496258,
0.561593340876897));
#61532=CARTESIAN_POINT('Ctrl Pts',(-13.1656112363807,-1.16164680714707,
-0.768748592633631));
#61533=CARTESIAN_POINT('Ctrl Pts',(-13.0860676091637,0.0186468059951288,
-1.39285677650551));
#61534=CARTESIAN_POINT('Ctrl Pts',(-13.0065239819466,1.18180997643742,-0.737375672791089));
#61535=CARTESIAN_POINT('Ctrl Pts',(-12.9269803547296,1.25926827663031,0.595517515026806));
#61536=CARTESIAN_POINT('Ctrl Pts',(-12.8474367275125,0.179862336254169,
1.38132083283659));
#61537=CARTESIAN_POINT('Ctrl Pts',(-12.7678931002954,-1.0647794866572,0.898132700676888));
#61538=CARTESIAN_POINT('Ctrl Pts',(-12.6883494730784,-1.33122997809048,
-0.410151738585083));
#61539=CARTESIAN_POINT('Ctrl Pts',(-12.6088058458613,-0.374706472475756,
-1.34163808932065));
#61540=CARTESIAN_POINT('Ctrl Pts',(-12.5292622186442,0.926052274160795,
-1.04058872219181));
#61541=CARTESIAN_POINT('Ctrl Pts',(-12.4497185914272,1.37606556746074,0.216428411443782));
#61542=CARTESIAN_POINT('Ctrl Pts',(-12.3701749642101,0.561915316568623,
1.27461715045607));
#61543=CARTESIAN_POINT('Ctrl Pts',(-12.2906313369931,-0.768455145719422,
1.1618409496349));
#61544=CARTESIAN_POINT('Ctrl Pts',(-12.211087709776,-1.39286144210078,-0.0182949812813028));
#61545=CARTESIAN_POINT('Ctrl Pts',(-12.1315440825589,-0.737674164708033,
-1.18162368373076));
#61546=CARTESIAN_POINT('Ctrl Pts',(-12.0520004553419,0.595199415261899,
-1.25941865926429));
#61547=CARTESIAN_POINT('Ctrl Pts',(-11.9724568281248,1.3812753570299,-0.180211240751194));
#61548=CARTESIAN_POINT('Ctrl Pts',(-11.8929132009078,0.898401626530242,
1.06455259178631));
#61549=CARTESIAN_POINT('Ctrl Pts',(-11.8133695736907,-0.409815467802085,
1.33133353656448));
#61550=CARTESIAN_POINT('Ctrl Pts',(-11.7338259464736,-1.34154339876018,
0.375045347223708));
#61551=CARTESIAN_POINT('Ctrl Pts',(-11.6542823192566,-1.04082260215243,
-0.925789400500909));
#61552=CARTESIAN_POINT('Ctrl Pts',(-11.5747386920395,0.216080821741205,
-1.37612019159185));
#61553=CARTESIAN_POINT('Ctrl Pts',(-11.4951950648225,1.27447517462567,-0.562237256408714));
#61554=CARTESIAN_POINT('Ctrl Pts',(-11.4156514376054,1.16203501799428,0.768161649775757));
#61555=CARTESIAN_POINT('Ctrl Pts',(-11.3361078103884,-0.0179431554001853,
1.39286601882789));
#61556=CARTESIAN_POINT('Ctrl Pts',(-11.2565641831713,-1.18143731563344,
0.737972609559454));
#61557=CARTESIAN_POINT('Ctrl Pts',(-11.1770205559542,-1.2595689615441,-0.5948812775217));
#61558=CARTESIAN_POINT('Ctrl Pts',(-11.0974769287372,-0.18056013375031,
-1.38122979309427));
#61559=CARTESIAN_POINT('Ctrl Pts',(-11.0179333015201,1.06432562899421,-0.898670495063273));
#61560=CARTESIAN_POINT('Ctrl Pts',(-10.938389674303,1.33143701009596,0.409479170871799));
#61561=CARTESIAN_POINT('Ctrl Pts',(-10.858846047086,0.375384198042811,1.34144862260576));
#61562=CARTESIAN_POINT('Ctrl Pts',(-10.7793024198689,-0.925526467773234,
1.04105641570588));
#61563=CARTESIAN_POINT('Ctrl Pts',(-10.6997587926519,-1.37617472792294,
-0.215733218252087));
#61564=CARTESIAN_POINT('Ctrl Pts',(-10.6202151654348,-0.562559160376593,
-1.27433311748048));
#61565=CARTESIAN_POINT('Ctrl Pts',(-10.5406715382178,0.767868104821389,
-1.1622290122128));
#61566=CARTESIAN_POINT('Ctrl Pts',(-10.4611279110007,1.39287050668653,0.0175913283742381));
#61567=CARTESIAN_POINT('Ctrl Pts',(-10.3815842837836,0.73827100732634,1.18125087215736));
#61568=CARTESIAN_POINT('Ctrl Pts',(-10.3020406565666,-0.594563101826563,
1.25971918346015));
#61569=CARTESIAN_POINT('Ctrl Pts',(-10.2224970293495,-1.38118414103261,
0.180909015229188));
#61570=CARTESIAN_POINT('Ctrl Pts',(-10.1429534021325,-0.898939306258771,
-1.06409859829537));
#61571=CARTESIAN_POINT('Ctrl Pts',(-10.0634097749154,0.40914284781568,-1.33154039867832));
#61572=CARTESIAN_POINT('Ctrl Pts',(-9.98386614769835,1.34135376086346,-0.375723024911412));
#61573=CARTESIAN_POINT('Ctrl Pts',(-9.90432252048127,1.04129016283722,0.9252634759946));
#61574=CARTESIAN_POINT('Ctrl Pts',(-9.82477889326422,-0.215385600998657,
1.3762291764505));
#61575=CARTESIAN_POINT('Ctrl Pts',(-9.74523526604716,-1.27419097902953,
0.562881028451743));
#61576=CARTESIAN_POINT('Ctrl Pts',(-9.6656916388301,-1.16242293227811,-0.767574510875076));
#61577=CARTESIAN_POINT('Ctrl Pts',(-9.58614801161304,0.0172395002259546,
-1.39287490567643));
#61578=CARTESIAN_POINT('Ctrl Pts',(-9.50660438439598,1.18106435331442,-0.738569357989597));
#61579=CARTESIAN_POINT('Ctrl Pts',(-9.42706075717891,1.25986932500286,0.59424488819676));
#61580=CARTESIAN_POINT('Ctrl Pts',(-9.34751712996187,0.181257885165623,
1.3811384008478));
#61581=CARTESIAN_POINT('Ctrl Pts',(-9.26797350274479,-1.06387149970427,
0.89920806009964));
#61582=CARTESIAN_POINT('Ctrl Pts',(-9.18842987552775,-1.33164370230497,
-0.408806498655169));
#61583=CARTESIAN_POINT('Ctrl Pts',(-9.10888624831068,-0.37606182780791,
-1.34125881353932));
#61584=CARTESIAN_POINT('Ctrl Pts',(-9.02934262109362,0.925000425181733,
-1.04152384353156));
#61585=CARTESIAN_POINT('Ctrl Pts',(-8.94979899387657,1.37628353717109,0.215037970003031));
#61586=CARTESIAN_POINT('Ctrl Pts',(-8.87025536665949,0.563202860613652,
1.27404875928191));
#61587=CARTESIAN_POINT('Ctrl Pts',(-8.79071173944245,-0.767280867955522,
1.16261677817781));
#61588=CARTESIAN_POINT('Ctrl Pts',(-8.71116811222538,-1.39287921579729,
-0.0168876709777203));
#61589=CARTESIAN_POINT('Ctrl Pts',(-8.63162448500833,-0.738867661530245,
-1.1808777591165));
#61590=CARTESIAN_POINT('Ctrl Pts',(-8.55208085779126,0.59392663665258,-1.26001938616266));
#61591=CARTESIAN_POINT('Ctrl Pts',(-8.47253723057421,1.38109257254281,-0.181606743537313));
#61592=CARTESIAN_POINT('Ctrl Pts',(-8.39299360335714,0.899476756568682,
1.06364433323544));
#61593=CARTESIAN_POINT('Ctrl Pts',(-8.3134499761401,-0.408470123411764,
1.33174692096928));
#61594=CARTESIAN_POINT('Ctrl Pts',(-8.23390634892301,-1.3411637806394,0.376400606710692));
#61595=CARTESIAN_POINT('Ctrl Pts',(-8.15436272170597,-1.04175745777397,
-0.924737315351474));
#61596=CARTESIAN_POINT('Ctrl Pts',(-8.0748190944889,0.214690325287459,-1.37633781008121));
#61597=CARTESIAN_POINT('Ctrl Pts',(-7.99527546727185,1.27390645824667,-0.563524656841738));
#61598=CARTESIAN_POINT('Ctrl Pts',(-7.91573184005478,1.16281054989956,0.766987176081464));
#61599=CARTESIAN_POINT('Ctrl Pts',(-7.83618821283773,-0.016535840652032,
1.39288343704887));
#61600=CARTESIAN_POINT('Ctrl Pts',(-7.75664458562066,-1.18069108957553,
0.739165917929196));
#61601=CARTESIAN_POINT('Ctrl Pts',(-7.67710095840361,-1.26016936692994,
-0.593608347214357));
#61602=CARTESIAN_POINT('Ctrl Pts',(-7.59755733118654,-0.181955590322025,
-1.38104665612053));
#61603=CARTESIAN_POINT('Ctrl Pts',(-7.51801370396949,1.06341709890332,-0.899745395648787));
#61604=CARTESIAN_POINT('Ctrl Pts',(-7.43847007675242,1.3318500546647,0.408133722106875));
#61605=CARTESIAN_POINT('Ctrl Pts',(-7.35892644953538,0.376739361598168,
1.34106866216976));
#61606=CARTESIAN_POINT('Ctrl Pts',(-7.2793828223183,-0.92447414652058,1.04199100554956));
#61607=CARTESIAN_POINT('Ctrl Pts',(-7.19983919510125,-1.37639199517741,
-0.214342666874064));
#61608=CARTESIAN_POINT('Ctrl Pts',(-7.12029556788419,-0.563846417115518,
-1.27376407593289));
#61609=CARTESIAN_POINT('Ctrl Pts',(-7.04075194066713,0.766693435271625,
-1.16300424743101));
#61610=CARTESIAN_POINT('Ctrl Pts',(-6.96120831345008,1.39288756943087,0.0161840092713161));
#61611=CARTESIAN_POINT('Ctrl Pts',(-6.88166468623301,0.73946412716746,1.1805043447034));
#61612=CARTESIAN_POINT('Ctrl Pts',(-6.80212105901595,-0.593290019902356,
1.26031926729517));
#61613=CARTESIAN_POINT('Ctrl Pts',(-6.7225774317989,-1.38100065158391,0.182304425497526));
#61614=CARTESIAN_POINT('Ctrl Pts',(-6.64303380458182,-0.900013977322796,
-1.06318979672246));
#61615=CARTESIAN_POINT('Ctrl Pts',(-6.56349017736478,0.407797294762003,
-1.33195310338462));
#61616=CARTESIAN_POINT('Ctrl Pts',(-6.4839465501477,1.34097345813645,-0.377078092448702));
#61617=CARTESIAN_POINT('Ctrl Pts',(-6.40440292293066,1.04222448684345,0.924210918705832));
#61618=CARTESIAN_POINT('Ctrl Pts',(-6.32485929571359,-0.213994994785076,
1.37644609245625));
#61619=CARTESIAN_POINT('Ctrl Pts',(-6.24531566849654,-1.27362161234968,
0.564168141414408));
#61620=CARTESIAN_POINT('Ctrl Pts',(-6.16577204127946,-1.16319787075975,
-0.766399645544771));
#61621=CARTESIAN_POINT('Ctrl Pts',(-6.08622841406241,0.0158321768580185,
-1.39289161294304));
#61622=CARTESIAN_POINT('Ctrl Pts',(-6.00668478684535,1.18031752451205,-0.739762289225985));
#61623=CARTESIAN_POINT('Ctrl Pts',(-5.92714115962829,1.26046908724875,0.592971654736946));
#61624=CARTESIAN_POINT('Ctrl Pts',(-5.84759753241124,0.182653249041503,
1.38095455893587));
#61625=CARTESIAN_POINT('Ctrl Pts',(-5.76805390519417,-1.06296242670733,
0.900282501573585));
#61626=CARTESIAN_POINT('Ctrl Pts',(-5.68851027797711,-1.3320560671225,-0.407460841398637));
#61627=CARTESIAN_POINT('Ctrl Pts',(-5.60896665076006,-0.377416799240644,
-1.34087816854557));
#61628=CARTESIAN_POINT('Ctrl Pts',(-5.52942302354299,0.923947631924043,
-1.0424579016407));
#61629=CARTESIAN_POINT('Ctrl Pts',(-5.44987939632593,1.37650010191426,0.213647309042655));
#61630=CARTESIAN_POINT('Ctrl Pts',(-5.37033576910888,0.564489829717927,
1.27347906750608));
#61631=CARTESIAN_POINT('Ctrl Pts',(-5.29079214189181,-0.76610580691961,
1.16339141987348));
#61632=CARTESIAN_POINT('Ctrl Pts',(-5.21124851467476,-1.39289556758514,
-0.0154803434345617));
#61633=CARTESIAN_POINT('Ctrl Pts',(-5.13170488745769,-0.740060404085762,
-1.1801306290134));
#61634=CARTESIAN_POINT('Ctrl Pts',(-5.05216126024064,0.592653251738383,
-1.26061882678114));
#61635=CARTESIAN_POINT('Ctrl Pts',(-4.97261763302358,1.38090837817934,-0.183002060931766));
#61636=CARTESIAN_POINT('Ctrl Pts',(-4.89307400580652,0.900550968384048,
1.06273498887245));
#61637=CARTESIAN_POINT('Ctrl Pts',(-4.81353037858945,-0.407124362038215,
1.33215894587174));
#61638=CARTESIAN_POINT('Ctrl Pts',(-4.7339867513724,-1.34078279340317,0.377755481952438));
#61639=CARTESIAN_POINT('Ctrl Pts',(-4.65444312415534,-1.04269124992645,
-0.923684286191978));
#61640=CARTESIAN_POINT('Ctrl Pts',(-4.57489949693828,0.213299609668962,
-1.37655402354802));
#61641=CARTESIAN_POINT('Ctrl Pts',(-4.49535586972123,1.27333644141125,-0.564811482005513));
#61642=CARTESIAN_POINT('Ctrl Pts',(-4.41581224250416,1.1635848947598,0.765811919414912));
#61643=CARTESIAN_POINT('Ctrl Pts',(-4.33626861528711,-0.0151285090234098,
1.39289943335687));
#61644=CARTESIAN_POINT('Ctrl Pts',(-4.25672498807004,-1.17994365821935,
0.740358471727794));
#61645=CARTESIAN_POINT('Ctrl Pts',(-4.17718136085298,-1.26076848588279,
-0.592334810927032));
#61646=CARTESIAN_POINT('Ctrl Pts',(-4.09763773363592,-0.183350861145989,
-1.38086210931729));
#61647=CARTESIAN_POINT('Ctrl Pts',(-4.01809410641886,1.06250748323233,-0.900819377736997));
#61648=CARTESIAN_POINT('Ctrl Pts',(-3.9385504792018,1.3322617396258,0.406787856702201));
#61649=CARTESIAN_POINT('Ctrl Pts',(-3.85900685198474,0.378094140562434,
1.34068733271538));
#61650=CARTESIAN_POINT('Ctrl Pts',(-3.77946322476769,-0.923420881526489,
1.04292453168578));
#61651=CARTESIAN_POINT('Ctrl Pts',(-3.69991959755062,-1.37660785735405,
-0.21295189668622));
#61652=CARTESIAN_POINT('Ctrl Pts',(-3.62037597033357,-0.565133098256669,
-1.27319373407426));
#61653=CARTESIAN_POINT('Ctrl Pts',(-3.5408323431165,0.765517983049464,-1.16377829540639));
#61654=CARTESIAN_POINT('Ctrl Pts',(-3.46128871589945,1.39290321025801,0.0147766736470439));
#61655=CARTESIAN_POINT('Ctrl Pts',(-3.38174508868238,0.740656492133029,
1.17975661214186));
#61656=CARTESIAN_POINT('Ctrl Pts',(-3.30220146146532,-0.592016332323219,
1.2609180645441));
#61657=CARTESIAN_POINT('Ctrl Pts',(-3.22265783424827,-1.38081575235259,
0.183699649662051));
#61658=CARTESIAN_POINT('Ctrl Pts',(-3.1431142070312,-0.901087729615471,
-1.06227990980161));
#61659=CARTESIAN_POINT('Ctrl Pts',(-3.06357057981415,0.406451325412254,
-1.33236444837786));
#61660=CARTESIAN_POINT('Ctrl Pts',(-2.98402695259708,1.34059178648789,-0.378432775049564));
#61661=CARTESIAN_POINT('Ctrl Pts',(-2.90448332538003,1.04315774690456,0.923157417945318));
#61662=CARTESIAN_POINT('Ctrl Pts',(-2.82493969816297,-0.212604170117943,
1.37666160332707));
#61663=CARTESIAN_POINT('Ctrl Pts',(-2.74539607094591,-1.2730509455016,0.565454678454453));
#61664=CARTESIAN_POINT('Ctrl Pts',(-2.66585244372885,-1.16397162180588,
-0.765223997848736));
#61665=CARTESIAN_POINT('Ctrl Pts',(-2.58630881651179,0.0144248373372911,
-1.3929068982755));
#61666=CARTESIAN_POINT('Ctrl Pts',(-2.50676518929473,1.17956949077493,-0.740954465306795));
#61667=CARTESIAN_POINT('Ctrl Pts',(-2.42722156207767,1.26106756278956,0.591697815993344));
#61668=CARTESIAN_POINT('Ctrl Pts',(-2.34767793486061,0.184048426393107,
1.38076930720073));
#61669=CARTESIAN_POINT('Ctrl Pts',(-2.26813430764355,-1.06205226847233,
0.901356024168364));
#61670=CARTESIAN_POINT('Ctrl Pts',(-2.18859068042649,-1.33246707235384,
-0.406114768505075));
#61671=CARTESIAN_POINT('Ctrl Pts',(-2.10904705320943,-0.378771384950898,
-1.34049615412855));
#61672=CARTESIAN_POINT('Ctrl Pts',(-2.02950342599237,0.922893894627693,
-1.04339089670334));
#61673=CARTESIAN_POINT('Ctrl Pts',(-1.94995979877531,1.37671526305346,0.21225643214144));
#61674=CARTESIAN_POINT('Ctrl Pts',(-1.87041617155825,0.56577621956083,1.2729080716121));
#61675=CARTESIAN_POINT('Ctrl Pts',(-1.79087254434119,-0.764929958104375,
1.16416488170923));
#61676=CARTESIAN_POINT('Ctrl Pts',(-1.71132891712414,-1.39291050827911,
-0.0140730148512983));
#61677=CARTESIAN_POINT('Ctrl Pts',(-1.63178528990707,-0.74125237059894,
-1.17938226616436));
#61678=CARTESIAN_POINT('Ctrl Pts',(-1.55224166269001,0.591379222800219,
-1.26121703368907));
#61679=CARTESIAN_POINT('Ctrl Pts',(-1.47269803547295,1.3807228481852,-0.18439709057274));
#61680=CARTESIAN_POINT('Ctrl Pts',(-1.3931544082559,0.901624120319131,1.06182436804775));
#61681=CARTESIAN_POINT('Ctrl Pts',(-1.31361078103883,-0.405777918272958,
1.33256997446379));
#61682=CARTESIAN_POINT('Ctrl Pts',(-1.23406715382177,-1.34040094379007,
0.379109281433699));
#61683=CARTESIAN_POINT('Ctrl Pts',(-1.15452352660471,-1.04362301661124,
-0.922629004235279));
#61684=CARTESIAN_POINT('Ctrl Pts',(-1.07497989938766,0.211906852253127,
-1.3767713178738));
#61685=CARTESIAN_POINT('Ctrl Pts',(-0.995436272170595,1.27276858673064,
-0.566093011994411));
#61686=CARTESIAN_POINT('Ctrl Pts',(-0.915892644953538,1.16435148089155,
0.76462692514249));
#61687=CARTESIAN_POINT('Ctrl Pts',(-0.836349017736476,-0.0137086904440423,
1.39293100582981));
#61688=CARTESIAN_POINT('Ctrl Pts',(-0.75680539051942,-1.17921869337341,
0.741518007289884));
#61689=CARTESIAN_POINT('Ctrl Pts',(-0.67726176330236,-1.26132138808091,
-0.590999433913082));
#61690=CARTESIAN_POINT('Ctrl Pts',(-0.597718136085294,-0.184831240778329,
-1.38079239774389));
#61691=CARTESIAN_POINT('Ctrl Pts',(-0.518174508868238,1.06175884240671,
-0.901671642965467));
#61692=CARTESIAN_POINT('Ctrl Pts',(-0.438630881651178,1.33236304935347,
0.405021101276792));
#61693=CARTESIAN_POINT('Ctrl Pts',(-0.35908725443412,0.380047119706207,
1.34111457344272));
#61694=CARTESIAN_POINT('Ctrl Pts',(-0.279543627217059,-0.923604039966345,
1.04221933963793));
#61695=CARTESIAN_POINT('Ctrl Pts',(-0.226514542405686,-1.22368627072144,
0.208991815207804));
#61696=CARTESIAN_POINT('Ctrl Pts',(-0.2,-1.1640875192389,-0.178872328917063));
#61697=CARTESIAN_POINT('Ctrl Pts',(-34.7464852262806,-0.551480035116971,
1.14734422509872));
#61698=CARTESIAN_POINT('Ctrl Pts',(-34.719970683875,-0.933765454838236,
0.963595728282564));
#61699=CARTESIAN_POINT('Ctrl Pts',(-34.6669415990636,-1.49352775050342,
0.187080277793629));
#61700=CARTESIAN_POINT('Ctrl Pts',(-34.5873979718465,-0.963838494838092,
-1.1580287513703));
#61701=CARTESIAN_POINT('Ctrl Pts',(-34.5078543446294,0.452586213068269,
-1.43553205749614));
#61702=CARTESIAN_POINT('Ctrl Pts',(-34.4283107174124,1.45257317513127,-0.396124700743783));
#61703=CARTESIAN_POINT('Ctrl Pts',(-34.3487670901953,1.11845427959544,1.00817593102252));
#61704=CARTESIAN_POINT('Ctrl Pts',(-34.2692234629783,-0.243346736507173,
1.48576990397941));
#61705=CARTESIAN_POINT('Ctrl Pts',(-34.1896798357612,-1.38149478299821,
0.598688827541391));
#61706=CARTESIAN_POINT('Ctrl Pts',(-34.1101362085442,-1.25054175940707,
-0.83853864419688));
#61707=CARTESIAN_POINT('Ctrl Pts',(-34.0305925813271,0.0292850707204112,
-1.50534226452188));
#61708=CARTESIAN_POINT('Ctrl Pts',(-33.95104895411,1.28219436924234,-0.789258183429619));
#61709=CARTESIAN_POINT('Ctrl Pts',(-33.871505326893,1.35718503035677,0.651922322116352));
#61710=CARTESIAN_POINT('Ctrl Pts',(-33.7919616996759,0.185353446897111,
1.49418397750811));
#61711=CARTESIAN_POINT('Ctrl Pts',(-33.7124180724589,-1.1567565536606,0.963774909575826));
#61712=CARTESIAN_POINT('Ctrl Pts',(-33.6328744452418,-1.43617882914026,
-0.452037693320334));
#61713=CARTESIAN_POINT('Ctrl Pts',(-33.5533308180247,-0.396212159812758,
-1.45257081728134));
#61714=CARTESIAN_POINT('Ctrl Pts',(-33.4737871908077,1.00774629157814,-1.11865742453962));
#61715=CARTESIAN_POINT('Ctrl Pts',(-33.3942435635906,1.48590880876346,0.242944316826441));
#61716=CARTESIAN_POINT('Ctrl Pts',(-33.3146999363735,0.598996939754183,
1.38135780288018));
#61717=CARTESIAN_POINT('Ctrl Pts',(-33.2351563091566,-0.838201232648247,
1.25074599961759));
#61718=CARTESIAN_POINT('Ctrl Pts',(-33.1556126819394,-1.50536094578838,
-0.0289008665489891));
#61719=CARTESIAN_POINT('Ctrl Pts',(-33.0760690547224,-0.789576059365041,
-1.28199705793266));
#61720=CARTESIAN_POINT('Ctrl Pts',(-32.9965254275053,0.651576341838971,
-1.35734855625107));
#61721=CARTESIAN_POINT('Ctrl Pts',(-32.9169818002883,1.4941387685048,-0.185731439607652));
#61722=CARTESIAN_POINT('Ctrl Pts',(-32.8374381730712,0.964066192735147,
1.15651338081008));
#61723=CARTESIAN_POINT('Ctrl Pts',(-32.7578945458541,-0.45167445189681,
1.43629280328175));
#61724=CARTESIAN_POINT('Ctrl Pts',(-32.6783509186371,-1.45247093343298,
0.396579139408509));
#61725=CARTESIAN_POINT('Ctrl Pts',(-32.59880729142,-1.1189118095244,-1.00746374050411));
#61726=CARTESIAN_POINT('Ctrl Pts',(-32.519263664203,0.242568913490285,-1.48597010353709));
#61727=CARTESIAN_POINT('Ctrl Pts',(-32.4397200369859,1.38120649258727,-0.599345852627567));
#61728=CARTESIAN_POINT('Ctrl Pts',(-32.3601764097689,1.25095766374634,0.837885284336153));
#61729=CARTESIAN_POINT('Ctrl Pts',(-32.2806327825517,-0.0285206140419742,
1.50536819444095));
#61730=CARTESIAN_POINT('Ctrl Pts',(-32.2010891553348,-1.28179758182883,
0.789899857861043));
#61731=CARTESIAN_POINT('Ctrl Pts',(-32.1215455281176,-1.35751309302076,
-0.651233466973292));
#61732=CARTESIAN_POINT('Ctrl Pts',(-32.0420019009006,-0.18610884223578,
-1.49409180610823));
#61733=CARTESIAN_POINT('Ctrl Pts',(-31.9624582736835,1.15626982951559,-0.964358287974677));
#61734=CARTESIAN_POINT('Ctrl Pts',(-31.8829146464665,1.436406846299,0.451311641927037));
#61735=CARTESIAN_POINT('Ctrl Pts',(-31.8033710192494,0.396946009130357,
1.45237071440808));
#61736=CARTESIAN_POINT('Ctrl Pts',(-31.7238273920324,-1.00718108059297,
1.1191662508893));
#61737=CARTESIAN_POINT('Ctrl Pts',(-31.6442837648153,-1.4860313269786,-0.242193561996057));
#61738=CARTESIAN_POINT('Ctrl Pts',(-31.5647401375982,-0.599694714891924,
-1.38105505870149));
#61739=CARTESIAN_POINT('Ctrl Pts',(-31.4851965103812,0.837569276047795,
-1.25116926674808));
#61740=CARTESIAN_POINT('Ctrl Pts',(-31.4056528831641,1.50537535048078,0.0281403695611341));
#61741=CARTESIAN_POINT('Ctrl Pts',(-31.3261092559471,0.790223604150294,
1.28159801875546));
#61742=CARTESIAN_POINT('Ctrl Pts',(-31.24656562873,-0.650890549604056,1.35767754591078));
#61743=CARTESIAN_POINT('Ctrl Pts',(-31.1670220015129,-1.49404474888693,
0.18648623154965));
#61744=CARTESIAN_POINT('Ctrl Pts',(-31.0874783742959,-0.964650321421056,
-1.15602620368936));
#61745=CARTESIAN_POINT('Ctrl Pts',(-31.0079347470788,0.450948803023003,
-1.43652079806952));
#61746=CARTESIAN_POINT('Ctrl Pts',(-30.9283911198618,1.45227040279163,-0.397312853315405));
#61747=CARTESIAN_POINT('Ctrl Pts',(-30.8488474926447,1.1194206208098,1.0068983563101));
#61748=CARTESIAN_POINT('Ctrl Pts',(-30.7693038654276,-0.241818195028865,
1.48609245566592));
#61749=CARTESIAN_POINT('Ctrl Pts',(-30.6897602382106,-1.38090353671155,
0.600043538863403));
#61750=CARTESIAN_POINT('Ctrl Pts',(-30.6102166109935,-1.25138078991632,
-0.837253214304121));
#61751=CARTESIAN_POINT('Ctrl Pts',(-30.5306729837765,0.0277601232818883,
-1.50538241048232));
#61752=CARTESIAN_POINT('Ctrl Pts',(-30.4511293565594,1.28139837391439,-0.790547300016728));
#61753=CARTESIAN_POINT('Ctrl Pts',(-30.3715857293424,1.35784191217663,0.650547590703944));
#61754=CARTESIAN_POINT('Ctrl Pts',(-30.2920421021253,0.186863608965661,
1.49399759634295));
#61755=CARTESIAN_POINT('Ctrl Pts',(-30.2124984749082,-1.1557825041059,0.964942293319604));
#61756=CARTESIAN_POINT('Ctrl Pts',(-30.1329548476912,-1.43663465818619,
-0.450585935346916));
#61757=CARTESIAN_POINT('Ctrl Pts',(-30.0534112204741,-0.397679672150927,
-1.45216999851674));
#61758=CARTESIAN_POINT('Ctrl Pts',(-29.973867593257,1.00661556778455,-1.11967491930827));
#61759=CARTESIAN_POINT('Ctrl Pts',(-29.89432396604,1.48615348953668,0.241442812632994));
#61760=CARTESIAN_POINT('Ctrl Pts',(-29.8147803388229,0.600392324550558,
1.38075192661642));
#61761=CARTESIAN_POINT('Ctrl Pts',(-29.7352367116059,-0.836937099141528,
1.25159223324322));
#61762=CARTESIAN_POINT('Ctrl Pts',(-29.6556930843888,-1.50538937443656,
-0.0273798752314642));
#61763=CARTESIAN_POINT('Ctrl Pts',(-29.5761494571718,-0.790870945444198,
-1.28119864731679));
#61764=CARTESIAN_POINT('Ctrl Pts',(-29.4966058299547,0.65020459029722,-1.35800619180864));
#61765=CARTESIAN_POINT('Ctrl Pts',(-29.4170622027377,1.49395034847806,-0.187240974459272));
#61766=CARTESIAN_POINT('Ctrl Pts',(-29.3375185755206,0.965234203652314,
1.15553873078052));
#61767=CARTESIAN_POINT('Ctrl Pts',(-29.2579749483035,-0.45022303892228,
1.43674842664183));
#61768=CARTESIAN_POINT('Ctrl Pts',(-29.1784313210864,-1.45206950158965,
0.398046465613467));
#61769=CARTESIAN_POINT('Ctrl Pts',(-29.0988876938694,-1.11992914636859,
-1.0063327150343));
#61770=CARTESIAN_POINT('Ctrl Pts',(-29.0193440666523,0.241067414832435,
-1.486214428587));
#61771=CARTESIAN_POINT('Ctrl Pts',(-28.9398004394353,1.38060022842574,-0.600741071931139));
#61772=CARTESIAN_POINT('Ctrl Pts',(-28.8602568122182,1.2518035967153,0.836620930580172));
#61773=CARTESIAN_POINT('Ctrl Pts',(-28.7807131850012,-0.0269996254341221,
1.50539624234306));
#61774=CARTESIAN_POINT('Ctrl Pts',(-28.7011695577841,-1.2809988389754,0.791194540412063));
#61775=CARTESIAN_POINT('Ctrl Pts',(-28.621625930567,-1.35817038479635,-0.649861548405748));
#61776=CARTESIAN_POINT('Ctrl Pts',(-28.54208230335,-0.187618328006441,-1.49390300529527));
#61777=CARTESIAN_POINT('Ctrl Pts',(-28.4625386761329,1.15529488372878,-0.965526052400598));
#61778=CARTESIAN_POINT('Ctrl Pts',(-28.3829950489158,1.43686210342921,0.449860113772244));
#61779=CARTESIAN_POINT('Ctrl Pts',(-28.3034514216988,0.398413233679613,
1.45196891201676));
#61780=CARTESIAN_POINT('Ctrl Pts',(-28.2239077944817,-1.00604979807743,
1.12018330197452));
#61781=CARTESIAN_POINT('Ctrl Pts',(-28.1443641672647,-1.486275272813,-0.240692001651152));
#61782=CARTESIAN_POINT('Ctrl Pts',(-28.0648205400476,-0.601089780982883,
-1.38044844214919));
#61783=CARTESIAN_POINT('Ctrl Pts',(-27.9852769128306,0.836304708640234,
-1.25201488031906));
#61784=CARTESIAN_POINT('Ctrl Pts',(-27.9057332856135,1.50540301420138,0.0266193739141349));
#61785=CARTESIAN_POINT('Ctrl Pts',(-27.8261896583965,0.791518084899668,
1.28079894890297));
#61786=CARTESIAN_POINT('Ctrl Pts',(-27.7466460311794,-0.649518465051427,
1.35833449112927));
#61787=CARTESIAN_POINT('Ctrl Pts',(-27.6671024039623,-1.49385556679761,
0.18799566958307));
#61788=CARTESIAN_POINT('Ctrl Pts',(-27.5875587767453,-0.96581783954581,
-1.15505096296625));
#61789=CARTESIAN_POINT('Ctrl Pts',(-27.5080151495282,0.449497159919988,
-1.43697568854106));
#61790=CARTESIAN_POINT('Ctrl Pts',(-27.4284715223111,1.4518682298045,-0.398779976325944));
#61791=CARTESIAN_POINT('Ctrl Pts',(-27.3489278950941,1.12043738610985,1.00576681693199));
#61792=CARTESIAN_POINT('Ctrl Pts',(-27.269384267877,-0.240316573113117,
1.48633602221078));
#61793=CARTESIAN_POINT('Ctrl Pts',(-27.18984064066,-1.38029656779647,0.601438451683525));
#61794=CARTESIAN_POINT('Ctrl Pts',(-27.1102970134429,-1.25222608404103,
-0.835988433341909));
#61795=CARTESIAN_POINT('Ctrl Pts',(-27.0307533862258,0.0262391206957839,
-1.50540969001109));
#61796=CARTESIAN_POINT('Ctrl Pts',(-26.9512097590088,1.28059897711225,-0.791841578886351));
#61797=CARTESIAN_POINT('Ctrl Pts',(-26.8716661317917,1.35849851079693,0.649175340256163));
#61798=CARTESIAN_POINT('Ctrl Pts',(-26.7921225045747,0.188372999165078,
1.49380803298809));
#61799=CARTESIAN_POINT('Ctrl Pts',(-26.7125788773576,-1.15480696850846,
0.966109565069344));
#61800=CARTESIAN_POINT('Ctrl Pts',(-26.6330352501406,-1.43708918197015,
-0.449134177388628));
#61801=CARTESIAN_POINT('Ctrl Pts',(-26.5534916229235,-0.399146693529099,
-1.45176745495929));
#61802=CARTESIAN_POINT('Ctrl Pts',(-26.4739479957064,1.005483771616,-1.12069139875839));
#61803=CARTESIAN_POINT('Ctrl Pts',(-26.3944043684894,1.48639667677647,0.239941129242241));
#61804=CARTESIAN_POINT('Ctrl Pts',(-26.3148607412723,0.601787084010857,
1.38014460537724));
#61805=CARTESIAN_POINT('Ctrl Pts',(-26.2353171140552,-0.835672104705342,
1.25243720786774));
#61806=CARTESIAN_POINT('Ctrl Pts',(-26.1557734868382,-1.50541626977177,
-0.0258588658032874));
#61807=CARTESIAN_POINT('Ctrl Pts',(-26.0762298596211,-0.792165022351513,
-1.280398923616));
#61808=CARTESIAN_POINT('Ctrl Pts',(-25.9966862324041,0.648832174041817,
-1.35866244378887));
#61809=CARTESIAN_POINT('Ctrl Pts',(-25.917142605187,1.49376040386974,-0.188750316728418));
#61810=CARTESIAN_POINT('Ctrl Pts',(-25.83759897797,0.966401228952598,1.154562900371));
#61811=CARTESIAN_POINT('Ctrl Pts',(-25.7580553507529,-0.448771166201346,
1.43720258370922));
#61812=CARTESIAN_POINT('Ctrl Pts',(-25.6785117235359,-1.45166658748755,
0.399513385265661));
#61813=CARTESIAN_POINT('Ctrl Pts',(-25.5989680963187,-1.12094533990392,
-1.00520066214756));
#61814=CARTESIAN_POINT('Ctrl Pts',(-25.5194244691017,0.239565670062516,
-1.48645723650622));
#61815=CARTESIAN_POINT('Ctrl Pts',(-25.4398808418846,1.37999255490122,-0.602135677942593));
#61816=CARTESIAN_POINT('Ctrl Pts',(-25.3603372146676,1.2526482517857,0.835355722750746));
#61817=CARTESIAN_POINT('Ctrl Pts',(-25.2807935874506,-0.0254786092609561,
1.50542275348299));
#61818=CARTESIAN_POINT('Ctrl Pts',(-25.2012499602335,-1.280198788427,0.792488415274466));
#61819=CARTESIAN_POINT('Ctrl Pts',(-25.1217063330164,-1.35882629009462,
-0.648488966430325));
#61820=CARTESIAN_POINT('Ctrl Pts',(-25.0421627057993,-0.189127622248968,
-1.49371267944563));
#61821=CARTESIAN_POINT('Ctrl Pts',(-24.9626190785823,1.15431875856946,-0.966692831176921));
#61822=CARTESIAN_POINT('Ctrl Pts',(-24.8830754513652,1.43731589375105,0.448408126381329));
#61823=CARTESIAN_POINT('Ctrl Pts',(-24.8035318241482,0.399880051512201,
1.45156562739574));
#61824=CARTESIAN_POINT('Ctrl Pts',(-24.7239881969311,-1.00491748854471,
1.12119920953021));
#61825=CARTESIAN_POINT('Ctrl Pts',(-24.6444445697141,-1.48651770139613,
-0.239190195597884));
#61826=CARTESIAN_POINT('Ctrl Pts',(-24.564900942497,-0.602484233456529,
-1.3798404163781));
#61827=CARTESIAN_POINT('Ctrl Pts',(-24.48535731528,0.835039287498288,-1.25285921578146));
#61828=CARTESIAN_POINT('Ctrl Pts',(-24.4058136880629,1.50542914114434,0.025098351092998));
#61829=CARTESIAN_POINT('Ctrl Pts',(-24.3262700608458,0.792811757634631,
1.27999857155798));
#61830=CARTESIAN_POINT('Ctrl Pts',(-24.2467264336288,-0.648145717443526,
1.35899004970375));
#61831=CARTESIAN_POINT('Ctrl Pts',(-24.1671828064117,-1.49366485971877,
0.189504915702711));
#61832=CARTESIAN_POINT('Ctrl Pts',(-24.0876391791947,-0.966984371723771,
-1.15407454311936));
#61833=CARTESIAN_POINT('Ctrl Pts',(-24.0080955519776,0.44804505795169,-1.4374291120884));
#61834=CARTESIAN_POINT('Ctrl Pts',(-23.9285519247605,1.45146457469027,-0.400246692245398));
#61835=CARTESIAN_POINT('Ctrl Pts',(-23.8490082975435,1.1214530076211,1.00463425082552));
#61836=CARTESIAN_POINT('Ctrl Pts',(-23.7694646703264,-0.238814705872275,
1.48657807144237));
#61837=CARTESIAN_POINT('Ctrl Pts',(-23.6899210431094,-1.37968818981758,
0.602832750530412));
#61838=CARTESIAN_POINT('Ctrl Pts',(-23.6103774158923,-1.25307009984157,
-0.834722798968145));
#61839=CARTESIAN_POINT('Ctrl Pts',(-23.5308337886753,0.0247180913237032,
-1.50543543275542));
#61840=CARTESIAN_POINT('Ctrl Pts',(-23.4512901614581,1.27979827302174,-0.79313504941136));
#61841=CARTESIAN_POINT('Ctrl Pts',(-23.3717465342411,1.35915372260579,0.647802427103359));
#61842=CARTESIAN_POINT('Ctrl Pts',(-23.292202907024,0.18988219706556,1.49361694469223));
#61843=CARTESIAN_POINT('Ctrl Pts',(-23.212659279807,-1.15383025403633,0.967275850574507));
#61844=CARTESIAN_POINT('Ctrl Pts',(-23.1331156525899,-1.43754223871406,
-0.447681960935607));
#61845=CARTESIAN_POINT('Ctrl Pts',(-23.0535720253729,-0.400613307441811,
-1.4513634293776));
#61846=CARTESIAN_POINT('Ctrl Pts',(-22.9740283981558,1.00435094900806,-1.1217067341604));
#61847=CARTESIAN_POINT('Ctrl Pts',(-22.8944847709387,1.48663834664108,0.238439200909679));
#61848=CARTESIAN_POINT('Ctrl Pts',(-22.8149411437217,0.603181229142014,
1.37953587522939));
#61849=CARTESIAN_POINT('Ctrl Pts',(-22.7353975165046,-0.834406257180535,
1.25328090395256));
#61850=CARTESIAN_POINT('Ctrl Pts',(-22.6558538892876,-1.50544162831582,
-0.0243378299773199));
#61851=CARTESIAN_POINT('Ctrl Pts',(-22.5763102620705,-0.793458290584012,
-1.27959789283106));
#61852=CARTESIAN_POINT('Ctrl Pts',(-22.4967666348535,0.647459095431727,
-1.35931730879031));
#61853=CARTESIAN_POINT('Ctrl Pts',(-22.4172230076364,1.49356893436906,-0.190259466313405));
#61854=CARTESIAN_POINT('Ctrl Pts',(-22.3376793804193,0.967567267710527,
1.15358589133595));
#61855=CARTESIAN_POINT('Ctrl Pts',(-22.2581357532023,-0.447318835356281,
1.4376552736208));
#61856=CARTESIAN_POINT('Ctrl Pts',(-22.1785921259852,-1.4512621914642,0.400979897078039));
#61857=CARTESIAN_POINT('Ctrl Pts',(-22.0990484987682,-1.12196038913188,
-1.00406758311043));
#61858=CARTESIAN_POINT('Ctrl Pts',(-22.0195048715511,0.23806368073406,-1.48669852698842));
#61859=CARTESIAN_POINT('Ctrl Pts',(-21.939961244334,1.37938347262324,-0.603529669269067));
#61860=CARTESIAN_POINT('Ctrl Pts',(-21.860417617117,1.25349162810098,0.834089662155657));
#61861=CARTESIAN_POINT('Ctrl Pts',(-21.7808739898999,-0.0239575670781471,
1.50544772782514));
#61862=CARTESIAN_POINT('Ctrl Pts',(-21.7013303626828,-1.27939743099873,
0.793781481131954));
#61863=CARTESIAN_POINT('Ctrl Pts',(-21.6217867354658,-1.35948080824685,
-0.647115722450521));
#61864=CARTESIAN_POINT('Ctrl Pts',(-21.5422431082487,-0.190636723422224,
-1.49352082875232));
#61865=CARTESIAN_POINT('Ctrl Pts',(-21.4626994810317,1.1533414550338,-0.96785862311327));
#61866=CARTESIAN_POINT('Ctrl Pts',(-21.3831558538146,1.43776821680141,0.446955681236838));
#61867=CARTESIAN_POINT('Ctrl Pts',(-21.3036122265976,0.40134646113074,1.4511608609565));
#61868=CARTESIAN_POINT('Ctrl Pts',(-21.2240685993805,-1.00378415315067,
1.1222139725194));
#61869=CARTESIAN_POINT('Ctrl Pts',(-21.1445249721634,-1.48675861248054,
-0.237688145369336));
#61870=CARTESIAN_POINT('Ctrl Pts',(-21.0649813449464,-0.603878070889381,
-1.37923098200885));
#61871=CARTESIAN_POINT('Ctrl Pts',(-20.9854377177293,0.833773013913679,
-1.2537022722734));
#61872=CARTESIAN_POINT('Ctrl Pts',(-20.9058940905122,1.505453731283,0.0235773026504012));
#61873=CARTESIAN_POINT('Ctrl Pts',(-20.8263504632952,0.794104621034608,
1.27919688753752));
#61874=CARTESIAN_POINT('Ctrl Pts',(-20.7468068360781,-0.646772308181659,
1.35964422096501));
#61875=CARTESIAN_POINT('Ctrl Pts',(-20.6672632088611,-1.49347262784509,
0.191013968367933));
#61876=CARTESIAN_POINT('Ctrl Pts',(-20.587719581644,-0.96814991676412,-1.15309694514547));
#61877=CARTESIAN_POINT('Ctrl Pts',(-20.508175954427,0.446592498600472,-1.43788106824869));
#61878=CARTESIAN_POINT('Ctrl Pts',(-20.4286323272099,1.45105943786099,-0.40171299957647));
#61879=CARTESIAN_POINT('Ctrl Pts',(-20.3490886999928,1.12246748430675,1.00350065914689));
#61880=CARTESIAN_POINT('Ctrl Pts',(-20.2695450727758,-0.23731259483952,
1.48681860311361));
#61881=CARTESIAN_POINT('Ctrl Pts',(-20.1900014455587,-1.37907840339596,
0.604226433980696));
#61882=CARTESIAN_POINT('Ctrl Pts',(-20.1104578183417,-1.25391283645635,
-0.833456312474847));
#61883=CARTESIAN_POINT('Ctrl Pts',(-20.0309141911246,0.0231970367183806,
-1.50545963868902));
#61884=CARTESIAN_POINT('Ctrl Pts',(-19.9513705639075,1.27899626246024,-0.794427710271308));
#61885=CARTESIAN_POINT('Ctrl Pts',(-19.8718269366905,1.35980754693434,0.646428852647062));
#61886=CARTESIAN_POINT('Ctrl Pts',(-19.7922833094734,0.191391201126432,
1.49342433165044));
#61887=CARTESIAN_POINT('Ctrl Pts',(-19.7127396822564,-1.15285236168658,
0.968441148644485));
#61888=CARTESIAN_POINT('Ctrl Pts',(-19.6331960550393,-1.43799382795542,
-0.446229287470345));
#61889=CARTESIAN_POINT('Ctrl Pts',(-19.5536524278222,-0.402079512391888,
-1.45095792218413));
#61890=CARTESIAN_POINT('Ctrl Pts',(-19.4741088006052,1.00321710111716,-1.12272092447779));
#61891=CARTESIAN_POINT('Ctrl Pts',(-19.3945651733881,1.48687849888381,0.23693702916853));
#61892=CARTESIAN_POINT('Ctrl Pts',(-19.3150215461711,0.604574758520824,
1.37892573679429));
#61893=CARTESIAN_POINT('Ctrl Pts',(-19.235477918954,-0.83313955785933,1.25412332063643));
#61894=CARTESIAN_POINT('Ctrl Pts',(-19.1559342917369,-1.50546545004281,
-0.0228167693063023));
#61895=CARTESIAN_POINT('Ctrl Pts',(-19.0763906645199,-0.794750748821478,
-1.27879555577969));
#61896=CARTESIAN_POINT('Ctrl Pts',(-18.9968470373028,0.646085355868609,
-1.35997078614444));
#61897=CARTESIAN_POINT('Ctrl Pts',(-18.9173034100858,1.49337594017145,-0.191768421673692));
#61898=CARTESIAN_POINT('Ctrl Pts',(-18.8377597828687,0.96873231873582,1.15260770467272));
#61899=CARTESIAN_POINT('Ctrl Pts',(-18.7582161556517,-0.445866047869633,
1.43810649591444));
#61900=CARTESIAN_POINT('Ctrl Pts',(-18.6786725284346,-1.45085631393239,
0.402445999553601));
#61901=CARTESIAN_POINT('Ctrl Pts',(-18.5991289012175,-1.12297429301632,
-1.00293347907958));
#61902=CARTESIAN_POINT('Ctrl Pts',(-18.5195852740005,0.236561448380347,
-1.48693829978732));
#61903=CARTESIAN_POINT('Ctrl Pts',(-18.4400416467834,1.37877298221359,-0.604923044487492));
#61904=CARTESIAN_POINT('Ctrl Pts',(-18.3604980195663,1.25433372480018,0.832822750087366));
#61905=CARTESIAN_POINT('Ctrl Pts',(-18.2809543923493,-0.0224365004384819,
1.50547116534401));
#61906=CARTESIAN_POINT('Ctrl Pts',(-18.2014107651322,-1.27859476750868,
0.795073736664478));
#61907=CARTESIAN_POINT('Ctrl Pts',(-18.1218671379152,-1.36013393858487,
-0.645741817868261));
#61908=CARTESIAN_POINT('Ctrl Pts',(-18.0423235106981,-0.192145629985613,
-1.49332745341121));
#61909=CARTESIAN_POINT('Ctrl Pts',(-17.9627798834811,1.15236297411951,-0.969023427019504));
#61910=CARTESIAN_POINT('Ctrl Pts',(-17.883236256264,1.43821907211853,0.445502779821528));
#61911=CARTESIAN_POINT('Ctrl Pts',(-17.8036926290469,0.402812461038192,
1.45075461311227));
#61912=CARTESIAN_POINT('Ctrl Pts',(-17.7241490018299,-1.00264979305227,
1.12322758990617));
#61913=CARTESIAN_POINT('Ctrl Pts',(-17.6446053746128,-1.4869980058203,-0.236185852498931));
#61914=CARTESIAN_POINT('Ctrl Pts',(-17.5650617473958,-0.60527129185852,
-1.37862013966361));
#61915=CARTESIAN_POINT('Ctrl Pts',(-17.4855181201787,0.832505889179132,
-1.25454404893421));
#61916=CARTESIAN_POINT('Ctrl Pts',(-17.4059744929616,1.50547678459225,0.0220562301391384));
#61917=CARTESIAN_POINT('Ctrl Pts',(-17.3264308657446,0.795396673779736,
1.27839389766));
#61918=CARTESIAN_POINT('Ctrl Pts',(-17.2468872385275,-0.645398238667895,
1.36029700424524));
#61919=CARTESIAN_POINT('Ctrl Pts',(-17.1673436113104,-1.49327887137281,
0.192522826038173));
#61920=CARTESIAN_POINT('Ctrl Pts',(-17.0877999840934,-0.969314473476995,
-1.15211817004255));
#61921=CARTESIAN_POINT('Ctrl Pts',(-17.0082563568763,0.445139483349166,
-1.43833155656052));
#61922=CARTESIAN_POINT('Ctrl Pts',(-16.9287127296593,1.45065281973025,-0.403178896822321));
#61923=CARTESIAN_POINT('Ctrl Pts',(-16.8491691024422,1.12348081513121,1.00236604305328));
#61924=CARTESIAN_POINT('Ctrl Pts',(-16.7696254752252,-0.235810241548242,
1.48705761697896));
#61925=CARTESIAN_POINT('Ctrl Pts',(-16.6900818480081,-1.37846720915408,
0.605619500611681));
#61926=CARTESIAN_POINT('Ctrl Pts',(-16.610538220791,-1.25475429302508,-0.832188975154876));
#61927=CARTESIAN_POINT('Ctrl Pts',(-16.530994593574,0.0216759584325402,
-1.50548230778718));
#61928=CARTESIAN_POINT('Ctrl Pts',(-16.4514509663569,1.27819294624648,-0.79571956014662));
#61929=CARTESIAN_POINT('Ctrl Pts',(-16.3719073391399,1.36045998311514,0.645054618289458));
#61930=CARTESIAN_POINT('Ctrl Pts',(-16.2923637119228,0.192900009807252,
1.49323019405936));
#61931=CARTESIAN_POINT('Ctrl Pts',(-16.2128200847058,-1.15187329245748,
0.969605458089701));
#61932=CARTESIAN_POINT('Ctrl Pts',(-16.1332764574887,-1.43844394923324,
-0.444776158475778));
#61933=CARTESIAN_POINT('Ctrl Pts',(-16.0537328302716,-0.403545306882577,
-1.45055093379282));
#61934=CARTESIAN_POINT('Ctrl Pts',(-15.9741892030546,1.00208222910077,-1.12373396867525));
#61935=CARTESIAN_POINT('Ctrl Pts',(-15.8946455758375,1.4871171332595,0.235434615552267));
#61936=CARTESIAN_POINT('Ctrl Pts',(-15.8151019486204,0.605967670724726,
1.37831419069479));
#61937=CARTESIAN_POINT('Ctrl Pts',(-15.7355583214034,-0.831872008034821,
1.25496445705936));
#61938=CARTESIAN_POINT('Ctrl Pts',(-15.6560146941863,-1.50548773492844,
-0.0212956853429847));
#61939=CARTESIAN_POINT('Ctrl Pts',(-15.5764710669693,-0.796042395744522,
-1.27799191328095));
#61940=CARTESIAN_POINT('Ctrl Pts',(-15.4969274397522,0.644710956754863,
-1.36062287518416));
#61941=CARTESIAN_POINT('Ctrl Pts',(-15.4173838125351,1.49318142147395,-0.193277181268826));
#61942=CARTESIAN_POINT('Ctrl Pts',(-15.3378401853181,0.969896380839092,
1.1516283413799));
#61943=CARTESIAN_POINT('Ctrl Pts',(-15.2582965581011,-0.444412805224505,
1.43855625012951));
#61944=CARTESIAN_POINT('Ctrl Pts',(-15.178752930884,-1.45044895530648,0.403911691195623));
#61945=CARTESIAN_POINT('Ctrl Pts',(-15.0992093036669,-1.12398705052216,
-1.0017983512128));
#61946=CARTESIAN_POINT('Ctrl Pts',(-15.0196656764499,0.235058974534927,
-1.48717655465811));
#61947=CARTESIAN_POINT('Ctrl Pts',(-14.9401220492328,1.37816108429549,-0.606315802175471));
#61948=CARTESIAN_POINT('Ctrl Pts',(-14.8605784220157,1.25517454102367,0.831554987839188));
#61949=CARTESIAN_POINT('Ctrl Pts',(-14.7810347947987,-0.0209154108947242,
1.50549306601567));
#61950=CARTESIAN_POINT('Ctrl Pts',(-14.7014911675816,-1.27779079877622,
0.796365180552865));
#61951=CARTESIAN_POINT('Ctrl Pts',(-14.6219475403646,-1.36078568044193,
-0.644367254086051));
#61952=CARTESIAN_POINT('Ctrl Pts',(-14.5424039131475,-0.193654340398797,
-1.49313255361971));
#61953=CARTESIAN_POINT('Ctrl Pts',(-14.4628602859304,1.15138331682546,-0.970187241706543));
#61954=CARTESIAN_POINT('Ctrl Pts',(-14.3833166587134,1.43866845924216,0.444049423618571));
#61955=CARTESIAN_POINT('Ctrl Pts',(-14.3037730314963,0.404278049738003,
1.45034688427777));
#61956=CARTESIAN_POINT('Ctrl Pts',(-14.2242294042793,-1.00151440940753,
1.12424006065575));
#61957=CARTESIAN_POINT('Ctrl Pts',(-14.1446857770622,-1.48723588117101,
-0.234683318520279));
#61958=CARTESIAN_POINT('Ctrl Pts',(-14.0651421498451,-0.606663894941661,
-1.37800788996596));
#61959=CARTESIAN_POINT('Ctrl Pts',(-13.9855985226281,0.8312379145882,-1.25538454490456));
#61960=CARTESIAN_POINT('Ctrl Pts',(-13.906054895411,1.50549830104856,0.0205351351119899));
#61961=CARTESIAN_POINT('Ctrl Pts',(-13.8265112681939,0.796687914551029,
1.27758960274516));
#61962=CARTESIAN_POINT('Ctrl Pts',(-13.7469676409769,-0.644023510304975,
1.36094839887803));
#61963=CARTESIAN_POINT('Ctrl Pts',(-13.6674240137598,-1.49308359049973,
0.194031487173097));
#61964=CARTESIAN_POINT('Ctrl Pts',(-13.5878803865428,-0.970478040673556,
-1.15113821880979));
#61965=CARTESIAN_POINT('Ctrl Pts',(-13.5083367593257,0.443686013681124,
-1.43878057656404));
#61966=CARTESIAN_POINT('Ctrl Pts',(-13.4287931321087,1.45024472071316,-0.404644382486428));
#61967=CARTESIAN_POINT('Ctrl Pts',(-13.3492495048916,1.12449299905994,1.00123040370303));
#61968=CARTESIAN_POINT('Ctrl Pts',(-13.2697058776745,-0.234307647532164,
1.4872951127944));
#61969=CARTESIAN_POINT('Ctrl Pts',(-13.1901622504575,-1.37785460771592,
0.607011949001187));
#61970=CARTESIAN_POINT('Ctrl Pts',(-13.1106186232404,-1.25559446868872,
-0.830920788302052));
#61971=CARTESIAN_POINT('Ctrl Pts',(-13.0310749960233,0.020154858019065,
-1.50550344002676));
#61972=CARTESIAN_POINT('Ctrl Pts',(-12.9515313688063,1.27738832520053,-0.797010597718466));
#61973=CARTESIAN_POINT('Ctrl Pts',(-12.8719877415892,1.36111103048212,0.643679725433465));
#61974=CARTESIAN_POINT('Ctrl Pts',(-12.7924441143722,0.194408621567738,
1.49303453211717));
#61975=CARTESIAN_POINT('Ctrl Pts',(-12.7129004871551,-1.15089304734852,
0.970768777721553));
#61976=CARTESIAN_POINT('Ctrl Pts',(-12.6333568599381,-1.43889260208799,
-0.443322575435331));
#61977=CARTESIAN_POINT('Ctrl Pts',(-12.553813232721,-0.405010689417524,
-1.45014246461917));
#61978=CARTESIAN_POINT('Ctrl Pts',(-12.474269605504,1.00094633411743,-1.1247458657186));
#61979=CARTESIAN_POINT('Ctrl Pts',(-12.3947259782869,1.48735424952452,0.233931961594643));
#61980=CARTESIAN_POINT('Ctrl Pts',(-12.3151823510698,0.607359964331746,
1.37770123755521));
#61981=CARTESIAN_POINT('Ctrl Pts',(-12.2356387238528,-0.830603609001021,
1.25580431236267));
#61982=CARTESIAN_POINT('Ctrl Pts',(-12.1560950966357,-1.50550848294994,
-0.0197745796402064));
#61983=CARTESIAN_POINT('Ctrl Pts',(-12.0765514694186,-0.797333230034552,
-1.27718696615524));
#61984=CARTESIAN_POINT('Ctrl Pts',(-11.9970078422016,0.643335899493558,
-1.36127357524379));
#61985=CARTESIAN_POINT('Ctrl Pts',(-11.9174642149845,1.49298537847513,-0.19478574355858));
#61986=CARTESIAN_POINT('Ctrl Pts',(-11.8379205877675,0.971059452831992,
1.15064780245729));
#61987=CARTESIAN_POINT('Ctrl Pts',(-11.7583769605504,-0.442959108904438,
1.43900453580687));
#61988=CARTESIAN_POINT('Ctrl Pts',(-11.6788333333333,-1.45004011600234,
0.405376970507859));
#61989=CARTESIAN_POINT('Ctrl Pts',(-11.5992897061163,-1.12499866061553,
-1.00066220066888));
#61990=CARTESIAN_POINT('Ctrl Pts',(-11.5197460788992,0.233556260731656,
-1.48741329135758));
#61991=CARTESIAN_POINT('Ctrl Pts',(-11.4402024516822,1.37754777949356,-0.607707940911187));
#61992=CARTESIAN_POINT('Ctrl Pts',(-11.3606588244651,1.25601407591308,0.830286376705301));
#61993=CARTESIAN_POINT('Ctrl Pts',(-11.281115197248,-0.0193942999996536,
1.50551342981779));
#61994=CARTESIAN_POINT('Ctrl Pts',(-11.201571570031,-1.27698552562212,0.797655811478712));
#61995=CARTESIAN_POINT('Ctrl Pts',(-11.1220279428139,-1.36143603315269,
-0.642992032507123));
#61996=CARTESIAN_POINT('Ctrl Pts',(-11.0424843155969,-0.195162853121622,
-1.49293612957676));
#61997=CARTESIAN_POINT('Ctrl Pts',(-10.9629406883798,1.15040248415175,-0.971350065986352));
#61998=CARTESIAN_POINT('Ctrl Pts',(-10.8833970611627,1.43911637771354,0.442595614111609));
#61999=CARTESIAN_POINT('Ctrl Pts',(-10.8038534339457,0.405743225734111,
1.44993767486918));
#62000=CARTESIAN_POINT('Ctrl Pts',(-10.7243098067286,-1.00037800337546,
1.12525138373465));
#62001=CARTESIAN_POINT('Ctrl Pts',(-10.6447661795116,-1.48747223828985,
-0.23318054496715));
#62002=CARTESIAN_POINT('Ctrl Pts',(-10.5652225522945,-0.608055878717266,
-1.37739423354083));
#62003=CARTESIAN_POINT('Ctrl Pts',(-10.4856789250774,0.829969091435158,
-1.25622375932652));
#62004=CARTESIAN_POINT('Ctrl Pts',(-10.4061352978604,1.50551828062998,0.0190140191216825));
#62005=CARTESIAN_POINT('Ctrl Pts',(-10.3265916706433,0.797978342030396,
1.27678400361401));
#62006=CARTESIAN_POINT('Ctrl Pts',(-10.2470480434263,-0.642648124496163,
1.36159840419844));
#62007=CARTESIAN_POINT('Ctrl Pts',(-10.1675044162092,-1.4928867854252,0.195539950232733));
#62008=CARTESIAN_POINT('Ctrl Pts',(-10.0879607889921,-0.971640617166035,
-1.15015709244756));
#62009=CARTESIAN_POINT('Ctrl Pts',(-10.0084171617751,0.442232091080033,
-1.43922812780085));
#62010=CARTESIAN_POINT('Ctrl Pts',(-9.92887353455803,1.44983514122626,-0.406109455072875));
#62011=CARTESIAN_POINT('Ctrl Pts',(-9.84932990734096,1.1255040350598,1.00009374225535));
#62012=CARTESIAN_POINT('Ctrl Pts',(-9.76978628012392,-0.232804814325147,
1.48753109031752));
#62013=CARTESIAN_POINT('Ctrl Pts',(-9.69024265290684,-1.37724059970678,
0.608403777727809));
#62014=CARTESIAN_POINT('Ctrl Pts',(-9.61069902568979,-1.25643336258963,
-0.829651753210869));
#62015=CARTESIAN_POINT('Ctrl Pts',(-9.53115539847272,0.0186337370306052,
-1.5055230353862));
#62016=CARTESIAN_POINT('Ctrl Pts',(-9.45161177125567,1.27658240014378,-0.798300821668966));
#62017=CARTESIAN_POINT('Ctrl Pts',(-9.37206814403861,1.36176068837068,0.642304175482586));
#62018=CARTESIAN_POINT('Ctrl Pts',(-9.29252451682155,0.195917034867912,
1.49283734602358));
#62019=CARTESIAN_POINT('Ctrl Pts',(-9.21298088960449,-1.14991162736034,
0.971931106352556));
#62020=CARTESIAN_POINT('Ctrl Pts',(-9.13343726238743,-1.43933978606171,
-0.441868539832883));
#62021=CARTESIAN_POINT('Ctrl Pts',(-9.05389363517037,-0.406475658500802,
-1.44973251508011));
#62022=CARTESIAN_POINT('Ctrl Pts',(-8.97435000795331,0.999809417326651,
-1.12575661457488));
#62023=CARTESIAN_POINT('Ctrl Pts',(-8.89480638073625,1.48758984743686,0.232429068829558));
#62024=CARTESIAN_POINT('Ctrl Pts',(-8.81526275351918,0.608751637920644,
1.37708687800122));
#62025=CARTESIAN_POINT('Ctrl Pts',(-8.73571912630213,-0.829334362052652,
1.25664288568904));
#62026=CARTESIAN_POINT('Ctrl Pts',(-8.65617549908508,-1.50552769408614,
-0.0182534537506204));
#62027=CARTESIAN_POINT('Ctrl Pts',(-8.576631871868,-0.798623250373908,-1.27638071522427));
#62028=CARTESIAN_POINT('Ctrl Pts',(-8.49708824465096,0.641960185488325,
-1.3619228856591));
#62029=CARTESIAN_POINT('Ctrl Pts',(-8.41754461743388,1.49278781137509,-0.196294107003054));
#62030=CARTESIAN_POINT('Ctrl Pts',(-8.33800099021684,0.97222153352733,1.14966608890581));
#62031=CARTESIAN_POINT('Ctrl Pts',(-8.25845736299977,-0.441504960393397,
1.43945135248894));
#62032=CARTESIAN_POINT('Ctrl Pts',(-8.17891373578272,-1.44962979643727,
0.406841835994534));
#62033=CARTESIAN_POINT('Ctrl Pts',(-8.09937010856564,-1.12600912226377,
-0.999525028607551));
#62034=CARTESIAN_POINT('Ctrl Pts',(-8.0198264813486,0.232053308504426,-1.48764850964411));
#62035=CARTESIAN_POINT('Ctrl Pts',(-7.94028285413152,1.37693306843394,-0.609099459273521));
#62036=CARTESIAN_POINT('Ctrl Pts',(-7.86073922691448,1.25685232861138,0.829016917980754));
#62037=CARTESIAN_POINT('Ctrl Pts',(-7.78119559969741,-0.0178731693060422,
1.50553225672953));
#62038=CARTESIAN_POINT('Ctrl Pts',(-7.70165197248036,-1.27617894886838,
0.798945628124588));
#62039=CARTESIAN_POINT('Ctrl Pts',(-7.6221083452633,-1.36208499605328,-0.641616154535358));
#62040=CARTESIAN_POINT('Ctrl Pts',(-7.54256471804624,-0.196671166614124,
-1.49273818148288));
#62041=CARTESIAN_POINT('Ctrl Pts',(-7.46302109082917,1.14942047709957,-0.972511898671863));
#62042=CARTESIAN_POINT('Ctrl Pts',(-7.38347746361211,1.43956282707545,0.441141352784717));
#62043=CARTESIAN_POINT('Ctrl Pts',(-7.30393383639506,0.407207987530731,
1.4495269853043));
#62044=CARTESIAN_POINT('Ctrl Pts',(-7.22439020917799,-0.999240576116165,
1.12626155811037));
#62045=CARTESIAN_POINT('Ctrl Pts',(-7.14484658196094,-1.48770707693553,
-0.231677533373667));
#62046=CARTESIAN_POINT('Ctrl Pts',(-7.06530295474388,-0.609447241764305,
-1.37677917101476));
#62047=CARTESIAN_POINT('Ctrl Pts',(-6.98575932752682,0.828699421015416,
-1.25706169134332));
#62048=CARTESIAN_POINT('Ctrl Pts',(-6.90621570030976,1.50553672331607,0.0174928837211134));
#62049=CARTESIAN_POINT('Ctrl Pts',(-6.8266720730927,0.799267954900482,1.27597710108895));
#62050=CARTESIAN_POINT('Ctrl Pts',(-6.74712844587562,-0.641272082645586,
1.36224701954293));
#62051=CARTESIAN_POINT('Ctrl Pts',(-6.6675848186586,-1.49268845635011,0.197048213677092));
#62052=CARTESIAN_POINT('Ctrl Pts',(-6.5880411914415,-0.972802201767608,
-1.14917479195737));
#62053=CARTESIAN_POINT('Ctrl Pts',(-6.50849756422447,0.440777717030083,
-1.43967420981412));
#62054=CARTESIAN_POINT('Ctrl Pts',(-6.42895393700739,1.44942408168774,-0.407574113086008));
#62055=CARTESIAN_POINT('Ctrl Pts',(-6.34941030979035,1.12651392209859,0.998956059870634));
#62056=CARTESIAN_POINT('Ctrl Pts',(-6.26986668257328,-0.231301743461309,
1.48776554930739));
#62057=CARTESIAN_POINT('Ctrl Pts',(-6.19032305535623,-1.37662518575351,
0.609794985370748));
#62058=CARTESIAN_POINT('Ctrl Pts',(-6.11077942813915,-1.25727097387143,
-0.828381871176925));
#62059=CARTESIAN_POINT('Ctrl Pts',(-6.0312358009221,0.0171125970200911,
-1.50554109384546));
#62060=CARTESIAN_POINT('Ctrl Pts',(-5.95169217370504,1.2757751718989,-0.799590230680999));
#62061=CARTESIAN_POINT('Ctrl Pts',(-5.87214854648798,1.36240895611768,0.64092796984103));
#62062=CARTESIAN_POINT('Ctrl Pts',(-5.79260491927093,0.197425248167845,
1.49263863597994));
#62063=CARTESIAN_POINT('Ctrl Pts',(-5.71306129205386,-1.14892903349483,
0.973092442796056));
#62064=CARTESIAN_POINT('Ctrl Pts',(-5.63351766483681,-1.43978550069785,
-0.440414053152718));
#62065=CARTESIAN_POINT('Ctrl Pts',(-5.55397403761974,-0.407940212636969,
-1.44932108559419));
#62066=CARTESIAN_POINT('Ctrl Pts',(-5.47443041040269,0.998671479889131,
-1.12676621421227));
#62067=CARTESIAN_POINT('Ctrl Pts',(-5.39488678318562,1.48782392675596,0.230925938791301));
#62068=CARTESIAN_POINT('Ctrl Pts',(-5.31534315596856,0.610142690070709,
1.37647111265999));
#62069=CARTESIAN_POINT('Ctrl Pts',(-5.23579952875151,-0.828064268485496,
1.25748017618243));
#62070=CARTESIAN_POINT('Ctrl Pts',(-5.15625590153445,-1.50554536831745,
-0.0167323092272154));
#62071=CARTESIAN_POINT('Ctrl Pts',(-5.07671227431738,-0.799912455445589,
-1.27557316131109));
#62072=CARTESIAN_POINT('Ctrl Pts',(-4.99716864710033,0.64058381614358,-1.36257080576721));
#62073=CARTESIAN_POINT('Ctrl Pts',(-4.91762501988326,1.49258872037557,-0.197802270062393));
#62074=CARTESIAN_POINT('Ctrl Pts',(-4.83808139266621,0.973382621738716,
1.14868320172765));
#62075=CARTESIAN_POINT('Ctrl Pts',(-4.75853776544914,-0.440050361175798,
1.43989669971953));
#62076=CARTESIAN_POINT('Ctrl Pts',(-4.67899413823209,-1.44921799703017,
0.408306286160309));
#62077=CARTESIAN_POINT('Ctrl Pts',(-4.59945051101503,-1.12701843443538,
-0.998386836189773));
#62078=CARTESIAN_POINT('Ctrl Pts',(-4.51990688379797,0.230550119387597,
-1.48788220927752));
#62079=CARTESIAN_POINT('Ctrl Pts',(-4.44036325658091,1.37631695174408,-0.610490355841967));
#62080=CARTESIAN_POINT('Ctrl Pts',(-4.36081962936385,1.25768929826291,0.827746612961421));
#62081=CARTESIAN_POINT('Ctrl Pts',(-4.28127600214679,-0.0163520203667641,
1.50554954673173));
#62082=CARTESIAN_POINT('Ctrl Pts',(-4.20173237492973,-1.27537106933841,
0.800234629173721));
#62083=CARTESIAN_POINT('Ctrl Pts',(-4.12218874771268,-1.36273256848119,
-0.640239621575252));
#62084=CARTESIAN_POINT('Ctrl Pts',(-4.04264512049561,-0.198179279336608,
-1.49253870954017));
#62085=CARTESIAN_POINT('Ctrl Pts',(-3.96310149327855,1.1484372966715,-0.973672738577014));
#62086=CARTESIAN_POINT('Ctrl Pts',(-3.88355786606149,1.44000780687209,0.439686641122523));
#62087=CARTESIAN_POINT('Ctrl Pts',(-3.80401423884443,0.408672333632629,
1.44911481600231));
#62088=CARTESIAN_POINT('Ctrl Pts',(-3.72447061162738,-0.998102128790777,
1.12727058275177));
#62089=CARTESIAN_POINT('Ctrl Pts',(-3.64492698441031,-1.48794039686834,
-0.230174285274219));
#62090=CARTESIAN_POINT('Ctrl Pts',(-3.56538335719326,-0.610837982662363,
-1.37616270301558));
#62091=CARTESIAN_POINT('Ctrl Pts',(-3.48583972997619,0.827428904625004,
-1.25789834009956));
#62092=CARTESIAN_POINT('Ctrl Pts',(-3.40629610275914,1.50555362908805,0.0159717304630367));
#62093=CARTESIAN_POINT('Ctrl Pts',(-3.32675247554207,0.800556751844799,
1.27516889599378));
#62094=CARTESIAN_POINT('Ctrl Pts',(-3.24720884832502,-0.639895386158011,
1.36289424424926));
#62095=CARTESIAN_POINT('Ctrl Pts',(-3.16766522110796,-1.49248860347686,
0.198556275966578));
#62096=CARTESIAN_POINT('Ctrl Pts',(-3.08812159389089,-0.973962793292614,
-1.14819131834222));
#62097=CARTESIAN_POINT('Ctrl Pts',(-3.00857796667384,0.439322893016301,
-1.44011882214814));
#62098=CARTESIAN_POINT('Ctrl Pts',(-2.92903433945677,1.44901154251677,-0.409038355031158));
#62099=CARTESIAN_POINT('Ctrl Pts',(-2.84949071223972,1.12752265914617,0.997817357711321));
#62100=CARTESIAN_POINT('Ctrl Pts',(-2.76994708502266,-0.229798436476582,
1.48799848952268));
#62101=CARTESIAN_POINT('Ctrl Pts',(-2.6904034578056,-1.37600836648151,0.611185570513587));
#62102=CARTESIAN_POINT('Ctrl Pts',(-2.61085983058853,-1.2581073016844,-0.827111143503776));
#62103=CARTESIAN_POINT('Ctrl Pts',(-2.53131620337148,0.0155914395504356,
-1.50555761537229));
#62104=CARTESIAN_POINT('Ctrl Pts',(-2.45177257615442,1.27496664127071,-0.800878823464588));
#62105=CARTESIAN_POINT('Ctrl Pts',(-2.37222894893736,1.3630558330979,0.639551109963632));
#62106=CARTESIAN_POINT('Ctrl Pts',(-2.2926853217203,0.198933259858434,1.49243840209429));
#62107=CARTESIAN_POINT('Ctrl Pts',(-2.21314169450324,-1.14794526662311,
0.974252786046452));
#62108=CARTESIAN_POINT('Ctrl Pts',(-2.13359806728618,-1.44022974579189,
-0.438959117221064));
#62109=CARTESIAN_POINT('Ctrl Pts',(-2.05405444006912,-0.409404349855524,
-1.4489081759335));
#62110=CARTESIAN_POINT('Ctrl Pts',(-1.97451081285206,0.997532522064249,
-1.12777466482976));
#62111=CARTESIAN_POINT('Ctrl Pts',(-1.894967185635,1.48805648895523,0.229422575348086));
#62112=CARTESIAN_POINT('Ctrl Pts',(-1.81542355841794,0.611533116111903,
1.37585393773064));
#62113=CARTESIAN_POINT('Ctrl Pts',(-1.73587993120088,-0.826793323427721,
1.25831619139526));
#62114=CARTESIAN_POINT('Ctrl Pts',(-1.65633630398382,-1.50556151733331,
-0.0152111635795861));
#62115=CARTESIAN_POINT('Ctrl Pts',(-1.57679267676677,-0.801200821712858,
-1.2747642749542));
#62116=CARTESIAN_POINT('Ctrl Pts',(-1.4972490495497,0.639206750689721,-1.36321739238898));
#62117=CARTESIAN_POINT('Ctrl Pts',(-1.41770542233265,1.49238818572684,-0.199310122096324));
#62118=CARTESIAN_POINT('Ctrl Pts',(-1.33816179511559,0.97454256435248,1.1476989348545));
#62119=CARTESIAN_POINT('Ctrl Pts',(-1.25861816789852,-0.438595024378369,
1.44034097006356));
#62120=CARTESIAN_POINT('Ctrl Pts',(-1.17907454068146,-1.44880526550185,
0.409769573563957));
#62121=CARTESIAN_POINT('Ctrl Pts',(-1.0995309134644,-1.12802555733051,-0.997246208780835));
#62122=CARTESIAN_POINT('Ctrl Pts',(-1.01998728624735,0.22904472334399,-1.48811707718389));
#62123=CARTESIAN_POINT('Ctrl Pts',(-0.940443659030285,1.37570317207231,
-0.611875528990654));
#62124=CARTESIAN_POINT('Ctrl Pts',(-0.860900031813226,1.25851788170227,
0.826465782811734));
#62125=CARTESIAN_POINT('Ctrl Pts',(-0.781356404596167,-0.0148173746002297,
1.50558367261418));
#62126=CARTESIAN_POINT('Ctrl Pts',(-0.701812777379109,-1.27458747328757,
0.801487941651361));
#62127=CARTESIAN_POINT('Ctrl Pts',(-0.622269150162049,-1.36333018639518,
-0.638796246547649));
#62128=CARTESIAN_POINT('Ctrl Pts',(-0.542725522944984,-0.199779384003955,
-1.49246336007472));
#62129=CARTESIAN_POINT('Ctrl Pts',(-0.463181895727926,1.14762810985679,
-0.974593930371403));
#62130=CARTESIAN_POINT('Ctrl Pts',(-0.383638268510868,1.44011730997828,
0.437777000149017));
#62131=CARTESIAN_POINT('Ctrl Pts',(-0.304094641293808,0.41078325908372,
1.44957660963075));
#62132=CARTESIAN_POINT('Ctrl Pts',(-0.224551014076749,-0.998300100086838,
1.12650835861515));
#62133=CARTESIAN_POINT('Ctrl Pts',(-0.171521929265376,-1.32265134589549,
0.225893933992271));
#62134=CARTESIAN_POINT('Ctrl Pts',(-0.145007386859689,-1.2582325722701,
-0.193338547834049));
#62135=CARTESIAN_POINT('Ctrl Pts',(-34.6914926131403,-0.592743564845966,
1.23319225136785));
#62136=CARTESIAN_POINT('Ctrl Pts',(-34.6649780707346,-1.00363282292421,
1.03569509444031));
#62137=CARTESIAN_POINT('Ctrl Pts',(-34.6119489859233,-1.60527835398769,
0.20107823259307));
#62138=CARTESIAN_POINT('Ctrl Pts',(-34.5324053587062,-1.03595602557903,
-1.24467622864298));
#62139=CARTESIAN_POINT('Ctrl Pts',(-34.4528617314891,0.486450185413046,
-1.54294323461826));
#62140=CARTESIAN_POINT('Ctrl Pts',(-34.3733181042721,1.56125942409536,-0.425764039114321));
#62141=CARTESIAN_POINT('Ctrl Pts',(-34.293774477055,1.20214066618724,1.08361093293141));
#62142=CARTESIAN_POINT('Ctrl Pts',(-34.214230849838,-0.261554730735344,
1.59694004015695));
#62143=CARTESIAN_POINT('Ctrl Pts',(-34.1346872226209,-1.4848627155046,0.643484672649936));
#62144=CARTESIAN_POINT('Ctrl Pts',(-34.0551435954039,-1.34411136080804,
-0.901280832617842));
#62145=CARTESIAN_POINT('Ctrl Pts',(-33.9755999681868,0.0314762749515779,
-1.61797686836768));
#62146=CARTESIAN_POINT('Ctrl Pts',(-33.8960563409697,1.37813232185068,-0.848313047507812));
#62147=CARTESIAN_POINT('Ctrl Pts',(-33.8165127137527,1.45873402811122,0.70070127041307));
#62148=CARTESIAN_POINT('Ctrl Pts',(-33.7369690865356,0.199222194592942,
1.60598368203102));
#62149=CARTESIAN_POINT('Ctrl Pts',(-33.6574254593185,-1.24330884096325,
1.03588768266065));
#62150=CARTESIAN_POINT('Ctrl Pts',(-33.5778818321015,-1.54363839982021,
-0.485860623633696));
#62151=CARTESIAN_POINT('Ctrl Pts',(-33.4983382048844,-0.425858042155266,
-1.56125688982344));
#62152=CARTESIAN_POINT('Ctrl Pts',(-33.4187945776674,1.08314914646654,-1.2023590110968));
#62153=CARTESIAN_POINT('Ctrl Pts',(-33.3392509504503,1.59708933824868,0.261122200705366));
#62154=CARTESIAN_POINT('Ctrl Pts',(-33.2597073232333,0.643815838820516,
1.48471548608867));
#62155=CARTESIAN_POINT('Ctrl Pts',(-33.1801636960162,-0.900918174839821,
1.34433088293534));
#62156=CARTESIAN_POINT('Ctrl Pts',(-33.1006200687992,-1.61799694742729,
-0.0310633233745565));
#62157=CARTESIAN_POINT('Ctrl Pts',(-33.021076441582,-0.848654707954505,
-1.37792024706712));
#62158=CARTESIAN_POINT('Ctrl Pts',(-32.941532814365,0.700329402766152,-1.45890978954474));
#62159=CARTESIAN_POINT('Ctrl Pts',(-32.8619891871479,1.60593509034306,-0.19962846994738));
#62160=CARTESIAN_POINT('Ctrl Pts',(-32.7824455599309,1.03620076057325,1.24304747312922));
#62161=CARTESIAN_POINT('Ctrl Pts',(-32.7029019327138,-0.485470203305545,
1.54376090187762));
#62162=CARTESIAN_POINT('Ctrl Pts',(-32.6233583054968,-1.5611495323407,0.426252480357849));
#62163=CARTESIAN_POINT('Ctrl Pts',(-32.5438146782797,-1.20263242999344,
-1.08284545400225));
#62164=CARTESIAN_POINT('Ctrl Pts',(-32.4642710510626,0.260718708470727,
-1.59715521929662));
#62165=CARTESIAN_POINT('Ctrl Pts',(-32.3847274238456,1.48455285426756,-0.644190858489808));
#62166=CARTESIAN_POINT('Ctrl Pts',(-32.3051837966285,1.34455838446256,0.900578586247502));
#62167=CARTESIAN_POINT('Ctrl Pts',(-32.2256401694115,-0.0306546191383235,
1.61800473844763));
#62168=CARTESIAN_POINT('Ctrl Pts',(-32.1460965421944,-1.37770584551247,
0.849002734107022));
#62169=CARTESIAN_POINT('Ctrl Pts',(-32.0665529149774,-1.45908663749064,
-0.699960872887939));
#62170=CARTESIAN_POINT('Ctrl Pts',(-31.9870092877603,-0.200034111067518,
-1.60588461406724));
#62171=CARTESIAN_POINT('Ctrl Pts',(-31.9074656605433,1.2427856985348,-1.03651471132854));
#62172=CARTESIAN_POINT('Ctrl Pts',(-31.8279220333262,1.54388347796431,0.485080246713917));
#62173=CARTESIAN_POINT('Ctrl Pts',(-31.7483784061091,0.426646800465404,
1.56104181460244));
#62174=CARTESIAN_POINT('Ctrl Pts',(-31.6688347788921,-1.0825416445573,1.20290590948875));
#62175=CARTESIAN_POINT('Ctrl Pts',(-31.589291151675,-1.59722102367513,-0.260315271956998));
#62176=CARTESIAN_POINT('Ctrl Pts',(-31.509747524458,-0.644565823763341,
-1.48439008960595));
#62177=CARTESIAN_POINT('Ctrl Pts',(-31.4302038972409,0.900238933191302,
-1.34478582028906));
#62178=CARTESIAN_POINT('Ctrl Pts',(-31.3506602700238,1.61801242992563,0.0302459235288119));
#62179=CARTESIAN_POINT('Ctrl Pts',(-31.2711166428068,0.84935070414651,1.37749135048094));
#62180=CARTESIAN_POINT('Ctrl Pts',(-31.1915730155897,-0.699592297325916,
1.45926339528072));
#62181=CARTESIAN_POINT('Ctrl Pts',(-31.1120293883726,-1.60583403587161,
0.200439737877182));
#62182=CARTESIAN_POINT('Ctrl Pts',(-31.0324857611556,-1.03682859566712,
-1.24252384383195));
#62183=CARTESIAN_POINT('Ctrl Pts',(-30.9529421339385,0.484690259023074,
-1.54400595597689));
#62184=CARTESIAN_POINT('Ctrl Pts',(-30.8733985067214,1.56093399734461,-0.427041093125412));
#62185=CARTESIAN_POINT('Ctrl Pts',(-30.7938548795045,1.20317931219395,1.08223776592412));
#62186=CARTESIAN_POINT('Ctrl Pts',(-30.7143112522873,-0.259911818812566,
1.59728672620964));
#62187=CARTESIAN_POINT('Ctrl Pts',(-30.6347676250703,-1.48422723024795,
0.644940747878795));
#62188=CARTESIAN_POINT('Ctrl Pts',(-30.5552239978532,-1.34501317030866,
-0.89989922268008));
#62189=CARTESIAN_POINT('Ctrl Pts',(-30.4756803706362,0.0298372259863291,
-1.61802001817944));
#62190=CARTESIAN_POINT('Ctrl Pts',(-30.3961367434191,1.37727676756359,-0.849698619990381));
#62191=CARTESIAN_POINT('Ctrl Pts',(-30.3165931162021,1.45944005996512,0.699223677125539));
#62192=CARTESIAN_POINT('Ctrl Pts',(-30.237049488985,0.200845351898754,1.60578335522094));
#62193=CARTESIAN_POINT('Ctrl Pts',(-30.1575058617679,-1.2422619098531,1.03714241385265));
#62194=CARTESIAN_POINT('Ctrl Pts',(-30.0779622345509,-1.54412833547777,
-0.484300240407358));
#62195=CARTESIAN_POINT('Ctrl Pts',(-29.9984186073338,-0.427435358539164,
-1.56082608049534));
#62196=CARTESIAN_POINT('Ctrl Pts',(-29.9188749801167,1.08193381824142,-1.2034526381331));
#62197=CARTESIAN_POINT('Ctrl Pts',(-29.8393313528997,1.5973523268331,0.259508349085033));
#62198=CARTESIAN_POINT('Ctrl Pts',(-29.7597877256826,0.64531563084537,1.48406427619244));
#62199=CARTESIAN_POINT('Ctrl Pts',(-29.6802440984655,-0.899559454752963,
1.34524043451292));
#62200=CARTESIAN_POINT('Ctrl Pts',(-29.6007004712485,-1.61802750319939,
-0.0294285265401461));
#62201=CARTESIAN_POINT('Ctrl Pts',(-29.5211568440314,-0.85004648162128,
-1.37706209677242));
#62202=CARTESIAN_POINT('Ctrl Pts',(-29.4416132168144,0.698855012312891,
-1.45961663153347));
#62203=CARTESIAN_POINT('Ctrl Pts',(-29.3620695895973,1.60573257211715,-0.201250953105849));
#62204=CARTESIAN_POINT('Ctrl Pts',(-29.2825259623803,1.0374561658658,1.24199989661473));
#62205=CARTESIAN_POINT('Ctrl Pts',(-29.2029823351632,-0.483910190892033,
1.54425061645926));
#62206=CARTESIAN_POINT('Ctrl Pts',(-29.1234387079461,-1.56071806406133,
0.427829596681443));
#62207=CARTESIAN_POINT('Ctrl Pts',(-29.0438950807291,-1.20372588728886,
-1.08162980152852));
#62208=CARTESIAN_POINT('Ctrl Pts',(-28.964351453512,0.259104862800183,-1.59741782554135));
#62209=CARTESIAN_POINT('Ctrl Pts',(-28.884807826295,1.48390122744979,-0.645690472639149));
#62210=CARTESIAN_POINT('Ctrl Pts',(-28.8052641990779,1.34546761288737,0.899219629431616));
#62211=CARTESIAN_POINT('Ctrl Pts',(-28.7257205718609,-0.0290198252163337,
1.61803488498499));
#62212=CARTESIAN_POINT('Ctrl Pts',(-28.6461769446438,-1.37684733812111,
0.850394289017024));
#62213=CARTESIAN_POINT('Ctrl Pts',(-28.5666333174267,-1.4597931099745,-0.698486302911472));
#62214=CARTESIAN_POINT('Ctrl Pts',(-28.4870896902097,-0.201656541472631,
-1.60568168656345));
#62215=CARTESIAN_POINT('Ctrl Pts',(-28.4075460629926,1.24173780413355,-1.03776985168656));
#62216=CARTESIAN_POINT('Ctrl Pts',(-28.3280024357755,1.54437279891356,0.48352011050198));
#62217=CARTESIAN_POINT('Ctrl Pts',(-28.2484588085585,0.428223807527087,
1.56060994804947));
#62218=CARTESIAN_POINT('Ctrl Pts',(-28.1689151813414,-1.08132571580484,
1.20399905964379));
#62219=CARTESIAN_POINT('Ctrl Pts',(-28.0893715541244,-1.59748322233021,
-0.258701359983772));
#62220=CARTESIAN_POINT('Ctrl Pts',(-28.0098279269073,-0.646065273236205,
-1.4837380840304));
#62221=CARTESIAN_POINT('Ctrl Pts',(-27.9302842996902,0.898879746737731,
-1.34569470541749));
#62222=CARTESIAN_POINT('Ctrl Pts',(-27.8507406724732,1.61804216353577,0.0286111220409825));
#62223=CARTESIAN_POINT('Ctrl Pts',(-27.7711970452561,0.850742042155411,
1.37663249162338));
#62224=CARTESIAN_POINT('Ctrl Pts',(-27.6916534180391,-0.698117548944819,
1.45996949527695));
#62225=CARTESIAN_POINT('Ctrl Pts',(-27.612109790822,-1.60563069856312,0.202062116973198));
#62226=CARTESIAN_POINT('Ctrl Pts',(-27.532566163605,-1.03808347129492,-1.24147563242629));
#62227=CARTESIAN_POINT('Ctrl Pts',(-27.4530225363878,0.483129999262114,
-1.54449488283288));
#62228=CARTESIAN_POINT('Ctrl Pts',(-27.3734789091709,1.56050173246666,-0.42861799105092));
#62229=CARTESIAN_POINT('Ctrl Pts',(-27.2939352819538,1.20427215518044,1.08102156108979));
#62230=CARTESIAN_POINT('Ctrl Pts',(-27.2143916547367,-0.258297840661568,
1.5975485171955));
#62231=CARTESIAN_POINT('Ctrl Pts',(-27.1348480275197,-1.48357484594468,
0.6464400326126));
#62232=CARTESIAN_POINT('Ctrl Pts',(-27.0553044003026,-1.3459217120888,-0.898539806693006));
#62233=CARTESIAN_POINT('Ctrl Pts',(-26.9757607730855,0.0282024170401897,
-1.61804933885128));
#62234=CARTESIAN_POINT('Ctrl Pts',(-26.8962171458685,1.37641755729295,-0.851089741014233));
#62235=CARTESIAN_POINT('Ctrl Pts',(-26.8166735186514,1.46014578742956,0.697748750436479));
#62236=CARTESIAN_POINT('Ctrl Pts',(-26.7371298914343,0.202467679581668,
1.60557960811938));
#62237=CARTESIAN_POINT('Ctrl Pts',(-26.6575862642173,-1.24121338150966,
1.03839702467087));
#62238=CARTESIAN_POINT('Ctrl Pts',(-26.5780426370002,-1.54461686820943,
-0.482739857197281));
#62239=CARTESIAN_POINT('Ctrl Pts',(-26.4984990097832,-0.429012147227839,
-1.56039341731979));
#62240=CARTESIAN_POINT('Ctrl Pts',(-26.4189553825661,1.08071733740276,-1.20454517388143));
#62241=CARTESIAN_POINT('Ctrl Pts',(-26.3394117553491,1.59761371013306,0.257894304859269));
#62242=CARTESIAN_POINT('Ctrl Pts',(-26.259868128132,0.646814750744472,1.48341151320304));
#62243=CARTESIAN_POINT('Ctrl Pts',(-26.1803245009149,-0.898199809319099,
1.34614863288684));
#62244=CARTESIAN_POINT('Ctrl Pts',(-26.1007808736979,-1.61805641093105,
-0.0277937102399868));
#62245=CARTESIAN_POINT('Ctrl Pts',(-26.0212372464808,-0.851437385571346,
-1.3762025351435));
#62246=CARTESIAN_POINT('Ctrl Pts',(-25.9416936192638,0.697379907409941,
-1.4603219864211));
#62247=CARTESIAN_POINT('Ctrl Pts',(-25.8621499920467,1.60552841523551,-0.202873229272194));
#62248=CARTESIAN_POINT('Ctrl Pts',(-25.7826063648297,1.0387105117944,1.24095105140041));
#62249=CARTESIAN_POINT('Ctrl Pts',(-25.7030627376125,-0.482349684332396,
1.54473875503543));
#62250=CARTESIAN_POINT('Ctrl Pts',(-25.6235191103955,-1.56028500261578,
0.429406276032671));
#62251=CARTESIAN_POINT('Ctrl Pts',(-25.5439754831784,-1.20481811572932,
-1.08041304476317));
#62252=CARTESIAN_POINT('Ctrl Pts',(-25.4644318559614,0.257490752602664,
-1.59767880113873));
#62253=CARTESIAN_POINT('Ctrl Pts',(-25.3848882287443,1.48324808581591,-0.647189427607864));
#62254=CARTESIAN_POINT('Ctrl Pts',(-25.3053446015273,1.34637546779709,0.897859754637735));
#62255=CARTESIAN_POINT('Ctrl Pts',(-25.2258009743102,-0.0273850016665038,
1.61806337977463));
#62256=CARTESIAN_POINT('Ctrl Pts',(-25.1462573470932,-1.37598742518878,
0.851784975804522));
#62257=CARTESIAN_POINT('Ctrl Pts',(-25.0667137198762,-1.4604980922403,-0.697011019888793));
#62258=CARTESIAN_POINT('Ctrl Pts',(-24.987170092659,-0.20327876601885,-1.60547711991477));
#62259=CARTESIAN_POINT('Ctrl Pts',(-24.907626465442,1.24068864211528,-1.03902393264549));
#62260=CARTESIAN_POINT('Ctrl Pts',(-24.828082838225,1.54486054330308,0.481959480692382));
#62261=CARTESIAN_POINT('Ctrl Pts',(-24.7485392110078,0.429800377440236,
1.56017648836156));
#62262=CARTESIAN_POINT('Ctrl Pts',(-24.6689955837908,-1.08010868319043,
1.20509098070668));
#62263=CARTESIAN_POINT('Ctrl Pts',(-24.5894519565737,-1.59774379020835,
-0.257087183917484));
#62264=CARTESIAN_POINT('Ctrl Pts',(-24.5099083293567,-0.64756406317891,
-1.48308456379371));
#62265=CARTESIAN_POINT('Ctrl Pts',(-24.4303647021396,0.89751964267059,-1.3466022168051));
#62266=CARTESIAN_POINT('Ctrl Pts',(-24.3508210749226,1.61807024538158,0.0269762913457571));
#62267=CARTESIAN_POINT('Ctrl Pts',(-24.2712774477055,0.852132511691634,
1.37577222744249));
#62268=CARTESIAN_POINT('Ctrl Pts',(-24.1917338204884,-0.6966420878965,1.46067410487595));
#62269=CARTESIAN_POINT('Ctrl Pts',(-24.1121901932714,-1.60542572216043,
0.20368428979582));
#62270=CARTESIAN_POINT('Ctrl Pts',(-24.0326465660543,-1.03933728720419,
-1.24042615367099));
#62271=CARTESIAN_POINT('Ctrl Pts',(-23.9531029388373,0.481569246302081,
-1.54498223300464));
#62272=CARTESIAN_POINT('Ctrl Pts',(-23.8735593116202,1.56006787456402,-0.430194451425465));
#62273=CARTESIAN_POINT('Ctrl Pts',(-23.7940156844032,1.20536376879613,1.07980425270396));
#62274=CARTESIAN_POINT('Ctrl Pts',(-23.7144720571861,-0.256683598829453,
1.59780867733779));
#62275=CARTESIAN_POINT('Ctrl Pts',(-23.6349284299691,-1.48292094714688,
0.647938657433694));
#62276=CARTESIAN_POINT('Ctrl Pts',(-23.555384802752,-1.34682887989642,-0.89717947343935));
#62277=CARTESIAN_POINT('Ctrl Pts',(-23.4758411755349,0.0265675793038584,
-1.61807700775145));
#62278=CARTESIAN_POINT('Ctrl Pts',(-23.3962975483179,1.37555694191836,-0.852479993210494));
#62279=CARTESIAN_POINT('Ctrl Pts',(-23.3167539211008,1.46085002431682,0.696273111456646));
#62280=CARTESIAN_POINT('Ctrl Pts',(-23.2372102938837,0.204089800577218,
1.60537422197577));
#62281=CARTESIAN_POINT('Ctrl Pts',(-23.1576666666667,-1.2401635860843,1.03965057545047));
#62282=CARTESIAN_POINT('Ctrl Pts',(-23.0781230394496,-1.54510382413234,
-0.481178981186404));
#62283=CARTESIAN_POINT('Ctrl Pts',(-22.9985794122325,-0.430588497963164,
-1.55995916123012));
#62284=CARTESIAN_POINT('Ctrl Pts',(-22.9190357850155,1.07949975332317,-1.20563647998025));
#62285=CARTESIAN_POINT('Ctrl Pts',(-22.8394921577984,1.59787346252289,0.256279997364353));
#62286=CARTESIAN_POINT('Ctrl Pts',(-22.7599485305814,0.648313210348325,
1.48275723588584));
#62287=CARTESIAN_POINT('Ctrl Pts',(-22.6804049033644,-0.896839246965747,
1.34705545705657));
#62288=CARTESIAN_POINT('Ctrl Pts',(-22.6008612761472,-1.61808366688383,
-0.0261588655668692));
#62289=CARTESIAN_POINT('Ctrl Pts',(-22.5213176489302,-0.852827420338917,
-1.37534156863015));
#62290=CARTESIAN_POINT('Ctrl Pts',(-22.4417740217131,0.695904090592774,
-1.46102585055167));
#62291=CARTESIAN_POINT('Ctrl Pts',(-22.3622303944961,1.60532261936409,-0.204495298337127));
#62292=CARTESIAN_POINT('Ctrl Pts',(-22.282686767279,1.03996379736434,1.23990093937197));
#62293=CARTESIAN_POINT('Ctrl Pts',(-22.203143140062,-0.48078868537029,1.5452253166784));
#62294=CARTESIAN_POINT('Ctrl Pts',(-22.1235995128449,-1.5598503483668,0.430982517028184));
#62295=CARTESIAN_POINT('Ctrl Pts',(-22.0440558856279,-1.20590911424163,
-1.07919518506752));
#62296=CARTESIAN_POINT('Ctrl Pts',(-21.9645122584108,0.255876379547943,
-1.59793814575953));
#62297=CARTESIAN_POINT('Ctrl Pts',(-21.8849686311937,1.48259343002106,-0.648687721898869));
#62298=CARTESIAN_POINT('Ctrl Pts',(-21.8054250039767,1.34728194827107,0.896498963271491));
#62299=CARTESIAN_POINT('Ctrl Pts',(-21.7258813767596,-0.0257501501609023,
1.61809022277828));
#62300=CARTESIAN_POINT('Ctrl Pts',(-21.6463377495426,-1.37512610759159,
0.853174793054725));
#62301=CARTESIAN_POINT('Ctrl Pts',(-21.5667941223255,-1.46120158356928,
-0.695535025328411));
#62302=CARTESIAN_POINT('Ctrl Pts',(-21.4872504951084,-0.204900783049728,
-1.60527091432866));
#62303=CARTESIAN_POINT('Ctrl Pts',(-21.4077068678914,1.23963821355074,-1.04027695292585));
#62304=CARTESIAN_POINT('Ctrl Pts',(-21.3281632406743,1.5453467106351,0.480398358878597));
#62305=CARTESIAN_POINT('Ctrl Pts',(-21.2486196134573,0.431376508595433,
1.55974143598097));
#62306=CARTESIAN_POINT('Ctrl Pts',(-21.1690759862402,-1.07889054795642,
1.2061816715629));
#62307=CARTESIAN_POINT('Ctrl Pts',(-21.0895323590231,-1.59800272704358,
-0.25547274540593));
#62308=CARTESIAN_POINT('Ctrl Pts',(-21.0099887318061,-0.649062192061473,
-1.48242952956298));
#62309=CARTESIAN_POINT('Ctrl Pts',(-20.930445104589,0.896158622378259,-1.34750835352552));
#62310=CARTESIAN_POINT('Ctrl Pts',(-20.850901477372,1.61809667543438,0.0253414331119925));
#62311=CARTESIAN_POINT('Ctrl Pts',(-20.7713578501549,0.853522111335798,
1.37491055881641));
#62312=CARTESIAN_POINT('Ctrl Pts',(-20.6918142229379,-0.695165915687114,
1.46137722335845));
#62313=CARTESIAN_POINT('Ctrl Pts',(-20.6122705957208,-1.60521910687279,
0.205306254689137));
#62314=CARTESIAN_POINT('Ctrl Pts',(-20.5327269685037,-1.040590042115,-1.23937540863738));
#62315=CARTESIAN_POINT('Ctrl Pts',(-20.4531833412867,0.480008001736251,
-1.54546800599468));
#62316=CARTESIAN_POINT('Ctrl Pts',(-20.3736397140696,1.55963242407961,-0.431770472639713));
#62317=CARTESIAN_POINT('Ctrl Pts',(-20.2940960868525,1.20645415192664,1.07858584200931));
#62318=CARTESIAN_POINT('Ctrl Pts',(-20.2145524596354,-0.255069094964123,
1.59806720637092));
#62319=CARTESIAN_POINT('Ctrl Pts',(-20.1350088324184,-1.48226553452206,
0.64943662081221));
#62320=CARTESIAN_POINT('Ctrl Pts',(-20.0554652052013,-1.34773467280543,
-0.895818224307807));
#62321=CARTESIAN_POINT('Ctrl Pts',(-19.9759215779843,0.024932714446255,
-1.61810302485173));
#62322=CARTESIAN_POINT('Ctrl Pts',(-19.8963779507672,1.37469492231839,-0.853869375159925));
#62323=CARTESIAN_POINT('Ctrl Pts',(-19.8168343235502,1.46155276990797,0.694796761692446));
#62324=CARTESIAN_POINT('Ctrl Pts',(-19.7372906963331,0.205711713229446,
1.60516719699979));
#62325=CARTESIAN_POINT('Ctrl Pts',(-19.6577470691161,-1.23911252464868,
1.04090306491178));
#62326=CARTESIAN_POINT('Ctrl Pts',(-19.578203441899,-1.54558920274938,-0.479617613968146));
#62327=CARTESIAN_POINT('Ctrl Pts',(-19.4986598146819,-0.432164409135939,
-1.55952331266966));
#62328=CARTESIAN_POINT('Ctrl Pts',(-19.4191161874649,1.07828106724562,-1.2067265553155));
#62329=CARTESIAN_POINT('Ctrl Pts',(-19.3395725602478,1.59813158373743,0.254665428248228));
#62330=CARTESIAN_POINT('Ctrl Pts',(-19.2600289330308,0.649811008127239,
1.48210144490876));
#62331=CARTESIAN_POINT('Ctrl Pts',(-19.1804853058137,-0.895477769081822,
1.34796090609639));
#62332=CARTESIAN_POINT('Ctrl Pts',(-19.1009416785966,-1.61810927102991,
-0.0245239941897118));
#62333=CARTESIAN_POINT('Ctrl Pts',(-19.0213980513796,-0.854216584504992,
-1.37447919811127));
#62334=CARTESIAN_POINT('Ctrl Pts',(-18.9418544241625,0.694427563367922,
-1.46172822320664));
#62335=CARTESIAN_POINT('Ctrl Pts',(-18.8623107969455,1.60511518471297,-0.206117158644834));
#62336=CARTESIAN_POINT('Ctrl Pts',(-18.7827671697284,1.04121602129628,1.23884956160137));
#62337=CARTESIAN_POINT('Ctrl Pts',(-18.7032235425113,-0.479227195599194,
1.5457103008915));
#62338=CARTESIAN_POINT('Ctrl Pts',(-18.6236799152943,-1.55941410175808,
0.432558318058966));
#62339=CARTESIAN_POINT('Ctrl Pts',(-18.5441362880772,-1.20699888171208,
-1.0779762236848));
#62340=CARTESIAN_POINT('Ctrl Pts',(-18.4645926608602,0.254261745284025,
-1.59819585913902));
#62341=CARTESIAN_POINT('Ctrl Pts',(-18.3850490336431,1.48193726073355,-0.650185353982615));
#62342=CARTESIAN_POINT('Ctrl Pts',(-18.3055054064261,1.34818705338395,0.895137256722049));
#62343=CARTESIAN_POINT('Ctrl Pts',(-18.225961779209,-0.0241152723685061,
1.61811541396853));
#62344=CARTESIAN_POINT('Ctrl Pts',(-18.1464181519919,-1.37426338620882,
0.854563739348813));
#62345=CARTESIAN_POINT('Ctrl Pts',(-18.0668745247748,-1.46190358324326,
-0.694058320737146));
#62346=CARTESIAN_POINT('Ctrl Pts',(-17.9873308975578,-0.206522590909396,
-1.60506307001564));
#62347=CARTESIAN_POINT('Ctrl Pts',(-17.9077872703407,1.23858651951227,-1.04152891124848));
#62348=CARTESIAN_POINT('Ctrl Pts',(-17.8282436431237,1.5458313004133,0.478836746654323));
#62349=CARTESIAN_POINT('Ctrl Pts',(-17.7487000159066,0.432952199383627,
1.55930479135185));
#62350=CARTESIAN_POINT('Ctrl Pts',(-17.6691563886895,-1.07767131134634,
1.20727113109899));
#62351=CARTESIAN_POINT('Ctrl Pts',(-17.5896127614725,-1.59826003257156,
-0.253858046097263));
#62352=CARTESIAN_POINT('Ctrl Pts',(-17.5100691342554,-0.6505596583545,-1.48177298200691));
#62353=CARTESIAN_POINT('Ctrl Pts',(-17.4305255070384,0.89479668725018,-1.34841311465369));
#62354=CARTESIAN_POINT('Ctrl Pts',(-17.3509818798213,1.6181214536672,0.0237065490086662));
#62355=CARTESIAN_POINT('Ctrl Pts',(-17.2714382526043,0.854910839669279,
1.3740474866248));
#62356=CARTESIAN_POINT('Ctrl Pts',(-17.1918946253872,-0.693689033823637,
1.46207885000666));
#62357=CARTESIAN_POINT('Ctrl Pts',(-17.1123509981702,-1.60501085291113,
0.20692800999731));
#62358=CARTESIAN_POINT('Ctrl Pts',(-17.0328073709531,-1.04184173474845,
-1.23832339839813));
#62359=CARTESIAN_POINT('Ctrl Pts',(-16.953263743736,0.4784462671584,-1.54595220130706));
#62360=CARTESIAN_POINT('Ctrl Pts',(-16.873720116519,1.55919538145794,-0.433346053084831));
#62361=CARTESIAN_POINT('Ctrl Pts',(-16.7941764893019,1.2075433034589,1.07736633024962));
#62362=CARTESIAN_POINT('Ctrl Pts',(-16.7146328620849,-0.253454330713697,
1.59832410403098));
#62363=CARTESIAN_POINT('Ctrl Pts',(-16.6350892348678,-1.4816086087393,0.650933921219002));
#62364=CARTESIAN_POINT('Ctrl Pts',(-16.5555456076507,-1.34863908989118,
-0.894456060687972));
#62365=CARTESIAN_POINT('Ctrl Pts',(-16.4760019804337,0.0232978241362747,
-1.61812739012554));
#62366=CARTESIAN_POINT('Ctrl Pts',(-16.3964583532166,1.373831499373,-0.855257885444212));
#62367=CARTESIAN_POINT('Ctrl Pts',(-16.3169147259995,1.46225402348564,0.693319702650978));
#62368=CARTESIAN_POINT('Ctrl Pts',(-16.2373710987825,0.207333415882653,
1.60495853340278));
#62369=CARTESIAN_POINT('Ctrl Pts',(-16.1578274715654,-1.23806019827577,
1.04215449177621));
#62370=CARTESIAN_POINT('Ctrl Pts',(-16.0782838443484,-1.54607300356507,
-0.478055757136395));
#62371=CARTESIAN_POINT('Ctrl Pts',(-15.9987402171313,-0.43373987913742,
-1.55908587208332));
#62372=CARTESIAN_POINT('Ctrl Pts',(-15.9191965899143,1.07706128041417,-1.20781539877439));
#62373=CARTESIAN_POINT('Ctrl Pts',(-15.8396529626972,1.59838807351318,0.253050599159107));
#62374=CARTESIAN_POINT('Ctrl Pts',(-15.7601093354801,0.65130814255221,1.48144414094125));
#62375=CARTESIAN_POINT('Ctrl Pts',(-15.6805657082631,-0.894115377057167,
1.348864979082));
#62376=CARTESIAN_POINT('Ctrl Pts',(-15.601022081046,-1.61813322334315,-0.0228890977774511));
#62377=CARTESIAN_POINT('Ctrl Pts',(-15.521478453829,-0.85560487665146,-1.3736154244672));
#62378=CARTESIAN_POINT('Ctrl Pts',(-15.4419348266119,0.692950327242719,
-1.46242910366902));
#62379=CARTESIAN_POINT('Ctrl Pts',(-15.3623911993948,1.60490611149391,-0.207738808539605));
#62380=CARTESIAN_POINT('Ctrl Pts',(-15.2828475721778,1.04246718231184,1.23779691916194));
#62381=CARTESIAN_POINT('Ctrl Pts',(-15.2033039449607,-0.477665216613179,
1.54619370717962));
#62382=CARTESIAN_POINT('Ctrl Pts',(-15.1237603177437,-1.55897626323499,
0.434133677516307));
#62383=CARTESIAN_POINT('Ctrl Pts',(-15.0442166905266,-1.20808741702816,
-1.07675616185941));
#62384=CARTESIAN_POINT('Ctrl Pts',(-14.9646730633095,0.252646851459204,
-1.59845194101409));
#62385=CARTESIAN_POINT('Ctrl Pts',(-14.8851294360925,1.48127957862323,-0.65168232233028));
#62386=CARTESIAN_POINT('Ctrl Pts',(-14.8055858088754,1.34909078221174,0.893774636379497));
#62387=CARTESIAN_POINT('Ctrl Pts',(-14.7260421816584,-0.0224803699582582,
1.61813895331967));
#62388=CARTESIAN_POINT('Ctrl Pts',(-14.6464985544413,-1.37339926192116,
0.855951813268913));
#62389=CARTESIAN_POINT('Ctrl Pts',(-14.5669549272242,-1.46260409054564,
-0.692580907622451));
#62390=CARTESIAN_POINT('Ctrl Pts',(-14.4874113000072,-0.208144187942263,
-1.60485358718789));
#62391=CARTESIAN_POINT('Ctrl Pts',(-14.4078676727901,1.23753356107348,-1.04277980633532));
#62392=CARTESIAN_POINT('Ctrl Pts',(-14.3283240455731,1.546314312143,0.477274645613715));
#62393=CARTESIAN_POINT('Ctrl Pts',(-14.248780418356,0.434527448196287,1.55886655491996));
#62394=CARTESIAN_POINT('Ctrl Pts',(-14.1692367911389,-1.07645097460485,
1.20835935820277));
#62395=CARTESIAN_POINT('Ctrl Pts',(-14.0896931639219,-1.59851570652962,
-0.252243087639847));
#62396=CARTESIAN_POINT('Ctrl Pts',(-14.0101495367048,-0.652056460529289,
-1.48111492179574));
#62397=CARTESIAN_POINT('Ctrl Pts',(-13.9306059094878,0.893433838676696,
-1.34931649926596));
#62398=CARTESIAN_POINT('Ctrl Pts',(-13.8510622822707,1.61814458005474,0.0220716407047407));
#62399=CARTESIAN_POINT('Ctrl Pts',(-13.7715186550536,0.8562986952744,1.37318301174874));
#62400=CARTESIAN_POINT('Ctrl Pts',(-13.6919750278366,-0.692211443813764,
1.46277898410431));
#62401=CARTESIAN_POINT('Ctrl Pts',(-13.6124314006195,-1.60480096048804,
0.208549554064757));
#62402=CARTESIAN_POINT('Ctrl Pts',(-13.5328877734025,-1.04309236382677,
-1.23727012402718));
#62403=CARTESIAN_POINT('Ctrl Pts',(-13.4533441461854,0.47688404416288,-1.54643481844753));
#62404=CARTESIAN_POINT('Ctrl Pts',(-13.3738005189684,1.55875674714518,-0.434921191152319));
#62405=CARTESIAN_POINT('Ctrl Pts',(-13.2942568917513,1.20863122228096,1.07614571866991));
#62406=CARTESIAN_POINT('Ctrl Pts',(-13.2147132645342,-0.251839307726659,
1.59857937005571));
#62407=CARTESIAN_POINT('Ctrl Pts',(-13.1351696373171,-1.48095017046926,
0.652430557125475));
#62408=CARTESIAN_POINT('Ctrl Pts',(-13.0556260101001,-1.34954213023036,
-0.893092983970473));
#62409=CARTESIAN_POINT('Ctrl Pts',(-12.976082382883,0.0216629100430018,
-1.618150103548));
#62410=CARTESIAN_POINT('Ctrl Pts',(-12.896538755666,1.37296667396363,-0.856645522645844));
#62411=CARTESIAN_POINT('Ctrl Pts',(-12.8169951284489,1.46295378433393,0.691841935840126));
#62412=CARTESIAN_POINT('Ctrl Pts',(-12.7374515012319,0.208954906881307,
1.60474823139775));
#62413=CARTESIAN_POINT('Ctrl Pts',(-12.6579078740148,-1.23700660803984,
1.04340485476622));
#62414=CARTESIAN_POINT('Ctrl Pts',(-12.5783642467977,-1.5465552260855,-0.476493412285577));
#62415=CARTESIAN_POINT('Ctrl Pts',(-12.4988206195807,-0.43531490635929,
-1.55864683991769));
#62416=CARTESIAN_POINT('Ctrl Pts',(-12.4192769923636,1.07584039407407,-1.20890300924538));
#62417=CARTESIAN_POINT('Ctrl Pts',(-12.3397333651465,1.59864293158829,0.251435511745501));
#62418=CARTESIAN_POINT('Ctrl Pts',(-12.2601897379295,0.652804612094871,
1.48078532465434));
#62419=CARTESIAN_POINT('Ctrl Pts',(-12.1806461107124,-0.892752072282623,
1.34976767509045));
#62420=CARTESIAN_POINT('Ctrl Pts',(-12.1011024834954,-1.61815552379909,
-0.0212541779991121));
#62421=CARTESIAN_POINT('Ctrl Pts',(-12.0215588562783,-0.856992295361072,
-1.37275024857972));
#62422=CARTESIAN_POINT('Ctrl Pts',(-11.9420152290613,0.691472383725218,
-1.4631284912233));
#62423=CARTESIAN_POINT('Ctrl Pts',(-11.8624716018442,1.60469539992036,-0.209360246365963));
#62424=CARTESIAN_POINT('Ctrl Pts',(-11.7829279746271,1.04371727913374,1.23674301312827));
#62425=CARTESIAN_POINT('Ctrl Pts',(-11.7033843474101,-0.476102750006793,
1.54667553504926));
#62426=CARTESIAN_POINT('Ctrl Pts',(-11.623840720193,-1.55853683324449,0.435708593792007));
#62427=CARTESIAN_POINT('Ctrl Pts',(-11.544297092976,-1.20917471907862,-1.07553500083685));
#62428=CARTESIAN_POINT('Ctrl Pts',(-11.4647534657589,0.251031699722106,
-1.59870639112332));
#62429=CARTESIAN_POINT('Ctrl Pts',(-11.3852098385419,1.48062038436146,-0.65317862541366));
#62430=CARTESIAN_POINT('Ctrl Pts',(-11.3056662113248,1.34999313383188,0.892411103634845));
#62431=CARTESIAN_POINT('Ctrl Pts',(-11.2261225841077,-0.0208454445991207,
1.61816084080769));
#62432=CARTESIAN_POINT('Ctrl Pts',(-11.1465789568907,-1.3725337356108,0.85733901339797));
#62433=CARTESIAN_POINT('Ctrl Pts',(-11.0670353296736,-1.46330310476127,
-0.691102787492547));
#62434=CARTESIAN_POINT('Ctrl Pts',(-10.9874917024566,-0.209765572492934,
-1.60464246605925));
#62435=CARTESIAN_POINT('Ctrl Pts',(-10.9079480752395,1.23647933930929,-1.04402963690943));
#62436=CARTESIAN_POINT('Ctrl Pts',(-10.8284044480224,1.54679574533111,0.475712057351421));
#62437=CARTESIAN_POINT('Ctrl Pts',(-10.7488608208054,0.43610225342541,1.5584267271326));
#62438=CARTESIAN_POINT('Ctrl Pts',(-10.6693171935883,-1.07522953897768,
1.20944635176342));
#62439=CARTESIAN_POINT('Ctrl Pts',(-10.5897735663712,-1.59876974865677,
-0.250627871682214));
#62440=CARTESIAN_POINT('Ctrl Pts',(-10.5102299391542,-0.65355259705794,
-1.48045534960118));
#62441=CARTESIAN_POINT('Ctrl Pts',(-10.4306863119371,0.892070078048929,
-1.35021850644024));
#62442=CARTESIAN_POINT('Ctrl Pts',(-10.3511426847201,1.61816605457342,0.0204367098691262));
#62443=CARTESIAN_POINT('Ctrl Pts',(-10.271599057503,0.857685676734452,1.37231713507066));
#62444=CARTESIAN_POINT('Ctrl Pts',(-10.1920554302859,-0.690733147165762,
1.46347762493672));
#62445=CARTESIAN_POINT('Ctrl Pts',(-10.1125118030689,-1.60458942981779,
0.210170885236279));
#62446=CARTESIAN_POINT('Ctrl Pts',(-10.0329681758518,-1.0443419280733,-1.23621558659974));
#62447=CARTESIAN_POINT('Ctrl Pts',(-9.95342454863478,0.475321334344385,
-1.54691585692338));
#62448=CARTESIAN_POINT('Ctrl Pts',(-9.87388092141771,1.55831652158906,-0.436495885234337));
#62449=CARTESIAN_POINT('Ctrl Pts',(-9.79433729420066,1.20971790728238,1.07492400851611));
#62450=CARTESIAN_POINT('Ctrl Pts',(-9.7147936669836,-0.250224027651638,
1.59883300418455));
#62451=CARTESIAN_POINT('Ctrl Pts',(-9.63525003976653,-1.48029022038403,
0.653926527003873));
#62452=CARTESIAN_POINT('Ctrl Pts',(-9.55570641254947,-1.35044379290116,
-0.891728995546662));
#62453=CARTESIAN_POINT('Ctrl Pts',(-9.47616278533242,0.020027973835256,
-1.61817116509597));
#62454=CARTESIAN_POINT('Ctrl Pts',(-9.39661915811536,1.37210044697314,-0.858032285348334));
#62455=CARTESIAN_POINT('Ctrl Pts',(-9.3170755308983,1.46365205173851,0.690363462768413));
#62456=CARTESIAN_POINT('Ctrl Pts',(-9.23753190368124,0.210576184570202,
1.60453629119936));
#62457=CARTESIAN_POINT('Ctrl Pts',(-9.15798827646418,-1.23595175501641,
1.04465415260547));
#62458=CARTESIAN_POINT('Ctrl Pts',(-9.07844464924712,-1.54703586981845,
-0.474930581010598));
#62459=CARTESIAN_POINT('Ctrl Pts',(-8.99890102203006,-0.436889489193695,
-1.5582062166209));
#62460=CARTESIAN_POINT('Ctrl Pts',(-8.919357394813,1.07461840947157,-1.20998938561821));
#62461=CARTESIAN_POINT('Ctrl Pts',(-8.83981376759594,1.59889615770264,0.249820167656086));
#62462=CARTESIAN_POINT('Ctrl Pts',(-8.76027014037887,0.654300415227634,
1.48012499672052));
#62463=CARTESIAN_POINT('Ctrl Pts',(-8.68072651316183,-0.891387856149781,
1.35066899320027));
#62464=CARTESIAN_POINT('Ctrl Pts',(-8.60118288594476,-1.61817617237499,
-0.0196192365235215));
#62465=CARTESIAN_POINT('Ctrl Pts',(-8.5216392587277,-0.858378839217572,
-1.37188367133204));
#62466=CARTESIAN_POINT('Ctrl Pts',(-8.44209563151065,0.689993734324072,
-1.46382638515553));
#62467=CARTESIAN_POINT('Ctrl Pts',(-8.36255200429358,1.60448305020737,-0.210981470468792));
#62468=CARTESIAN_POINT('Ctrl Pts',(-8.28300837707653,1.04496631048598,1.23568784457617));
#62469=CARTESIAN_POINT('Ctrl Pts',(-8.20346474985946,-0.47453979737503,
1.5471557840086));
#62470=CARTESIAN_POINT('Ctrl Pts',(-8.12392112264241,-1.55809581223514,
0.437283065278374));
#62471=CARTESIAN_POINT('Ctrl Pts',(-8.04437749542533,-1.21026078675358,
-1.07431274186363));
#62472=CARTESIAN_POINT('Ctrl Pts',(-7.96483386820829,0.249416291721394,
-1.59895920920702));
#62473=CARTESIAN_POINT('Ctrl Pts',(-7.88529024099122,1.47995967862121,-0.654674261705304));
#62474=CARTESIAN_POINT('Ctrl Pts',(-7.80574661377416,1.3508941073232,0.891046659880044));
#62475=CARTESIAN_POINT('Ctrl Pts',(-7.72620298655711,-0.0192104979600539,
1.6181810764102));
#62476=CARTESIAN_POINT('Ctrl Pts',(-7.64665935934005,-1.37166680816123,
0.858725338319981));
#62477=CARTESIAN_POINT('Ctrl Pts',(-7.56711573212298,-1.46400062517662,
-0.689623961856359));
#62478=CARTESIAN_POINT('Ctrl Pts',(-7.48757210490593,-0.211386742906221,
-1.60442970684522));
#62479=CARTESIAN_POINT('Ctrl Pts',(-7.40802847768886,1.23542385529583,-1.04527840169494));
#62480=CARTESIAN_POINT('Ctrl Pts',(-7.32848485047181,1.54727559948621,0.47414898346256));
#62481=CARTESIAN_POINT('Ctrl Pts',(-7.24894122325474,0.437676613463291,
1.55798530843885));
#62482=CARTESIAN_POINT('Ctrl Pts',(-7.16939759603769,-1.07400700571175,
1.21053211067118));
#62483=CARTESIAN_POINT('Ctrl Pts',(-7.08985396882063,-1.59902215869365,
-0.24901239987327));
#62484=CARTESIAN_POINT('Ctrl Pts',(-7.01031034160357,-0.655048066413094,
-1.47979426609663));
#62485=CARTESIAN_POINT('Ctrl Pts',(-6.93076671438651,0.89070540675921,-1.35111913525562));
#62486=CARTESIAN_POINT('Ctrl Pts',(-6.85122308716945,1.61818587720126,0.0188017581709107));
#62487=CARTESIAN_POINT('Ctrl Pts',(-6.77167945995239,0.859071782633506,
1.3714498574745));
#62488=CARTESIAN_POINT('Ctrl Pts',(-6.69213583273532,-0.689254145388818,
1.46417477179069));
#62489=CARTESIAN_POINT('Ctrl Pts',(-6.61259220551828,-1.60437626111631,
0.211792001856658));
#62490=CARTESIAN_POINT('Ctrl Pts',(-6.5330485783012,-1.04559042621242,-1.23515978719228));
#62491=CARTESIAN_POINT('Ctrl Pts',(-6.45350495108415,0.473758139298161,
-1.54739531624361));
#62492=CARTESIAN_POINT('Ctrl Pts',(-6.37396132386709,1.55787470523904,-0.438070133723317));
#62493=CARTESIAN_POINT('Ctrl Pts',(-6.29441769665004,1.21080335735372,1.07370120103544));
#62494=CARTESIAN_POINT('Ctrl Pts',(-6.21487406943297,-0.24860849213754,
1.59908500615853));
#62495=CARTESIAN_POINT('Ctrl Pts',(-6.13533044221592,-1.47962875915735,
0.655421829327089));
#62496=CARTESIAN_POINT('Ctrl Pts',(-6.05578681499884,-1.35134407698311,
-0.89036409680908));
#62497=CARTESIAN_POINT('Ctrl Pts',(-5.9762431877818,0.0183930171821651,
-1.61819057474788));
#62498=CARTESIAN_POINT('Ctrl Pts',(-5.89669956056472,1.37123281928574,-0.859418172136015));
#62499=CARTESIAN_POINT('Ctrl Pts',(-5.81715593334767,1.4643488249866,0.688884284945115));
#62500=CARTESIAN_POINT('Ctrl Pts',(-5.73761230613061,0.212197247294186,
1.60432271302402));
#62501=CARTESIAN_POINT('Ctrl Pts',(-5.65806867891356,-1.23489564028233,
1.04590238401853));
#62502=CARTESIAN_POINT('Ctrl Pts',(-5.57852505169649,-1.5475149342732,-0.4733672649068));
#62503=CARTESIAN_POINT('Ctrl Pts',(-5.49898142447944,-0.438463626033293,
-1.5577640026428));
#62504=CARTESIAN_POINT('Ctrl Pts',(-5.41943779726238,1.07339532785422,-1.21107452678385));
#62505=CARTESIAN_POINT('Ctrl Pts',(-5.3398941700453,1.59914775159766,0.248204568539948));
#62506=CARTESIAN_POINT('Ctrl Pts',(-5.26035054282826,0.655795550423491,
1.4794631578139));
#62507=CARTESIAN_POINT('Ctrl Pts',(-5.18080691561119,-0.890022730051382,
1.35156893249138));
#62508=CARTESIAN_POINT('Ctrl Pts',(-5.10126328839414,-1.61819516904976,
-0.0179842750198703));
#62509=CARTESIAN_POINT('Ctrl Pts',(-5.02171966117707,-0.859764506805417,
-1.37101569360878));
#62510=CARTESIAN_POINT('Ctrl Pts',(-4.94217603396002,0.688514380548778,
-1.46452278475327));
#62511=CARTESIAN_POINT('Ctrl Pts',(-4.86263240674296,1.60426906257179,-0.212602479193019));
#62512=CARTESIAN_POINT('Ctrl Pts',(-4.7830887795259,1.04621427509339,1.23463141458283));
#62513=CARTESIAN_POINT('Ctrl Pts',(-4.70354515230884,-0.472976360313382,
1.54763445356733));
#62514=CARTESIAN_POINT('Ctrl Pts',(-4.62400152509178,-1.55765320065716,
0.438857090368179));
#62515=CARTESIAN_POINT('Ctrl Pts',(-4.54445789787472,-1.21134561894431,
-1.07308938618757));
#62516=CARTESIAN_POINT('Ctrl Pts',(-4.46491427065766,0.247800629106233,
-1.59921039500703));
#62517=CARTESIAN_POINT('Ctrl Pts',(-4.3853706434406,1.4792974620769,-0.656169229678419));
#62518=CARTESIAN_POINT('Ctrl Pts',(-4.30582701622354,1.35179370176602,0.88968130650793));
#62519=CARTESIAN_POINT('Ctrl Pts',(-4.22628338900648,-0.0175755317101194,
1.61819966010659));
#62520=CARTESIAN_POINT('Ctrl Pts',(-4.14673976178942,-1.37079848045747,
0.860110786619649));
#62521=CARTESIAN_POINT('Ctrl Pts',(-4.06719613457236,-1.46469665107959,
-0.688144432223473));
#62522=CARTESIAN_POINT('Ctrl Pts',(-3.9876525073553,-0.213007697527226,
-1.60421530976304));
#62523=CARTESIAN_POINT('Ctrl Pts',(-3.90810888013824,1.23436711011067,-1.04652609941703));
#62524=CARTESIAN_POINT('Ctrl Pts',(-3.82856525292118,1.54775387411837,0.472585425542845));
#62525=CARTESIAN_POINT('Ctrl Pts',(-3.74902162570412,0.439250526702823,
1.55754229928924));
#62526=CARTESIAN_POINT('Ctrl Pts',(-3.66947799848706,-1.07278337605506,
1.21161663381776));
#62527=CARTESIAN_POINT('Ctrl Pts',(-3.58993437127001,-1.59927293638262,
-0.247396673862219));
#62528=CARTESIAN_POINT('Ctrl Pts',(-3.51039074405294,-0.656542867068056,
-1.4791316719569));
#62529=CARTESIAN_POINT('Ctrl Pts',(-3.43084711683588,0.889339826200543,
-1.35201838479272));
#62530=CARTESIAN_POINT('Ctrl Pts',(-3.35130348961882,1.61820404791809,0.017166787279032));
#62531=CARTESIAN_POINT('Ctrl Pts',(-3.27175986240176,0.860457011556571,
1.37058117984569));
#62532=CARTESIAN_POINT('Ctrl Pts',(-3.1922162351847,-0.687774439992805,
1.46487042395443));
#62533=CARTESIAN_POINT('Ctrl Pts',(-3.11267260796765,-1.60416145460112,
0.213412902271105));
#62534=CARTESIAN_POINT('Ctrl Pts',(-3.03312898075058,-1.04683785696976,
-1.23410272688283));
#62535=CARTESIAN_POINT('Ctrl Pts',(-2.95358535353353,0.472194460620347,
-1.54787319591841));
#62536=CARTESIAN_POINT('Ctrl Pts',(-2.87404172631646,1.55743129854565,-0.439643935012751));
#62537=CARTESIAN_POINT('Ctrl Pts',(-2.79449809909941,1.21188757138778,1.07247729747732));
#62538=CARTESIAN_POINT('Ctrl Pts',(-2.71495447188235,-0.246992702835222,
1.59933537571829));
#62539=CARTESIAN_POINT('Ctrl Pts',(-2.63541084466529,-1.47896578746142,
0.656916462572719));
#62540=CARTESIAN_POINT('Ctrl Pts',(-2.55586721744822,-1.35224298156292,
-0.888998289158813));
#62541=CARTESIAN_POINT('Ctrl Pts',(-2.47632359023117,0.0167580417635838,
-1.61820833246908));
#62542=CARTESIAN_POINT('Ctrl Pts',(-2.39677996301411,1.37036379176648,-0.860803181622379));
#62543=CARTESIAN_POINT('Ctrl Pts',(-2.31723633579705,1.46504410340623,0.687404403933919));
#62544=CARTESIAN_POINT('Ctrl Pts',(-2.23769270857999,0.21381809332376,1.60410749698785));
#62545=CARTESIAN_POINT('Ctrl Pts',(-2.15814908136293,-1.2338382647739,1.04714954792454));
#62546=CARTESIAN_POINT('Ctrl Pts',(-2.07860545414587,-1.54799241922993,
-0.471803465937055));
#62547=CARTESIAN_POINT('Ctrl Pts',(-1.99906182692881,-0.440037314760149,
-1.55732019773846));
#62548=CARTESIAN_POINT('Ctrl Pts',(-1.91951819971175,1.07217114950081,-1.21215843295618));
#62549=CARTESIAN_POINT('Ctrl Pts',(-1.83997457249469,1.59939771485701,0.246588718554731));
#62550=CARTESIAN_POINT('Ctrl Pts',(-1.76043094527763,0.657290012662976,
1.47879980384918));
#62551=CARTESIAN_POINT('Ctrl Pts',(-1.68088731806057,-0.888656688751067,
1.35246750108129));
#62552=CARTESIAN_POINT('Ctrl Pts',(-1.60134369084351,-1.61821252638751,
-0.016349312307876));
#62553=CARTESIAN_POINT('Ctrl Pts',(-1.52180006362645,-0.861149272826775,
-1.37014628374404));
#62554=CARTESIAN_POINT('Ctrl Pts',(-1.44225643640939,0.687034278579223,
-1.46521775108889));
#62555=CARTESIAN_POINT('Ctrl Pts',(-1.36271280919233,1.60405352326847,-0.214223153619904));
#62556=CARTESIAN_POINT('Ctrl Pts',(-1.28316918197528,1.04746100838583,1.23357350166125));
#62557=CARTESIAN_POINT('Ctrl Pts',(-1.20362555475821,-0.47141213048378,
1.54811196566333));
#62558=CARTESIAN_POINT('Ctrl Pts',(-1.12408192754115,-1.55720958721362,
0.440429865694213));
#62559=CARTESIAN_POINT('Ctrl Pts',(-1.04453830032409,-1.21242809804978,
-1.07186341332639));
#62560=CARTESIAN_POINT('Ctrl Pts',(-0.964994673107033,0.246182594434854,
-1.59946283649398));
#62561=CARTESIAN_POINT('Ctrl Pts',(-0.885451045889976,1.47863775741399,
-0.657658045986899));
#62562=CARTESIAN_POINT('Ctrl Pts',(-0.805907418672914,1.352684282513,0.888304640480979));
#62563=CARTESIAN_POINT('Ctrl Pts',(-0.726363791455857,-0.0159260587564186,
1.61823633939855));
#62564=CARTESIAN_POINT('Ctrl Pts',(-0.646820164238798,-1.36995625320173,
0.861457876012838));
#62565=CARTESIAN_POINT('Ctrl Pts',(-0.567276537021739,-1.46533898470946,
-0.686593059182217));
#62566=CARTESIAN_POINT('Ctrl Pts',(-0.487732909804673,-0.214727527229581,
-1.60413432240554));
#62567=CARTESIAN_POINT('Ctrl Pts',(-0.408189282587616,1.23349737730688,
-1.04751621777734));
#62568=CARTESIAN_POINT('Ctrl Pts',(-0.328645655370557,1.54787157060309,
0.470532899021241));
#62569=CARTESIAN_POINT('Ctrl Pts',(-0.249102028153498,0.441519398461233,
1.55803864581879));
#62570=CARTESIAN_POINT('Ctrl Pts',(-0.169558400936438,-1.07299616020733,
1.21079737759236));
#62571=CARTESIAN_POINT('Ctrl Pts',(-0.116529316125065,-1.42161642106954,
0.242796052776739));
#62572=CARTESIAN_POINT('Ctrl Pts',(-0.0900147737193787,-1.35237762530129,
-0.207804766751035));
#62573=CARTESIAN_POINT('Ctrl Pts',(-34.6365,-0.63400709457496,1.31904027763697));
#62574=CARTESIAN_POINT('Ctrl Pts',(-34.6099854575943,-1.07350019101018,
1.10779446059807));
#62575=CARTESIAN_POINT('Ctrl Pts',(-34.5569563727829,-1.71702895747196,
0.215076187392512));
#62576=CARTESIAN_POINT('Ctrl Pts',(-34.4774127455659,-1.10807355631996,
-1.33132370591566));
#62577=CARTESIAN_POINT('Ctrl Pts',(-34.3978691183488,0.520314157757823,
-1.65035441174038));
#62578=CARTESIAN_POINT('Ctrl Pts',(-34.3183254911318,1.66994567305946,-0.45540337748486));
#62579=CARTESIAN_POINT('Ctrl Pts',(-34.2387818639147,1.28582705277904,1.1590459348403));
#62580=CARTESIAN_POINT('Ctrl Pts',(-34.1592382366976,-0.279762724963516,
1.70811017633449));
#62581=CARTESIAN_POINT('Ctrl Pts',(-34.0796946094806,-1.58823064801099,
0.688280517758478));
#62582=CARTESIAN_POINT('Ctrl Pts',(-34.0001509822635,-1.43768096220901,
-0.964023021038801));
#62583=CARTESIAN_POINT('Ctrl Pts',(-33.9206073550465,0.0336674791827454,
-1.73061147221349));
#62584=CARTESIAN_POINT('Ctrl Pts',(-33.8410637278294,1.47407027445902,-0.907367911586003));
#62585=CARTESIAN_POINT('Ctrl Pts',(-33.7615201006124,1.56028302586567,0.749480218709788));
#62586=CARTESIAN_POINT('Ctrl Pts',(-33.6819764733952,0.213090942288775,
1.71778338655393));
#62587=CARTESIAN_POINT('Ctrl Pts',(-33.6024328461783,-1.32986112826589,
1.10800045574547));
#62588=CARTESIAN_POINT('Ctrl Pts',(-33.5228892189612,-1.65109797050015,
-0.519683553947057));
#62589=CARTESIAN_POINT('Ctrl Pts',(-33.4433455917441,-0.455503924497776,
-1.66994296236554));
#62590=CARTESIAN_POINT('Ctrl Pts',(-33.3638019645271,1.15855200135494,-1.28606059765399));
#62591=CARTESIAN_POINT('Ctrl Pts',(-33.28425833731,1.70826986773391,0.27930008458429));
#62592=CARTESIAN_POINT('Ctrl Pts',(-33.2047147100929,0.688634737886851,
1.58807316929715));
#62593=CARTESIAN_POINT('Ctrl Pts',(-33.1251710828759,-0.963635117031397,
1.43791576625308));
#62594=CARTESIAN_POINT('Ctrl Pts',(-33.0456274556588,-1.73063294906621,
-0.0332257802001231));
#62595=CARTESIAN_POINT('Ctrl Pts',(-32.9660838284418,-0.907733356543969,
-1.47384343620158));
#62596=CARTESIAN_POINT('Ctrl Pts',(-32.8865402012247,0.749082463693335,
-1.56047102283841));
#62597=CARTESIAN_POINT('Ctrl Pts',(-32.8069965740076,1.71773141218131,-0.213525500287109));
#62598=CARTESIAN_POINT('Ctrl Pts',(-32.7274529467906,1.10833532841135,1.32958156544835));
#62599=CARTESIAN_POINT('Ctrl Pts',(-32.6479093195735,-0.519265954714281,
1.65122900047349));
#62600=CARTESIAN_POINT('Ctrl Pts',(-32.5683656923565,-1.66982813124843,
0.45592582130719));
#62601=CARTESIAN_POINT('Ctrl Pts',(-32.4888220651394,-1.28635305046249,
-1.15822716750039));
#62602=CARTESIAN_POINT('Ctrl Pts',(-32.4092784379224,0.27886850345117,-1.70834033505615));
#62603=CARTESIAN_POINT('Ctrl Pts',(-32.3297348107052,1.58789921594784,-0.689035864352048));
#62604=CARTESIAN_POINT('Ctrl Pts',(-32.2501911834882,1.43815910517878,0.963271888158851));
#62605=CARTESIAN_POINT('Ctrl Pts',(-32.1706475562711,-0.0327886242346749,
1.7306412824543));
#62606=CARTESIAN_POINT('Ctrl Pts',(-32.0911039290542,-1.47361410919611,
0.908105610353001));
#62607=CARTESIAN_POINT('Ctrl Pts',(-32.011560301837,-1.56066018196052,-0.748688278802587));
#62608=CARTESIAN_POINT('Ctrl Pts',(-31.93201667462,-0.213959379899255,-1.71767742202626));
#62609=CARTESIAN_POINT('Ctrl Pts',(-31.8524730474029,1.32930156755401,-1.1086711346824));
#62610=CARTESIAN_POINT('Ctrl Pts',(-31.7729294201859,1.65136010962961,0.518848851500797));
#62611=CARTESIAN_POINT('Ctrl Pts',(-31.6933857929688,0.456347591800452,
1.66971291479679));
#62612=CARTESIAN_POINT('Ctrl Pts',(-31.6138421657518,-1.15790220852164,
1.2866455680882));
#62613=CARTESIAN_POINT('Ctrl Pts',(-31.5342985385347,-1.70841072037166,
-0.27843698191794));
#62614=CARTESIAN_POINT('Ctrl Pts',(-31.4547549113176,-0.689436932634756,
-1.58772512051041));
#62615=CARTESIAN_POINT('Ctrl Pts',(-31.3752112841006,0.962908590334806,
-1.43840237383004));
#62616=CARTESIAN_POINT('Ctrl Pts',(-31.2956676568835,1.73064950937048,0.0323514774964916));
#62617=CARTESIAN_POINT('Ctrl Pts',(-31.2161240296665,0.908477804142727,
1.47338468220642));
#62618=CARTESIAN_POINT('Ctrl Pts',(-31.1365804024494,-0.748294045047776,
1.56084924465066));
#62619=CARTESIAN_POINT('Ctrl Pts',(-31.0570367752323,-1.71762332285629,
0.214393244204715));
#62620=CARTESIAN_POINT('Ctrl Pts',(-30.9774931480153,-1.10900686991318,
-1.32902148397453));
#62621=CARTESIAN_POINT('Ctrl Pts',(-30.8979495207982,0.518431715023144,
-1.65149111388425));
#62622=CARTESIAN_POINT('Ctrl Pts',(-30.8184058935812,1.66959759189759,-0.456769332935423));
#62623=CARTESIAN_POINT('Ctrl Pts',(-30.7388622663641,1.28693800357811,1.15757717553815));
#62624=CARTESIAN_POINT('Ctrl Pts',(-30.659318639147,-0.278005442596269,
1.70848099675336));
#62625=CARTESIAN_POINT('Ctrl Pts',(-30.57977501193,-1.58755092378435,0.689837956894189));
#62626=CARTESIAN_POINT('Ctrl Pts',(-30.5002313847129,-1.43864555070099,
-0.96254523105604));
#62627=CARTESIAN_POINT('Ctrl Pts',(-30.4206877574959,0.0319143286907724,
-1.73065762587657));
#62628=CARTESIAN_POINT('Ctrl Pts',(-30.3411441302788,1.47315516121278,-0.908849939964034));
#62629=CARTESIAN_POINT('Ctrl Pts',(-30.2616005030618,1.56103820775362,0.747899763547134));
#62630=CARTESIAN_POINT('Ctrl Pts',(-30.1820568758447,0.214827094831843,
1.71756911409893));
#62631=CARTESIAN_POINT('Ctrl Pts',(-30.1025132486276,-1.3287413156003,1.1093425343857));
#62632=CARTESIAN_POINT('Ctrl Pts',(-30.0229696214106,-1.65162201276936,
-0.5180145454678));
#62633=CARTESIAN_POINT('Ctrl Pts',(-29.9434259941935,-0.457191044927401,
-1.66948216247395));
#62634=CARTESIAN_POINT('Ctrl Pts',(-29.8638823669764,1.15725206869828,-1.28723035695793));
#62635=CARTESIAN_POINT('Ctrl Pts',(-29.7843387397594,1.70855116412952,0.277573885537073));
#62636=CARTESIAN_POINT('Ctrl Pts',(-29.7047951125423,0.690238937140185,
1.58737662576847));
#62637=CARTESIAN_POINT('Ctrl Pts',(-29.6252514853252,-0.962181810364402,
1.43888863578262));
#62638=CARTESIAN_POINT('Ctrl Pts',(-29.5457078581082,-1.73066563196221,
-0.0314771778488288));
#62639=CARTESIAN_POINT('Ctrl Pts',(-29.4661642308911,-0.909222017798363,
-1.47292554622804));
#62640=CARTESIAN_POINT('Ctrl Pts',(-29.3866206036741,0.747505434328563,
-1.5612270712583));
#62641=CARTESIAN_POINT('Ctrl Pts',(-29.307076976457,1.71751479575623,-0.215260931752423));
#62642=CARTESIAN_POINT('Ctrl Pts',(-29.2275333492399,1.10967812807928,1.32846106244894));
#62643=CARTESIAN_POINT('Ctrl Pts',(-29.1479897220229,-0.517597342861786,
1.65175280627669));
#62644=CARTESIAN_POINT('Ctrl Pts',(-29.0684460948058,-1.66936662653302,
0.457612727749417));
#62645=CARTESIAN_POINT('Ctrl Pts',(-28.9889024675888,-1.28752262820913,
-1.15692688802273));
#62646=CARTESIAN_POINT('Ctrl Pts',(-28.9093588403717,0.277142310767931,
-1.7086212224957));
#62647=CARTESIAN_POINT('Ctrl Pts',(-28.8298152131547,1.58720222647384,-0.69063987334716));
#62648=CARTESIAN_POINT('Ctrl Pts',(-28.7502715859376,1.43913162905944,0.961818328283063));
#62649=CARTESIAN_POINT('Ctrl Pts',(-28.6707279587206,-0.0310400249985448,
1.73067352762691));
#62650=CARTESIAN_POINT('Ctrl Pts',(-28.5911843315035,-1.47269583726682,
0.909594037621987));
#62651=CARTESIAN_POINT('Ctrl Pts',(-28.5116407042864,-1.56141583515265,
-0.747111057417198));
#62652=CARTESIAN_POINT('Ctrl Pts',(-28.4320970770693,-0.215694754938821,
-1.71746036783163));
#62653=CARTESIAN_POINT('Ctrl Pts',(-28.3525534498523,1.32818072453831,-1.11001365097253));
#62654=CARTESIAN_POINT('Ctrl Pts',(-28.2730098226352,1.65188349439792,0.517180107231717));
#62655=CARTESIAN_POINT('Ctrl Pts',(-28.1934661954182,0.45803438137456,1.66925098408218));
#62656=CARTESIAN_POINT('Ctrl Pts',(-28.1139225682011,-1.15660163353224,
1.28781481731305));
#62657=CARTESIAN_POINT('Ctrl Pts',(-28.0343789409841,-1.70869117184742,
-0.276710718316393));
#62658=CARTESIAN_POINT('Ctrl Pts',(-27.954835313767,-0.691040765489525,
-1.5870277259116));
#62659=CARTESIAN_POINT('Ctrl Pts',(-27.87529168655,0.961454784835226,-1.43937453051593));
#62660=CARTESIAN_POINT('Ctrl Pts',(-27.7957480593328,1.73068131287016,0.0306028701678309));
#62661=CARTESIAN_POINT('Ctrl Pts',(-27.7162044321159,0.909965999411154,
1.4724660343438));
#62662=CARTESIAN_POINT('Ctrl Pts',(-27.6366608048987,-0.746716632838211,
1.56160449942463));
#62663=CARTESIAN_POINT('Ctrl Pts',(-27.5571171776817,-1.71740583032862,
0.216128564363326));
#62664=CARTESIAN_POINT('Ctrl Pts',(-27.4775735504647,-1.11034910304403,
-1.32790030188634));
#62665=CARTESIAN_POINT('Ctrl Pts',(-27.3980299232476,0.516762838604242,
-1.6520140771247));
#62666=CARTESIAN_POINT('Ctrl Pts',(-27.3184862960305,1.66913523512881,-0.458456005775898));
#62667=CARTESIAN_POINT('Ctrl Pts',(-27.2389426688135,1.28810692425103,1.1562763052476));
#62668=CARTESIAN_POINT('Ctrl Pts',(-27.1593990415964,-0.276279108210019,
1.70876101218022));
#62669=CARTESIAN_POINT('Ctrl Pts',(-27.0798554143793,-1.58685312409289,
0.691441613541677));
#62670=CARTESIAN_POINT('Ctrl Pts',(-27.0003117871623,-1.43961734013658,
-0.961091180044105));
#62671=CARTESIAN_POINT('Ctrl Pts',(-26.9207681599452,0.0301657133845961,
-1.73068898769146));
#62672=CARTESIAN_POINT('Ctrl Pts',(-26.8412245327282,1.47223613747364,-0.910337903142115));
#62673=CARTESIAN_POINT('Ctrl Pts',(-26.7616809055111,1.56179306406219,0.746322160616793));
#62674=CARTESIAN_POINT('Ctrl Pts',(-26.6821372782941,0.216562359998259,
1.71735118325067));
#62675=CARTESIAN_POINT('Ctrl Pts',(-26.602593651077,-1.32761979451087,1.11068448427239));
#62676=CARTESIAN_POINT('Ctrl Pts',(-26.52305002386,-1.65214455444872,-0.516345537005934));
#62677=CARTESIAN_POINT('Ctrl Pts',(-26.4435063966428,-0.458877600926578,
-1.66901937968028));
#62678=CARTESIAN_POINT('Ctrl Pts',(-26.3639627694258,1.15595090318951,-1.28839894900448));
#62679=CARTESIAN_POINT('Ctrl Pts',(-26.2844191422087,1.70883074348965,0.275847480476298));
#62680=CARTESIAN_POINT('Ctrl Pts',(-26.2048755149917,0.691842417478086,
1.58667842102884));
#62681=CARTESIAN_POINT('Ctrl Pts',(-26.1253318877746,-0.960727513932856,
1.43986005790594));
#62682=CARTESIAN_POINT('Ctrl Pts',(-26.0457882605576,-1.73069655209032,
-0.0297285546766869));
#62683=CARTESIAN_POINT('Ctrl Pts',(-25.9662446333405,-0.910709748791179,
-1.472006146671));
#62684=CARTESIAN_POINT('Ctrl Pts',(-25.8867010061235,0.745927640778065,
-1.56198152905332));
#62685=CARTESIAN_POINT('Ctrl Pts',(-25.8071573789064,1.71729642660127,-0.21699614181597));
#62686=CARTESIAN_POINT('Ctrl Pts',(-25.7276137516893,1.1110197946362,1.32733920242982));
#62687=CARTESIAN_POINT('Ctrl Pts',(-25.6480701244723,-0.515928202463446,
1.65227492636163));
#62688=CARTESIAN_POINT('Ctrl Pts',(-25.5685264972552,-1.668903417744,0.459299166799682));
#62689=CARTESIAN_POINT('Ctrl Pts',(-25.4889828700381,-1.28869089155473,
-1.15562542737878));
#62690=CARTESIAN_POINT('Ctrl Pts',(-25.4094392428211,0.275415835142812,
-1.70890036577125));
#62691=CARTESIAN_POINT('Ctrl Pts',(-25.329895615604,1.5865036167306,-0.692243177273134));
#62692=CARTESIAN_POINT('Ctrl Pts',(-25.250351988387,1.44010268380848,0.960363786524726));
#62693=CARTESIAN_POINT('Ctrl Pts',(-25.1708083611699,-0.0292913940720509,
1.73070400606627));
#62694=CARTESIAN_POINT('Ctrl Pts',(-25.0912647339529,-1.47177606195057,
0.911081536334578));
#62695=CARTESIAN_POINT('Ctrl Pts',(-25.0117211067358,-1.56216989438597,
-0.745533073347261));
#62696=CARTESIAN_POINT('Ctrl Pts',(-24.9321774795187,-0.217429909788733,
-1.71724156038391));
#62697=CARTESIAN_POINT('Ctrl Pts',(-24.8526338523017,1.32705852566112,-1.11135503411405));
#62698=CARTESIAN_POINT('Ctrl Pts',(-24.7730902250846,1.65240519285512,0.515510835003435));
#62699=CARTESIAN_POINT('Ctrl Pts',(-24.6935465978676,0.45972070336827,1.66878734932737));
#62700=CARTESIAN_POINT('Ctrl Pts',(-24.6140029706505,-1.15529987783615,
1.28898275188315));
#62701=CARTESIAN_POINT('Ctrl Pts',(-24.5344593434335,-1.70896987902057,
-0.274984172237085));
#62702=CARTESIAN_POINT('Ctrl Pts',(-24.4549157162164,-0.692643892901292,
-1.58632871120933));
#62703=CARTESIAN_POINT('Ctrl Pts',(-24.3753720889993,0.959999997842893,
-1.44034521782875));
#62704=CARTESIAN_POINT('Ctrl Pts',(-24.2958284617823,1.73071134961881,0.028854231598518));
#62705=CARTESIAN_POINT('Ctrl Pts',(-24.2162848345652,0.91145326574864,1.471545883327));
#62706=CARTESIAN_POINT('Ctrl Pts',(-24.1367412073482,-0.745138458349476,
1.56235816004816));
#62707=CARTESIAN_POINT('Ctrl Pts',(-24.0571975801311,-1.71718658460209,
0.217863663888931));
#62708=CARTESIAN_POINT('Ctrl Pts',(-23.977653952914,-1.1116902026846,-1.32677776422261));
#62709=CARTESIAN_POINT('Ctrl Pts',(-23.8981103256969,0.515093434652472,
-1.65253535392088));
#62710=CARTESIAN_POINT('Ctrl Pts',(-23.8185666984799,1.66867117443778,-0.460142210605531));
#62711=CARTESIAN_POINT('Ctrl Pts',(-23.7390230712628,1.28927452997115,1.1549742545824));
#62712=CARTESIAN_POINT('Ctrl Pts',(-23.6594794440458,-0.27455249178663,
1.7090392832332));
#62713=CARTESIAN_POINT('Ctrl Pts',(-23.5799358168287,-1.58615370447617,
0.693044564336977));
#62714=CARTESIAN_POINT('Ctrl Pts',(-23.5003921896117,-1.44058765995127,
-0.959636147910556));
#62715=CARTESIAN_POINT('Ctrl Pts',(-23.4208485623946,0.0284170672840143,
-1.73071858274749));
#62716=CARTESIAN_POINT('Ctrl Pts',(-23.3413049351776,1.47131561081499,-0.91182493700963));
#62717=CARTESIAN_POINT('Ctrl Pts',(-23.2617613079605,1.56254632602784,0.744743795809934));
#62718=CARTESIAN_POINT('Ctrl Pts',(-23.1822176807434,0.218297404088875,
1.71713149925932));
#62719=CARTESIAN_POINT('Ctrl Pts',(-23.1026740535264,-1.32649691813226,
1.11202530032643));
#62720=CARTESIAN_POINT('Ctrl Pts',(-23.0231304263093,-1.65266540955062,
-0.514676001437202));
#62721=CARTESIAN_POINT('Ctrl Pts',(-22.9435867990922,-0.460563688484515,
-1.66855489308264));
#62722=CARTESIAN_POINT('Ctrl Pts',(-22.8640431718752,1.15464855763828,-1.28956622580011));
#62723=CARTESIAN_POINT('Ctrl Pts',(-22.7844995446581,1.7091085784047,0.274120793819028));
#62724=CARTESIAN_POINT('Ctrl Pts',(-22.7049559174411,0.693445191554635,
1.58597859654229));
#62725=CARTESIAN_POINT('Ctrl Pts',(-22.625412290224,-0.959272236750958,
1.44083001016057));
#62726=CARTESIAN_POINT('Ctrl Pts',(-22.5458686630069,-1.73072570545184,
-0.0279799011564179));
#62727=CARTESIAN_POINT('Ctrl Pts',(-22.4663250357899,-0.912196550093822,
-1.47108524442924));
#62728=CARTESIAN_POINT('Ctrl Pts',(-22.3867814085729,0.74434908575382,-1.56273439231303));
#62729=CARTESIAN_POINT('Ctrl Pts',(-22.3072377813557,1.71707630435912,-0.218731130360849));
#62730=CARTESIAN_POINT('Ctrl Pts',(-22.2276941541387,1.11236032701816,1.32621598740799));
#62731=CARTESIAN_POINT('Ctrl Pts',(-22.1481505269216,-0.5142585353843,1.65279535973601));
#62732=CARTESIAN_POINT('Ctrl Pts',(-22.0686068997046,-1.66843850526939,
0.460985136978328));
#62733=CARTESIAN_POINT('Ctrl Pts',(-21.9890632724875,-1.28985783935138,
-1.15432278702462));
#62734=CARTESIAN_POINT('Ctrl Pts',(-21.9095196452705,0.273689078361827,
-1.70917776453064));
#62735=CARTESIAN_POINT('Ctrl Pts',(-21.8299760180534,1.58580338741888,-0.693845774528669));
#62736=CARTESIAN_POINT('Ctrl Pts',(-21.7504323908364,1.44107226844117,0.958908264387324));
#62737=CARTESIAN_POINT('Ctrl Pts',(-21.6708887636193,-0.0275427332436607,
1.73073271773141));
#62738=CARTESIAN_POINT('Ctrl Pts',(-21.5913451364023,-1.47085478418445,
0.912568104977495));
#62739=CARTESIAN_POINT('Ctrl Pts',(-21.5118015091852,-1.5629223588917,-0.7439543282063));
#62740=CARTESIAN_POINT('Ctrl Pts',(-21.4322578819681,-0.219164842677231,
-1.717020999905));
#62741=CARTESIAN_POINT('Ctrl Pts',(-21.352714254751,1.32593497206768,-1.11269528273844));
#62742=CARTESIAN_POINT('Ctrl Pts',(-21.273170627534,1.65292520446879,0.513841036520355));
#62743=CARTESIAN_POINT('Ctrl Pts',(-21.1936270003169,0.461406556060124,
1.66832201100544));
#62744=CARTESIAN_POINT('Ctrl Pts',(-21.1140833730999,-1.15399694276216,
1.29014937060639));
#62745=CARTESIAN_POINT('Ctrl Pts',(-21.0345397458828,-1.70924684160662,
-0.273257345442523));
#62746=CARTESIAN_POINT('Ctrl Pts',(-20.9549961186657,-0.694246313233563,
-1.58562807711711));
#62747=CARTESIAN_POINT('Ctrl Pts',(-20.8754524914487,0.958544230842836,
-1.44131443477765));
#62748=CARTESIAN_POINT('Ctrl Pts',(-20.7959088642316,1.73073961958576,0.0271055635735854));
#62749=CARTESIAN_POINT('Ctrl Pts',(-20.7163652370146,0.912939601636987,
1.4706242300953));
#62750=CARTESIAN_POINT('Ctrl Pts',(-20.6368216097975,-0.743559523192568,
1.56311022575189));
#62751=CARTESIAN_POINT('Ctrl Pts',(-20.5572779825805,-1.71696558590049,
0.219598541010339));
#62752=CARTESIAN_POINT('Ctrl Pts',(-20.4777343553634,-1.11303016746587,
-1.3256538721293));
#62753=CARTESIAN_POINT('Ctrl Pts',(-20.3981907281463,0.513423504872026,
-1.65305494374066));
#62754=CARTESIAN_POINT('Ctrl Pts',(-20.3186471009293,1.66820541029823,-0.461827945702956));
#62755=CARTESIAN_POINT('Ctrl Pts',(-20.2391034737122,1.29044081954653,1.15367102487173));
#62756=CARTESIAN_POINT('Ctrl Pts',(-20.1595598464952,-0.272825595088725,
1.70931580962822));
#62757=CARTESIAN_POINT('Ctrl Pts',(-20.0800162192781,-1.58545266564817,
0.694646807643726));
#62758=CARTESIAN_POINT('Ctrl Pts',(-20.0004725920611,-1.44155650915452,
-0.958180136140769));
#62759=CARTESIAN_POINT('Ctrl Pts',(-19.9209289648439,0.0266683921741259,
-1.73074641101443));
#62760=CARTESIAN_POINT('Ctrl Pts',(-19.841385337627,1.47039358217654,-0.913311040048543));
#62761=CARTESIAN_POINT('Ctrl Pts',(-19.7618417104098,1.5632979928816,0.743164670737831));
#62762=CARTESIAN_POINT('Ctrl Pts',(-19.6822980831928,0.220032225332462,
1.71691006234914));
#62763=CARTESIAN_POINT('Ctrl Pts',(-19.6027544559757,-1.32537268761077,
1.11336498117908));
#62764=CARTESIAN_POINT('Ctrl Pts',(-19.5232108287587,-1.65318457754334,
-0.513005940465945));
#62765=CARTESIAN_POINT('Ctrl Pts',(-19.4436672015416,-0.462249305879991,
-1.66808870315519));
#62766=CARTESIAN_POINT('Ctrl Pts',(-19.3641235743246,1.15334503337407,-1.29073218615321));
#62767=CARTESIAN_POINT('Ctrl Pts',(-19.2845799471075,1.70938466859105,0.272393827327927));
#62768=CARTESIAN_POINT('Ctrl Pts',(-19.2050363198905,0.695047257733653,
1.58527715302323));
#62769=CARTESIAN_POINT('Ctrl Pts',(-19.1254926926734,-0.957815980304312,
1.44179849155635));
#62770=CARTESIAN_POINT('Ctrl Pts',(-19.0459490654563,-1.73075309201701,
-0.0262312190731219));
#62771=CARTESIAN_POINT('Ctrl Pts',(-18.9664054382393,-0.913682420188505,
-1.47016284044285));
#62772=CARTESIAN_POINT('Ctrl Pts',(-18.8868618110222,0.742769770867235,
-1.56348566026885));
#62773=CARTESIAN_POINT('Ctrl Pts',(-18.8073181838051,1.71685442925448,-0.220465895615978));
#62774=CARTESIAN_POINT('Ctrl Pts',(-18.7277745565881,1.11369972385674,1.32509141853002));
#62775=CARTESIAN_POINT('Ctrl Pts',(-18.648230929371,-0.512588343328754,
1.65331410586857));
#62776=CARTESIAN_POINT('Ctrl Pts',(-18.568687302154,-1.66797188958377,0.462670636564333));
#62777=CARTESIAN_POINT('Ctrl Pts',(-18.4891436749369,-1.29102347040784,
-1.15301896829003));
#62778=CARTESIAN_POINT('Ctrl Pts',(-18.4096000477198,0.271962042187704,
-1.70945341849072));
#62779=CARTESIAN_POINT('Ctrl Pts',(-18.3300564205028,1.58510153925351,-0.695447663477738));
#62780=CARTESIAN_POINT('Ctrl Pts',(-18.2505127932857,1.44204038196771,0.957451763356733));
#62781=CARTESIAN_POINT('Ctrl Pts',(-18.1709691660687,-0.0257940442985307,
1.73075966259305));
#62782=CARTESIAN_POINT('Ctrl Pts',(-18.0914255388516,-1.46993200490897,
0.914053742033148));
#62783=CARTESIAN_POINT('Ctrl Pts',(-18.0118819116345,-1.56367322790166,
-0.742374823606033));
#62784=CARTESIAN_POINT('Ctrl Pts',(-17.9323382844175,-0.220899551833179,
-1.71679868662007));
#62785=CARTESIAN_POINT('Ctrl Pts',(-17.8527946572004,1.32481006490503,-1.11403439547746));
#62786=CARTESIAN_POINT('Ctrl Pts',(-17.7732510299834,1.65344352870807,0.51217071348712));
#62787=CARTESIAN_POINT('Ctrl Pts',(-17.6937074027663,0.46309193772906,1.66785496959143));
#62788=CARTESIAN_POINT('Ctrl Pts',(-17.6141637755492,-1.1526928296404,1.29131467229181));
#62789=CARTESIAN_POINT('Ctrl Pts',(-17.5346201483322,-1.70952205932282,
-0.271530239695595));
#62790=CARTESIAN_POINT('Ctrl Pts',(-17.4550765211151,-0.695848024850479,
-1.58492582435021));
#62791=CARTESIAN_POINT('Ctrl Pts',(-17.3755328938981,0.957087485321226,
-1.44228218037317));
#62792=CARTESIAN_POINT('Ctrl Pts',(-17.295989266681,1.73076612274215,0.025356867878193));
#62793=CARTESIAN_POINT('Ctrl Pts',(-17.216445639464,0.914425005558822,1.46970107558961));
#62794=CARTESIAN_POINT('Ctrl Pts',(-17.1369020122469,-0.741979828979377,
1.56386069576808));
#62795=CARTESIAN_POINT('Ctrl Pts',(-17.0573583850298,-1.71674283444945,
0.221333193956447));
#62796=CARTESIAN_POINT('Ctrl Pts',(-16.9778147578128,-1.11436899601991,
-1.32452862675371));
#62797=CARTESIAN_POINT('Ctrl Pts',(-16.8982711305957,0.511753050967637,
-1.6535728460536));
#62798=CARTESIAN_POINT('Ctrl Pts',(-16.8187275033786,1.66773794318562,-0.463513209347343));
#62799=CARTESIAN_POINT('Ctrl Pts',(-16.7391838761616,1.29160579178658,1.15236661744596));
#62800=CARTESIAN_POINT('Ctrl Pts',(-16.6596402489446,-0.271098419879153,
1.709590591083));
#62801=CARTESIAN_POINT('Ctrl Pts',(-16.5800966217275,-1.58475000832453,
0.696248341826323));
#62802=CARTESIAN_POINT('Ctrl Pts',(-16.5005529945104,-1.44252388675729,
-0.956723146221068));
#62803=CARTESIAN_POINT('Ctrl Pts',(-16.4210093672934,0.0249196898400101,
-1.73077247246389));
#62804=CARTESIAN_POINT('Ctrl Pts',(-16.3414657400763,1.46947005249952,-0.914796210741802));
#62805=CARTESIAN_POINT('Ctrl Pts',(-16.2619221128592,1.56404806385614,0.741584787012495));
#62806=CARTESIAN_POINT('Ctrl Pts',(-16.1823784856422,0.221766821958055,
1.7166868727462));
#62807=CARTESIAN_POINT('Ctrl Pts',(-16.1028348584251,-1.32424710409405,
1.11470352546272));
#62808=CARTESIAN_POINT('Ctrl Pts',(-16.0232912312081,-1.6537020578969,-0.511335355797014));
#62809=CARTESIAN_POINT('Ctrl Pts',(-15.943747603991,-0.463934451392264,
-1.66762081037383));
#62810=CARTESIAN_POINT('Ctrl Pts',(-15.8642039767739,1.15204033172758,-1.29189682887354));
#62811=CARTESIAN_POINT('Ctrl Pts',(-15.7846603495569,1.70965901376687,0.270666582765945));
#62812=CARTESIAN_POINT('Ctrl Pts',(-15.7051167223398,0.696648614379695,
1.58457409118771));
#62813=CARTESIAN_POINT('Ctrl Pts',(-15.6255730951228,-0.956358746079515,
1.44276550110464));
#62814=CARTESIAN_POINT('Ctrl Pts',(-15.5460294679057,-1.73077871175787,
-0.0244825102119152));
#62815=CARTESIAN_POINT('Ctrl Pts',(-15.4664858406887,-0.915167357558401,
-1.46923893565345));
#62816=CARTESIAN_POINT('Ctrl Pts',(-15.3869422134716,0.741189697730577,
-1.56423533215388));
#62817=CARTESIAN_POINT('Ctrl Pts',(-15.3073985862545,1.71663080151387,-0.222200435810386));
#62818=CARTESIAN_POINT('Ctrl Pts',(-15.2278549590375,1.11503798378458,1.32396549694398));
#62819=CARTESIAN_POINT('Ctrl Pts',(-15.1483113318204,-0.510917628001855,
1.65383116422973));
#62820=CARTESIAN_POINT('Ctrl Pts',(-15.0687677046033,-1.66750357116349,
0.464355663836996));
#62821=CARTESIAN_POINT('Ctrl Pts',(-14.9892240773863,-1.29218778353415,
-1.15171397250602));
#62822=CARTESIAN_POINT('Ctrl Pts',(-14.9096804501692,0.270234728383482,
-1.70972732737007));
#62823=CARTESIAN_POINT('Ctrl Pts',(-14.8301368229522,1.58439807295096,-0.697048842485089));
#62824=CARTESIAN_POINT('Ctrl Pts',(-14.7505931957351,1.44300702339981,0.955994284919805));
#62825=CARTESIAN_POINT('Ctrl Pts',(-14.671049568518,-0.0240453290217912,
1.73078484062367));
#62826=CARTESIAN_POINT('Ctrl Pts',(-14.591505941301,-1.46900772506611,0.91553844598496));
#62827=CARTESIAN_POINT('Ctrl Pts',(-14.5119623140839,-1.56442250064936,
-0.740794561158851));
#62828=CARTESIAN_POINT('Ctrl Pts',(-14.4324186868669,-0.222634035485727,
-1.71657462075608));
#62829=CARTESIAN_POINT('Ctrl Pts',(-14.3528750596498,1.3236838053215,-1.11537237096409));
#62830=CARTESIAN_POINT('Ctrl Pts',(-14.2733314324328,1.65396016504384,0.510499867608859));
#62831=CARTESIAN_POINT('Ctrl Pts',(-14.1937878052157,0.46477684665457,1.66738622556214));
#62832=CARTESIAN_POINT('Ctrl Pts',(-14.1142441779986,-1.15138753980216,
1.29247865574979));
#62833=CARTESIAN_POINT('Ctrl Pts',(-14.0347005507816,-1.70979553188824,
-0.269802856759417));
#62834=CARTESIAN_POINT('Ctrl Pts',(-13.9551569235645,-0.697449026116917,
-1.58422195362553));
#62835=CARTESIAN_POINT('Ctrl Pts',(-13.8756132963474,0.955629762765192,
-1.44324845362737));
#62836=CARTESIAN_POINT('Ctrl Pts',(-13.7960696691304,1.73079085906093,0.0236081462974931));
#62837=CARTESIAN_POINT('Ctrl Pts',(-13.7165260419133,0.915909475997773,
1.46877642075232));
#62838=CARTESIAN_POINT('Ctrl Pts',(-13.6369824146963,-0.740399377322555,
1.5646095693306));
#62839=CARTESIAN_POINT('Ctrl Pts',(-13.5574387874792,-1.71651833047635,
0.223067620956417));
#62840=CARTESIAN_POINT('Ctrl Pts',(-13.4778951602621,-1.11570668697998,
-1.32340202924457));
#62841=CARTESIAN_POINT('Ctrl Pts',(-13.3983515330451,0.510082074644636,
-1.65408906033102));
#62842=CARTESIAN_POINT('Ctrl Pts',(-13.318807905828,1.66726877357721,-0.465197999818213));
#62843=CARTESIAN_POINT('Ctrl Pts',(-13.239264278611,1.29276944550198,1.15106103363678));
#62844=CARTESIAN_POINT('Ctrl Pts',(-13.1597206513939,-0.269370967921155,
1.70986362731701));
#62845=CARTESIAN_POINT('Ctrl Pts',(-13.0801770241769,-1.5840457332226,0.697849165249764));
#62846=CARTESIAN_POINT('Ctrl Pts',(-13.0006333969598,-1.44348979177201,
-0.955265179638894));
#62847=CARTESIAN_POINT('Ctrl Pts',(-12.9210897697427,0.023170962066939,
-1.73079676706925));
#62848=CARTESIAN_POINT('Ctrl Pts',(-12.8415461425257,1.46854502272674,-0.916280447573221));
#62849=CARTESIAN_POINT('Ctrl Pts',(-12.7620025153086,1.56479653818574,0.740004146246785));
#62850=CARTESIAN_POINT('Ctrl Pts',(-12.6824588880916,0.223501192194875,
1.71646193067834));
#62851=CARTESIAN_POINT('Ctrl Pts',(-12.6029152608745,-1.32312016873115,
1.11604093181088));
#62852=CARTESIAN_POINT('Ctrl Pts',(-12.5233716336574,-1.65421785008302,
-0.509664249135823));
#62853=CARTESIAN_POINT('Ctrl Pts',(-12.4438280064404,-0.465619123301057,
-1.66715121521621));
#62854=CARTESIAN_POINT('Ctrl Pts',(-12.3642843792233,1.15073445403071,-1.29306015277216));
#62855=CARTESIAN_POINT('Ctrl Pts',(-12.2847407520063,1.70993161365207,0.26893906189636));
#62856=CARTESIAN_POINT('Ctrl Pts',(-12.2051971247892,0.698249259857993,
1.58386941175347));
#62857=CARTESIAN_POINT('Ctrl Pts',(-12.1256534975721,-0.954900535564221,
1.44373103781822));
#62858=CARTESIAN_POINT('Ctrl Pts',(-12.0461098703551,-1.73080256464825,
-0.0227337763580157));
#62859=CARTESIAN_POINT('Ctrl Pts',(-11.966566243138,-0.91665136068759,-1.46831353100421));
#62860=CARTESIAN_POINT('Ctrl Pts',(-11.8870226159209,0.739608867956876,
-1.5649834072028));
#62861=CARTESIAN_POINT('Ctrl Pts',(-11.8074789887039,1.71640542136559,-0.223934749173347));
#62862=CARTESIAN_POINT('Ctrl Pts',(-11.7279353614868,1.11637510543549,1.32283822379925));
#62863=CARTESIAN_POINT('Ctrl Pts',(-11.6483917342698,-0.509246391109146,
1.65434653429165));
#62864=CARTESIAN_POINT('Ctrl Pts',(-11.5688481070527,-1.66703355048665,
0.466040217076157));
#62865=CARTESIAN_POINT('Ctrl Pts',(-11.4893044798357,-1.29335077754172,
-1.15040780100482));
#62866=CARTESIAN_POINT('Ctrl Pts',(-11.4097608526186,0.268507138712558,
-1.70999949088906));
#62867=CARTESIAN_POINT('Ctrl Pts',(-11.3302172254015,1.58369298922935,-0.698649309916132));
#62868=CARTESIAN_POINT('Ctrl Pts',(-11.2506735981845,1.44397219175068,0.954535830564389));
#62869=CARTESIAN_POINT('Ctrl Pts',(-11.1711299709674,-0.0222965891985885,
1.73080825179759));
#62870=CARTESIAN_POINT('Ctrl Pts',(-11.0915863437504,-1.46808194559948,
0.917022215317227));
#62871=CARTESIAN_POINT('Ctrl Pts',(-11.0120427165333,-1.56517017636985,
-0.73921354247797));
#62872=CARTESIAN_POINT('Ctrl Pts',(-10.9324990893162,-0.224368291864247,
-1.71634880254173));
#62873=CARTESIAN_POINT('Ctrl Pts',(-10.8529554620992,1.32255619446684,-1.11670920783251));
#62874=CARTESIAN_POINT('Ctrl Pts',(-10.7734118348821,1.65447511294868,0.508828500591231));
#62875=CARTESIAN_POINT('Ctrl Pts',(-10.6938682076651,0.46646128111671,1.66691577939602));
#62876=CARTESIAN_POINT('Ctrl Pts',(-10.614324580448,-1.1500810745799,1.29364131979218));
#62877=CARTESIAN_POINT('Ctrl Pts',(-10.5347809532309,-1.71006725902369,
-0.268075198397277));
#62878=CARTESIAN_POINT('Ctrl Pts',(-10.4552373260139,-0.699049315398613,
-1.58351646566153));
#62879=CARTESIAN_POINT('Ctrl Pts',(-10.3756936987968,0.954171064662698,
-1.44421325355396));
#62880=CARTESIAN_POINT('Ctrl Pts',(-10.2961500715798,1.73081382851686,0.0218594006165701));
#62881=CARTESIAN_POINT('Ctrl Pts',(-10.2166064443627,0.917393011438508,
1.46785026652732));
#62882=CARTESIAN_POINT('Ctrl Pts',(-10.1370628171456,-0.738818169835363,
1.565356845675));
#62883=CARTESIAN_POINT('Ctrl Pts',(-10.0575191899286,-1.71629207421038,
0.224801820239825));
#62884=CARTESIAN_POINT('Ctrl Pts',(-9.97797556271151,-1.11704323898056,
-1.32227408075192));
#62885=CARTESIAN_POINT('Ctrl Pts',(-9.89843193549448,0.50841057760874,-1.65460358604592));
#62886=CARTESIAN_POINT('Ctrl Pts',(-9.81888830827739,1.66679790195186,-0.466882315395799));
#62887=CARTESIAN_POINT('Ctrl Pts',(-9.73934468106036,1.29393177950496,1.14975427477686));
#62888=CARTESIAN_POINT('Ctrl Pts',(-9.65980105384328,-0.26764324097813,
1.71013491805157));
#62889=CARTESIAN_POINT('Ctrl Pts',(-9.58025742662623,-1.58333984106127,
0.699449276279938));
#62890=CARTESIAN_POINT('Ctrl Pts',(-9.50071379940916,-1.44445422321269,
-0.953806237882455));
#62891=CARTESIAN_POINT('Ctrl Pts',(-9.42117017219211,0.0214222106399076,
-1.73081929480574));
#62892=CARTESIAN_POINT('Ctrl Pts',(-9.34162654497504,1.4676184938025,-0.917763749027703));
#62893=CARTESIAN_POINT('Ctrl Pts',(-9.26208291775799,1.56554341510633,0.73842275005424));
#62894=CARTESIAN_POINT('Ctrl Pts',(-9.18253929054093,0.22523533427249,1.71623523637514));
#62895=CARTESIAN_POINT('Ctrl Pts',(-9.10299566332387,-1.32199188267247,
1.11737719885839));
#62896=CARTESIAN_POINT('Ctrl Pts',(-9.02345203610681,-1.65473195357519,
-0.507992622188313));
#62897=CARTESIAN_POINT('Ctrl Pts',(-8.94390840888974,-0.467303319886586,
-1.66667991816168));
#62898=CARTESIAN_POINT('Ctrl Pts',(-8.86436478167269,1.14942740161649,-1.29422215666154));
#62899=CARTESIAN_POINT('Ctrl Pts',(-8.78482115445563,1.71020246796842,0.267211266482613));
#62900=CARTESIAN_POINT('Ctrl Pts',(-8.70527752723857,0.699849192534625,
1.58316311543983));
#62901=CARTESIAN_POINT('Ctrl Pts',(-8.62573390002151,-0.953441350246909,
1.4446951007115));
#62902=CARTESIAN_POINT('Ctrl Pts',(-8.54619027280445,-1.73082465066384,
-0.0209850192964212));
#62903=CARTESIAN_POINT('Ctrl Pts',(-8.46664664558739,-0.918134428061233,
-1.46738662743981));
#62904=CARTESIAN_POINT('Ctrl Pts',(-8.38710301837034,0.738027283159815,
-1.56572988465197));
#62905=CARTESIAN_POINT('Ctrl Pts',(-8.30755939115327,1.71617828903966,-0.225668833934531));
#62906=CARTESIAN_POINT('Ctrl Pts',(-8.22801576393622,1.11771108744463,1.32170960024654));
#62907=CARTESIAN_POINT('Ctrl Pts',(-8.14847213671915,-0.507574634356665,
1.65486021552826));
#62908=CARTESIAN_POINT('Ctrl Pts',(-8.06892850950209,-1.66656182803301,
0.467724294562213));
#62909=CARTESIAN_POINT('Ctrl Pts',(-7.98938488228503,-1.29451245124338,
-1.1491004551197));
#62910=CARTESIAN_POINT('Ctrl Pts',(-7.90984125506798,0.266779274938363,
-1.71026990876992));
#62911=CARTESIAN_POINT('Ctrl Pts',(-7.83029762785091,1.58298628880849,-0.700249064137086));
#62912=CARTESIAN_POINT('Ctrl Pts',(-7.75075400063385,1.44493588603502,0.953076401779334));
#62913=CARTESIAN_POINT('Ctrl Pts',(-7.6712103734168,-0.020547826614065,
1.73082989609086));
#62914=CARTESIAN_POINT('Ctrl Pts',(-7.59166674619973,-1.46715466745408,
0.918505048515373));
#62915=CARTESIAN_POINT('Ctrl Pts',(-7.51212311898269,-1.56591625429995,
-0.737631769177359));
#62916=CARTESIAN_POINT('Ctrl Pts',(-7.4325794917656,-0.226102319198319,
-1.71612123220756));
#62917=CARTESIAN_POINT('Ctrl Pts',(-7.35303586454856,1.32142723349209,-1.11804490471801));
#62918=CARTESIAN_POINT('Ctrl Pts',(-7.27349223733149,1.65498837189696,0.507156614140401));
#62919=CARTESIAN_POINT('Ctrl Pts',(-7.19394861011444,0.468145239395855,
1.6664436315734));
#62920=CARTESIAN_POINT('Ctrl Pts',(-7.11440498289737,-1.14877343530734,
1.29480266323198));
#62921=CARTESIAN_POINT('Ctrl Pts',(-7.03486135568031,-1.71033724045177,
-0.266347266372873));
#62922=CARTESIAN_POINT('Ctrl Pts',(-6.95531772846326,-0.700648891061883,
-1.5828093611785));
#62923=CARTESIAN_POINT('Ctrl Pts',(-6.87577410124619,0.952711392503003,
-1.44517657916793));
#62924=CARTESIAN_POINT('Ctrl Pts',(-6.79623047402915,1.73083503108646,0.0201106326207077));
#62925=CARTESIAN_POINT('Ctrl Pts',(-6.71668684681207,0.918875610366531,
1.46692261386005));
#62926=CARTESIAN_POINT('Ctrl Pts',(-6.63714321959502,-0.737236208132049,
1.56610252403845));
#62927=CARTESIAN_POINT('Ctrl Pts',(-6.55759959237796,-1.7160640658825,0.226535790036225));
#62928=CARTESIAN_POINT('Ctrl Pts',(-6.47805596516089,-1.11837865065723,
-1.32114478242718));
#62929=CARTESIAN_POINT('Ctrl Pts',(-6.39851233794384,0.506738561566241,
-1.65511642267311));
#62930=CARTESIAN_POINT('Ctrl Pts',(-6.31896871072678,1.66632532879034,-0.468566154360624));
#62931=CARTESIAN_POINT('Ctrl Pts',(-6.23942508350972,1.29509279260886,1.14844634220024));
#62932=CARTESIAN_POINT('Ctrl Pts',(-6.15988145629267,-0.265915240813773,
1.71040446300967));
#62933=CARTESIAN_POINT('Ctrl Pts',(-6.0803378290756,-1.58263233256119,0.70104867328343));
#62934=CARTESIAN_POINT('Ctrl Pts',(-6.00079420185854,-1.44541718009479,
-0.952346322441234));
#62935=CARTESIAN_POINT('Ctrl Pts',(-5.92125057464147,0.0196734373442374,
-1.7308400556503));
#62936=CARTESIAN_POINT('Ctrl Pts',(-5.84170694742443,1.46669046667259,-0.919246113591029));
#62937=CARTESIAN_POINT('Ctrl Pts',(-5.76216332020736,1.56628869385553,0.736840600049199));
#62938=CARTESIAN_POINT('Ctrl Pts',(-5.6826196929903,0.226969246420528,1.7160067900681));
#62939=CARTESIAN_POINT('Ctrl Pts',(-5.60307606577325,-1.32086224706982,
1.118712325241));
#62940=CARTESIAN_POINT('Ctrl Pts',(-5.52353243855618,-1.65524436784856,
-0.506320476660882));
#62941=CARTESIAN_POINT('Ctrl Pts',(-5.44398881133913,-0.468987039429618,
-1.66620691969142));
#62942=CARTESIAN_POINT('Ctrl Pts',(-5.36444518412206,1.1481191758193,-1.29538283935543));
#62943=CARTESIAN_POINT('Ctrl Pts',(-5.284901556905,1.71047157643935,0.265483198288593));
#62944=CARTESIAN_POINT('Ctrl Pts',(-5.20535792968795,0.701448410776275,
1.58245520296781));
#62945=CARTESIAN_POINT('Ctrl Pts',(-5.12581430247088,-0.951981191617268,
1.44565768880032));
#62946=CARTESIAN_POINT('Ctrl Pts',(-5.04627067525383,-1.73084496978208,
-0.019236240812523));
#62947=CARTESIAN_POINT('Ctrl Pts',(-4.96672704803676,-0.919616558165243,
-1.46645822590648));
#62948=CARTESIAN_POINT('Ctrl Pts',(-4.88718342081971,0.736444944953975,
-1.56647476373933));
#62949=CARTESIAN_POINT('Ctrl Pts',(-4.80763979360264,1.71594940476801,-0.227402688323648));
#62950=CARTESIAN_POINT('Ctrl Pts',(-4.7280961663856,1.11904592844805,1.32057962743803));
#62951=CARTESIAN_POINT('Ctrl Pts',(-4.64855253916852,-0.505902359450965,
1.65537220741512));
#62952=CARTESIAN_POINT('Ctrl Pts',(-4.56900891195147,-1.66608840428416,
0.46940789457605));
#62953=CARTESIAN_POINT('Ctrl Pts',(-4.4894652847344,-1.29567280345324,-1.14779193618536));
#62954=CARTESIAN_POINT('Ctrl Pts',(-4.40992165751735,0.265051138824868,
-1.71053858073654));
#62955=CARTESIAN_POINT('Ctrl Pts',(-4.33037803030029,1.58227797240973,-0.701848103514873));
#62956=CARTESIAN_POINT('Ctrl Pts',(-4.25083440308323,1.44589810526913,0.951616000054438));
#62957=CARTESIAN_POINT('Ctrl Pts',(-4.17129077586617,-0.0187990430534725,
1.73084977348145));
#62958=CARTESIAN_POINT('Ctrl Pts',(-4.09174714864911,-1.46622589157654,
0.919986944065575));
#62959=CARTESIAN_POINT('Ctrl Pts',(-4.01220352143205,-1.56666073367799,
-0.736049242871692));
#62960=CARTESIAN_POINT('Ctrl Pts',(-3.93265989421499,-0.227836115717847,
-1.71589190998592));
#62961=CARTESIAN_POINT('Ctrl Pts',(-3.85311626699793,1.32029692354984,-1.11937946025705));
#62962=CARTESIAN_POINT('Ctrl Pts',(-3.77357263978087,1.65549994136465,0.505484209963166));
#62963=CARTESIAN_POINT('Ctrl Pts',(-3.69402901256381,0.469828719773019,
1.66596978257618));
#62964=CARTESIAN_POINT('Ctrl Pts',(-3.61448538534676,-1.14746462331935,
1.29596268488375));
#62965=CARTESIAN_POINT('Ctrl Pts',(-3.53494175812969,-1.71060547589691,
-0.264619062450219));
#62966=CARTESIAN_POINT('Ctrl Pts',(-3.45539813091264,-0.702247751473749,
-1.58210064089821));
#62967=CARTESIAN_POINT('Ctrl Pts',(-3.37585450369557,0.951250747776082,
-1.44613842948588));
#62968=CARTESIAN_POINT('Ctrl Pts',(-3.29631087647852,1.73085446674812,0.0183618440950245));
#62969=CARTESIAN_POINT('Ctrl Pts',(-3.21676724926145,0.920357271268342,
1.46599346369761));
#62970=CARTESIAN_POINT('Ctrl Pts',(-3.13722362204439,-0.735653493827597,
1.5668466036596));
#62971=CARTESIAN_POINT('Ctrl Pts',(-3.05767999482733,-1.71583430572539,
0.22826952857563));
#62972=CARTESIAN_POINT('Ctrl Pts',(-2.97813636761028,-1.1197129206469,-1.32001413542344));
#62973=CARTESIAN_POINT('Ctrl Pts',(-2.89859274039322,0.505066028224394,
-1.65562756968869));
#62974=CARTESIAN_POINT('Ctrl Pts',(-2.81904911317615,1.66585105457453,-0.470249514994343));
#62975=CARTESIAN_POINT('Ctrl Pts',(-2.7395054859591,1.29625248362939,1.14713723724332));
#62976=CARTESIAN_POINT('Ctrl Pts',(-2.65996185874204,-0.264186969193862,
1.7106722619139));
#62977=CARTESIAN_POINT('Ctrl Pts',(-2.58041823152498,-1.58192320844134,
0.702647354631853));
#62978=CARTESIAN_POINT('Ctrl Pts',(-2.50087460430791,-1.44637866144143,
-0.950885434813853));
#62979=CARTESIAN_POINT('Ctrl Pts',(-2.42133097709086,0.0179246439767291,
-1.73085904956586));
#62980=CARTESIAN_POINT('Ctrl Pts',(-2.3417873498738,1.46576094226225,-0.920727539780172));
#62981=CARTESIAN_POINT('Ctrl Pts',(-2.26224372265674,1.56703237371457,0.735257697904209));
#62982=CARTESIAN_POINT('Ctrl Pts',(-2.18270009543968,0.228702926789087,
1.71577659188141));
#62983=CARTESIAN_POINT('Ctrl Pts',(-2.10315646822262,-1.31973126292469,
1.12004630980263));
#62984=CARTESIAN_POINT('Ctrl Pts',(-2.02361284100556,-1.65575509266798,
-0.504647814653044));
#62985=CARTESIAN_POINT('Ctrl Pts',(-1.9440692137885,-0.470670279664775,
-1.66573221954342));
#62986=CARTESIAN_POINT('Ctrl Pts',(-1.86452558657144,1.14680977693736,-1.2965422010826));
#62987=CARTESIAN_POINT('Ctrl Pts',(-1.78498195935438,1.71073894075879,0.263754861761375));
#62988=CARTESIAN_POINT('Ctrl Pts',(-1.70543833213732,0.70304690921405,1.58174566996773));
#62989=CARTESIAN_POINT('Ctrl Pts',(-1.62589470492026,-0.950520054074415,
1.44661881076732));
#62990=CARTESIAN_POINT('Ctrl Pts',(-1.5463510777032,-1.73086353544171,-0.017487461036164));
#62991=CARTESIAN_POINT('Ctrl Pts',(-1.46680745048614,-0.921097723940694,
-1.46552829253389));
#62992=CARTESIAN_POINT('Ctrl Pts',(-1.38726382326908,0.734861806468727,
-1.5672181097888));
#62993=CARTESIAN_POINT('Ctrl Pts',(-1.30772019605202,1.71571886081011,-0.229136185143489));
#62994=CARTESIAN_POINT('Ctrl Pts',(-1.22817656883497,1.12037945241918,1.319448068468));
#62995=CARTESIAN_POINT('Ctrl Pts',(-1.1486329416179,-0.504229236589193,
1.6558829612631));
#62996=CARTESIAN_POINT('Ctrl Pts',(-1.06908931440084,-1.6656139089254,0.471090157824471));
#62997=CARTESIAN_POINT('Ctrl Pts',(-0.98954568718378,-1.29683063876905,
-1.14648061787195));
#62998=CARTESIAN_POINT('Ctrl Pts',(-0.910002059966725,0.263320465525717,
-1.71080859580406));
#62999=CARTESIAN_POINT('Ctrl Pts',(-0.830458432749663,1.58157234275566,
-0.703440562983143));
#63000=CARTESIAN_POINT('Ctrl Pts',(-0.750914805532606,1.44685068332373,
0.950143498150224));
#63001=CARTESIAN_POINT('Ctrl Pts',(-0.671371178315544,-0.0170347429126065,
1.73088900618291));
#63002=CARTESIAN_POINT('Ctrl Pts',(-0.591827551098487,-1.46532503311589,
0.921427810374316));
#63003=CARTESIAN_POINT('Ctrl Pts',(-0.512283923881428,-1.56734778302374,
-0.734389871816786));
#63004=CARTESIAN_POINT('Ctrl Pts',(-0.432740296664362,-0.229675670455208,
-1.71580528473636));
#63005=CARTESIAN_POINT('Ctrl Pts',(-0.353196669447305,1.31936664475697,
-1.12043850518328));
#63006=CARTESIAN_POINT('Ctrl Pts',(-0.273653042230246,1.65562583122791,
0.503288797893469));
#63007=CARTESIAN_POINT('Ctrl Pts',(-0.194109415013187,0.472255537838747,
1.66650068200683));
#63008=CARTESIAN_POINT('Ctrl Pts',(-0.114565787796127,-1.14769222032782,
1.29508639656957));
#63009=CARTESIAN_POINT('Ctrl Pts',(-0.0615367029847541,-1.5205814962436,
0.259698171561206));
#63010=CARTESIAN_POINT('Ctrl Pts',(-0.0350221605790679,-1.44652267833248,
-0.222270985668021));
#63011=CARTESIAN_POINT('Ctrl Pts',(-0.547155045842891,-1.46121426462895,
-0.000470658046818673));
#63012=CARTESIAN_POINT('Ctrl Pts',(-0.535531338522404,-1.46184924216179,
-0.215008973536607));
#63013=CARTESIAN_POINT('Ctrl Pts',(-0.523907631201916,-1.41768133724367,
-0.429300105994831));
#63014=CARTESIAN_POINT('Ctrl Pts',(-0.512283923881429,-1.32739863927768,
-0.621989493604839));
#63015=CARTESIAN_POINT('Ctrl Pts',(-0.485769381475741,-1.12145707883424,
-1.06152834278995));
#63016=CARTESIAN_POINT('Ctrl Pts',(-0.459254839070054,-0.675566374644769,
-1.38866681376314));
#63017=CARTESIAN_POINT('Ctrl Pts',(-0.432740296664367,-0.194447303347988,
-1.45300825265757));
#63018=CARTESIAN_POINT('Ctrl Pts',(-0.40622575425868,0.286671767948793,
-1.51734969155201));
#63019=CARTESIAN_POINT('Ctrl Pts',(-0.379711211852995,0.80301920635284,
-1.31889409836768));
#63020=CARTESIAN_POINT('Ctrl Pts',(-0.353196669447309,1.11723612330005,
-0.949045084596062));
#63021=CARTESIAN_POINT('Ctrl Pts',(-0.326682127041623,1.43145304024725,
-0.579196070824442));
#63022=CARTESIAN_POINT('Ctrl Pts',(-0.300167584635933,1.5435394357376,-0.037953636465458));
#63023=CARTESIAN_POINT('Ctrl Pts',(-0.273653042230246,1.40235425125123,
0.426536228066234));
#63024=CARTESIAN_POINT('Ctrl Pts',(-0.249102028153501,1.27162450307314,
0.856628402697813));
#63025=CARTESIAN_POINT('Ctrl Pts',(-0.224551014076758,0.923746142995881,
1.22091487580054));
#63026=CARTESIAN_POINT('Ctrl Pts',(-0.200000000000013,0.502021735097343,
1.37727613462784));
#63027=CARTESIAN_POINT('',(-34.6365,-0.684664424539681,-0.958295198918239));
#63028=CARTESIAN_POINT('Ctrl Pts',(-34.6365,-0.686154072602779,-0.9596222324959));
#63029=CARTESIAN_POINT('Ctrl Pts',(-34.6365,-0.7119101001333,-0.945613082101837));
#63030=CARTESIAN_POINT('Ctrl Pts',(-34.6365,-0.737057208054438,-0.930606615436407));
#63031=CARTESIAN_POINT('Ctrl Pts',(-34.6365,-0.761530234615434,-0.914615833182014));
#63032=CARTESIAN_POINT('Ctrl Pts',(-34.6365,-0.801891049947194,-0.888243900475965));
#63033=CARTESIAN_POINT('Ctrl Pts',(-34.6365,-0.840419847997269,-0.859197627341817));
#63034=CARTESIAN_POINT('Ctrl Pts',(-34.6365,-0.877044577847601,-0.827775063525897));
#63035=CARTESIAN_POINT('Ctrl Pts',(-34.6365,-0.891050333973354,-0.815758680949148));
#63036=CARTESIAN_POINT('Ctrl Pts',(-34.6365,-0.904777454305529,-0.803394278639855));
#63037=CARTESIAN_POINT('Ctrl Pts',(-34.6365,-0.918221120557909,-0.790696745740664));
#63038=CARTESIAN_POINT('Ctrl Pts',(-34.6365,-0.926551929996928,-0.782828302345611));
#63039=CARTESIAN_POINT('Ctrl Pts',(-34.6365,-0.934775354469558,-0.774830435851512));
#63040=CARTESIAN_POINT('Ctrl Pts',(-34.6365,-0.942885419604258,-0.766711271506816));
#63041=CARTESIAN_POINT('Ctrl Pts',(-34.6365,-0.978536944636376,-0.731019746708046));
#63042=CARTESIAN_POINT('Ctrl Pts',(-34.6365,-1.01191327669552,-0.693076341324169));
#63043=CARTESIAN_POINT('Ctrl Pts',(-34.6365,-1.04293679416646,-0.653208812595354));
#63044=CARTESIAN_POINT('Ctrl Pts',(-34.6365,-1.06541205389432,-0.624326431230085));
#63045=CARTESIAN_POINT('Ctrl Pts',(-34.6365,-1.08665213278273,-0.594432978370132));
#63046=CARTESIAN_POINT('Ctrl Pts',(-34.6365,-1.10661916861093,-0.563638328343162));
#63047=CARTESIAN_POINT('Ctrl Pts',(-34.6365,-1.11501890060192,-0.550683635958747));
#63048=CARTESIAN_POINT('Ctrl Pts',(-34.6365,-1.12319324208052,-0.537569324701878));
#63049=CARTESIAN_POINT('Ctrl Pts',(-34.6365,-1.13113891356507,-0.524303043918853));
#63050=CARTESIAN_POINT('Ctrl Pts',(-34.6365,-1.1380110222127,-0.51282920900531));
#63051=CARTESIAN_POINT('Ctrl Pts',(-34.6365,-1.14471355135492,-0.50123871631513));
#63052=CARTESIAN_POINT('Ctrl Pts',(-34.6365,-1.15123207412817,-0.48955905836601));
#63053=CARTESIAN_POINT('Ctrl Pts',(-34.6365,-1.17683516242865,-0.443684352670734));
#63054=CARTESIAN_POINT('Ctrl Pts',(-34.6365,-1.19964285363905,-0.396372122447951));
#63055=CARTESIAN_POINT('Ctrl Pts',(-34.6365,-1.21956940907531,-0.347951651152172));
#63056=CARTESIAN_POINT('Ctrl Pts',(-34.6365,-1.23986899619782,-0.298624732672669));
#63057=CARTESIAN_POINT('Ctrl Pts',(-34.6365,-1.2571793448604,-0.248146802693327));
#63058=CARTESIAN_POINT('Ctrl Pts',(-34.6365,-1.27137376561068,-0.196827051143323));
#63059=CARTESIAN_POINT('Ctrl Pts',(-34.6365,-1.27949212467089,-0.167475225007287));
#63060=CARTESIAN_POINT('Ctrl Pts',(-34.6365,-1.28659049471938,-0.137847386060878));
#63061=CARTESIAN_POINT('Ctrl Pts',(-34.6365,-1.29263849229147,-0.10799760567475));
#63062=CARTESIAN_POINT('Ctrl Pts',(-34.6365,-1.29646959968636,-0.0890892458399302));
#63063=CARTESIAN_POINT('Ctrl Pts',(-34.6365,-1.2998791327864,-0.0700917822900422));
#63064=CARTESIAN_POINT('Ctrl Pts',(-34.6365,-1.3028582061524,-0.0510186173543007));
#63065=CARTESIAN_POINT('Ctrl Pts',(-34.6365,-1.30433493626761,-0.0415640274223254));
#63066=CARTESIAN_POINT('Ctrl Pts',(-34.6365,-1.30570555790757,-0.0320922880145657));
#63067=CARTESIAN_POINT('Ctrl Pts',(-34.6365,-1.30696764581746,-0.0226173109335764));
#63068=CARTESIAN_POINT('Ctrl Pts',(-34.6365,-1.31420352572401,0.0317052095011377));
#63069=CARTESIAN_POINT('Ctrl Pts',(-34.6365,-1.31789275479354,0.0862397373277177));
#63070=CARTESIAN_POINT('Ctrl Pts',(-34.6365,-1.31791881756557,0.140657257014611));
#63071=CARTESIAN_POINT('Ctrl Pts',(-34.6365,-1.31792247004294,0.148283412776851));
#63072=CARTESIAN_POINT('Ctrl Pts',(-34.6365,-1.31785410762944,0.155907313822103));
#63073=CARTESIAN_POINT('Ctrl Pts',(-34.6365,-1.31771333721581,0.163528092935519));
#63074=CARTESIAN_POINT('Ctrl Pts',(-34.6365,-1.31674443923682,0.21598057418652));
#63075=CARTESIAN_POINT('Ctrl Pts',(-34.6365,-1.3123496251762,0.268284454830481));
#63076=CARTESIAN_POINT('Ctrl Pts',(-34.6365,-1.30473184284742,0.320221776691518));
#63077=CARTESIAN_POINT('Ctrl Pts',(-34.6365,-1.3006747321352,0.347882775101802));
#63078=CARTESIAN_POINT('Ctrl Pts',(-34.6365,-1.29570254950683,0.375439959013181));
#63079=CARTESIAN_POINT('Ctrl Pts',(-34.6365,-1.28984013681239,0.402860769972335));
#63080=CARTESIAN_POINT('Ctrl Pts',(-34.6365,-1.28632199418306,0.419316507395516));
#63081=CARTESIAN_POINT('Ctrl Pts',(-34.6365,-1.28248316633568,0.435723131009655));
#63082=CARTESIAN_POINT('Ctrl Pts',(-34.6365,-1.27832836254595,0.452073542754125));
#63083=CARTESIAN_POINT('Ctrl Pts',(-34.6365,-1.27547249914963,0.463312230494656));
#63084=CARTESIAN_POINT('Ctrl Pts',(-34.6365,-1.27246679788216,0.474525738156413));
#63085=CARTESIAN_POINT('Ctrl Pts',(-34.6365,-1.26931881447351,0.485691489535342));
#63086=CARTESIAN_POINT('Ctrl Pts',(-34.6365,-1.25443545775983,0.538482066605106));
#63087=CARTESIAN_POINT('Ctrl Pts',(-34.6365,-1.23635097763686,0.590308106442404));
#63088=CARTESIAN_POINT('Ctrl Pts',(-34.6365,-1.21530442574023,0.640933424389205));
#63089=CARTESIAN_POINT('Ctrl Pts',(-34.6365,-1.19380245740259,0.692654199788485));
#63090=CARTESIAN_POINT('Ctrl Pts',(-34.6365,-1.16920862107615,0.743122685571138));
#63091=CARTESIAN_POINT('Ctrl Pts',(-34.6365,-1.14172291998422,0.792087274667335));
#63092=CARTESIAN_POINT('Ctrl Pts',(-34.6365,-1.12633431912328,0.819501402304143));
#63093=CARTESIAN_POINT('Ctrl Pts',(-34.6365,-1.11003826917362,0.846444039154066));
#63094=CARTESIAN_POINT('Ctrl Pts',(-34.6365,-1.09286303313459,0.872869290765076));
#63095=CARTESIAN_POINT('Ctrl Pts',(-34.6365,-1.08109837366658,0.89097000774234));
#63096=CARTESIAN_POINT('Ctrl Pts',(-34.6365,-1.06892110442247,0.908827940355749));
#63097=CARTESIAN_POINT('Ctrl Pts',(-34.6365,-1.05633909029096,0.92642773863922));
#63098=CARTESIAN_POINT('Ctrl Pts',(-34.6365,-1.04773945000675,0.938456968040044));
#63099=CARTESIAN_POINT('Ctrl Pts',(-34.6365,-1.03894684652451,0.950370403618958));
#63100=CARTESIAN_POINT('Ctrl Pts',(-34.6365,-1.0299848727059,0.962135775346617));
#63101=CARTESIAN_POINT('Ctrl Pts',(-34.6365,-0.994691270463756,1.00846958064347));
#63102=CARTESIAN_POINT('Ctrl Pts',(-34.6365,-0.956729926976582,1.05257580844336));
#63103=CARTESIAN_POINT('Ctrl Pts',(-34.6365,-0.916323904549539,1.09419408100751));
#63104=CARTESIAN_POINT('Ctrl Pts',(-34.6365,-0.874305894879269,1.13747270320345));
#63105=CARTESIAN_POINT('Ctrl Pts',(-34.6365,-0.829644031989242,1.1780622586008));
#63106=CARTESIAN_POINT('Ctrl Pts',(-34.6365,-0.782534111930377,1.21564789997407));
#63107=CARTESIAN_POINT('Ctrl Pts',(-34.6365,-0.738322170255781,1.25092145132208));
#63108=CARTESIAN_POINT('Ctrl Pts',(-34.6365,-0.691953185744718,1.28355000577543));
#63109=CARTESIAN_POINT('Ctrl Pts',(-34.6365,-0.643551181830037,1.31323998384329));
#63110=CARTESIAN_POINT('Ctrl Pts',(-34.6365,-0.640378555707157,1.31518608508678));
#63111=CARTESIAN_POINT('Ctrl Pts',(-34.6365,-0.637197183227053,1.31711954607524));
#63112=CARTESIAN_POINT('Ctrl Pts',(-34.6365,-0.634007094575281,1.31904027763682));
#63113=CARTESIAN_POINT('Ctrl Pts',(-34.6365,-0.686154072602774,-0.959622232495904));
#63114=CARTESIAN_POINT('Ctrl Pts',(-34.6119489859232,-0.390562334310552,
-1.1685227208061));
#63115=CARTESIAN_POINT('Ctrl Pts',(-34.5608834294408,0.441559859931502,
-1.30438298146528));
#63116=CARTESIAN_POINT('Ctrl Pts',(-34.4833033305527,1.34388692616717,-0.366485362373245));
#63117=CARTESIAN_POINT('Ctrl Pts',(-34.4037597033356,1.03476789300364,0.932740929113639));
#63118=CARTESIAN_POINT('Ctrl Pts',(-34.3242160761186,-0.225138742279001,
1.37459976780186));
#63119=CARTESIAN_POINT('Ctrl Pts',(-34.2603404700946,-1.07071564015608,
0.715550826767906));
#63120=CARTESIAN_POINT('Ctrl Pts',(-34.2229794064764,-1.17675281276781,
0.161639855406849));
#63121=CARTESIAN_POINT('Ctrl Pts',(-34.2121328852638,-1.17605840265479,
0.000574308414346206));
#63122=CARTESIAN_POINT('Origin',(-34.6365,-3.28582941601228E-17,0.));
#63123=CARTESIAN_POINT('',(-34.6365,-1.4635,-1.79227059055215E-16));
#63124=CARTESIAN_POINT('Origin',(-34.6365,0.,0.));
#63125=CARTESIAN_POINT('Origin',(-34.6365,0.,0.));
#63126=CARTESIAN_POINT('',(-34.6365,0.6846644245395,-0.958295198918368));
#63127=CARTESIAN_POINT('Ctrl Pts',(-34.6365,0.635548045752339,1.32098221395624));
#63128=CARTESIAN_POINT('Ctrl Pts',(-34.6365,0.666498491669791,1.30253980504351));
#63129=CARTESIAN_POINT('Ctrl Pts',(-34.6365,0.696670008128909,1.28290514074601));
#63130=CARTESIAN_POINT('Ctrl Pts',(-34.6365,0.725984184660265,1.26207365955444));
#63131=CARTESIAN_POINT('Ctrl Pts',(-34.6365,0.773073530585445,1.22861064131428));
#63132=CARTESIAN_POINT('Ctrl Pts',(-34.6365,0.817952842411402,1.19206056398115));
#63133=CARTESIAN_POINT('Ctrl Pts',(-34.6365,0.860470315479712,1.15273759731246));
#63134=CARTESIAN_POINT('Ctrl Pts',(-34.6365,0.882577900258638,1.13229104306898));
#63135=CARTESIAN_POINT('Ctrl Pts',(-34.6365,0.904046247749025,1.1110942774146));
#63136=CARTESIAN_POINT('Ctrl Pts',(-34.6365,0.924849238970118,1.08918893459142));
#63137=CARTESIAN_POINT('Ctrl Pts',(-34.6365,0.933737523857988,1.07982965901852));
#63138=CARTESIAN_POINT('Ctrl Pts',(-34.6365,0.942504822960868,1.07034025158081));
#63139=CARTESIAN_POINT('Ctrl Pts',(-34.6365,0.951138112600303,1.06073646803148));
#63140=CARTESIAN_POINT('Ctrl Pts',(-34.6365,0.989630872686237,1.01791662165531));
#63141=CARTESIAN_POINT('Ctrl Pts',(-34.6365,1.02551732004391,0.972769428249441));
#63142=CARTESIAN_POINT('Ctrl Pts',(-34.6365,1.05864549743232,0.925607080115083));
#63143=CARTESIAN_POINT('Ctrl Pts',(-34.6365,1.0806661582941,0.894257752878159));
#63144=CARTESIAN_POINT('Ctrl Pts',(-34.6365,1.10146719775831,0.862017405404437));
#63145=CARTESIAN_POINT('Ctrl Pts',(-34.6365,1.12099192934309,0.828973605276758));
#63146=CARTESIAN_POINT('Ctrl Pts',(-34.6365,1.12904366504594,0.815346788227294));
#63147=CARTESIAN_POINT('Ctrl Pts',(-34.6365,1.13687822907506,0.801583312066227));
#63148=CARTESIAN_POINT('Ctrl Pts',(-34.6365,1.14449112932449,0.787689263461989));
#63149=CARTESIAN_POINT('Ctrl Pts',(-34.6365,1.15119354448111,0.775456910626577));
#63150=CARTESIAN_POINT('Ctrl Pts',(-34.6365,1.15772571146099,0.763119959343411));
#63151=CARTESIAN_POINT('Ctrl Pts',(-34.6365,1.16407270727518,0.750706322535687));
#63152=CARTESIAN_POINT('Ctrl Pts',(-34.6365,1.18968499603057,0.700613072164659));
#63153=CARTESIAN_POINT('Ctrl Pts',(-34.6365,1.21232701568682,0.649200916818433));
#63154=CARTESIAN_POINT('Ctrl Pts',(-34.6365,1.23185338093466,0.596758023613943));
#63155=CARTESIAN_POINT('Ctrl Pts',(-34.6365,1.25088764177288,0.545636798762549));
#63156=CARTESIAN_POINT('Ctrl Pts',(-34.6365,1.26696143620811,0.493535096364606));
#63157=CARTESIAN_POINT('Ctrl Pts',(-34.6365,1.27989180385019,0.440714302555275));
#63158=CARTESIAN_POINT('Ctrl Pts',(-34.6365,1.28743198375341,0.409912526536342));
#63159=CARTESIAN_POINT('Ctrl Pts',(-34.6365,1.29390232703675,0.378866200024003));
#63160=CARTESIAN_POINT('Ctrl Pts',(-34.6365,1.29925840715535,0.347628297483629));
#63161=CARTESIAN_POINT('Ctrl Pts',(-34.6365,1.30273792407846,0.327334947099519));
#63162=CARTESIAN_POINT('Ctrl Pts',(-34.6365,1.30574706385875,0.306960769457363));
#63163=CARTESIAN_POINT('Ctrl Pts',(-34.6365,1.30827220879121,0.286520718592337));
#63164=CARTESIAN_POINT('Ctrl Pts',(-34.6365,1.30983744822857,0.273850723573731));
#63165=CARTESIAN_POINT('Ctrl Pts',(-34.6365,1.31121690877827,0.261151572677647));
#63166=CARTESIAN_POINT('Ctrl Pts',(-34.6365,1.31240507505011,0.248453673487265));
#63167=CARTESIAN_POINT('Ctrl Pts',(-34.6365,1.31731668013685,0.195963489467908));
#63168=CARTESIAN_POINT('Ctrl Pts',(-34.6365,1.3189760904167,0.143408381037281));
#63169=CARTESIAN_POINT('Ctrl Pts',(-34.6365,1.31722292331031,0.0910320624908964));
#63170=CARTESIAN_POINT('Ctrl Pts',(-34.6365,1.31692479917861,0.0821255273229491));
#63171=CARTESIAN_POINT('Ctrl Pts',(-34.6365,1.31652787382802,0.0732241778386358));
#63172=CARTESIAN_POINT('Ctrl Pts',(-34.6365,1.31603120806162,0.0643292382201927));
#63173=CARTESIAN_POINT('Ctrl Pts',(-34.6365,1.31309184640608,0.0116873083521665));
#63174=CARTESIAN_POINT('Ctrl Pts',(-34.6365,1.30666269163376,-0.0407318065592056));
#63175=CARTESIAN_POINT('Ctrl Pts',(-34.6365,1.29689813812491,-0.0926593050314029));
#63176=CARTESIAN_POINT('Ctrl Pts',(-34.6365,1.29219527731605,-0.117668927565173));
#63177=CARTESIAN_POINT('Ctrl Pts',(-34.6365,1.28671806309696,-0.142564201344602));
#63178=CARTESIAN_POINT('Ctrl Pts',(-34.6365,1.28048041312089,-0.167312876218102));
#63179=CARTESIAN_POINT('Ctrl Pts',(-34.6365,1.27563401943483,-0.186541563641289));
#63180=CARTESIAN_POINT('Ctrl Pts',(-34.6365,1.27032853396833,-0.205681726868499));
#63181=CARTESIAN_POINT('Ctrl Pts',(-34.6365,1.26456972207496,-0.224717452852664));
#63182=CARTESIAN_POINT('Ctrl Pts',(-34.6365,1.26182301144504,-0.23379669209109));
#63183=CARTESIAN_POINT('Ctrl Pts',(-34.6365,1.25897402305304,-0.242849070418405));
#63184=CARTESIAN_POINT('Ctrl Pts',(-34.6365,1.25602686354908,-0.251863406655858));
#63185=CARTESIAN_POINT('Ctrl Pts',(-34.6365,1.23970756016791,-0.30177848171073));
#63186=CARTESIAN_POINT('Ctrl Pts',(-34.6365,1.22035602282228,-0.350615852547003));
#63187=CARTESIAN_POINT('Ctrl Pts',(-34.6365,1.19814539365861,-0.398117840475043));
#63188=CARTESIAN_POINT('Ctrl Pts',(-34.6365,1.17602990897011,-0.445416342419949));
#63189=CARTESIAN_POINT('Ctrl Pts',(-34.6365,1.15107898465775,-0.491391780007035));
#63190=CARTESIAN_POINT('Ctrl Pts',(-34.6365,1.12342395860753,-0.53575743875993));
#63191=CARTESIAN_POINT('Ctrl Pts',(-34.6365,1.10893424546816,-0.559002604662186));
#63192=CARTESIAN_POINT('Ctrl Pts',(-34.6365,1.09370162121455,-0.581805236030971));
#63193=CARTESIAN_POINT('Ctrl Pts',(-34.6365,1.07774169884391,-0.604119277574196));
#63194=CARTESIAN_POINT('Ctrl Pts',(-34.6365,1.06683927858885,-0.619362275180545));
#63195=CARTESIAN_POINT('Ctrl Pts',(-34.6365,1.05559742596417,-0.634377204151687));
#63196=CARTESIAN_POINT('Ctrl Pts',(-34.6365,1.04402064985082,-0.649148328629702));
#63197=CARTESIAN_POINT('Ctrl Pts',(-34.6365,1.03779477786861,-0.657092088544632));
#63198=CARTESIAN_POINT('Ctrl Pts',(-34.6365,1.03147122864614,-0.664966126131085));
#63199=CARTESIAN_POINT('Ctrl Pts',(-34.6365,1.02506186124697,-0.672754796849972));
#63200=CARTESIAN_POINT('Ctrl Pts',(-34.6365,0.993012679416858,-0.711700999889751));
#63201=CARTESIAN_POINT('Ctrl Pts',(-34.6365,0.958759462630057,-0.748595252324693));
#63202=CARTESIAN_POINT('Ctrl Pts',(-34.6365,0.922431964225527,-0.783185558398445));
#63203=CARTESIAN_POINT('Ctrl Pts',(-34.6365,0.886691317016434,-0.817217076684392));
#63204=CARTESIAN_POINT('Ctrl Pts',(-34.6365,0.8489421255063,-0.849019106260595));
#63205=CARTESIAN_POINT('Ctrl Pts',(-34.6365,0.809283769251354,-0.878307498888002));
#63206=CARTESIAN_POINT('Ctrl Pts',(-34.6365,0.769625412996408,-0.907595891515409));
#63207=CARTESIAN_POINT('Ctrl Pts',(-34.6365,0.728057253858435,-0.934371344062744));
#63208=CARTESIAN_POINT('Ctrl Pts',(-34.6365,0.684664424539256,-0.958295198918542));
#63209=CARTESIAN_POINT('Origin',(-34.6365,0.,0.));
#63210=CARTESIAN_POINT('Origin',(-35.5608671147362,0.,0.));
#63211=CARTESIAN_POINT('Ctrl Pts',(-34.6365,0.684664424539256,-0.958295198918542));
#63212=CARTESIAN_POINT('Ctrl Pts',(-34.6099854575943,1.00396030307469,-0.7301707867521));
#63213=CARTESIAN_POINT('Ctrl Pts',(-34.556956372783,1.39099115610471,0.0663998364373292));
#63214=CARTESIAN_POINT('Ctrl Pts',(-34.4774127455658,0.694817159188923,
1.20840932237519));
#63215=CARTESIAN_POINT('Ctrl Pts',(-34.3978691183489,-0.640240458638742,
1.23665911837698));
#63216=CARTESIAN_POINT('Ctrl Pts',(-34.3423539080722,-1.16129644075106,
0.464741691095696));
#63217=CARTESIAN_POINT('Ctrl Pts',(-34.3133532402014,-1.17949500306512,
0.0373805274982975));
#63218=CARTESIAN_POINT('Ctrl Pts',(-34.3108671147362,-1.17925499677644,
0.000722179416794018));
#63219=CARTESIAN_POINT('Ctrl Pts',(-34.8014778394209,0.850780204044596,
-1.19080027477568));
#63220=CARTESIAN_POINT('Ctrl Pts',(-34.7749632970152,1.24754481303337,-0.90732748580884));
#63221=CARTESIAN_POINT('Ctrl Pts',(-34.7219342122039,1.72847850304328,0.0825100069000186));
#63222=CARTESIAN_POINT('Ctrl Pts',(-34.6423905849868,0.863396232199179,
1.50159799897799));
#63223=CARTESIAN_POINT('Ctrl Pts',(-34.5628469577697,-0.795577933532765,
1.53670186350626));
#63224=CARTESIAN_POINT('Ctrl Pts',(-34.4833033305527,-1.72329896479418,
0.162331246392712));
#63225=CARTESIAN_POINT('Ctrl Pts',(-34.4037597033356,-1.06805600758911,
-1.36234908588761));
#63226=CARTESIAN_POINT('Ctrl Pts',(-34.3242160761186,0.568491528314387,
-1.63484710452143));
#63227=CARTESIAN_POINT('Ctrl Pts',(-34.2446724489015,1.68272306300853,-0.405770608944271));
#63228=CARTESIAN_POINT('Ctrl Pts',(-34.1651288216845,1.25109966684745,1.19625105692336));
#63229=CARTESIAN_POINT('Ctrl Pts',(-34.0855851944674,-0.329898722146615,
1.69921054064198));
#63230=CARTESIAN_POINT('Ctrl Pts',(-34.0060415672503,-1.60781789259073,
0.641187468103347));
#63231=CARTESIAN_POINT('Ctrl Pts',(-33.9264979400333,-1.40867154360034,
-1.00590667876807));
#63232=CARTESIAN_POINT('Ctrl Pts',(-33.8469543128162,0.0845950055721448,
-1.72888150200373));
#63233=CARTESIAN_POINT('Ctrl Pts',(-33.7674106855992,1.50014467527073,-0.863574913031011));
#63234=CARTESIAN_POINT('Ctrl Pts',(-33.6878670583821,1.53754245201339,0.795084121240462));
#63235=CARTESIAN_POINT('Ctrl Pts',(-33.608323431165,0.162430821126508,1.7233135521795));
#63236=CARTESIAN_POINT('Ctrl Pts',(-33.528779803948,-1.36190254265914,1.06837077475386));
#63237=CARTESIAN_POINT('Ctrl Pts',(-33.4492361767309,-1.63508373563369,
-0.568063115508245));
#63238=CARTESIAN_POINT('Ctrl Pts',(-33.3696925495139,-0.406146596378477,
-1.6826286527699));
#63239=CARTESIAN_POINT('Ctrl Pts',(-33.2901489222968,1.19590916357646,-1.25139750262871));
#63240=CARTESIAN_POINT('Ctrl Pts',(-33.2106052950798,1.69930742894605,0.329467246193458));
#63241=CARTESIAN_POINT('Ctrl Pts',(-33.1310616678627,0.641586397136989,
1.60765707275096));
#63242=CARTESIAN_POINT('Ctrl Pts',(-33.0515180406457,-1.00554704922936,
1.40892495536101));
#63243=CARTESIAN_POINT('Ctrl Pts',(-32.9719744134285,-1.72890480566619,
-0.0841579713322476));
#63244=CARTESIAN_POINT('Ctrl Pts',(-32.8924307862115,-0.863952760758447,
-1.49992666957161));
#63245=CARTESIAN_POINT('Ctrl Pts',(-32.8128871589944,0.794695172738762,
-1.53774314294755));
#63246=CARTESIAN_POINT('Ctrl Pts',(-32.7333435317774,1.72327275966808,-0.162866159028769));
#63247=CARTESIAN_POINT('Ctrl Pts',(-32.6537999045603,1.06871459261237,1.3616326630319));
#63248=CARTESIAN_POINT('Ctrl Pts',(-32.5742562773433,-0.567650007920692,
1.63522715811347));
#63249=CARTESIAN_POINT('Ctrl Pts',(-32.4947126501262,-1.68252605239498,
0.406571608589262));
#63250=CARTESIAN_POINT('Ctrl Pts',(-32.4151690229091,-1.25169951705268,
-1.1955930364733));
#63251=CARTESIAN_POINT('Ctrl Pts',(-32.3356253956921,0.329037992840854,
-1.69939059348022));
#63252=CARTESIAN_POINT('Ctrl Pts',(-32.256081768475,1.60749496826621,-0.641992458602764));
#63253=CARTESIAN_POINT('Ctrl Pts',(-32.176538141258,1.40917890001414,1.00519113488724));
#63254=CARTESIAN_POINT('Ctrl Pts',(-32.0969945140409,-0.0837212598430693,
1.72892600783361));
#63255=CARTESIAN_POINT('Ctrl Pts',(-32.0174508868239,-1.49970839530019,
0.864331602438092));
#63256=CARTESIAN_POINT('Ctrl Pts',(-31.9379072596068,-1.53794382684947,
-0.79430672624796));
#63257=CARTESIAN_POINT('Ctrl Pts',(-31.8583636323897,-0.163301438553533,
-1.72323156600474));
#63258=CARTESIAN_POINT('Ctrl Pts',(-31.7788200051727,1.36136267124702,-1.06905849570687));
#63259=CARTESIAN_POINT('Ctrl Pts',(-31.6992763779556,1.63537048958156,0.567236944947783));
#63260=CARTESIAN_POINT('Ctrl Pts',(-31.6197327507385,0.406996587841936,
1.68242330208339));
#63261=CARTESIAN_POINT('Ctrl Pts',(-31.5401891235215,-1.19527682939084,
1.2520014740524));
#63262=CARTESIAN_POINT('Ctrl Pts',(-31.4606454963044,-1.69947365153686,
-0.32860873031615));
#63263=CARTESIAN_POINT('Ctrl Pts',(-31.3811018690874,-0.642398478081434,
-1.60733275499092));
#63264=CARTESIAN_POINT('Ctrl Pts',(-31.3015582418703,1.0048351558706,-1.40943275803939));
#63265=CARTESIAN_POINT('Ctrl Pts',(-31.2220146146532,1.72894709997597,0.0832845447410718));
#63266=CARTESIAN_POINT('Ctrl Pts',(-31.1424709874362,0.86471038882106,1.49949002443263));
#63267=CARTESIAN_POINT('Ctrl Pts',(-31.0629273602191,-0.793918228999244,
1.5381444131065));
#63268=CARTESIAN_POINT('Ctrl Pts',(-30.9833837330021,-1.72319026243643,
0.163736707406421));
#63269=CARTESIAN_POINT('Ctrl Pts',(-30.903840105785,-1.06940233057072,-1.36109259247046));
#63270=CARTESIAN_POINT('Ctrl Pts',(-30.824296478568,0.566823845772114,-1.63551371677897));
#63271=CARTESIAN_POINT('Ctrl Pts',(-30.7447528513508,1.68232044443492,-0.407421541090209));
#63272=CARTESIAN_POINT('Ctrl Pts',(-30.6652092241339,1.252303351168,1.19496054602713));
#63273=CARTESIAN_POINT('Ctrl Pts',(-30.5856655969168,-0.328179446823656,
1.69955660117295));
#63274=CARTESIAN_POINT('Ctrl Pts',(-30.5061219696997,-1.60717043916454,
0.642804456568018));
#63275=CARTESIAN_POINT('Ctrl Pts',(-30.4265783424826,-1.40968652613872,
-1.00447911274003));
#63276=CARTESIAN_POINT('Ctrl Pts',(-30.3470347152656,0.0828478243250561,
-1.72896808180852));
#63277=CARTESIAN_POINT('Ctrl Pts',(-30.2674910880485,1.49927155789386,-0.865089120032475));
#63278=CARTESIAN_POINT('Ctrl Pts',(-30.1879474608315,1.53834490122586,0.793529681096073));
#63279=CARTESIAN_POINT('Ctrl Pts',(-30.1084038336144,0.164171965812518,
1.72314884892434));
#63280=CARTESIAN_POINT('Ctrl Pts',(-30.0288602063974,-1.36082242685268,
1.06974609720383));
#63281=CARTESIAN_POINT('Ctrl Pts',(-29.9493165791803,-1.63565683962635,
-0.566410710431554));
#63282=CARTESIAN_POINT('Ctrl Pts',(-29.8697729519632,-0.407846468343938,
-1.68221747945009));
#63283=CARTESIAN_POINT('Ctrl Pts',(-29.7902293247462,1.19464418642185,-1.25260514838337));
#63284=CARTESIAN_POINT('Ctrl Pts',(-29.7106856975292,1.69963944237293,0.327750142392453));
#63285=CARTESIAN_POINT('Ctrl Pts',(-29.631142070312,0.643210394042013,1.60700802079652));
#63286=CARTESIAN_POINT('Ctrl Pts',(-29.5515984430951,-1.00412300552109,
1.40994020429639));
#63287=CARTESIAN_POINT('Ctrl Pts',(-29.4720548158779,-1.72898895332844,
-0.0824110986231344));
#63288=CARTESIAN_POINT('Ctrl Pts',(-29.3925111886609,-0.865467796048966,
-1.49905299569768));
#63289=CARTESIAN_POINT('Ctrl Pts',(-29.3129675614438,0.793141082563654,
-1.53854529119483));
#63290=CARTESIAN_POINT('Ctrl Pts',(-29.2334239342268,1.7231073254709,-0.164607213744022));
#63291=CARTESIAN_POINT('Ctrl Pts',(-29.1538803070097,1.07008979558436,1.36055217441091));
#63292=CARTESIAN_POINT('Ctrl Pts',(-29.0743366797926,-0.565997538952522,
1.63579985811459));
#63293=CARTESIAN_POINT('Ctrl Pts',(-28.9947930525756,-1.68211440713543,
0.408271369576005));
#63294=CARTESIAN_POINT('Ctrl Pts',(-28.9152494253585,-1.2529068656793,-1.19432775059517));
#63295=CARTESIAN_POINT('Ctrl Pts',(-28.8357057981415,0.327320817049945,
-1.69972217513151));
#63296=CARTESIAN_POINT('Ctrl Pts',(-28.7561621709244,1.60684549989723,-0.643616290477521));
#63297=CARTESIAN_POINT('Ctrl Pts',(-28.6766185437074,1.41019379249622,1.00376683423649));
#63298=CARTESIAN_POINT('Ctrl Pts',(-28.5970749164902,-0.0819743676631687,
1.72900971453438));
#63299=CARTESIAN_POINT('Ctrl Pts',(-28.5175312892732,-1.49883433785804,
0.865846416846369));
#63300=CARTESIAN_POINT('Ctrl Pts',(-28.4379876620562,-1.53874558300063,
-0.79275243342678));
#63301=CARTESIAN_POINT('Ctrl Pts',(-28.3584440348391,-0.165042451173157,
-1.72306569207874));
#63302=CARTESIAN_POINT('Ctrl Pts',(-28.2789004076221,1.36028183516239,-1.0704334256904));
#63303=CARTESIAN_POINT('Ctrl Pts',(-28.199356780405,1.63594277223457,0.565584331361386));
#63304=CARTESIAN_POINT('Ctrl Pts',(-28.1198131531879,0.408696244759305,
1.68201122749751));
#63305=CARTESIAN_POINT('Ctrl Pts',(-28.0402695259709,-1.19401123856729,
1.25320850303652));
#63306=CARTESIAN_POINT('Ctrl Pts',(-27.9607258987538,-1.69980479944342,
-0.326891470823519));
#63307=CARTESIAN_POINT('Ctrl Pts',(-27.8811822715368,-0.644022145848643,
-1.60668287647704));
#63308=CARTESIAN_POINT('Ctrl Pts',(-27.8016386443197,1.00341059890898,-1.41044729072205));
#63309=CARTESIAN_POINT('Ctrl Pts',(-27.7220950171026,1.72903036542503,0.0815376314730298));
#63310=CARTESIAN_POINT('Ctrl Pts',(-27.6425513898856,0.866224982400531,
1.49861558438888));
#63311=CARTESIAN_POINT('Ctrl Pts',(-27.5630077626685,-0.79236373371025,
1.53894577663048));
#63312=CARTESIAN_POINT('Ctrl Pts',(-27.4834641354515,-1.72302394875053,
0.165477678072159));
#63313=CARTESIAN_POINT('Ctrl Pts',(-27.4039205082344,-1.07077698750001,
-1.36001140912437));
#63314=CARTESIAN_POINT('Ctrl Pts',(-27.3243768810173,0.565171087684503,
-1.63608558197716));
#63315=CARTESIAN_POINT('Ctrl Pts',(-27.2448332538003,1.68190794054292,-0.409121093866723));
#63316=CARTESIAN_POINT('Ctrl Pts',(-27.1652896265832,1.2535100604358,1.19369465035841));
#63317=CARTESIAN_POINT('Ctrl Pts',(-27.0857459993662,-0.326462103740574,
1.69988731530338));
#63318=CARTESIAN_POINT('Ctrl Pts',(-27.0062023721491,-1.60652015054632,
0.644427960129485));
#63319=CARTESIAN_POINT('Ctrl Pts',(-26.926658744932,-1.41070069895768,-1.00305429956127));
#63320=CARTESIAN_POINT('Ctrl Pts',(-26.847115117715,0.0811008900805756,
-1.72905090599906));
#63321=CARTESIAN_POINT('Ctrl Pts',(-26.7675714904979,1.49839673530418,-0.866603492687293));
#63322=CARTESIAN_POINT('Ctrl Pts',(-26.6880278632808,1.5391458720716,0.791974983438858));
#63323=CARTESIAN_POINT('Ctrl Pts',(-26.6084842360638,0.165912894413254,
1.72298209548894));
#63324=CARTESIAN_POINT('Ctrl Pts',(-26.5289406088467,-1.3597408963141,1.07112048099127));
#63325=CARTESIAN_POINT('Ctrl Pts',(-26.4493969816297,-1.63622828733326,
-0.56475780794824));
#63326=CARTESIAN_POINT('Ctrl Pts',(-26.3698533544126,-0.409545916871159,
-1.68180454627825));
#63327=CARTESIAN_POINT('Ctrl Pts',(-26.2903097271955,1.19337798598872,-1.25381153785789));
#63328=CARTESIAN_POINT('Ctrl Pts',(-26.2107660999785,1.69996972270612,0.326032715828498));
#63329=CARTESIAN_POINT('Ctrl Pts',(-26.1312224727614,0.644833733294154,
1.60635732211546));
#63330=CARTESIAN_POINT('Ctrl Pts',(-26.0516788455444,-1.0026979362161,1.41095401718695));
#63331=CARTESIAN_POINT('Ctrl Pts',(-25.9721352183273,-1.72907133625517,
-0.0806641435136772));
#63332=CARTESIAN_POINT('Ctrl Pts',(-25.8925915911103,-0.866981947682513,
-1.49817779061788));
#63333=CARTESIAN_POINT('Ctrl Pts',(-25.8130479638931,0.791586182637417,
-1.53934586931123));
#63334=CARTESIAN_POINT('Ctrl Pts',(-25.7335043366762,1.72294013229662,-0.166348100168679));
#63335=CARTESIAN_POINT('Ctrl Pts',(-25.653960709459,1.07146390614228,1.35947029674884));
#63336=CARTESIAN_POINT('Ctrl Pts',(-25.574417082242,-0.564344492178976,
1.63637088829376));
#63337=CARTESIAN_POINT('Ctrl Pts',(-25.4948734550249,-1.6817010447101,0.409970713745494));
#63338=CARTESIAN_POINT('Ctrl Pts',(-25.4153298278079,-1.25411293528354,
-1.19306124547843));
#63339=CARTESIAN_POINT('Ctrl Pts',(-25.3357862005908,0.325603307114701,
-1.7000520216464));
#63340=CARTESIAN_POINT('Ctrl Pts',(-25.2562425733738,1.60619439119485,-0.645239465316747));
#63341=CARTESIAN_POINT('Ctrl Pts',(-25.1766989461567,1.4112072453937,1.00234150889622));
#63342=CARTESIAN_POINT('Ctrl Pts',(-25.0971553189396,-0.0802273918002108,
1.72909165619205));
#63343=CARTESIAN_POINT('Ctrl Pts',(-25.0176116917226,-1.49795875034397,
0.867360347362028));
#63344=CARTESIAN_POINT('Ctrl Pts',(-24.9380680645055,-1.53954576833661,
-0.791197331330738));
#63345=CARTESIAN_POINT('Ctrl Pts',(-24.8585244372885,-0.166783295310653,
-1.72289805917627));
#63346=CARTESIAN_POINT('Ctrl Pts',(-24.7789808100714,1.35919961044586,-1.0718072629311));
#63347=CARTESIAN_POINT('Ctrl Pts',(-24.6994371828543,1.63651338484955,0.563931140403065));
#63348=CARTESIAN_POINT('Ctrl Pts',(-24.6198935556373,0.41039548446264,1.68159743584507));
#63349=CARTESIAN_POINT('Ctrl Pts',(-24.5403499284202,-1.19274442884774,
1.25441425269356));
#63350=CARTESIAN_POINT('Ctrl Pts',(-24.4608063012032,-1.70013421211895,
-0.325173877626586));
#63351=CARTESIAN_POINT('Ctrl Pts',(-24.3812626739861,-0.645645156171385,
-1.60603135779488));
#63352=CARTESIAN_POINT('Ctrl Pts',(-24.3017190467691,1.00198501762436,-1.41146038356177));
#63353=CARTESIAN_POINT('Ctrl Pts',(-24.222175419552,1.72911186580841,0.0797906349680398));
#63354=CARTESIAN_POINT('Ctrl Pts',(-24.142631792335,0.867738691701698,1.49773961449641));
#63355=CARTESIAN_POINT('Ctrl Pts',(-24.0630881651179,-0.790808429543632,
1.53974556913497));
#63356=CARTESIAN_POINT('Ctrl Pts',(-23.9835445379008,-1.72285587613056,
0.167218479811407));
#63357=CARTESIAN_POINT('Ctrl Pts',(-23.9040009106837,-1.07215055133584,
-1.35892883742244));
#63358=CARTESIAN_POINT('Ctrl Pts',(-23.8244572834667,0.563517752646911,
-1.63665577699155));
#63359=CARTESIAN_POINT('Ctrl Pts',(-23.7449136562497,1.68149371968977,-0.410820228995473));
#63360=CARTESIAN_POINT('Ctrl Pts',(-23.6653700290326,1.25471549006868,1.19242753611687));
#63361=CARTESIAN_POINT('Ctrl Pts',(-23.5858264018155,-0.324744427391516,
1.70021629411854));
#63362=CARTESIAN_POINT('Ctrl Pts',(-23.5062827745985,-1.60586822192594,
0.646050805832219));
#63363=CARTESIAN_POINT('Ctrl Pts',(-23.4267391473814,-1.41171343167502,
-1.00162846242325));
#63364=CARTESIAN_POINT('Ctrl Pts',(-23.3471955201644,0.079353873044988,
-1.72913196510295));
#63365=CARTESIAN_POINT('Ctrl Pts',(-23.2676518929473,1.49752038308919,-0.868116980677408));
#63366=CARTESIAN_POINT('Ctrl Pts',(-23.1881082657303,1.53994527169359,0.790419477300873));
#63367=CARTESIAN_POINT('Ctrl Pts',(-23.1085646385131,0.167653653643207,
1.72281358316218));
#63368=CARTESIAN_POINT('Ctrl Pts',(-23.0290210112961,-1.35865797769581,
1.07249377133462));
#63369=CARTESIAN_POINT('Ctrl Pts',(-22.9494773840791,-1.63679806471068,
-0.563104328936848));
#63370=CARTESIAN_POINT('Ctrl Pts',(-22.869933756862,-0.411244947316943,
-1.68138989625081));
#63371=CARTESIAN_POINT('Ctrl Pts',(-22.7903901296449,1.19211056730603,-1.25501664738972));
#63372=CARTESIAN_POINT('Ctrl Pts',(-22.7108465024279,1.70029826763994,0.324314956436899));
#63373=CARTESIAN_POINT('Ctrl Pts',(-22.6313028752108,0.646456414273326,
1.60570498359846));
#63374=CARTESIAN_POINT('Ctrl Pts',(-22.5517592479938,-1.00127184331565,
1.41196638971731));
#63375=CARTESIAN_POINT('Ctrl Pts',(-22.4722156207767,-1.7291519540744,-0.0789171060589664));
#63376=CARTESIAN_POINT('Ctrl Pts',(-22.3926719935596,-0.868495214265015,
-1.49730105613627));
#63377=CARTESIAN_POINT('Ctrl Pts',(-22.3131283663426,0.790030474627313,
-1.54014487599972));
#63378=CARTESIAN_POINT('Ctrl Pts',(-22.2335847391255,1.72277118027384,-0.168088816778282));
#63379=CARTESIAN_POINT('Ctrl Pts',(-22.1540411119085,1.07283692290551,1.3583870312833));
#63380=CARTESIAN_POINT('Ctrl Pts',(-22.0744974846914,-0.562690869299256,
1.63694024799786));
#63381=CARTESIAN_POINT('Ctrl Pts',(-21.9949538574743,-1.68128596553483,
0.411669639399906));
#63382=CARTESIAN_POINT('Ctrl Pts',(-21.9154102302573,-1.25531772463745,
-1.19179352243544));
#63383=CARTESIAN_POINT('Ctrl Pts',(-21.8358666030402,0.323885464790162,
-1.7003801326779));
#63384=CARTESIAN_POINT('Ctrl Pts',(-21.7563229758232,1.60554164282283,-0.646861981468851));
#63385=CARTESIAN_POINT('Ctrl Pts',(-21.6767793486061,1.41221925767248,1.00091516032431));
#63386=CARTESIAN_POINT('Ctrl Pts',(-21.5972357213891,-0.0784803340378172,
1.72917183272148));
#63387=CARTESIAN_POINT('Ctrl Pts',(-21.517692094172,-1.49708163365169,0.868873392440369));
#63388=CARTESIAN_POINT('Ctrl Pts',(-21.4381484669549,-1.54034438204061,
-0.789641421547753));
#63389=CARTESIAN_POINT('Ctrl Pts',(-21.3586048397378,-0.168523969188844,
-1.72272866746823));
#63390=CARTESIAN_POINT('Ctrl Pts',(-21.2790612125208,1.35811599820218,-1.07318000602664));
#63391=CARTESIAN_POINT('Ctrl Pts',(-21.1995175853037,1.63708232684401,0.562277373760544));
#63392=CARTESIAN_POINT('Ctrl Pts',(-21.1199739580867,0.412094305217296,
1.68118192754845));
#63393=CARTESIAN_POINT('Ctrl Pts',(-21.0404303308696,-1.19147640152535,
1.25561872179266));
#63394=CARTESIAN_POINT('Ctrl Pts',(-20.9608867036526,-1.7004618892272,-0.323455952478681));
#63395=CARTESIAN_POINT('Ctrl Pts',(-20.8813430764355,-0.647267507392897,
-1.6053781996095));
#63396=CARTESIAN_POINT('Ctrl Pts',(-20.8017994492184,1.00055841347199,-1.41247203552441));
#63397=CARTESIAN_POINT('Ctrl Pts',(-20.7222558220014,1.72919160104291,0.0780435570094322));
#63398=CARTESIAN_POINT('Ctrl Pts',(-20.6427121947843,0.869251515179363,
1.49686211564941));
#63399=CARTESIAN_POINT('Ctrl Pts',(-20.5631685675672,-0.789252318087039,
1.54054378980355));
#63400=CARTESIAN_POINT('Ctrl Pts',(-20.4836249403502,-1.72268604474808,
0.168959110847153));
#63401=CARTESIAN_POINT('Ctrl Pts',(-20.4040813131331,-1.0735230206761,-1.35784487846974));
#63402=CARTESIAN_POINT('Ctrl Pts',(-20.3245376859161,0.561863842347068,
-1.63722430124007));
#63403=CARTESIAN_POINT('Ctrl Pts',(-20.244994058699,1.68107778229831,-0.412518944741988));
#63404=CARTESIAN_POINT('Ctrl Pts',(-20.1654504314819,1.25591963883615,1.19115920459598));
#63405=CARTESIAN_POINT('Ctrl Pts',(-20.0859068042649,-0.323026419529885,
1.70054353728264));
#63406=CARTESIAN_POINT('Ctrl Pts',(-20.0063631770479,-1.60521465396887,
0.647672992019612));
#63407=CARTESIAN_POINT('Ctrl Pts',(-19.9268195498308,-1.41272472325696,
-1.00020160278146));
#63408=CARTESIAN_POINT('Ctrl Pts',(-19.8472759226137,0.0776067750016528,
-1.72921125903745));
#63409=CARTESIAN_POINT('Ctrl Pts',(-19.7677322953967,1.49664250214346,-0.869629582457851));
#63410=CARTESIAN_POINT('Ctrl Pts',(-19.6881886681796,1.5407430992758,0.788863164269974));
#63411=CARTESIAN_POINT('Ctrl Pts',(-19.6086450409625,0.16939424172542,1.72264331211609));
#63412=CARTESIAN_POINT('Ctrl Pts',(-19.5291014137455,-1.35757367210328,
1.07386596683201));
#63413=CARTESIAN_POINT('Ctrl Pts',(-19.4495577865284,-1.63736617117698,
-0.561450275085237));
#63414=CARTESIAN_POINT('Ctrl Pts',(-19.3700141593114,-0.412943557946916,
-1.68097352979105));
#63415=CARTESIAN_POINT('Ctrl Pts',(-19.2904705320943,1.19084193166757,-1.2562204757487));
#63416=CARTESIAN_POINT('Ctrl Pts',(-19.2109269048772,1.70062507683899,0.322596865971154));
#63417=CARTESIAN_POINT('Ctrl Pts',(-19.1313832776602,0.648078435323101,
1.6050510059114));
#63418=CARTESIAN_POINT('Ctrl Pts',(-19.0518396504431,-0.999844728275466,
1.41297732085402));
#63419=CARTESIAN_POINT('Ctrl Pts',(-18.9722960232261,-1.72923080670383,
-0.0771699880423723));
#63420=CARTESIAN_POINT('Ctrl Pts',(-18.892752396009,-0.870007594251728,
-1.49642279314783));
#63421=CARTESIAN_POINT('Ctrl Pts',(-18.8132087687919,0.788473960121406,
-1.54094231044465));
#63422=CARTESIAN_POINT('Ctrl Pts',(-18.7336651415749,1.72260046957501,-0.169829361795908));
#63423=CARTESIAN_POINT('Ctrl Pts',(-18.6541215143578,1.07420884447249,1.35730237912011));
#63424=CARTESIAN_POINT('Ctrl Pts',(-18.5745778871408,-0.561036672001411,
1.63750793664569));
#63425=CARTESIAN_POINT('Ctrl Pts',(-18.4950342599237,-1.68086917003333,
0.413368144804963));
#63426=CARTESIAN_POINT('Ctrl Pts',(-18.4154906327066,-1.25652123251115,
-1.19052458276035));
#63427=CARTESIAN_POINT('Ctrl Pts',(-18.3359470054896,0.32216729182992,-1.70070650789106));
#63428=CARTESIAN_POINT('Ctrl Pts',(-18.2564033782725,1.60488725544752,-0.648483837277519));
#63429=CARTESIAN_POINT('Ctrl Pts',(-18.1768597510555,1.41322982829946,0.999487789976802));
#63430=CARTESIAN_POINT('Ctrl Pts',(-18.0973161238384,-0.076733196159435,
1.72925024404081));
#63431=CARTESIAN_POINT('Ctrl Pts',(-18.0177724966213,-1.49620298867657,
0.870385550536859));
#63432=CARTESIAN_POINT('Ctrl Pts',(-17.9382288694043,-1.5411414232974,-0.788084705666147));
#63433=CARTESIAN_POINT('Ctrl Pts',(-17.8586852421872,-0.170264471030831,
-1.72255751712755));
#63434=CARTESIAN_POINT('Ctrl Pts',(-17.7791416149702,1.35703099953753,-1.07455165357568));
#63435=CARTESIAN_POINT('Ctrl Pts',(-17.6995979877531,1.63764959763715,0.560623033122007));
#63436=CARTESIAN_POINT('Ctrl Pts',(-17.6200543605361,0.413792705289065,
1.68076470303181));
#63437=CARTESIAN_POINT('Ctrl Pts',(-17.540510733319,-1.19020715789459,1.25682190910428));
#63438=CARTESIAN_POINT('Ctrl Pts',(-17.460967106102,-1.70078783043366,-0.321737697133566));
#63439=CARTESIAN_POINT('Ctrl Pts',(-17.3814234788849,-0.648889197856976,
-1.60472340258768));
#63440=CARTESIAN_POINT('Ctrl Pts',(-17.3018798516678,0.999130787908217,
-1.41348224557719));
#63441=CARTESIAN_POINT('Ctrl Pts',(-17.2223362244507,1.72926957104715,0.0762963993807335));
#63442=CARTESIAN_POINT('Ctrl Pts',(-17.1427925972337,0.870763451289146,
1.49598308874367));
#63443=CARTESIAN_POINT('Ctrl Pts',(-17.0632489700166,-0.787695400929053,
1.54134043782133));
#63444=CARTESIAN_POINT('Ctrl Pts',(-16.9837053427996,-1.72251445477646,
0.170699569402452));
#63445=CARTESIAN_POINT('Ctrl Pts',(-16.9041617155825,-1.07489439411967,
-1.35675953337286));
#63446=CARTESIAN_POINT('Ctrl Pts',(-16.8246180883654,0.560209358473387,
-1.63779115414233));
#63447=CARTESIAN_POINT('Ctrl Pts',(-16.7450744611484,1.68066012879314,-0.41421723937211));
#63448=CARTESIAN_POINT('Ctrl Pts',(-16.6655308339313,1.25712250550892,1.18988965709052));
#63449=CARTESIAN_POINT('Ctrl Pts',(-16.5859872067143,-0.321308081909528,
1.70086904446158));
#63450=CARTESIAN_POINT('Ctrl Pts',(-16.5064435794972,-1.60455944734232,
0.649294517035638));
#63451=CARTESIAN_POINT('Ctrl Pts',(-16.4268999522802,-1.41373457267109,
-0.998773722092515));
#63452=CARTESIAN_POINT('Ctrl Pts',(-16.3473563250631,0.0758595977341116,
-1.7292887877216));
#63453=CARTESIAN_POINT('Ctrl Pts',(-16.267812697846,1.49576309336319,-0.871141296484464));
#63454=CARTESIAN_POINT('Ctrl Pts',(-16.188269070629,1.54153935400376,0.787306045934945));
#63455=CARTESIAN_POINT('Ctrl Pts',(-16.1087254434119,0.171134656882987,
1.72247128252449));
#63456=CARTESIAN_POINT('Ctrl Pts',(-16.0291818161949,-1.35648798064341,
1.07523706608263));
#63457=CARTESIAN_POINT('Ctrl Pts',(-15.9496381889778,-1.63793260615219,
-0.559795648081974));
#63458=CARTESIAN_POINT('Ctrl Pts',(-15.8700945617607,-0.414641747027034,
-1.68055544732401));
#63459=CARTESIAN_POINT('Ctrl Pts',(-15.7905509345437,1.18957208036842,-1.25742302170589));
#63460=CARTESIAN_POINT('Ctrl Pts',(-15.7110073073266,1.70095014996966,0.320878446185189));
#63461=CARTESIAN_POINT('Ctrl Pts',(-15.6314636801096,0.649699794787615,
1.60439538972193));
#63462=CARTESIAN_POINT('Ctrl Pts',(-15.5519200528925,-0.998416592552452,
1.41398680956506));
#63463=CARTESIAN_POINT('Ctrl Pts',(-15.4723764256755,-1.72930789406296,
-0.0754227912474636));
#63464=CARTESIAN_POINT('Ctrl Pts',(-15.3928327984584,-0.871519086098719,
-1.49554300254914));
#63465=CARTESIAN_POINT('Ctrl Pts',(-15.3132891712414,0.786916640708664,
-1.54173817183197));
#63466=CARTESIAN_POINT('Ctrl Pts',(-15.2337455440242,1.72242800037439,-0.171569733444734));
#63467=CARTESIAN_POINT('Ctrl Pts',(-15.1542019168073,1.07557966944271,1.35621634136652));
#63468=CARTESIAN_POINT('Ctrl Pts',(-15.0746582895901,-0.559381901974127,
1.63807395365773));
#63469=CARTESIAN_POINT('Ctrl Pts',(-14.9951146623731,-1.68045065863108,
0.41506622822674));
#63470=CARTESIAN_POINT('Ctrl Pts',(-14.915571035156,-1.25772345767604,-1.18925442774851));
#63471=CARTESIAN_POINT('Ctrl Pts',(-14.836027407939,0.320448789987955,-1.70103114695273));
#63472=CARTESIAN_POINT('Ctrl Pts',(-14.7564837807219,1.60423122973695,-0.65010503108709));
#63473=CARTESIAN_POINT('Ctrl Pts',(-14.6769401535048,1.41423895624302,0.998059399310818));
#63474=CARTESIAN_POINT('Ctrl Pts',(-14.5973965262878,-0.0749859799485997,
1.72932689006999));
#63475=CARTESIAN_POINT('Ctrl Pts',(-14.5178528990708,-1.49532281631557,
0.871896820107827));
#63476=CARTESIAN_POINT('Ctrl Pts',(-14.4383092718537,-1.54193689129333,
-0.786527185275081));
#63477=CARTESIAN_POINT('Ctrl Pts',(-14.3587656446366,-0.172004799059819,
-1.72238460832893));
#63478=CARTESIAN_POINT('Ctrl Pts',(-14.2792220174195,1.3559446155595,-1.07592220417798));
#63479=CARTESIAN_POINT('Ctrl Pts',(-14.1996783902025,1.6382151966499,0.558968120176268));
#63480=CARTESIAN_POINT('Ctrl Pts',(-14.1201347629854,0.415490682944149,
1.68034576272107));
#63481=CARTESIAN_POINT('Ctrl Pts',(-14.0405911357684,-1.18893669925114,
1.25802381340014));
#63482=CARTESIAN_POINT('Ctrl Pts',(-13.9610475085513,-1.70111203540558,
-0.320019113345276));
#63483=CARTESIAN_POINT('Ctrl Pts',(-13.8815038813343,-0.650510225908176,
-1.60406696739786));
#63484=CARTESIAN_POINT('Ctrl Pts',(-13.8019602541172,0.99770214239043,-1.41449101268888));
#63485=CARTESIAN_POINT('Ctrl Pts',(-13.7224166269001,1.7293457757415,0.0745491638655046));
#63486=CARTESIAN_POINT('Ctrl Pts',(-13.6428729996831,0.872274498487625,
1.49510253467652));
#63487=CARTESIAN_POINT('Ctrl Pts',(-13.563329372466,-0.786137679659009,
1.5421355123751));
#63488=CARTESIAN_POINT('Ctrl Pts',(-13.4837857452489,-1.72234110639089,
0.172439853700588));
#63489=CARTESIAN_POINT('Ctrl Pts',(-13.4042421180319,-1.07626467026662,
-1.35567280323974));
#63490=CARTESIAN_POINT('Ctrl Pts',(-13.3246984908148,0.558554302714798,
-1.63835633511968));
#63491=CARTESIAN_POINT('Ctrl Pts',(-13.2451548635978,1.68024075960064,-0.415915111152186));
#63492=CARTESIAN_POINT('Ctrl Pts',(-13.1656112363807,1.25832408885909,1.18861889489651));
#63493=CARTESIAN_POINT('Ctrl Pts',(-13.0860676091637,-0.319589416284583,
1.70119281532309));
#63494=CARTESIAN_POINT('Ctrl Pts',(-13.0065239819466,-1.60390260271513,
0.650915379225009));
#63495=CARTESIAN_POINT('Ctrl Pts',(-12.9269803547296,-1.41474297888655,
-0.997344821814044));
#63496=CARTESIAN_POINT('Ctrl Pts',(-12.8474367275125,0.074112343025946,
-1.72936455107628));
#63497=CARTESIAN_POINT('Ctrl Pts',(-12.7678931002954,1.4948821576461,-0.872652121214035));
#63498=CARTESIAN_POINT('Ctrl Pts',(-12.6883494730784,1.54233403506462,0.785748123885319));
#63499=CARTESIAN_POINT('Ctrl Pts',(-12.6088058458613,0.172874897339258,
1.72229749456301));
#63500=CARTESIAN_POINT('Ctrl Pts',(-12.5292622186442,-1.35540090442454,
1.07660706768682));
#63501=CARTESIAN_POINT('Ctrl Pts',(-12.4497185914272,-1.63849736905809,
-0.558140449616154));
#63502=CARTESIAN_POINT('Ctrl Pts',(-12.3701749642101,-0.416339512823747,
-1.68013564927648));
#63503=CARTESIAN_POINT('Ctrl Pts',(-12.2906313369931,1.18830101470491,-1.2586242840337));
#63504=CARTESIAN_POINT('Ctrl Pts',(-12.211087709776,1.70127348670011,0.319159698833231));
#63505=CARTESIAN_POINT('Ctrl Pts',(-12.1315440825589,0.651320491011731,
1.60373813569929));
#63506=CARTESIAN_POINT('Ctrl Pts',(-12.0520004553419,-0.996987437604471,
1.41499485481993));
#63507=CARTESIAN_POINT('Ctrl Pts',(-11.9724568281248,-1.72938321607311,
-0.0736755174578175));
#63508=CARTESIAN_POINT('Ctrl Pts',(-11.8929132009078,-0.873029688263015,
-1.49466168523832));
#63509=CARTESIAN_POINT('Ctrl Pts',(-11.8133695736907,0.785358517978902,
-1.54253245934923));
#63510=CARTESIAN_POINT('Ctrl Pts',(-11.7338259464736,1.72225377284807,-0.173309929948049));
#63511=CARTESIAN_POINT('Ctrl Pts',(-11.6542823192566,1.0769493964167,1.35512891913123));
#63512=CARTESIAN_POINT('Ctrl Pts',(-11.5747386920395,-0.557726560906682,
1.63863829845615));
#63513=CARTESIAN_POINT('Ctrl Pts',(-11.4951950648225,-1.68003043175534,
0.41676388793174));
#63514=CARTESIAN_POINT('Ctrl Pts',(-11.4156514376054,-1.25892439890481,
-1.18798305869662));
#63515=CARTESIAN_POINT('Ctrl Pts',(-11.3361078103884,0.31872996101865,-1.70135404953147));
#63516=CARTESIAN_POINT('Ctrl Pts',(-11.2565641831713,1.60357356636082,-0.651725561242555));
#63517=CARTESIAN_POINT('Ctrl Pts',(-11.1770205559542,1.41524664047297,0.996629989784558));
#63518=CARTESIAN_POINT('Ctrl Pts',(-11.0974769287371,-0.073238687189009,
1.7294017707308));
#63519=CARTESIAN_POINT('Ctrl Pts',(-11.0179333015201,-1.49444111746723,
0.873407199610443));
#63520=CARTESIAN_POINT('Ctrl Pts',(-10.938389674303,-1.54273078521631,-0.784968861964558));
#63521=CARTESIAN_POINT('Ctrl Pts',(-10.858846047086,-0.173744951499187,
-1.7222099412489));
#63522=CARTESIAN_POINT('Ctrl Pts',(-10.7793024198689,1.35485684737718,-1.0772916564344));
#63523=CARTESIAN_POINT('Ctrl Pts',(-10.6997587926519,1.63877912330483,0.557312636612794));
#63524=CARTESIAN_POINT('Ctrl Pts',(-10.6202151654348,0.417188236449154,
1.67992510704391));
#63525=CARTESIAN_POINT('Ctrl Pts',(-10.5406715382178,-1.18766502689197,
1.25922443345327));
#63526=CARTESIAN_POINT('Ctrl Pts',(-10.4611279110007,-1.70143450381201,
-0.318300202868278));
#63527=CARTESIAN_POINT('Ctrl Pts',(-10.3815842837836,-0.652130589891605,
-1.60340889471017));
#63528=CARTESIAN_POINT('Ctrl Pts',(-10.3020406565666,0.996272478377053,
-1.41549833582965));
#63529=CARTESIAN_POINT('Ctrl Pts',(-10.2224970293495,1.7294202150482,0.0728018522474178));
#63530=CARTESIAN_POINT('Ctrl Pts',(-10.1429534021325,0.87378465523221,1.49422045434693));
#63531=CARTESIAN_POINT('Ctrl Pts',(-10.0634097749154,-0.784579155867149,
1.54292901265316));
#63532=CARTESIAN_POINT('Ctrl Pts',(-9.98386614769833,-1.7221659997683,0.17417996196498));
#63533=CARTESIAN_POINT('Ctrl Pts',(-9.90432252048128,-1.07763384771809,
-1.35458468917979));
#63534=CARTESIAN_POINT('Ctrl Pts',(-9.82477889326421,0.55689867676092,-1.63891984359515));
#63535=CARTESIAN_POINT('Ctrl Pts',(-9.74523526604717,1.6798196751489,-0.417612558348886));
#63536=CARTESIAN_POINT('Ctrl Pts',(-9.66569163883009,1.25952438765999,1.1873469193112));
#63537=CARTESIAN_POINT('Ctrl Pts',(-9.58614801161304,-0.317870424409565,
1.70151484953664));
#63538=CARTESIAN_POINT('Ctrl Pts',(-9.50660438439598,-1.60324412075788,
0.652535576933021));
#63539=CARTESIAN_POINT('Ctrl Pts',(-9.42706075717891,-1.41574994087386,
-0.995914903404769));
#63540=CARTESIAN_POINT('Ctrl Pts',(-9.34751712996185,0.072365012660848,
-1.72943854902412));
#63541=CARTESIAN_POINT('Ctrl Pts',(-9.26797350274479,1.49399969589152,-0.874162055104235));
#63542=CARTESIAN_POINT('Ctrl Pts',(-9.18842987552774,1.54312714164713,0.784189399711559));
#63543=CARTESIAN_POINT('Ctrl Pts',(-9.10888624831068,0.17461496131765,1.72212194840903));
#63544=CARTESIAN_POINT('Ctrl Pts',(-9.02934262109362,-1.35431244455638,
1.07797597024599));
#63545=CARTESIAN_POINT('Ctrl Pts',(-8.94979899387657,-1.63906045931814,
-0.556484681377506));
#63546=CARTESIAN_POINT('Ctrl Pts',(-8.87025536665949,-0.41803685360384,
-1.67971413607703));
#63547=CARTESIAN_POINT('Ctrl Pts',(-8.79071173944245,1.18702873597461,-1.25982426150579));
#63548=CARTESIAN_POINT('Ctrl Pts',(-8.71116811222537,1.70159508670024,0.317440625669869));
#63549=CARTESIAN_POINT('Ctrl Pts',(-8.63162448500832,0.652940522340951,
1.60307924451448));
#63550=CARTESIAN_POINT('Ctrl Pts',(-8.55208085779126,-0.99555726489053,
1.41600145558954));
#63551=CARTESIAN_POINT('Ctrl Pts',(-8.47253723057421,-1.72945677265738,
-0.0719281684571926));
#63552=CARTESIAN_POINT('Ctrl Pts',(-8.39299360335713,-0.874539399202495,
-1.49377884211506));
#63553=CARTESIAN_POINT('Ctrl Pts',(-8.31344997614009,0.783799593522696,
-1.54332517218559));
#63554=CARTESIAN_POINT('Ctrl Pts',(-8.23390634892302,1.7220777871739,-0.175049949529422));
#63555=CARTESIAN_POINT('Ctrl Pts',(-8.15436272170597,1.07831802399623,1.35404011352432));
#63556=CARTESIAN_POINT('Ctrl Pts',(-8.07481909448889,-0.556070650488905,
1.63920097046485));
#63557=CARTESIAN_POINT('Ctrl Pts',(-7.99527546727185,-1.67960848983507,
0.418461122186932));
#63558=CARTESIAN_POINT('Ctrl Pts',(-7.91573184005478,-1.26012405497151,
-1.1867104769025));
#63559=CARTESIAN_POINT('Ctrl Pts',(-7.83618821283773,0.317010806676624,
-1.70167521529765));
#63560=CARTESIAN_POINT('Ctrl Pts',(-7.75664458562067,1.60291426599049,-0.653345426089623));
#63561=CARTESIAN_POINT('Ctrl Pts',(-7.67710095840361,1.41625287996065,0.9951995628572));
#63562=CARTESIAN_POINT('Ctrl Pts',(-7.59755733118654,-0.0714913196643404,
1.72947488594679));
#63563=CARTESIAN_POINT('Ctrl Pts',(-7.5180137039695,-1.49355789303162,0.874916687502879));
#63564=CARTESIAN_POINT('Ctrl Pts',(-7.43847007675241,-1.54352310425593,
-0.783409737325367));
#63565=CARTESIAN_POINT('Ctrl Pts',(-7.35892644953538,-0.175484926572522,
-1.72203351606577));
#63566=CARTESIAN_POINT('Ctrl Pts',(-7.27938282231829,1.35376769610098,-1.07866000894696));
#63567=CARTESIAN_POINT('Ctrl Pts',(-7.19983919510126,1.63934137702629,0.555656584121541));
#63568=CARTESIAN_POINT('Ctrl Pts',(-7.12029556788418,0.418885364071158,
1.67950273642976));
#63569=CARTESIAN_POINT('Ctrl Pts',(-7.04075194066713,-1.18639214211523,
1.26042376803805));
#63570=CARTESIAN_POINT('Ctrl Pts',(-6.96120831345007,-1.70175523532376,
-0.316580967457275));
#63571=CARTESIAN_POINT('Ctrl Pts',(-6.88166468623301,-0.65375028815317,
-1.6027491851964));
#63572=CARTESIAN_POINT('Ctrl Pts',(-6.80212105901595,0.994841797327544,
-1.4165042139712));
#63573=CARTESIAN_POINT('Ctrl Pts',(-6.72257743179888,1.72949288889124,0.0710544663101945));
#63574=CARTESIAN_POINT('Ctrl Pts',(-6.64303380458183,0.875293919981295,
1.49333684865531));
#63575=CARTESIAN_POINT('Ctrl Pts',(-6.56349017736477,-0.78301983114445,
1.5437209378455));
#63576=CARTESIAN_POINT('Ctrl Pts',(-6.48394655014771,-1.72198913508746,
0.175919892419264));
#63577=CARTESIAN_POINT('Ctrl Pts',(-6.40440292293067,-1.07900192507638,
-1.35349519230379));
#63578=CARTESIAN_POINT('Ctrl Pts',(-6.32485929571358,0.555242482301849,
-1.63948167899348));
#63579=CARTESIAN_POINT('Ctrl Pts',(-6.24531566849655,1.6793968758678,-0.41930957922942));
#63580=CARTESIAN_POINT('Ctrl Pts',(-6.16577204127946,1.26072340068632,1.18607373163306));
#63581=CARTESIAN_POINT('Ctrl Pts',(-6.08622841406243,-0.316151108039277,
1.70183514677349));
#63582=CARTESIAN_POINT('Ctrl Pts',(-6.00668478684534,-1.60258400214274,
0.654155108505738));
#63583=CARTESIAN_POINT('Ctrl Pts',(-5.9271411596283,-1.41675545760511,-0.994483968324387));
#63584=CARTESIAN_POINT('Ctrl Pts',(-5.84759753241123,0.0706176084225559,
-1.72951078148959));
#63585=CARTESIAN_POINT('Ctrl Pts',(-5.76805390519418,1.49311570900028,-0.875671096613672));
#63586=CARTESIAN_POINT('Ctrl Pts',(-5.68851027797711,1.54391867294165,0.782629875004844));
#63587=CARTESIAN_POINT('Ctrl Pts',(-5.60896665076006,0.176354847041871,
1.72194464424177));
#63588=CARTESIAN_POINT('Ctrl Pts',(-5.529423023543,-1.3532226021501,1.07934377236272));
#63589=CARTESIAN_POINT('Ctrl Pts',(-5.44987939632593,-1.63962187635751,
-0.554828345056291));
#63590=CARTESIAN_POINT('Ctrl Pts',(-5.37033576910888,-0.41973376763463,
-1.67929090815595));
#63591=CARTESIAN_POINT('Ctrl Pts',(-5.29079214189181,1.1857552454763,-1.26102295289718));
#63592=CARTESIAN_POINT('Ctrl Pts',(-5.21124851467476,1.70191494964176,0.315721228449992));
#63593=CARTESIAN_POINT('Ctrl Pts',(-5.13170488745769,0.654559887121492,
1.60241871684011));
#63594=CARTESIAN_POINT('Ctrl Pts',(-5.05216126024064,-0.994126075870575,
1.41700661084632));
#63595=CARTESIAN_POINT('Ctrl Pts',(-4.97261763302358,-1.72952856374066,
-0.0701807460293178));
#63596=CARTESIAN_POINT('Ctrl Pts',(-4.89307400580652,-0.876048217376002,
-1.4928944740806));
#63597=CARTESIAN_POINT('Ctrl Pts',(-4.81353037858946,0.78223986893146,-1.5441163095318));
#63598=CARTESIAN_POINT('Ctrl Pts',(-4.7339867513724,1.72190004353153,-0.17678979041257));
#63599=CARTESIAN_POINT('Ctrl Pts',(-4.65444312415534,1.07968555078413,1.35294992565728));
#63600=CARTESIAN_POINT('Ctrl Pts',(-4.57489949693828,-0.554414172411219,
1.63976196910943));
#63601=CARTESIAN_POINT('Ctrl Pts',(-4.49535586972122,-1.67918483330103,
0.420157929259712));
#63602=CARTESIAN_POINT('Ctrl Pts',(-4.41581224250417,-1.26132242465148,
-1.18543668366527));
#63603=CARTESIAN_POINT('Ctrl Pts',(-4.3362686152871,0.315291328716861,-1.70199464392343));
#63604=CARTESIAN_POINT('Ctrl Pts',(-4.25672498807005,1.60225332929902,-0.654964623974668));
#63605=CARTESIAN_POINT('Ctrl Pts',(-4.17718136085298,1.41725767367884,0.993768119988983));
#63606=CARTESIAN_POINT('Ctrl Pts',(-4.09763773363593,-0.0697438791584081,
1.72954623564333));
#63607=CARTESIAN_POINT('Ctrl Pts',(-4.01809410641886,-1.49267314391039,
0.876425282244154));
#63608=CARTESIAN_POINT('Ctrl Pts',(-3.93855047920181,-1.54431384760333,
-0.781849812949146));
#63609=CARTESIAN_POINT('Ctrl Pts',(-3.85900685198474,-0.177224722503594,
-1.72185533295964));
#63610=CARTESIAN_POINT('Ctrl Pts',(-3.77946322476768,1.35267716284278,-1.08002726031877));
#63611=CARTESIAN_POINT('Ctrl Pts',(-3.69991959755063,1.63990195724028,0.553999964393108));
#63612=CARTESIAN_POINT('Ctrl Pts',(-3.62037597033356,0.420582064077634,
1.67907865130977));
#63613=CARTESIAN_POINT('Ctrl Pts',(-3.54083234311651,-1.18511804622036,
1.26162181593013));
#63614=CARTESIAN_POINT('Ctrl Pts',(-3.46128871589944,-1.70207422961342,
-0.314861408867349));
#63615=CARTESIAN_POINT('Ctrl Pts',(-3.38174508868239,-0.655369319039388,
-1.60208783953004));
#63616=CARTESIAN_POINT('Ctrl Pts',(-3.30220146146532,0.99341010070244,-1.4175086460866));
#63617=CARTESIAN_POINT('Ctrl Pts',(-3.22265783424827,1.7295637971964,0.0693070078375217));
#63618=CARTESIAN_POINT('Ctrl Pts',(-3.1431142070312,0.87680229119424,1.49245171850394));
#63619=CARTESIAN_POINT('Ctrl Pts',(-3.06357057981415,-0.781459707082962,
1.54451128714328));
#63620=CARTESIAN_POINT('Ctrl Pts',(-2.98402695259708,-1.72181051252855,
0.177659643287937));
#63621=CARTESIAN_POINT('Ctrl Pts',(-2.90448332538003,-1.08036890094558,
-1.3524043137253));
#63622=CARTESIAN_POINT('Ctrl Pts',(-2.82493969816297,0.553585721029618,
-1.64004184073856));
#63623=CARTESIAN_POINT('Ctrl Pts',(-2.74539607094591,1.6789723621865,-0.421006172066271));
#63624=CARTESIAN_POINT('Ctrl Pts',(-2.66585244372885,1.26192112671868,1.18479933317116));
#63625=CARTESIAN_POINT('Ctrl Pts',(-2.58630881651179,-0.31443146893764,
1.70215370668898));
#63626=CARTESIAN_POINT('Ctrl Pts',(-2.50676518929473,-1.60192224752698,
0.655773972323425));
#63627=CARTESIAN_POINT('Ctrl Pts',(-2.42722156207767,-1.4177595280854,-0.993052018097407));
#63628=CARTESIAN_POINT('Ctrl Pts',(-2.34767793486061,0.068870132154922,
-1.729581248278));
#63629=CARTESIAN_POINT('Ctrl Pts',(-2.26813430764355,1.49223019776091,-0.877179244431392));
#63630=CARTESIAN_POINT('Ctrl Pts',(-2.1885906804265,1.54470862835635,0.781069551792904));
#63631=CARTESIAN_POINT('Ctrl Pts',(-2.10904705320943,0.178094552325416,
1.7217655814153));
#63632=CARTESIAN_POINT('Ctrl Pts',(-2.02950342599238,-1.35213137753944,
1.08071047421022));
#63633=CARTESIAN_POINT('Ctrl Pts',(-1.94995979877531,-1.64018162108127,
-0.553171445322414));
#63634=CARTESIAN_POINT('Ctrl Pts',(-1.87041617155825,-0.421430250378147,
-1.67886596029095));
#63635=CARTESIAN_POINT('Ctrl Pts',(-1.79087254434119,1.18448053918477,-1.2622203677164));
#63636=CARTESIAN_POINT('Ctrl Pts',(-1.71132891712414,1.70223308530569,0.314001529299059));
#63637=CARTESIAN_POINT('Ctrl Pts',(-1.63178528990707,0.656178564515644,
1.60175651468699));
#63638=CARTESIAN_POINT('Ctrl Pts',(-1.55224166269002,-0.992693835592505,
1.41801039294902));
#63639=CARTESIAN_POINT('Ctrl Pts',(-1.47269803547296,-1.72959865836334,
-0.0684333912455062));
#63640=CARTESIAN_POINT('Ctrl Pts',(-1.3931544082559,-0.877556010062709,
-1.49200831766453));
#63641=CARTESIAN_POINT('Ctrl Pts',(-1.31361078103884,0.780679096811435,
-1.54490637237138));
#63642=CARTESIAN_POINT('Ctrl Pts',(-1.23406715382177,1.72172101468799,-0.178528498401339));
#63643=CARTESIAN_POINT('Ctrl Pts',(-1.15452352660472,1.0810510783977,1.35185654891102));
#63644=CARTESIAN_POINT('Ctrl Pts',(-1.07497989938766,-0.552755425847358,
1.64032472496632));
#63645=CARTESIAN_POINT('Ctrl Pts',(-0.995436272170598,-1.67876269403335,
0.421847794956357));
#63646=CARTESIAN_POINT('Ctrl Pts',(-0.915892644953538,-1.26251337329806,
-1.18414931936237));
#63647=CARTESIAN_POINT('Ctrl Pts',(-0.83634901773648,0.313559887373977,
-1.70233579666472));
#63648=CARTESIAN_POINT('Ctrl Pts',(-0.756805390519419,1.60161285332412,
-0.656538621811975));
#63649=CARTESIAN_POINT('Ctrl Pts',(-0.677261763302361,1.4182190784154,0.992251136832745));
#63650=CARTESIAN_POINT('Ctrl Pts',(-0.597718136085304,-0.0679167392546382,
1.7297762814003));
#63651=CARTESIAN_POINT('Ctrl Pts',(-0.518174508868237,-1.49193817974258,
0.877628180633763));
#63652=CARTESIAN_POINT('Ctrl Pts',(-0.438630881651179,-1.54481437551655,
-0.779708542229249));
#63653=CARTESIAN_POINT('Ctrl Pts',(-0.35908725443412,-0.179524439481945,
-1.72279441023562));
#63654=CARTESIAN_POINT('Ctrl Pts',(-0.279543627217061,1.35275091771125,
-1.07912501192066));
#63655=CARTESIAN_POINT('Ctrl Pts',(-0.226514542405688,1.54259118067785,
0.00486583246666068));
#63656=CARTESIAN_POINT('Ctrl Pts',(-0.2,1.38699088616441,0.466999498604503));
#63657=CARTESIAN_POINT('Ctrl Pts',(-34.7464852262806,0.795408277542816,
-1.1132985828233));
#63658=CARTESIAN_POINT('Ctrl Pts',(-34.7199706838749,1.16634997638047,-0.848275252789927));
#63659=CARTESIAN_POINT('Ctrl Pts',(-34.6669415990635,1.61598272073042,0.0771399500791215));
#63660=CARTESIAN_POINT('Ctrl Pts',(-34.5873979718465,0.807203207862427,
1.40386844011039));
#63661=CARTESIAN_POINT('Ctrl Pts',(-34.5078543446295,-0.743798775234758,
1.43668761512983));
#63662=CARTESIAN_POINT('Ctrl Pts',(-34.4283107174123,-1.61114028601272,
0.151766127691824));
#63663=CARTESIAN_POINT('Ctrl Pts',(-34.3487670901953,-0.998542967122596,
-1.2736823619854));
#63664=CARTESIAN_POINT('Ctrl Pts',(-34.2692234629782,0.531491994271277,
-1.52844520038366));
#63665=CARTESIAN_POINT('Ctrl Pts',(-34.1896798357612,1.57320521418612,-0.379361554962864));
#63666=CARTESIAN_POINT('Ctrl Pts',(-34.1101362085441,1.16967346714324,1.11839460788198));
#63667=CARTESIAN_POINT('Ctrl Pts',(-34.0305925813271,-0.308427691545578,
1.58861962571467));
#63668=CARTESIAN_POINT('Ctrl Pts',(-33.95104895411,-1.50317514966669,0.599456613073146));
#63669=CARTESIAN_POINT('Ctrl Pts',(-33.8715053268929,-1.31698998259737,
-0.940438546788035));
#63670=CARTESIAN_POINT('Ctrl Pts',(-33.7919616996759,0.0790892493159759,
-1.61635949102604));
#63671=CARTESIAN_POINT('Ctrl Pts',(-33.7124180724588,1.40250970409232,-0.807370259483987));
#63672=CARTESIAN_POINT('Ctrl Pts',(-33.6328744452418,1.43747349502384,0.743337102075247));
#63673=CARTESIAN_POINT('Ctrl Pts',(-33.5533308180247,0.151859221733174,
1.61115392399698));
#63674=CARTESIAN_POINT('Ctrl Pts',(-33.4737871908077,-1.27326488144399,
0.998837248074543));
#63675=CARTESIAN_POINT('Ctrl Pts',(-33.3942435635906,-1.52866643066679,
-0.531091464157164));
#63676=CARTESIAN_POINT('Ctrl Pts',(-33.3146999363736,-0.379713071742401,
-1.57311694851546));
#63677=CARTESIAN_POINT('Ctrl Pts',(-33.2351563091565,1.11807496622028,-1.16995191866883));
#63678=CARTESIAN_POINT('Ctrl Pts',(-33.1556126819394,1.58871020816909,0.308024297645402));
#63679=CARTESIAN_POINT('Ctrl Pts',(-33.0760690547224,0.599829578327863,
1.50302479657768));
#63680=CARTESIAN_POINT('Ctrl Pts',(-32.9965254275053,-0.940102323271568,
1.31722690138216));
#63681=CARTESIAN_POINT('Ctrl Pts',(-32.9169818002883,-1.61638127799984,
-0.0786806588829465));
#63682=CARTESIAN_POINT('Ctrl Pts',(-32.8374381730712,-0.807723515481981,
-1.40230588701147));
#63683=CARTESIAN_POINT('Ctrl Pts',(-32.7578945458541,0.742973467782488,
-1.43766112424875));
#63684=CARTESIAN_POINT('Ctrl Pts',(-32.678350918637,1.61111578641328,-0.152266226232503));
#63685=CARTESIAN_POINT('Ctrl Pts',(-32.59880729142,0.999158688993503,1.27301256658237));
#63686=CARTESIAN_POINT('Ctrl Pts',(-32.5192636642029,-0.530705243141331,
1.52880051868043));
#63687=CARTESIAN_POINT('Ctrl Pts',(-32.4397200369859,-1.57302102575292,
0.380110422584496));
#63688=CARTESIAN_POINT('Ctrl Pts',(-32.3601764097688,-1.1702342768756,-1.11777941383975));
#63689=CARTESIAN_POINT('Ctrl Pts',(-32.2806327825518,0.307622981690703,
-1.58878796004738));
#63690=CARTESIAN_POINT('Ctrl Pts',(-32.2010891553347,1.50287324245315,-0.60020921180962));
#63691=CARTESIAN_POINT('Ctrl Pts',(-32.1215455281177,1.3174643183768,0.939769573152954));
#63692=CARTESIAN_POINT('Ctrl Pts',(-32.0420019009006,-0.0782723701948242,
1.61640110025169));
#63693=CARTESIAN_POINT('Ctrl Pts',(-31.9624582736835,-1.40210181883799,
0.808077700742095));
#63694=CARTESIAN_POINT('Ctrl Pts',(-31.8829146464664,-1.43784874689912,
-0.742610302827902));
#63695=CARTESIAN_POINT('Ctrl Pts',(-31.8033710192494,-0.152673176153759,
-1.61107727378611));
#63696=CARTESIAN_POINT('Ctrl Pts',(-31.7238273920323,1.27276014686275,-0.999480209600985));
#63697=CARTESIAN_POINT('Ctrl Pts',(-31.6442837648153,1.52893452160575,0.530319063836459));
#63698=CARTESIAN_POINT('Ctrl Pts',(-31.5647401375983,0.380507742613516,
1.57292496281214));
#63699=CARTESIAN_POINT('Ctrl Pts',(-31.4851965103811,-1.11748378668527,
1.1705165813955));
#63700=CARTESIAN_POINT('Ctrl Pts',(-31.4056528831641,-1.58886561237809,
-0.30722165716086));
#63701=CARTESIAN_POINT('Ctrl Pts',(-31.326109255947,-0.600588806036943,
-1.50272158661857));
#63702=CARTESIAN_POINT('Ctrl Pts',(-31.24656562873,0.939436762569066,-1.31770165438161));
#63703=CARTESIAN_POINT('Ctrl Pts',(-31.1670220015129,1.61642081963931,0.0778640781290166));
#63704=CARTESIAN_POINT('Ctrl Pts',(-31.0874783742959,0.808431834304442,
1.40189766035522));
#63705=CARTESIAN_POINT('Ctrl Pts',(-31.0079347470788,-0.742247090418913,
1.43803627825968));
#63706=CARTESIAN_POINT('Ctrl Pts',(-30.9283911198618,-1.61103865840699,
0.153080116097703));
#63707=CARTESIAN_POINT('Ctrl Pts',(-30.8488474926447,-0.999801666418527,
-1.27250764581319));
#63708=CARTESIAN_POINT('Ctrl Pts',(-30.7693038654276,0.529932850685034,
-1.52906842704672));
#63709=CARTESIAN_POINT('Ctrl Pts',(-30.6897602382106,1.57282879952036,-0.380905038330596));
#63710=CARTESIAN_POINT('Ctrl Pts',(-30.6102166109935,1.17079881123042,1.11718808821421));
#63711=CARTESIAN_POINT('Ctrl Pts',(-30.5306729837765,-0.306820313027887,
1.58894316334467));
#63712=CARTESIAN_POINT('Ctrl Pts',(-30.4511293565594,-1.50256983490729,
0.600968361940099));
#63713=CARTESIAN_POINT('Ctrl Pts',(-30.3715857293423,-1.31793890631321,
-0.939103892044016));
#63714=CARTESIAN_POINT('Ctrl Pts',(-30.2920421021253,0.0774557810950461,
-1.61644043589649));
#63715=CARTESIAN_POINT('Ctrl Pts',(-30.2124984749082,1.40169341242787,-0.808785916286005));
#63716=CARTESIAN_POINT('Ctrl Pts',(-30.1329548476912,1.43822371786973,0.741883830652245));
#63717=CARTESIAN_POINT('Ctrl Pts',(-30.0534112204741,0.153487046274775,
1.61099994023964));
#63718=CARTESIAN_POINT('Ctrl Pts',(-29.973867593257,-1.27225506357436,1.00012305944603));
#63719=CARTESIAN_POINT('Ctrl Pts',(-29.89432396604,-1.52920223492915,-0.529546603722463));
#63720=CARTESIAN_POINT('Ctrl Pts',(-29.8147803388229,-0.381302309744958,
-1.57273253587807));
#63721=CARTESIAN_POINT('Ctrl Pts',(-29.7352367116059,1.11689231846367,-1.17108096636533));
#63722=CARTESIAN_POINT('Ctrl Pts',(-29.6556930843888,1.58902061293255,0.306418949318976));
#63723=CARTESIAN_POINT('Ctrl Pts',(-29.5761494571718,0.601347879499918,
1.50241798732817));
#63724=CARTESIAN_POINT('Ctrl Pts',(-29.4966058299547,-0.938770961601707,
1.3181760741569));
#63725=CARTESIAN_POINT('Ctrl Pts',(-29.4170622027376,-1.6164599490206,-0.0770474791191996));
#63726=CARTESIAN_POINT('Ctrl Pts',(-29.3375185755206,-0.809139946664935,
-1.40148907506886));
#63727=CARTESIAN_POINT('Ctrl Pts',(-29.2579749483035,0.741520523551474,
-1.43841106571739));
#63728=CARTESIAN_POINT('Ctrl Pts',(-29.1784313210865,1.61096111928633,-0.153893966658978));
#63729=CARTESIAN_POINT('Ctrl Pts',(-29.0988876938694,1.00044438866308,1.27200240016237));
#63730=CARTESIAN_POINT('Ctrl Pts',(-29.0193440666523,-0.529160322973449,
1.52933594524451));
#63731=CARTESIAN_POINT('Ctrl Pts',(-28.9398004394353,-1.57263617189136,
0.38169955683124));
#63732=CARTESIAN_POINT('Ctrl Pts',(-28.8602568122182,-1.17136304678224,
-1.1165964774525));
#63733=CARTESIAN_POINT('Ctrl Pts',(-28.7807131850011,0.306017566059744,
-1.58909796113681));
#63734=CARTESIAN_POINT('Ctrl Pts',(-28.7011695577841,1.5022660438909,-0.601727358692185));
#63735=CARTESIAN_POINT('Ctrl Pts',(-28.621625930567,1.31841315789754,0.93843797126338));
#63736=CARTESIAN_POINT('Ctrl Pts',(-28.54208230335,-0.0766391722275201,
1.61647935901037));
#63737=CARTESIAN_POINT('Ctrl Pts',(-28.4625386761329,-1.40128464829121,
0.809493925418639));
#63738=CARTESIAN_POINT('Ctrl Pts',(-28.3829950489159,-1.4385983217907,-0.741157169139769));
#63739=CARTESIAN_POINT('Ctrl Pts',(-28.3034514216988,-0.154300877224343,
-1.61092219554952));
#63740=CARTESIAN_POINT('Ctrl Pts',(-28.2239077944817,1.27174965559333,-1.0007656540492));
#63741=CARTESIAN_POINT('Ctrl Pts',(-28.1443641672647,1.52946955798429,0.528774008462636));
#63742=CARTESIAN_POINT('Ctrl Pts',(-28.0648205400476,0.382096779564106,
1.5725397075664));
#63743=CARTESIAN_POINT('Ctrl Pts',(-27.9852769128305,-1.11630056519958,
1.17164505246315));
#63744=CARTESIAN_POINT('Ctrl Pts',(-27.9057332856135,-1.5891752079525,-0.305616163275796));
#63745=CARTESIAN_POINT('Ctrl Pts',(-27.8261896583964,-0.602106799492688,
-1.50211400460516));
#63746=CARTESIAN_POINT('Ctrl Pts',(-27.7466460311794,0.938104921050279,
-1.31865015752001));
#63747=CARTESIAN_POINT('Ctrl Pts',(-27.6671024039623,1.61649866586457,0.0762308604460643));
#63748=CARTESIAN_POINT('Ctrl Pts',(-27.5875587767452,0.809847852524537,
1.40108013210797));
#63749=CARTESIAN_POINT('Ctrl Pts',(-27.5080151495282,-0.74079376744032,
1.43878548607771));
#63750=CARTESIAN_POINT('Ctrl Pts',(-27.4284715223112,-1.61088316903171,
0.154707777944918));
#63751=CARTESIAN_POINT('Ctrl Pts',(-27.3489278950941,-1.00108685558388,
-1.27149682988338));
#63752=CARTESIAN_POINT('Ctrl Pts',(-27.269384267877,0.528387660214671,-1.52960307313994));
#63753=CARTESIAN_POINT('Ctrl Pts',(-27.18984064066,1.57244314290934,-0.382493977918206));
#63754=CARTESIAN_POINT('Ctrl Pts',(-27.1102970134429,1.17192698339008,1.1160045817238));
#63755=CARTESIAN_POINT('Ctrl Pts',(-27.0307533862258,-0.305214740992747,
1.5892523533747));
#63756=CARTESIAN_POINT('Ctrl Pts',(-26.9512097590088,-1.50196186948066,
0.602486201877221));
#63757=CARTESIAN_POINT('Ctrl Pts',(-26.8716661317917,-1.31888707300918,
-0.937771810983659));
#63758=CARTESIAN_POINT('Ctrl Pts',(-26.7921225045747,0.0758225438008824,
-1.61651786958198));
#63759=CARTESIAN_POINT('Ctrl Pts',(-26.7125788773576,1.40087552653219,-0.810201727960045));
#63760=CARTESIAN_POINT('Ctrl Pts',(-26.6330352501405,1.43897255856648,0.740430318476311));
#63761=CARTESIAN_POINT('Ctrl Pts',(-26.5534916229235,0.155114668794731,
1.61084403973538));
#63762=CARTESIAN_POINT('Ctrl Pts',(-26.4739479957064,-1.27124392304863,
1.00140799324662));
#63763=CARTESIAN_POINT('Ctrl Pts',(-26.3944043684894,-1.52973649070296,
-0.528001278254208));
#63764=CARTESIAN_POINT('Ctrl Pts',(-26.3148607412723,-0.382891151868202,
-1.57234647792633));
#63765=CARTESIAN_POINT('Ctrl Pts',(-26.2353171140552,1.11570852704404,-1.17220883954503));
#63766=CARTESIAN_POINT('Ctrl Pts',(-26.1557734868382,1.58932939739848,0.304813299236206));
#63767=CARTESIAN_POINT('Ctrl Pts',(-26.0762298596211,0.602865565821572,
1.50180963852711));
#63768=CARTESIAN_POINT('Ctrl Pts',(-25.9966862324041,-0.937438641084768,
1.31912390434994));
#63769=CARTESIAN_POINT('Ctrl Pts',(-25.917142605187,-1.61653697016136,-0.0754142223180269));
#63770=CARTESIAN_POINT('Ctrl Pts',(-25.8375989779699,-0.810555551702585,
-1.40067083157693));
#63771=CARTESIAN_POINT('Ctrl Pts',(-25.7580553507529,0.740066822270931,
-1.43915953924508));
#63772=CARTESIAN_POINT('Ctrl Pts',(-25.6785117235358,1.61080480766303,-0.15552154974783));
#63773=CARTESIAN_POINT('Ctrl Pts',(-25.5989680963188,1.00172906701694,1.27099093510523));
#63774=CARTESIAN_POINT('Ctrl Pts',(-25.5194244691017,-0.527614862605903,
1.52986981066483));
#63775=CARTESIAN_POINT('Ctrl Pts',(-25.4398808418846,-1.57224971262355,
0.383288301388741));
#63776=CARTESIAN_POINT('Ctrl Pts',(-25.3603372146676,-1.17249062091002,
-1.11541240117919));
#63777=CARTESIAN_POINT('Ctrl Pts',(-25.2807935874505,0.304411838031798,
-1.58940634001894));
#63778=CARTESIAN_POINT('Ctrl Pts',(-25.2012499602335,1.50165731175422,-0.603244891301526));
#63779=CARTESIAN_POINT('Ctrl Pts',(-25.1217063330164,1.31936065152718,0.93710541137487));
#63780=CARTESIAN_POINT('Ctrl Pts',(-25.0421627057994,-0.0750058960235608,
1.61655596760149));
#63781=CARTESIAN_POINT('Ctrl Pts',(-24.9626190785823,-1.40046604725525,
0.810909323729573));
#63782=CARTESIAN_POINT('Ctrl Pts',(-24.8830754513652,-1.43934642810156,
-0.739703278847383));
#63783=CARTESIAN_POINT('Ctrl Pts',(-24.8035318241482,-0.155928420778242,
-1.61076547281716));
#63784=CARTESIAN_POINT('Ctrl Pts',(-24.7239881969311,1.27073786606932,-1.00205007687434));
#63785=CARTESIAN_POINT('Ctrl Pts',(-24.6444445697141,1.53000303301705,0.527228413294394));
#63786=CARTESIAN_POINT('Ctrl Pts',(-24.564900942497,0.383685426454499,1.57215284700716));
#63787=CARTESIAN_POINT('Ctrl Pts',(-24.4853573152799,-1.11511620414815,
1.17277232746708));
#63788=CARTESIAN_POINT('Ctrl Pts',(-24.4058136880629,-1.58948318123115,
-0.304010357405141));
#63789=CARTESIAN_POINT('Ctrl Pts',(-24.3262700608458,-0.603624178292887,
-1.5015048891717));
#63790=CARTESIAN_POINT('Ctrl Pts',(-24.2467264336287,0.936772121875235,
-1.31959731452578));
#63791=CARTESIAN_POINT('Ctrl Pts',(-24.1671828064117,1.61657486190117,0.0745975649435363));
#63792=CARTESIAN_POINT('Ctrl Pts',(-24.0876391791946,0.811263044018437,
1.40026117358021));
#63793=CARTESIAN_POINT('Ctrl Pts',(-24.0080955519776,-0.739339688228858,
1.43953322512401));
#63794=CARTESIAN_POINT('Ctrl Pts',(-23.9285519247605,-1.61072603520029,
0.156335281860002));
#63795=CARTESIAN_POINT('Ctrl Pts',(-23.8490082975435,-1.00237102279835,
-1.27048471595706));
#63796=CARTESIAN_POINT('Ctrl Pts',(-23.7694646703264,0.526841930344371,
-1.5301361577511));
#63797=CARTESIAN_POINT('Ctrl Pts',(-23.6899210431094,1.57205588108336,-0.384082527040115));
#63798=CARTESIAN_POINT('Ctrl Pts',(-23.6103774158923,1.17305395919821,1.11481993596979));
#63799=CARTESIAN_POINT('Ctrl Pts',(-23.5308337886752,-0.303608857381817,
1.58955992103022));
#63800=CARTESIAN_POINT('Ctrl Pts',(-23.4512901614582,-1.50135237078928,
0.604003426771492));
#63801=CARTESIAN_POINT('Ctrl Pts',(-23.3717465342411,-1.31983389333067,
-0.9364387726071));
#63802=CARTESIAN_POINT('Ctrl Pts',(-23.292202907024,0.0741892291039624,
-1.61659365305919));
#63803=CARTESIAN_POINT('Ctrl Pts',(-23.212659279807,1.40005621056488,-0.811616712546633));
#63804=CARTESIAN_POINT('Ctrl Pts',(-23.1331156525899,1.43971993030053,0.738976050438524));
#63805=CARTESIAN_POINT('Ctrl Pts',(-23.0535720253729,0.156742132967183,
1.61068649481492));
#63806=CARTESIAN_POINT('Ctrl Pts',(-22.9740283981558,-1.27023148478456,
1.00269190476851));
#63807=CARTESIAN_POINT('Ctrl Pts',(-22.8944847709387,-1.53026918485852,
-0.526455413780454));
#63808=CARTESIAN_POINT('Ctrl Pts',(-22.8149411437217,-0.384479603120299,
-1.57195881485831));
#63809=CARTESIAN_POINT('Ctrl Pts',(-22.7353975165047,1.11452359666304,-1.17333551608548));
#63810=CARTESIAN_POINT('Ctrl Pts',(-22.6558538892875,1.58963655941125,0.303207337987452));
#63811=CARTESIAN_POINT('Ctrl Pts',(-22.5763102620705,0.6043826367131,1.50119975661669));
#63812=CARTESIAN_POINT('Ctrl Pts',(-22.4967666348534,-0.936105363591735,
1.32007038792675));
#63813=CARTESIAN_POINT('Ctrl Pts',(-22.4172230076364,-1.61661234107435,
-0.0737808885309362));
#63814=CARTESIAN_POINT('Ctrl Pts',(-22.3376793804193,-0.81197032929159,
-1.39985115822233));
#63815=CARTESIAN_POINT('Ctrl Pts',(-22.2581357532022,0.738612365499613,
-1.43990654361919));
#63816=CARTESIAN_POINT('Ctrl Pts',(-22.1785921259852,1.61064685166359,-0.157148974073823));
#63817=CARTESIAN_POINT('Ctrl Pts',(-22.0990484987681,1.00301272276432,1.26997817256801));
#63818=CARTESIAN_POINT('Ctrl Pts',(-22.0195048715511,-0.526068863627305,
1.5304021143308));
#63819=CARTESIAN_POINT('Ctrl Pts',(-21.939961244334,-1.57186164833823,0.384876654669678));
#63820=CARTESIAN_POINT('Ctrl Pts',(-21.860417617117,-1.1736169981109,-1.11422718624679));
#63821=CARTESIAN_POINT('Ctrl Pts',(-21.7808739898999,0.302805799247685,
-1.58971309636936));
#63822=CARTESIAN_POINT('Ctrl Pts',(-21.7013303626829,1.50104704666367,-0.604761808093543));
#63823=CARTESIAN_POINT('Ctrl Pts',(-21.6217867354658,1.32030679829891,0.935771894850433));
#63824=CARTESIAN_POINT('Ctrl Pts',(-21.5422431082487,-0.0733725432504879,
1.61663092594545));
#63825=CARTESIAN_POINT('Ctrl Pts',(-21.4626994810317,-1.39964601656566,
0.812323894230727));
#63826=CARTESIAN_POINT('Ctrl Pts',(-21.3831558538146,-1.44009306506808,
-0.738248633435309));
#63827=CARTESIAN_POINT('Ctrl Pts',(-21.3036122265975,-0.157555805153939,
-1.61060710574882));
#63828=CARTESIAN_POINT('Ctrl Pts',(-21.2240685993805,1.26972477932356,-1.00333347676534));
#63829=CARTESIAN_POINT('Ctrl Pts',(-21.1445249721634,1.53053494615945,0.525682279909613));
#63830=CARTESIAN_POINT('Ctrl Pts',(-21.0649813449464,0.385273681662942,
1.5717643815293));
#63831=CARTESIAN_POINT('Ctrl Pts',(-20.9854377177293,-1.11393070473997,
1.17389840525652));
#63832=CARTESIAN_POINT('Ctrl Pts',(-20.9058940905123,-1.58978953189966,
-0.302404241188112));
#63833=CARTESIAN_POINT('Ctrl Pts',(-20.8263504632952,-0.605140940888606,
-1.50089424093996));
#63834=CARTESIAN_POINT('Ctrl Pts',(-20.7468068360781,0.935438366404454,
-1.32054312443209));
#63835=CARTESIAN_POINT('Ctrl Pts',(-20.667263208861,1.61664940767132,0.0729641932886911));
#63836=CARTESIAN_POINT('Ctrl Pts',(-20.587719581644,0.81267740734151,1.39944078560794));
#63837=CARTESIAN_POINT('Ctrl Pts',(-20.5081759544269,-0.737884854268845,
1.44027949463531));
#63838=CARTESIAN_POINT('Ctrl Pts',(-20.4286323272099,-1.61056725707314,
0.1579626261816));
#63839=CARTESIAN_POINT('Ctrl Pts',(-20.3490886999928,-1.00365416675107,
-1.26947130506739));
#63840=CARTESIAN_POINT('Ctrl Pts',(-20.2695450727758,0.525295662652017,
-1.53066768033603));
#63841=CARTESIAN_POINT('Ctrl Pts',(-20.1900014455587,1.57166701443773,-0.385670684074736));
#63842=CARTESIAN_POINT('Ctrl Pts',(-20.1104578183417,1.17417973750438,1.11363415216148));
#63843=CARTESIAN_POINT('Ctrl Pts',(-20.0309141911245,-0.302002663834377,
1.58986586599726));
#63844=CARTESIAN_POINT('Ctrl Pts',(-19.9513705639076,-1.50074133945531,
0.605520035074122));
#63845=CARTESIAN_POINT('Ctrl Pts',(-19.8718269366905,-1.32077936631118,
-0.935104778275095));
#63846=CARTESIAN_POINT('Ctrl Pts',(-19.7922833094734,0.0725558386715783,
-1.61666778625077));
#63847=CARTESIAN_POINT('Ctrl Pts',(-19.7127396822564,1.39923546536229,-0.813030868601358));
#63848=CARTESIAN_POINT('Ctrl Pts',(-19.6331960550393,1.44046583230898,0.737521028023404));
#63849=CARTESIAN_POINT('Ctrl Pts',(-19.5536524278223,0.158369437130823,
1.61052730563911));
#63850=CARTESIAN_POINT('Ctrl Pts',(-19.4741088006052,-1.26921774981566,
1.00397479270108));
#63851=CARTESIAN_POINT('Ctrl Pts',(-19.3945651733881,-1.53080031685203,
-0.524909011879212));
#63852=CARTESIAN_POINT('Ctrl Pts',(-19.315021546171,-0.386067661879754,
-1.57156954706974));
#63853=CARTESIAN_POINT('Ctrl Pts',(-19.235477918954,1.11333752853026,-1.17446099483654));
#63854=CARTESIAN_POINT('Ctrl Pts',(-19.1559342917369,1.58994209865731,0.301601067212078));
#63855=CARTESIAN_POINT('Ctrl Pts',(-19.0763906645199,0.605899090625881,
1.50058834221949));
#63856=CARTESIAN_POINT('Ctrl Pts',(-18.9968470373028,-0.934771130483621,
1.32101552392115));
#63857=CARTESIAN_POINT('Ctrl Pts',(-18.9173034100858,-1.61668606168263,
-0.0721474794252276));
#63858=CARTESIAN_POINT('Ctrl Pts',(-18.8377597828687,-0.813384277987742,
-1.39903005584178));
#63859=CARTESIAN_POINT('Ctrl Pts',(-18.7582161556516,0.737157154722223,
-1.44065207807719));
#63860=CARTESIAN_POINT('Ctrl Pts',(-18.6786725284346,1.61048725144926,-0.158776237975679));
#63861=CARTESIAN_POINT('Ctrl Pts',(-18.5991289012175,1.00429535459488,1.26896411358455));
#63862=CARTESIAN_POINT('Ctrl Pts',(-18.5195852740004,-0.524522327615841,
1.53093285569902));
#63863=CARTESIAN_POINT('Ctrl Pts',(-18.4400416467834,-1.57147197943155,
0.386464615052644));
#63864=CARTESIAN_POINT('Ctrl Pts',(-18.3604980195664,-1.17474217723504,
-1.11304083386521));
#63865=CARTESIAN_POINT('Ctrl Pts',(-18.2809543923493,0.301199451346863,
-1.59001822987494));
#63866=CARTESIAN_POINT('Ctrl Pts',(-18.2014107651322,1.50043524924223,-0.60627810751972));
#63867=CARTESIAN_POINT('Ctrl Pts',(-18.1218671379152,1.32125159724689,0.934437423051337));
#63868=CARTESIAN_POINT('Ctrl Pts',(-18.0423235106981,-0.0717391155756687,
1.61670423396573));
#63869=CARTESIAN_POINT('Ctrl Pts',(-17.962779883481,-1.39882455705954,0.813737635478094));
#63870=CARTESIAN_POINT('Ctrl Pts',(-17.883236256264,-1.44083823192808,-0.736793234388497));
#63871=CARTESIAN_POINT('Ctrl Pts',(-17.8036926290469,-0.159183028690188,
-1.61044709450615));
#63872=CARTESIAN_POINT('Ctrl Pts',(-17.7241490018299,1.26871039639025,-1.00461585241206));
#63873=CARTESIAN_POINT('Ctrl Pts',(-17.6446053746128,1.53106529686852,0.524135609886599));
#63874=CARTESIAN_POINT('Ctrl Pts',(-17.5650617473957,0.386861543568101,
1.57137431152937));
#63875=CARTESIAN_POINT('Ctrl Pts',(-17.4855181201787,-1.11274406818528,
1.17502328468195));
#63876=CARTESIAN_POINT('Ctrl Pts',(-17.4059744929616,-1.59009425964529,
-0.300797816264331));
#63877=CARTESIAN_POINT('Ctrl Pts',(-17.3264308657446,-0.606657085731434,
-1.50028206053333));
#63878=CARTESIAN_POINT('Ctrl Pts',(-17.2468872385275,0.934103655999516,
-1.32148758627337));
#63879=CARTESIAN_POINT('Ctrl Pts',(-17.1673436113105,1.61672230309892,0.0713307471489807));
#63880=CARTESIAN_POINT('Ctrl Pts',(-17.0877999840934,0.814090941049888,
1.39861896902866));
#63881=CARTESIAN_POINT('Ctrl Pts',(-17.0082563568763,-0.736429267045466,
1.44102429384975));
#63882=CARTESIAN_POINT('Ctrl Pts',(-16.9287127296593,-1.61040683481235,
0.159589809248418));
#63883=CARTESIAN_POINT('Ctrl Pts',(-16.8491691024422,-1.00493628613213,
-1.26845659824893));
#63884=CARTESIAN_POINT('Ctrl Pts',(-16.7696254752251,0.523748858716137,
-1.5311976403521));
#63885=CARTESIAN_POINT('Ctrl Pts',(-16.6900818480081,1.57127654336944,-0.38725844740078));
#63886=CARTESIAN_POINT('Ctrl Pts',(-16.610538220791,1.17530431715934,1.11244723150939));
#63887=CARTESIAN_POINT('Ctrl Pts',(-16.530994593574,-0.300396161990134,
1.5901701879635));
#63888=CARTESIAN_POINT('Ctrl Pts',(-16.4514509663569,-1.50012877610254,
0.607036025236869));
#63889=CARTESIAN_POINT('Ctrl Pts',(-16.3719073391398,-1.32172349098552,
-0.933769829349476));
#63890=CARTESIAN_POINT('Ctrl Pts',(-16.2923637119228,0.0709223741711957,
-1.61674026908103));
#63891=CARTESIAN_POINT('Ctrl Pts',(-16.2128200847057,1.39841329176228,-0.814444194680562));
#63892=CARTESIAN_POINT('Ctrl Pts',(-16.1332764574887,1.44121026383035,0.73606525271633));
#63893=CARTESIAN_POINT('Ctrl Pts',(-16.0537328302716,0.159996579624394,
1.61036647237043));
#63894=CARTESIAN_POINT('Ctrl Pts',(-15.9741892030546,-1.26820271917681,
1.00525665573467));
#63895=CARTESIAN_POINT('Ctrl Pts',(-15.8946455758375,-1.5313298861413,-0.523362074129152));
#63896=CARTESIAN_POINT('Ctrl Pts',(-15.8151019486205,-0.387655326525378,
-1.57117867495801));
#63897=CARTESIAN_POINT('Ctrl Pts',(-15.7355583214034,1.1121503238565,-1.17558527464926));
#63898=CARTESIAN_POINT('Ctrl Pts',(-15.6560146941863,1.59024601482475,0.299994488549867));
#63899=CARTESIAN_POINT('Ctrl Pts',(-15.5764710669692,0.60741492601182,1.49997539595966));
#63900=CARTESIAN_POINT('Ctrl Pts',(-15.4969274397522,-0.93343594312249,
1.32195931136829));
#63901=CARTESIAN_POINT('Ctrl Pts',(-15.4173838125351,-1.61675813191094,
-0.0705139966683875));
#63902=CARTESIAN_POINT('Ctrl Pts',(-15.3378401853181,-0.814797396347597,
-1.39820752527351));
#63903=CARTESIAN_POINT('Ctrl Pts',(-15.258296558101,0.73570119142432,-1.44139614185799));
#63904=CARTESIAN_POINT('Ctrl Pts',(-15.178752930884,1.61032600718294,-0.16040333979222));
#63905=CARTESIAN_POINT('Ctrl Pts',(-15.0992093036669,1.00557696119926,1.26794875919005));
#63906=CARTESIAN_POINT('Ctrl Pts',(-15.0196656764498,-0.522975256150292,
1.5314620342277));
#63907=CARTESIAN_POINT('Ctrl Pts',(-14.9401220492328,-1.57108070630129,
0.388052180916562));
#63908=CARTESIAN_POINT('Ctrl Pts',(-14.8605784220157,-1.17586615713382,
-1.1118533452455));
#63909=CARTESIAN_POINT('Ctrl Pts',(-14.7810347947987,0.299592795969159,
-1.59032174022419));
#63910=CARTESIAN_POINT('Ctrl Pts',(-14.7014911675816,1.49982192011447,-0.607793788032152));
#63911=CARTESIAN_POINT('Ctrl Pts',(-14.6219475403645,1.32219504740662,0.93310199733987));
#63912=CARTESIAN_POINT('Ctrl Pts',(-14.5424039131475,-0.0701056146665614,
1.61677589158748));
#63913=CARTESIAN_POINT('Ctrl Pts',(-14.4628602859304,-1.39800166957547,
0.815150546028472));
#63914=CARTESIAN_POINT('Ctrl Pts',(-14.3833166587134,-1.44158192792085,
-0.735337083192683));
#63915=CARTESIAN_POINT('Ctrl Pts',(-14.3037730314963,-0.160810089725831,
-1.61028543925251));
#63916=CARTESIAN_POINT('Ctrl Pts',(-14.2242294042792,1.26769471830488,-1.0058972025054));
#63917=CARTESIAN_POINT('Ctrl Pts',(-14.1446857770622,1.53159408460286,0.522588404804257));
#63918=CARTESIAN_POINT('Ctrl Pts',(-14.0651421498451,0.388449010549016,
1.57098263740558));
#63919=CARTESIAN_POINT('Ctrl Pts',(-13.9855985226281,-1.11155629569543,
1.17614696459504));
#63920=CARTESIAN_POINT('Ctrl Pts',(-13.906054895411,-1.59039736415696,-0.299191084273672));
#63921=CARTESIAN_POINT('Ctrl Pts',(-13.8265112681939,-0.608172611273664,
-1.49966834857674));
#63922=CARTESIAN_POINT('Ctrl Pts',(-13.7469676409769,0.932767992022944,
-1.32243069908551));
#63923=CARTESIAN_POINT('Ctrl Pts',(-13.6674240137598,1.61679354810954,0.0696972281918805));
#63924=CARTESIAN_POINT('Ctrl Pts',(-13.5878803865428,0.815503643700602,
1.3977957246813));
#63925=CARTESIAN_POINT('Ctrl Pts',(-13.5083367593257,-0.734972928044621,
1.44176762200704));
#63926=CARTESIAN_POINT('Ctrl Pts',(-13.4287931321086,-1.6102447685817,0.161216829399376));
#63927=CARTESIAN_POINT('Ctrl Pts',(-13.3492495048916,-1.00621737963268,
-1.26744059653753));
#63928=CARTESIAN_POINT('Ctrl Pts',(-13.2697058776745,0.522201520115732,
-1.53172603725832));
#63929=CARTESIAN_POINT('Ctrl Pts',(-13.1901622504575,1.5708844682771,-0.388845815397424));
#63930=CARTESIAN_POINT('Ctrl Pts',(-13.1106186232404,1.17642769701507,1.11125917522517));
#63931=CARTESIAN_POINT('Ctrl Pts',(-13.0310749960234,-0.298789353489053,
1.59047288661827));
#63932=CARTESIAN_POINT('Ctrl Pts',(-12.9515313688063,-1.49951468135628,
0.608551395712171));
#63933=CARTESIAN_POINT('Ctrl Pts',(-12.8719877415893,-1.32266626638989,
-0.932433927192988));
#63934=CARTESIAN_POINT('Ctrl Pts',(-12.7924441143722,0.0692888372703077,
-1.616811101476));
#63935=CARTESIAN_POINT('Ctrl Pts',(-12.7129004871551,1.39758969060416,-0.815856689341468));
#63936=CARTESIAN_POINT('Ctrl Pts',(-12.633356859938,1.44195322410471,0.734608726003382));
#63937=CARTESIAN_POINT('Ctrl Pts',(-12.553813232721,0.161623558786877,1.61020399517309));
#63938=CARTESIAN_POINT('Ctrl Pts',(-12.4742696055039,-1.26718639390419,
1.00653749256072));
#63939=CARTESIAN_POINT('Ctrl Pts',(-12.3947259782869,-1.53185789218571,
-0.521814602109434));
#63940=CARTESIAN_POINT('Ctrl Pts',(-12.3151823510698,-0.389242595436448,
-1.57078619892211));
#63941=CARTESIAN_POINT('Ctrl Pts',(-12.2356387238528,1.11096198385369,-1.17670835437596));
#63942=CARTESIAN_POINT('Ctrl Pts',(-12.1560950966357,1.59054830760332,0.298387603640872));
#63943=CARTESIAN_POINT('Ctrl Pts',(-12.0765514694187,0.608930141323501,
1.49936091846293));
#63944=CARTESIAN_POINT('Ctrl Pts',(-11.9970078422015,-0.93209980287133,
1.32290174930472));
#63945=CARTESIAN_POINT('Ctrl Pts',(-11.9174642149845,-1.61682855168572,
-0.0688804419279146));
#63946=CARTESIAN_POINT('Ctrl Pts',(-11.8379205877674,-0.816209682928599,
-1.39738356735719));
#63947=CARTESIAN_POINT('Ctrl Pts',(-11.7583769605504,0.734244477092241,
-1.44213873420202));
#63948=CARTESIAN_POINT('Ctrl Pts',(-11.6788333333333,1.61016311902928,-0.162030277862366));
#63949=CARTESIAN_POINT('Ctrl Pts',(-11.5992897061163,1.00685754126906,1.26693211042105));
#63950=CARTESIAN_POINT('Ctrl Pts',(-11.5197460788992,-0.52142765080999,
1.53198964937662));
#63951=CARTESIAN_POINT('Ctrl Pts',(-11.4402024516822,-1.57068782934691,
0.389639350640762));
#63952=CARTESIAN_POINT('Ctrl Pts',(-11.3606588244651,-1.1769889366598,-1.11066472159995));
#63953=CARTESIAN_POINT('Ctrl Pts',(-11.2811151972481,0.297985834754776,
-1.59062362710725));
#63954=CARTESIAN_POINT('Ctrl Pts',(-11.201571570031,1.49920705990647,-0.609308848083547));
#63955=CARTESIAN_POINT('Ctrl Pts',(-11.1220279428139,1.32313714781499,0.931765619079327));
#63956=CARTESIAN_POINT('Ctrl Pts',(-11.0424843155969,-0.06847204219078,
1.61684589873756));
#63957=CARTESIAN_POINT('Ctrl Pts',(-10.9629406883798,-1.39717735495351,
0.816562624439442));
#63958=CARTESIAN_POINT('Ctrl Pts',(-10.8833970611627,-1.44232415228718,
-0.733880181334382));
#63959=CARTESIAN_POINT('Ctrl Pts',(-10.8038534339457,-0.162436986599875,
-1.61012214015292));
#63960=CARTESIAN_POINT('Ctrl Pts',(-10.7243098067286,1.26667774610436,-1.00717752573727));
#63961=CARTESIAN_POINT('Ctrl Pts',(-10.6447661795116,1.53212130882261,0.521040666242096));
#63962=CARTESIAN_POINT('Ctrl Pts',(-10.5652225522945,0.390036080985107,
1.57058935955777));
#63963=CARTESIAN_POINT('Ctrl Pts',(-10.4856789250774,-1.11036738848296,
1.17726944384868));
#63964=CARTESIAN_POINT('Ctrl Pts',(-10.4061352978604,-1.59069884512526,
-0.297584046856419));
#63965=CARTESIAN_POINT('Ctrl Pts',(-10.3265916706433,-0.609687515968113,
-1.49905310569671));
#63966=CARTESIAN_POINT('Ctrl Pts',(-10.2470480434263,0.931431375838247,
-1.32337246190571));
#63967=CARTESIAN_POINT('Ctrl Pts',(-10.1675044162092,1.61686314263048,0.0680636380849846));
#63968=CARTESIAN_POINT('Ctrl Pts',(-10.0879607889922,0.816915513851456,
1.39697105340629));
#63969=CARTESIAN_POINT('Ctrl Pts',(-10.0084171617751,-0.733515838753049,
1.44250947834832));
#63970=CARTESIAN_POINT('Ctrl Pts',(-9.92887353455802,-1.61008105854661,
0.162843684973514));
#63971=CARTESIAN_POINT('Ctrl Pts',(-9.84932990734096,-1.00749744594493,
-1.26642330097038));
#63972=CARTESIAN_POINT('Ctrl Pts',(-9.7697862801239,0.520653648430462,-1.53225287051528));
#63973=CARTESIAN_POINT('Ctrl Pts',(-9.69024265290685,1.57049078956095,-0.39043278644415));
#63974=CARTESIAN_POINT('Ctrl Pts',(-9.61069902568979,1.17754987592476,1.11006998452165));
#63975=CARTESIAN_POINT('Ctrl Pts',(-9.53115539847272,-0.297182239971462,
1.59077396165257));
#63976=CARTESIAN_POINT('Ctrl Pts',(-9.45161177125567,-1.49889905584346,
0.610066144953023));
#63977=CARTESIAN_POINT('Ctrl Pts',(-9.37206814403861,-1.32360769156184,
-0.931097073169421));
#63978=CARTESIAN_POINT('Ctrl Pts',(-9.29252451682155,0.0676552296365225,
-1.61688028336335));
#63979=CARTESIAN_POINT('Ctrl Pts',(-9.21298088960448,1.39676466272872,-0.817268351142129));
#63980=CARTESIAN_POINT('Ctrl Pts',(-9.13343726238743,1.44269471237359,0.73315144937151));
#63981=CARTESIAN_POINT('Ctrl Pts',(-9.05389363517037,0.163250372957315,
1.61003987421294));
#63982=CARTESIAN_POINT('Ctrl Pts',(-8.97435000795331,-1.26616877503531,
1.00781730187167));
#63983=CARTESIAN_POINT('Ctrl Pts',(-8.89480638073625,-1.53238433444625,
-0.520266597399813));
#63984=CARTESIAN_POINT('Ctrl Pts',(-8.81526275351919,-0.390829466992555,
-1.57039211936273));
#63985=CARTESIAN_POINT('Ctrl Pts',(-8.73571912630214,1.10977250973498,-1.1778302328701));
#63986=CARTESIAN_POINT('Ctrl Pts',(-8.65617549908506,1.59084897668441,0.296780414125484));
#63987=CARTESIAN_POINT('Ctrl Pts',(-8.57663187186802,0.610444735014109,
1.4987449103566));
#63988=CARTESIAN_POINT('Ctrl Pts',(-8.49708824465095,-0.930762711094184,
1.32384283676835));
#63989=CARTESIAN_POINT('Ctrl Pts',(-8.4175446174339,-1.61689732093506,-0.0672468168714717));
#63990=CARTESIAN_POINT('Ctrl Pts',(-8.33800099021683,-0.817621136288996,
-1.39655818293396));
#63991=CARTESIAN_POINT('Ctrl Pts',(-8.25845736299976,0.732787013213042,
-1.44287985435121));
#63992=CARTESIAN_POINT('Ctrl Pts',(-8.17891373578272,1.60999858715454,-0.163657050525305));
#63993=CARTESIAN_POINT('Ctrl Pts',(-8.09937010856565,1.00813709349707,1.26591416831537));
#63994=CARTESIAN_POINT('Ctrl Pts',(-8.01982648134859,-0.519879513174783,
1.53251570060716));
#63995=CARTESIAN_POINT('Ctrl Pts',(-7.94028285413154,-1.57029334896946,
0.391226122605003));
#63996=CARTESIAN_POINT('Ctrl Pts',(-7.86073922691447,-1.17811051466681,
-1.10947496414194));
#63997=CARTESIAN_POINT('Ctrl Pts',(-7.78119559969742,0.296378569344132,
-1.59092389021595));
#63998=CARTESIAN_POINT('Ctrl Pts',(-7.70165197248035,1.49859066924594,-0.610823286127277));
#63999=CARTESIAN_POINT('Ctrl Pts',(-7.6221083452633,1.32407789751025,0.930428289633915));
#64000=CARTESIAN_POINT('Ctrl Pts',(-7.54256471804623,-0.066838399815906,
1.61691425534452));
#64001=CARTESIAN_POINT('Ctrl Pts',(-7.46302109082919,-1.39635161403515,
0.817973869269524));
#64002=CARTESIAN_POINT('Ctrl Pts',(-7.3834774636121,-1.44306490426939,-0.73242253030085));
#64003=CARTESIAN_POINT('Ctrl Pts',(-7.30393383639506,-0.164063717651527,
-1.60995719737409));
#64004=CARTESIAN_POINT('Ctrl Pts',(-7.22439020917799,1.26565948082683,-1.00845682080068));
#64005=CARTESIAN_POINT('Ctrl Pts',(-7.14484658196095,1.53264696898959,0.519492395780081));
#64006=CARTESIAN_POINT('Ctrl Pts',(-7.06530295474387,0.391622753256244,
1.57019447838741));
#64007=CARTESIAN_POINT('Ctrl Pts',(-6.98575932752683,-1.10917734776157,
1.178390721297));
#64008=CARTESIAN_POINT('Ctrl Pts',(-6.90621570030976,-1.59099870224241,
-0.295976705653066));
#64009=CARTESIAN_POINT('Ctrl Pts',(-6.8266720730927,-0.611201798268341,
-1.49843633252129));
#64010=CARTESIAN_POINT('Ctrl Pts',(-6.74712844587563,0.930093808809897,
-1.32431287377259));
#64011=CARTESIAN_POINT('Ctrl Pts',(-6.66758481865858,1.61693108659067,0.0664299784959112));
#64012=CARTESIAN_POINT('Ctrl Pts',(-6.58804119144151,0.818326550061182,
1.39614495604548));
#64013=CARTESIAN_POINT('Ctrl Pts',(-6.50849756422447,-0.732058000658186,
1.44324986211628));
#64014=CARTESIAN_POINT('Ctrl Pts',(-6.42895393700739,-1.60991570487421,
0.164470374310088));
#64015=CARTESIAN_POINT('Ctrl Pts',(-6.34941030979035,-1.00877648376213,
-1.26540471258597));
#64016=CARTESIAN_POINT('Ctrl Pts',(-6.26986668257327,0.519105245240422,
-1.53277813958516));
#64017=CARTESIAN_POINT('Ctrl Pts',(-6.19032305535623,1.57009550762287,-0.392019358920946));
#64018=CARTESIAN_POINT('Ctrl Pts',(-6.11077942813917,1.17867085274286,1.10887966061279));
#64019=CARTESIAN_POINT('Ctrl Pts',(-6.0312358009221,-0.295574823077957,
1.59107341275904));
#64020=CARTESIAN_POINT('Ctrl Pts',(-5.95169217370504,-1.49828190019252,
0.611580271413133));
#64021=CARTESIAN_POINT('Ctrl Pts',(-5.87214854648798,-1.32454776554033,
-0.929759268643466));
#64022=CARTESIAN_POINT('Ctrl Pts',(-5.79260491927093,0.0660215529374821,
-1.61694781467246));
#64023=CARTESIAN_POINT('Ctrl Pts',(-5.71306129205386,1.39593820897817,-0.818679178641469));
#64024=CARTESIAN_POINT('Ctrl Pts',(-5.63351766483681,1.44343472788007,0.731693424308328));
#64025=CARTESIAN_POINT('Ctrl Pts',(-5.55397403761973,0.164877020475022,
1.60987410965752));
#64026=CARTESIAN_POINT('Ctrl Pts',(-5.47443041040269,-1.265149863609,1.00909608236106));
#64027=CARTESIAN_POINT('Ctrl Pts',(-5.39488678318562,-1.53290921238552,
-0.518718061580541));
#64028=CARTESIAN_POINT('Ctrl Pts',(-5.31534315596856,-0.392415939573786,
-1.56999643668216));
#64029=CARTESIAN_POINT('Ctrl Pts',(-5.23579952875151,1.10858190271461,-1.17895090898645));
#64030=CARTESIAN_POINT('Ctrl Pts',(-5.15625590153444,1.59114802176109,0.295172921644379));
#64031=CARTESIAN_POINT('Ctrl Pts',(-5.07671227431739,0.611958705537498,
1.49812737226951));
#64032=CARTESIAN_POINT('Ctrl Pts',(-4.99716864710033,-0.929424669155988,
1.32478257279848));
#64033=CARTESIAN_POINT('Ctrl Pts',(-4.91762501988327,-1.61696443958877,
-0.0656131231666956));
#64034=CARTESIAN_POINT('Ctrl Pts',(-4.83808139266621,-0.819031754987941,
-1.3957313728464));
#64035=CARTESIAN_POINT('Ctrl Pts',(-4.75853776544915,0.73132880127457,-1.44361950154899));
#64036=CARTESIAN_POINT('Ctrl Pts',(-4.67899413823209,1.60983241172668,-0.165283656120365));
#64037=CARTESIAN_POINT('Ctrl Pts',(-4.59945051101503,1.00941561657705,1.26489493391218));
#64038=CARTESIAN_POINT('Ctrl Pts',(-4.51990688379797,-0.51833084482508,
1.53304018738233));
#64039=CARTESIAN_POINT('Ctrl Pts',(-4.44036325658091,-1.56989726557164,
0.392812495189444));
#64040=CARTESIAN_POINT('Ctrl Pts',(-4.36081962936385,-1.1792308900099,-1.10828407408602));
#64041=CARTESIAN_POINT('Ctrl Pts',(-4.28127600214679,0.294771001377991,
-1.59122252924377));
#64042=CARTESIAN_POINT('Ctrl Pts',(-4.20173237492973,1.49797274876209,-0.612337100617345));
#64043=CARTESIAN_POINT('Ctrl Pts',(-4.12218874771267,1.32501729553206,0.929090010368841));
#64044=CARTESIAN_POINT('Ctrl Pts',(-4.04264512049562,-0.065204689209657,
1.61698096133857));
#64045=CARTESIAN_POINT('Ctrl Pts',(-3.96310149327855,-1.39552444766335,
0.819384279078032));
#64046=CARTESIAN_POINT('Ctrl Pts',(-3.88355786606149,-1.44380418311125,
-0.730964131580138));
#64047=CARTESIAN_POINT('Ctrl Pts',(-3.80401423884443,-0.165690281220156,
-1.60979061108439));
#64048=CARTESIAN_POINT('Ctrl Pts',(-3.72447061162737,1.26463992351181,-1.00973508638967));
#64049=CARTESIAN_POINT('Ctrl Pts',(-3.64492698441031,1.53317106456717,0.517943594998788));
#64050=CARTESIAN_POINT('Ctrl Pts',(-3.56538335719325,0.393209025742654,
1.56979799429761));
#64051=CARTESIAN_POINT('Ctrl Pts',(-3.4858397299762,-1.10798617474608,1.17951079579536));
#64052=CARTESIAN_POINT('Ctrl Pts',(-3.40629610275913,-1.59129693520231,
-0.294369062304476));
#64053=CARTESIAN_POINT('Ctrl Pts',(-3.32675247554208,-0.612715456628484,
-1.49781802968016));
#64054=CARTESIAN_POINT('Ctrl Pts',(-3.24720884832501,0.928755292303373,
-1.32525193372606));
#64055=CARTESIAN_POINT('Ctrl Pts',(-3.16766522110795,1.61699737992072,0.0647962510922705));
#64056=CARTESIAN_POINT('Ctrl Pts',(-3.0881215938909,0.819736750889412,1.39531743344239));
#64057=CARTESIAN_POINT('Ctrl Pts',(-3.00857796667384,-0.730599415248462,
1.44398877255475));
#64058=CARTESIAN_POINT('Ctrl Pts',(-2.92903433945677,-1.60974870773295,
0.166096895749144));
#64059=CARTESIAN_POINT('Ctrl Pts',(-2.84949071223972,-1.01005449177923,
-1.26438483242538));
#64060=CARTESIAN_POINT('Ctrl Pts',(-2.76994708502266,0.517556312127521,
-1.53330184392934));
#64061=CARTESIAN_POINT('Ctrl Pts',(-2.6904034578056,1.56969862286412,-0.393605531212727));
#64062=CARTESIAN_POINT('Ctrl Pts',(-2.61085983058854,1.17979062632931,1.10768820472246));
#64063=CARTESIAN_POINT('Ctrl Pts',(-2.53131620337148,-0.293967104457652,
1.59137123961546));
#64064=CARTESIAN_POINT('Ctrl Pts',(-2.45177257615442,-1.49766321501792,
0.613093773578183));
#64065=CARTESIAN_POINT('Ctrl Pts',(-2.37222894893736,-1.32548648739524,
-0.928420515040416));
#64066=CARTESIAN_POINT('Ctrl Pts',(-2.2926853217203,0.06438780889704,-1.61701369522131));
#64067=CARTESIAN_POINT('Ctrl Pts',(-2.21314169450324,1.3951103300897,-0.820089170613862));
#64068=CARTESIAN_POINT('Ctrl Pts',(-2.13359806728618,1.44417327007082,0.730234652709602));
#64069=CARTESIAN_POINT('Ctrl Pts',(-2.05405444006912,0.166503499295801,
1.60970670090295));
#64070=CARTESIAN_POINT('Ctrl Pts',(-1.97451081285206,-1.2641296599373,1.01037383419081));
#64071=CARTESIAN_POINT('Ctrl Pts',(-1.894967185635,-1.53343252684967,-0.517168999017592));
#64072=CARTESIAN_POINT('Ctrl Pts',(-1.81542355841794,-0.394002008937513,
-1.56959914599798));
#64073=CARTESIAN_POINT('Ctrl Pts',(-1.73587993120088,1.10739015902935,-1.18007039161467));
#64074=CARTESIAN_POINT('Ctrl Pts',(-1.65633630398382,1.59144545197782,0.293565146883011));
#64075=CARTESIAN_POINT('Ctrl Pts',(-1.57679267676676,0.613472033412145,
1.49750826868494));
#64076=CARTESIAN_POINT('Ctrl Pts',(-1.49724904954971,-0.928085644379445,
1.32572102504447));
#64077=CARTESIAN_POINT('Ctrl Pts',(-1.41770542233264,-1.61702997219381,
-0.0639794927034563));
#64078=CARTESIAN_POINT('Ctrl Pts',(-1.33816179511559,-0.82044141494256,
-1.39490289077172));
#64079=CARTESIAN_POINT('Ctrl Pts',(-1.25861816789853,0.729869609984358,
-1.44435814417302));
#64080=CARTESIAN_POINT('Ctrl Pts',(-1.17907454068147,1.60966503474331,-0.166909202554005));
#64081=CARTESIAN_POINT('Ctrl Pts',(-1.0995309134644,1.01069227059636,1.26387271817383));
#64082=CARTESIAN_POINT('Ctrl Pts',(-1.01998728624735,-0.516780055630681,
1.53356631700391));
#64083=CARTESIAN_POINT('Ctrl Pts',(-0.940443659030288,-1.56950260069087,
0.394392378168218));
#64084=CARTESIAN_POINT('Ctrl Pts',(-0.860900031813227,-1.18034432730794,
-1.10708049621965));
#64085=CARTESIAN_POINT('Ctrl Pts',(-0.781356404596169,0.293152248650012,
-1.59154147850122));
#64086=CARTESIAN_POINT('Ctrl Pts',(-0.701812777379109,1.49737395733561,
-0.613808656846177));
#64087=CARTESIAN_POINT('Ctrl Pts',(-0.62226915016205,1.32591612848784,0.927671758094482));
#64088=CARTESIAN_POINT('Ctrl Pts',(-0.542725522944993,-0.0634964663375496,
1.61719603486571));
#64089=CARTESIAN_POINT('Ctrl Pts',(-0.463181895727927,-1.39483731768548,
0.820508888385569));
#64090=CARTESIAN_POINT('Ctrl Pts',(-0.383638268510867,-1.44427213481421,
-0.72896222268878));
#64091=CARTESIAN_POINT('Ctrl Pts',(-0.30409464129381,-0.167840324100667,
-1.61066856973343));
#64092=CARTESIAN_POINT('Ctrl Pts',(-0.22455101407675,1.26470887814029,-1.00889155965874));
#64093=CARTESIAN_POINT('Ctrl Pts',(-0.171521929265377,1.44219363372905,
0.00454914606926524));
#64094=CARTESIAN_POINT('Ctrl Pts',(-0.145007386859689,1.29672038264059,
0.436605441725649));
#64095=CARTESIAN_POINT('Ctrl Pts',(-34.6914926131403,0.740036351041036,
-1.03579689087092));
#64096=CARTESIAN_POINT('Ctrl Pts',(-34.6649780707346,1.08515513972758,-0.789223019771014));
#64097=CARTESIAN_POINT('Ctrl Pts',(-34.6119489859232,1.50348693841757,0.0717698932582256));
#64098=CARTESIAN_POINT('Ctrl Pts',(-34.5324053587062,0.751010183525675,
1.30613888124279));
#64099=CARTESIAN_POINT('Ctrl Pts',(-34.4528617314891,-0.69201961693675,
1.33667336675341));
#64100=CARTESIAN_POINT('Ctrl Pts',(-34.3733181042721,-1.49898160723127,
0.141201008990934));
#64101=CARTESIAN_POINT('Ctrl Pts',(-34.293774477055,-0.929029926656085,
-1.18501563808319));
#64102=CARTESIAN_POINT('Ctrl Pts',(-34.2142308498379,0.494492460228167,
-1.4220432962459));
#64103=CARTESIAN_POINT('Ctrl Pts',(-34.1346872226209,1.46368736536371,-0.352952500981455));
#64104=CARTESIAN_POINT('Ctrl Pts',(-34.0551435954038,1.08824726743903,1.0405381588406));
#64105=CARTESIAN_POINT('Ctrl Pts',(-33.9755999681868,-0.286956660944541,
1.47802871078736));
#64106=CARTESIAN_POINT('Ctrl Pts',(-33.8960563409697,-1.39853240674266,
0.557725758042946));
#64107=CARTESIAN_POINT('Ctrl Pts',(-33.8165127137527,-1.2253084215944,-0.874970414807997));
#64108=CARTESIAN_POINT('Ctrl Pts',(-33.7369690865356,0.0735834930598086,
-1.50383748004835));
#64109=CARTESIAN_POINT('Ctrl Pts',(-33.6574254593186,1.3048747329139,-0.751165605936964));
#64110=CARTESIAN_POINT('Ctrl Pts',(-33.5778818321015,1.33740453803429,0.691590082910031));
#64111=CARTESIAN_POINT('Ctrl Pts',(-33.4983382048844,0.141287622339839,
1.49899429581447));
#64112=CARTESIAN_POINT('Ctrl Pts',(-33.4187945776674,-1.18462722022883,
0.929303721395224));
#64113=CARTESIAN_POINT('Ctrl Pts',(-33.3392509504503,-1.42224912569989,
-0.494119812806082));
#64114=CARTESIAN_POINT('Ctrl Pts',(-33.2597073232332,-0.353279547106323,
-1.46360524426102));
#64115=CARTESIAN_POINT('Ctrl Pts',(-33.1801636960162,1.04024076886409,-1.08850633470896));
#64116=CARTESIAN_POINT('Ctrl Pts',(-33.1006200687991,1.47811298739213,0.286581349097347));
#64117=CARTESIAN_POINT('Ctrl Pts',(-33.021076441582,0.558072759518739,1.39839252040441));
#64118=CARTESIAN_POINT('Ctrl Pts',(-32.941532814365,-0.87465759731378,1.22552884740331));
#64119=CARTESIAN_POINT('Ctrl Pts',(-32.8619891871479,-1.5038577503335,-0.0732033464336459));
#64120=CARTESIAN_POINT('Ctrl Pts',(-32.7824455599309,-0.751494270205516,
-1.30468510445132));
#64121=CARTESIAN_POINT('Ctrl Pts',(-32.7029019327138,0.691251762826216,
-1.33757910554996));
#64122=CARTESIAN_POINT('Ctrl Pts',(-32.6233583054968,1.49895881315848,-0.141666293436237));
#64123=CARTESIAN_POINT('Ctrl Pts',(-32.5438146782797,0.929602785374642,
1.18439247013284));
#64124=CARTESIAN_POINT('Ctrl Pts',(-32.4642710510626,-0.493760478361972,
1.42237387924739));
#64125=CARTESIAN_POINT('Ctrl Pts',(-32.3847274238456,-1.46351599911086,
0.35364923657973));
#64126=CARTESIAN_POINT('Ctrl Pts',(-32.3051837966285,-1.08876903669851,
-1.03996579120621));
#64127=CARTESIAN_POINT('Ctrl Pts',(-32.2256401694115,0.286207970540554,
-1.47818532661454));
#64128=CARTESIAN_POINT('Ctrl Pts',(-32.1460965421944,1.39825151664009,-0.558425965016473));
#64129=CARTESIAN_POINT('Ctrl Pts',(-32.0665529149773,1.22574973673945,0.87434801141866));
#64130=CARTESIAN_POINT('Ctrl Pts',(-31.9870092877603,-0.0728234805465783,
1.50387619266977));
#64131=CARTESIAN_POINT('Ctrl Pts',(-31.9074656605432,-1.3044952423758,0.751823799046095));
#64132=CARTESIAN_POINT('Ctrl Pts',(-31.8279220333262,-1.33775366694877,
-0.690913879407841));
#64133=CARTESIAN_POINT('Ctrl Pts',(-31.7483784061091,-0.142044913753986,
-1.49892298156748));
#64134=CARTESIAN_POINT('Ctrl Pts',(-31.668834778892,1.18415762247848,-0.929901923495103));
#64135=CARTESIAN_POINT('Ctrl Pts',(-31.589291151675,1.42249855362995,0.493401182725134));
#64136=CARTESIAN_POINT('Ctrl Pts',(-31.5097475244579,0.354018897385096,
1.46342662354088));
#64137=CARTESIAN_POINT('Ctrl Pts',(-31.4302038972408,-1.03969074397971,
1.08903168873859));
#64138=CARTESIAN_POINT('Ctrl Pts',(-31.3506602700238,-1.47825757321933,
-0.285834584005571));
#64139=CARTESIAN_POINT('Ctrl Pts',(-31.2711166428067,-0.558779133992451,
-1.39811041824621));
#64140=CARTESIAN_POINT('Ctrl Pts',(-31.1915730155897,0.874038369267525,
-1.22597055072383));
#64141=CARTESIAN_POINT('Ctrl Pts',(-31.1120293883726,1.50389453930265,0.0724436115169605));
#64142=CARTESIAN_POINT('Ctrl Pts',(-31.0324857611556,0.752153279787823,
1.30430529627782));
#64143=CARTESIAN_POINT('Ctrl Pts',(-30.9529421339385,-0.690575951838579,
1.33792814341286));
#64144=CARTESIAN_POINT('Ctrl Pts',(-30.8733985067215,-1.49888705437755,
0.142423524788989));
#64145=CARTESIAN_POINT('Ctrl Pts',(-30.7938548795044,-0.93020100226633,
-1.18392269915593));
#64146=CARTESIAN_POINT('Ctrl Pts',(-30.7143112522874,0.493041855597954,
-1.42262313731447));
#64147=CARTESIAN_POINT('Ctrl Pts',(-30.6347676250702,1.4633371546058,-0.354388535570987));
#64148=CARTESIAN_POINT('Ctrl Pts',(-30.5552239978532,1.08929427129284,1.0394156304013));
#64149=CARTESIAN_POINT('Ctrl Pts',(-30.4756803706361,-0.28546117923212,
1.47832972551638));
#64150=CARTESIAN_POINT('Ctrl Pts',(-30.3961367434191,-1.39796923065005,
0.55913226731218));
#64151=CARTESIAN_POINT('Ctrl Pts',(-30.316593116202,-1.22619128648771,-0.873728671348003));
#64152=CARTESIAN_POINT('Ctrl Pts',(-30.237049488985,0.0720637378650388,
-1.50391278998447));
#64153=CARTESIAN_POINT('Ctrl Pts',(-30.1575058617679,1.30411526696189,-0.752482712539535));
#64154=CARTESIAN_POINT('Ctrl Pts',(-30.0779622345508,1.33810253451361,0.69023798020842));
#64155=CARTESIAN_POINT('Ctrl Pts',(-29.9984186073338,0.142802126737032,
1.49885103155494));
#64156=CARTESIAN_POINT('Ctrl Pts',(-29.9188749801168,-1.18368770029605,
0.930500021688224));
#64157=CARTESIAN_POINT('Ctrl Pts',(-29.8393313528997,-1.42274763023194,
-0.492682497013374));
#64158=CARTESIAN_POINT('Ctrl Pts',(-29.7597877256826,-0.354758151145976,
-1.46324759230604));
#64159=CARTESIAN_POINT('Ctrl Pts',(-29.6802440984655,1.03914045050549,-1.08955678434728));
#64160=CARTESIAN_POINT('Ctrl Pts',(-29.6007004712485,1.47840178349218,0.285087756245499));
#64161=CARTESIAN_POINT('Ctrl Pts',(-29.5211568440314,0.55948536495782,1.39782795385983));
#64162=CARTESIAN_POINT('Ctrl Pts',(-29.4416132168144,-0.873418917682327,
1.22641194401741));
#64163=CARTESIAN_POINT('Ctrl Pts',(-29.3620695895973,-1.50393094471276,
-0.071683859615264));
#64164=CARTESIAN_POINT('Ctrl Pts',(-29.2825259623802,-0.752812097280904,
-1.30392515444003));
#64165=CARTESIAN_POINT('Ctrl Pts',(-29.2029823351632,0.689899964539293,
-1.33827684023995));
#64166=CARTESIAN_POINT('Ctrl Pts',(-29.1234387079461,1.49881491310176,-0.143180719573932));
#64167=CARTESIAN_POINT('Ctrl Pts',(-29.0438950807291,0.930798981741808,
1.18345262591384));
#64168=CARTESIAN_POINT('Ctrl Pts',(-28.964351453512,-0.492323106994374,
1.42287203237443));
#64169=CARTESIAN_POINT('Ctrl Pts',(-28.884807826295,-1.4631579366473,0.355127744086476));
#64170=CARTESIAN_POINT('Ctrl Pts',(-28.8052641990779,-1.08981922788518,
-1.03886520430982));
#64171=CARTESIAN_POINT('Ctrl Pts',(-28.7257205718608,0.284714315069542,
-1.47847374714211));
#64172=CARTESIAN_POINT('Ctrl Pts',(-28.6461769446438,1.39768658788457,-0.559838426906849));
#64173=CARTESIAN_POINT('Ctrl Pts',(-28.5666333174267,1.22663252329886,0.873109108290266));
#64174=CARTESIAN_POINT('Ctrl Pts',(-28.4870896902097,-0.0713039767918712,
1.50394900348636));
#64175=CARTESIAN_POINT('Ctrl Pts',(-28.4075460629926,-1.30373495872438,
0.75314143399091));
#64176=CARTESIAN_POINT('Ctrl Pts',(-28.3280024357756,-1.33845106058076,
-0.689561904852759));
#64177=CARTESIAN_POINT('Ctrl Pts',(-28.2484588085585,-0.143559303275531,
-1.4987786990203));
#64178=CARTESIAN_POINT('Ctrl Pts',(-28.1689151813415,1.18321747602428,-0.931097882408006));
#64179=CARTESIAN_POINT('Ctrl Pts',(-28.0893715541243,1.422996343734,0.491963685563887));
#64180=CARTESIAN_POINT('Ctrl Pts',(-28.0098279269073,0.355497314368909,
1.4630681876353));
#64181=CARTESIAN_POINT('Ctrl Pts',(-27.9302842996902,-1.03858989183187,
1.09008160188979));
#64182=CARTESIAN_POINT('Ctrl Pts',(-27.8507406724732,-1.47854561646158,
-0.284340855728072));
#64183=CARTESIAN_POINT('Ctrl Pts',(-27.7711970452561,-0.560191453136734,
-1.39754513273328));
#64184=CARTESIAN_POINT('Ctrl Pts',(-27.6916534180391,0.87279924319158,-1.22685302431797));
#64185=CARTESIAN_POINT('Ctrl Pts',(-27.612109790822,1.50396696630412,0.0709240894191014));
#64186=CARTESIAN_POINT('Ctrl Pts',(-27.532566163605,0.753470722648544,1.30354467982705));
#64187=CARTESIAN_POINT('Ctrl Pts',(-27.4530225363879,-0.689223801170392,
1.33862519552494));
#64188=CARTESIAN_POINT('Ctrl Pts',(-27.3734789091708,-1.49874238931288,
0.143937877817675));
#64189=CARTESIAN_POINT('Ctrl Pts',(-27.2939352819538,-0.931396723667748,
-1.18298225064238));
#64190=CARTESIAN_POINT('Ctrl Pts',(-27.2143916547367,0.491604232744841,
-1.42312056430272));
#64191=CARTESIAN_POINT('Ctrl Pts',(-27.1348480275197,1.46297834527575,-0.355866861969689));
#64192=CARTESIAN_POINT('Ctrl Pts',(-27.0553044003026,1.09034390634437,1.03831451308919));
#64193=CARTESIAN_POINT('Ctrl Pts',(-26.9757607730855,-0.283967378244922,
1.47861739144602));
#64194=CARTESIAN_POINT('Ctrl Pts',(-26.8962171458685,-1.397403588415,0.560544443624956));
#64195=CARTESIAN_POINT('Ctrl Pts',(-26.8166735186514,-1.22707344706068,
-0.872489322406045));
#64196=CARTESIAN_POINT('Ctrl Pts',(-26.7371298914344,0.0705441975211899,
-1.50398483316489));
#64197=CARTESIAN_POINT('Ctrl Pts',(-26.6575862642173,1.30335431776021,-0.753799963232794));
#64198=CARTESIAN_POINT('Ctrl Pts',(-26.5780426370002,1.33879924506136,0.688885653513762));
#64199=CARTESIAN_POINT('Ctrl Pts',(-26.4984990097832,0.144316443176208,
1.49870598398182));
#64200=CARTESIAN_POINT('Ctrl Pts',(-26.4189553825661,-1.18274694978316,
0.931695505501969));
#64201=CARTESIAN_POINT('Ctrl Pts',(-26.339411755349,-1.42324469407266,-0.491244748560173));
#64202=CARTESIAN_POINT('Ctrl Pts',(-26.259868128132,-0.356236386865245,
-1.46288840957441));
#64203=CARTESIAN_POINT('Ctrl Pts',(-26.1803245009149,1.03803906809936,-1.09060614123218));
#64204=CARTESIAN_POINT('Ctrl Pts',(-26.1007808736979,1.47868907209085,0.283593882643916));
#64205=CARTESIAN_POINT('Ctrl Pts',(-26.0212372464808,0.560897398348989,
1.39726195493876));
#64206=CARTESIAN_POINT('Ctrl Pts',(-25.9416936192638,-0.87217934595343,
1.22729379151293));
#64207=CARTESIAN_POINT('Ctrl Pts',(-25.8621499920467,-1.50400260406754,
-0.0701643011223775));
#64208=CARTESIAN_POINT('Ctrl Pts',(-25.7826063648297,-0.754129155722656,
-1.30316387253598));
#64209=CARTESIAN_POINT('Ctrl Pts',(-25.7030627376126,0.688547461904444,
-1.33897320917892));
#64210=CARTESIAN_POINT('Ctrl Pts',(-25.6235191103955,1.49866948302943,-0.144694999326982));
#64211=CARTESIAN_POINT('Ctrl Pts',(-25.5439754831785,0.931994227891605,
1.18251157346162));
#64212=CARTESIAN_POINT('Ctrl Pts',(-25.4644318559614,-0.490885233032826,
1.42336873303591));
#64213=CARTESIAN_POINT('Ctrl Pts',(-25.3848882287444,-1.46279838053699,
0.356605889031989));
#64214=CARTESIAN_POINT('Ctrl Pts',(-25.3053446015273,-1.0908683065365,-1.03776355687995));
#64215=CARTESIAN_POINT('Ctrl Pts',(-25.2258009743102,0.283220368948894,
-1.47876065839148));
#64216=CARTESIAN_POINT('Ctrl Pts',(-25.1462573470932,1.39712023231358,-0.561250317286305));
#64217=CARTESIAN_POINT('Ctrl Pts',(-25.0667137198761,1.22751405766065,0.871869313853523));
#64218=CARTESIAN_POINT('Ctrl Pts',(-24.987170092659,-0.069784400246911,
1.50402027901093));
#64219=CARTESIAN_POINT('Ctrl Pts',(-24.907626465442,-1.30297334416653,0.754458300097118));
#64220=CARTESIAN_POINT('Ctrl Pts',(-24.8280828382249,-1.33914708786651,
-0.688209226364027));
#64221=CARTESIAN_POINT('Ctrl Pts',(-24.7485392110079,-0.14507354624583,
-1.49863288645805));
#64222=CARTESIAN_POINT('Ctrl Pts',(-24.6689955837908,1.18227612169278,-0.932292890817585));
#64223=CARTESIAN_POINT('Ctrl Pts',(-24.5894519565737,1.42349268118454,0.490525686185724));
#64224=CARTESIAN_POINT('Ctrl Pts',(-24.5099083293567,0.356975368446356,
1.46270825816925));
#64225=CARTESIAN_POINT('Ctrl Pts',(-24.4303647021396,-1.03748797944855,
1.0911304022406));
#64226=CARTESIAN_POINT('Ctrl Pts',(-24.3508210749226,-1.47883215034335,
-0.282846837183695));
#64227=CARTESIAN_POINT('Ctrl Pts',(-24.2712774477055,-0.56160320041439,
-1.39697842054852));
#64228=CARTESIAN_POINT('Ctrl Pts',(-24.1917338204884,0.871559226126107,
-1.2277342454898));
#64229=CARTESIAN_POINT('Ctrl Pts',(-24.1121901932714,1.50403785799393,0.0694044949190318));
#64230=CARTESIAN_POINT('Ctrl Pts',(-24.0326465660543,0.754787396335176,
1.30278273266401));
#64231=CARTESIAN_POINT('Ctrl Pts',(-23.9531029388373,-0.687870946914086,
1.33932088111306));
#64232=CARTESIAN_POINT('Ctrl Pts',(-23.8735593116202,-1.49859619427002,
0.145452083908596));
#64233=CARTESIAN_POINT('Ctrl Pts',(-23.7940156844031,-0.932591494260859,
-1.18204059449168));
#64234=CARTESIAN_POINT('Ctrl Pts',(-23.7144720571861,0.490166108041832,
-1.42361653851066));
#64235=CARTESIAN_POINT('Ctrl Pts',(-23.634928429969,1.46261804247694,-0.357344825084754));
#64236=CARTESIAN_POINT('Ctrl Pts',(-23.555384802752,1.09139242832774,1.03721233582272));
#64237=CARTESIAN_POINT('Ctrl Pts',(-23.4758411755349,-0.282473287372118,
1.4789035479419));
#64238=CARTESIAN_POINT('Ctrl Pts',(-23.3962975483179,-1.39683651965262,
0.561956047710764));
#64239=CARTESIAN_POINT('Ctrl Pts',(-23.3167539211008,-1.22795435498632,
-0.871249082790945));
#64240=CARTESIAN_POINT('Ctrl Pts',(-23.2372102938837,0.0690245851629364,
-1.50405534101542));
#64241=CARTESIAN_POINT('Ctrl Pts',(-23.1576666666667,1.30259203804057,-0.755116444415858));
#64242=CARTESIAN_POINT('Ctrl Pts',(-23.0781230394496,1.33949458890747,0.687532623576175));
#64243=CARTESIAN_POINT('Ctrl Pts',(-22.9985794122326,0.145830612291159,
1.49855940646767));
#64244=CARTESIAN_POINT('Ctrl Pts',(-22.9190357850155,-1.1818049918733,0.932890038202402));
#64245=CARTESIAN_POINT('Ctrl Pts',(-22.8394921577985,-1.42374030500635,
-0.48980649862406));
#64246=CARTESIAN_POINT('Ctrl Pts',(-22.7599485305814,-0.357714258923656,
-1.46252773346581));
#64247=CARTESIAN_POINT('Ctrl Pts',(-22.6804049033643,1.03693662602006,-1.09165438478123));
#64248=CARTESIAN_POINT('Ctrl Pts',(-22.6008612761473,1.47897485118257,0.282099719538004));
#64249=CARTESIAN_POINT('Ctrl Pts',(-22.5213176489302,0.562308859152876,
1.39669452963493));
#64250=CARTESIAN_POINT('Ctrl Pts',(-22.4417740217131,-0.870938883867826,
1.22817438613619));
#64251=CARTESIAN_POINT('Ctrl Pts',(-22.3622303944961,-1.50407272807429,
-0.068644671002907));
#64252=CARTESIAN_POINT('Ctrl Pts',(-22.282686767279,-0.755445444318166,
-1.30240126030838));
#64253=CARTESIAN_POINT('Ctrl Pts',(-22.2031431400619,0.687194256371912,
-1.33966821123866));
#64254=CARTESIAN_POINT('Ctrl Pts',(-22.1235995128449,1.49852252305334,-0.146209131369364));
#64255=CARTESIAN_POINT('Ctrl Pts',(-22.0440558856278,0.933188522623136,
1.18156931385272));
#64256=CARTESIAN_POINT('Ctrl Pts',(-21.9645122584108,-0.489446857955352,
1.42386398066373));
#64257=CARTESIAN_POINT('Ctrl Pts',(-21.8849686311937,-1.46243733114162,
0.358083669939449));
#64258=CARTESIAN_POINT('Ctrl Pts',(-21.8054250039767,-1.09191627158435,
-1.03666085005814));
#64259=CARTESIAN_POINT('Ctrl Pts',(-21.7258813767596,0.281726133705207,
-1.47904606006083));
#64260=CARTESIAN_POINT('Ctrl Pts',(-21.6463377495426,1.39655245050451,-0.562661634718235));
#64261=CARTESIAN_POINT('Ctrl Pts',(-21.5667941223254,1.22839433892534,0.870628629376558));
#64262=CARTESIAN_POINT('Ctrl Pts',(-21.4872504951085,-0.0682647524631571,
1.50409001916943));
#64263=CARTESIAN_POINT('Ctrl Pts',(-21.4077068678913,-1.30221039947963,
0.755774396021086));
#64264=CARTESIAN_POINT('Ctrl Pts',(-21.3281632406743,-1.33984174809555,
-0.686855845322866));
#64265=CARTESIAN_POINT('Ctrl Pts',(-21.2486196134572,-0.146587641119035,
-1.4984855440294));
#64266=CARTESIAN_POINT('Ctrl Pts',(-21.1690759862402,1.18133356044495,-0.933486947504037));
#64267=CARTESIAN_POINT('Ctrl Pts',(-21.0895323590231,1.4239875654749,0.48908718605868));
#64268=CARTESIAN_POINT('Ctrl Pts',(-21.0099887318061,0.358453058108589,
1.46234683551015));
#64269=CARTESIAN_POINT('Ctrl Pts',(-20.930445104589,-1.03638500795459,1.09217808872037));
#64270=CARTESIAN_POINT('Ctrl Pts',(-20.8509014773719,-1.47911717457211,
-0.281352529897543));
#64271=CARTESIAN_POINT('Ctrl Pts',(-20.7713578501549,-0.563014374384315,
-1.39641028227043));
#64272=CARTESIAN_POINT('Ctrl Pts',(-20.6918142229378,0.870318319336921,
-1.22861421333977));
#64273=CARTESIAN_POINT('Ctrl Pts',(-20.6122705957208,1.50410721429972,0.0678848295679509));
#64274=CARTESIAN_POINT('Ctrl Pts',(-20.5327269685037,0.756103299503655,
1.30201945556648));
#64275=CARTESIAN_POINT('Ctrl Pts',(-20.4531833412866,-0.686517390450649,
1.34001519946707));
#64276=CARTESIAN_POINT('Ctrl Pts',(-20.3736397140696,-1.49844846939821,
0.146966141516047));
#64277=CARTESIAN_POINT('Ctrl Pts',(-20.2940960868525,-0.933785312826044,
-1.18109773166504));
#64278=CARTESIAN_POINT('Ctrl Pts',(-20.2145524596355,0.488727482956969,
-1.42411105943198));
#64279=CARTESIAN_POINT('Ctrl Pts',(-20.1350088324184,1.46225624657716,-0.358822423407484));
#64280=CARTESIAN_POINT('Ctrl Pts',(-20.0554652052013,1.09243983617262,1.03610909972699));
#64281=CARTESIAN_POINT('Ctrl Pts',(-19.9759215779843,-0.280978908138871,
1.47918819471189));
#64282=CARTESIAN_POINT('Ctrl Pts',(-19.8963779507672,-1.39626802494175,
0.563367078128633));
#64283=CARTESIAN_POINT('Ctrl Pts',(-19.8168343235502,-1.22883400936541,
-0.870007953768733));
#64284=CARTESIAN_POINT('Ctrl Pts',(-19.7372906963331,0.0675049023415035,
-1.50412431346408));
#64285=CARTESIAN_POINT('Ctrl Pts',(-19.657747069116,1.30182842858112,-0.756432154744866));
#64286=CARTESIAN_POINT('Ctrl Pts',(-19.578203441899,1.34018856534215,0.686178891776835));
#64287=CARTESIAN_POINT('Ctrl Pts',(-19.4986598146819,0.147344632536228,
1.49841129916212));
#64288=CARTESIAN_POINT('Ctrl Pts',(-19.4191161874649,-1.18086182752804,
0.934083618570138));
#64289=CARTESIAN_POINT('Ctrl Pts',(-19.3395725602478,-1.42423446252709,
-0.488367748673187));
#64290=CARTESIAN_POINT('Ctrl Pts',(-19.2600289330307,-0.35919176581259,
-1.46216556434843));
#64291=CARTESIAN_POINT('Ctrl Pts',(-19.1804853058137,1.03583312539295,-1.09270151392437));
#64292=CARTESIAN_POINT('Ctrl Pts',(-19.1009416785966,1.47925912047564,0.280605268453003));
#64293=CARTESIAN_POINT('Ctrl Pts',(-19.0213980513796,0.563719745928661,
1.39612567852757));
#64294=CARTESIAN_POINT('Ctrl Pts',(-18.9418544241625,-0.869697532691776,
1.22905372698828));
#64295=CARTESIAN_POINT('Ctrl Pts',(-18.8623107969454,-1.50414131666142,
-0.0671249708080826));
#64296=CARTESIAN_POINT('Ctrl Pts',(-18.7827671697284,-0.756760961723758,
-1.30163731853572));
#64297=CARTESIAN_POINT('Ctrl Pts',(-18.7032235425113,0.685840349323042,
-1.34036184570973));
#64298=CARTESIAN_POINT('Ctrl Pts',(-18.6236799152943,1.49837403332351,-0.14772311415545));
#64299=CARTESIAN_POINT('Ctrl Pts',(-18.5441362880772,0.934381864717273,
1.180625848049));
#64300=CARTESIAN_POINT('Ctrl Pts',(-18.4645926608601,-0.488007983230271,
1.42435777475235));
#64301=CARTESIAN_POINT('Ctrl Pts',(-18.3850490336431,-1.46207478882976,
0.359561085300321));
#64302=CARTESIAN_POINT('Ctrl Pts',(-18.305505406426,-1.09296312195894,-1.03555708497007));
#64303=CARTESIAN_POINT('Ctrl Pts',(-18.225961779209,0.280231610863807,-1.47932995185882));
#64304=CARTESIAN_POINT('Ctrl Pts',(-18.1464181519919,1.39598324303695,-0.56407237776192));
#64305=CARTESIAN_POINT('Ctrl Pts',(-18.0668745247749,1.22927336619432,0.869387056125872));
#64306=CARTESIAN_POINT('Ctrl Pts',(-17.9873308975578,-0.0667450349919024,
1.50415822389065));
#64307=CARTESIAN_POINT('Ctrl Pts',(-17.9077872703407,-1.30144612544251,
0.75708972041933));
#64308=CARTESIAN_POINT('Ctrl Pts',(-17.8282436431237,-1.34053504055875,
-0.685501763110848));
#64309=CARTESIAN_POINT('Ctrl Pts',(-17.7487000159066,-0.148101586349544,
-1.49833667188476));
#64310=CARTESIAN_POINT('Ctrl Pts',(-17.6691563886896,1.18038979324296,-0.934680051248432));
#64311=CARTESIAN_POINT('Ctrl Pts',(-17.5896127614725,1.42448099609989,0.48764818665119));
#64312=CARTESIAN_POINT('Ctrl Pts',(-17.5100691342554,0.359930381847136,
1.46198392002693));
#64313=CARTESIAN_POINT('Ctrl Pts',(-17.4305255070384,-1.03528097847597,
1.09322466025962));
#64314=CARTESIAN_POINT('Ctrl Pts',(-17.3509818798213,-1.47940068885692,
-0.279857935395096));
#64315=CARTESIAN_POINT('Ctrl Pts',(-17.2714382526042,-0.564424973605891,
-1.39584071847899));
#64316=CARTESIAN_POINT('Ctrl Pts',(-17.1918946253872,0.869076524090815,
-1.22949292696956));
#64317=CARTESIAN_POINT('Ctrl Pts',(-17.1123509981701,1.50417503515068,0.0663650949172277));
#64318=CARTESIAN_POINT('Ctrl Pts',(-17.0328073709531,0.757418430810628,
1.30125484931366));
#64319=CARTESIAN_POINT('Ctrl Pts',(-16.953263743736,-0.685163133161878,
1.34070814987817));
#64320=CARTESIAN_POINT('Ctrl Pts',(-16.873720116519,-1.49829921484824,0.148480049094385));
#64321=CARTESIAN_POINT('Ctrl Pts',(-16.7941764893019,-0.934978178144577,
-1.18015366312501));
#64322=CARTESIAN_POINT('Ctrl Pts',(-16.7146328620849,0.487288358958884,
-1.42460412656187));
#64323=CARTESIAN_POINT('Ctrl Pts',(-16.6350892348678,1.46189295794575,-0.360299655429449));
#64324=CARTESIAN_POINT('Ctrl Pts',(-16.5555456076507,1.09348612880975,1.03500480592826));
#64325=CARTESIAN_POINT('Ctrl Pts',(-16.4760019804336,-0.279484242070737,
1.47947133146543));
#64326=CARTESIAN_POINT('Ctrl Pts',(-16.3964583532166,-1.39569810486277,
0.564777533438098));
#64327=CARTESIAN_POINT('Ctrl Pts',(-16.3169147259995,-1.22971240929995,
-0.868765936606435));
#64328=CARTESIAN_POINT('Ctrl Pts',(-16.2373710987825,0.0659851506082771,
-1.50419175044046));
#64329=CARTESIAN_POINT('Ctrl Pts',(-16.1578274715654,1.30106349016138,-0.757747092876659));
#64330=CARTESIAN_POINT('Ctrl Pts',(-16.0782838443484,1.34088117365694,0.684824459497715));
#64331=CARTESIAN_POINT('Ctrl Pts',(-15.9987402171313,0.148858502365802,
1.49826166221637));
#64332=CARTESIAN_POINT('Ctrl Pts',(-15.9191965899142,-1.1799174577102,0.9352762453867));
#64333=CARTESIAN_POINT('Ctrl Pts',(-15.8396529626972,-1.4247271661304,-0.486928500176328));
#64334=CARTESIAN_POINT('Ctrl Pts',(-15.7601093354801,-0.360668906023721,
-1.461801902592));
#64335=CARTESIAN_POINT('Ctrl Pts',(-15.6805657082631,1.03472856734457,-1.09374752759263));
#64336=CARTESIAN_POINT('Ctrl Pts',(-15.601022081046,1.47954187967984,0.279110530914547));
#64337=CARTESIAN_POINT('Ctrl Pts',(-15.521478453829,0.565130057236024,1.3955554021974));
#64338=CARTESIAN_POINT('Ctrl Pts',(-15.4419348266119,-0.868455293692529,
1.22993181317151));
#64339=CARTESIAN_POINT('Ctrl Pts',(-15.3623911993948,-1.50420836975891,
-0.0656052020893142));
#64340=CARTESIAN_POINT('Ctrl Pts',(-15.2828475721778,-0.758075706596474,
-1.30087204799788));
#64341=CARTESIAN_POINT('Ctrl Pts',(-15.2033039449607,0.684485742139975,
-1.34105411188401));
#64342=CARTESIAN_POINT('Ctrl Pts',(-15.1237603177436,1.4982240139915,-0.149236946139704));
#64343=CARTESIAN_POINT('Ctrl Pts',(-15.0442166905266,0.935574252955802,
1.17968117701358));
#64344=CARTESIAN_POINT('Ctrl Pts',(-14.9646730633095,-0.486568610326457,
1.42485011479767));
#64345=CARTESIAN_POINT('Ctrl Pts',(-14.8851294360925,-1.4617107539715,0.361038133606384));
#64346=CARTESIAN_POINT('Ctrl Pts',(-14.8055858088754,-1.0940088565916,-1.03445226274248));
#64347=CARTESIAN_POINT('Ctrl Pts',(-14.7260421816584,0.278736801950366,
-1.47961233349565));
#64348=CARTESIAN_POINT('Ctrl Pts',(-14.6464985544413,1.39541261049198,-0.565482544977215));
#64349=CARTESIAN_POINT('Ctrl Pts',(-14.5669549272242,1.23015113857024,0.868144595368921));
#64350=CARTESIAN_POINT('Ctrl Pts',(-14.4874113000072,-0.065225249384528,
1.50422489310497));
#64351=CARTESIAN_POINT('Ctrl Pts',(-14.4078676727901,-1.30068052283537,
0.758404271949116));
#64352=CARTESIAN_POINT('Ctrl Pts',(-14.328324045573,-1.34122696454837,-0.684146981110283));
#64353=CARTESIAN_POINT('Ctrl Pts',(-14.248780418356,-0.149615380391841,
-1.49818627017608));
#64354=CARTESIAN_POINT('Ctrl Pts',(-14.1692367911389,1.17944482105025,-0.935872200832809));
#64355=CARTESIAN_POINT('Ctrl Pts',(-14.0896931639219,1.42497297255581,0.486208689432246));
#64356=CARTESIAN_POINT('Ctrl Pts',(-14.0101495367048,0.361407338153881,
1.46161951209009));
#64357=CARTESIAN_POINT('Ctrl Pts',(-13.9306059094878,-1.03417589213971,
1.09427011578995));
#64358=CARTESIAN_POINT('Ctrl Pts',(-13.8510622822707,-1.47968269290834,
-0.27836305520207));
#64359=CARTESIAN_POINT('Ctrl Pts',(-13.7715186550536,-0.56583499663915,
-1.39526972975562));
#64360=CARTESIAN_POINT('Ctrl Pts',(-13.6919750278366,0.867833841655458,
-1.23037038548215));
#64361=CARTESIAN_POINT('Ctrl Pts',(-13.6124314006195,1.50424132047758,0.0648452925182609));
#64362=CARTESIAN_POINT('Ctrl Pts',(-13.5328877734025,0.758732788913574,
1.30048891468607));
#64363=CARTESIAN_POINT('Ctrl Pts',(-13.4533441461854,-0.683808176430229,
1.34139973163898));
#64364=CARTESIAN_POINT('Ctrl Pts',(-13.3738005189683,-1.49814843077251,
0.149993805098161));
#64365=CARTESIAN_POINT('Ctrl Pts',(-13.2942568917513,-0.936170088998737,
-1.17920838983532));
#64366=CARTESIAN_POINT('Ctrl Pts',(-13.2147132645342,0.485848737516666,
-1.42509573939696));
#64367=CARTESIAN_POINT('Ctrl Pts',(-13.1351696373171,1.46152817695356,-0.361776519642661));
#64368=CARTESIAN_POINT('Ctrl Pts',(-13.0556260101001,1.09453130517105,1.03389945555383));
#64369=CARTESIAN_POINT('Ctrl Pts',(-12.976082382883,-0.277989290693522,
1.47975295791346));
#64370=CARTESIAN_POINT('Ctrl Pts',(-12.896538755666,-1.39512675999743,0.566187412199333));
#64371=CARTESIAN_POINT('Ctrl Pts',(-12.8169951284489,-1.23058955389324,
-0.867523032571931));
#64372=CARTESIAN_POINT('Ctrl Pts',(-12.7374515012319,0.0644653315146698,
-1.50425765187572));
#64373=CARTESIAN_POINT('Ctrl Pts',(-12.6579078740148,1.30029722356223,-0.759061257468899));
#64374=CARTESIAN_POINT('Ctrl Pts',(-12.5783642467977,1.34157241314479,0.683469328121443));
#64375=CARTESIAN_POINT('Ctrl Pts',(-12.4988206195807,0.150372220234496,
1.49811049578318));
#64376=CARTESIAN_POINT('Ctrl Pts',(-12.4192769923636,-1.17897188338383,
0.936467917434619));
#64377=CARTESIAN_POINT('Ctrl Pts',(-12.3397333651466,-1.42521841531332,
-0.485488754602712));
#64378=CARTESIAN_POINT('Ctrl Pts',(-12.2601897379295,-0.36214567804915,
-1.46143674856774));
#64379=CARTESIAN_POINT('Ctrl Pts',(-12.1806461107125,1.03362295300247,-1.09479242471822));
#64380=CARTESIAN_POINT('Ctrl Pts',(-12.1011024834954,1.47982312850652,0.277615508448512));
#64381=CARTESIAN_POINT('Ctrl Pts',(-12.0215588562783,0.566539791635272,
1.39498370122657));
#64382=CARTESIAN_POINT('Ctrl Pts',(-11.9420152290612,-0.867212168138187,
1.23080864378951));
#64383=CARTESIAN_POINT('Ctrl Pts',(-11.8624716018442,-1.50427388729832,
-0.0640853663980119));
#64384=CARTESIAN_POINT('Ctrl Pts',(-11.7829279746271,-0.759389677594182,
-1.30010544947607));
#64385=CARTESIAN_POINT('Ctrl Pts',(-11.7033843474101,0.683130436205578,
-1.34174500905481));
#64386=CARTESIAN_POINT('Ctrl Pts',(-11.623840720193,1.4980724652105,-0.150750625776684));
#64387=CARTESIAN_POINT('Ctrl Pts',(-11.544297092976,0.936765686121424,1.17873530171087));
#64388=CARTESIAN_POINT('Ctrl Pts',(-11.4647534657589,-0.485128740713296,
1.42534100029708));
#64389=CARTESIAN_POINT('Ctrl Pts',(-11.3852098385418,-1.46134522693848,
0.362514813349782));
#64390=CARTESIAN_POINT('Ctrl Pts',(-11.3056662113248,-1.09505347441479,
-1.03334638450329));
#64391=CARTESIAN_POINT('Ctrl Pts',(-11.2261225841077,0.277241708490902,
-1.47989320468303));
#64392=CARTESIAN_POINT('Ctrl Pts',(-11.1465789568907,1.39484055345213,-0.566892134924538));
#64393=CARTESIAN_POINT('Ctrl Pts',(-11.0670353296736,1.231027655157,0.866901248374095));
#64394=CARTESIAN_POINT('Ctrl Pts',(-10.9874917024566,-0.0637053971925516,
1.50429002674433));
#64395=CARTESIAN_POINT('Ctrl Pts',(-10.9079480752395,-1.29991359243979,
0.75971804926844));
#64396=CARTESIAN_POINT('Ctrl Pts',(-10.8284044480224,-1.34191751935805,
-0.682791500704204));
#64397=CARTESIAN_POINT('Ctrl Pts',(-10.7488608208054,-0.151129021700562,
-1.49803433905693));
#64398=CARTESIAN_POINT('Ctrl Pts',(-10.6693171935883,1.17849864483154,-0.937063395040135));
#64399=CARTESIAN_POINT('Ctrl Pts',(-10.5897735663713,1.42546349434039,0.484768695871397));
#64400=CARTESIAN_POINT('Ctrl Pts',(-10.5102299391542,0.362883925521062,
1.46125361207163));
#64401=CARTESIAN_POINT('Ctrl Pts',(-10.4306863119371,-1.03306975007396,
1.09531445424409));
#64402=CARTESIAN_POINT('Ctrl Pts',(-10.3511426847201,-1.4799631864385,-0.276867890844559));
#64403=CARTESIAN_POINT('Ctrl Pts',(-10.271599057503,-0.56724444204462,-1.39469731668325));
#64404=CARTESIAN_POINT('Ctrl Pts',(-10.1920554302859,0.866590273299441,
-1.23124658798177));
#64405=CARTESIAN_POINT('Ctrl Pts',(-10.1125118030689,1.50430607021276,0.0633254239225505));
#64406=CARTESIAN_POINT('Ctrl Pts',(-10.0329681758518,0.760046372470701,
1.29972165246565));
#64407=CARTESIAN_POINT('Ctrl Pts',(-9.95342454863479,-0.682452521638949,
1.34208994404347));
#64408=CARTESIAN_POINT('Ctrl Pts',(-9.8738809214177,-1.49799611732492,0.151507407982049));
#64409=CARTESIAN_POINT('Ctrl Pts',(-9.79433729420066,-0.937361044171762,
-1.17826191276097));
#64410=CARTESIAN_POINT('Ctrl Pts',(-9.71479366698359,0.484408620100003,
-1.42558589743541));
#64411=CARTESIAN_POINT('Ctrl Pts',(-9.63525003976654,1.461161903973,-0.363253014539415));
#64412=CARTESIAN_POINT('Ctrl Pts',(-9.55570641254947,1.09557536418953,1.0327930497321));
#64413=CARTESIAN_POINT('Ctrl Pts',(-9.47616278533242,-0.276494055533358,
1.4800330737685));
#64414=CARTESIAN_POINT('Ctrl Pts',(-9.39661915811535,-1.39455399092905,
0.567596712973026));
#64415=CARTESIAN_POINT('Ctrl Pts',(-9.3170755308983,-1.23146544224981,-0.866279242934072));
#64416=CARTESIAN_POINT('Ctrl Pts',(-9.23753190368124,0.0629454466121958,
-1.50432201770258));
#64417=CARTESIAN_POINT('Ctrl Pts',(-9.15798827646418,1.29952962956593,-0.760374647180021));
#64418=CARTESIAN_POINT('Ctrl Pts',(-9.07844464924712,1.34226228310006,0.682113499031458));
#64419=CARTESIAN_POINT('Ctrl Pts',(-8.99890102203006,0.15188578459698,1.49795780001685));
#64420=CARTESIAN_POINT('Ctrl Pts',(-8.919357394813,-1.17802510551424,0.937658633497361));
#64421=CARTESIAN_POINT('Ctrl Pts',(-8.83981376759594,-1.42570820957437,
-0.484048513422119));
#64422=CARTESIAN_POINT('Ctrl Pts',(-8.76027014037887,-0.363622080381272,
-1.46107010264844));
#64423=CARTESIAN_POINT('Ctrl Pts',(-8.68072651316182,1.03251628349535,-1.09583620423442));
#64424=CARTESIAN_POINT('Ctrl Pts',(-8.60118288594475,1.48010286666857,0.276120202581098));
#64425=CARTESIAN_POINT('Ctrl Pts',(-8.5216392587277,0.567948947687269,1.39441057619872));
#64426=CARTESIAN_POINT('Ctrl Pts',(-8.44209563151064,-0.865968157297839,
1.23168421794716));
#64427=CARTESIAN_POINT('Ctrl Pts',(-8.36255200429358,-1.50433786921275,
-0.0625654652857498));
#64428=CARTESIAN_POINT('Ctrl Pts',(-8.28300837707652,-0.760702873375501,
-1.29933752375286));
#64429=CARTESIAN_POINT('Ctrl Pts',(-8.20346474985946,0.681774432903392,
-1.34243453651684));
#64430=CARTESIAN_POINT('Ctrl Pts',(-8.12392112264241,1.49791938713518,-0.152264151521192));
#64431=CARTESIAN_POINT('Ctrl Pts',(-8.04437749542534,0.937956162997909,
1.17778822310643));
#64432=CARTESIAN_POINT('Ctrl Pts',(-7.96483386820828,-0.483688375860664,
1.42583043074948));
#64433=CARTESIAN_POINT('Ctrl Pts',(-7.88529024099122,-1.46097820810384,
0.363991123023073));
#64434=CARTESIAN_POINT('Ctrl Pts',(-7.80574661377416,-1.09609697436211,
-1.03223945138139));
#64435=CARTESIAN_POINT('Ctrl Pts',(-7.72620298655711,0.275746332011639,
-1.48017256513424));
#64436=CARTESIAN_POINT('Ctrl Pts',(-7.64665935934005,1.39426707250139,-0.568301146164932));
#64437=CARTESIAN_POINT('Ctrl Pts',(-7.56711573212298,1.23190291505985,0.865657016410631));
#64438=CARTESIAN_POINT('Ctrl Pts',(-7.48757210490593,-0.0621854799674716,
1.50435362474225));
#64439=CARTESIAN_POINT('Ctrl Pts',(-7.40802847768887,-1.29914533503867,
0.761031051036168));
#64440=CARTESIAN_POINT('Ctrl Pts',(-7.3284848504718,-1.34260670428284,-0.681435323276333));
#64441=CARTESIAN_POINT('Ctrl Pts',(-7.24894122325475,-0.15264250873053,
-1.4978808786824));
#64442=CARTESIAN_POINT('Ctrl Pts',(-7.16939759603768,1.17755126555268,-0.938253632654406));
#64443=CARTESIAN_POINT('Ctrl Pts',(-7.08985396882063,1.4259525609529,0.483328207438623));
#64444=CARTESIAN_POINT('Ctrl Pts',(-7.01031034160357,0.364360142441329,
1.46088622034507));
#64445=CARTESIAN_POINT('Ctrl Pts',(-6.9307667143865,-1.0319625534079,1.09635767455596));
#64446=CARTESIAN_POINT('Ctrl Pts',(-6.85122308716946,-1.48024216916106,
-0.275372443848858));
#64447=CARTESIAN_POINT('Ctrl Pts',(-6.77167945995239,-0.568653308383513,
-1.39412347984619));
#64448=CARTESIAN_POINT('Ctrl Pts',(-6.69213583273533,0.865345820292249,
-1.23212153357398));
#64449=CARTESIAN_POINT('Ctrl Pts',(-6.61259220551826,1.5043692842901,0.0618054906816298));
#64450=CARTESIAN_POINT('Ctrl Pts',(-6.53304857830121,0.76135918014107,1.29895306343564));
#64451=CARTESIAN_POINT('Ctrl Pts',(-6.45350495108415,-0.681096170171921,
1.34277878638706));
#64452=CARTESIAN_POINT('Ctrl Pts',(-6.37396132386708,-1.49784227466095,
0.15302085620091));
#64453=CARTESIAN_POINT('Ctrl Pts',(-6.29441769665004,-0.938551042447882,
-1.17731423286814));
#64454=CARTESIAN_POINT('Ctrl Pts',(-6.21487406943297,0.482968008178995,
-1.42607460017684));
#64455=CARTESIAN_POINT('Ctrl Pts',(-6.13533044221592,1.46079413937795,-0.364729138612472));
#64456=CARTESIAN_POINT('Ctrl Pts',(-6.05578681499884,1.09661830479939,1.03168558959253));
#64457=CARTESIAN_POINT('Ctrl Pts',(-5.9762431877818,-0.274998538116634,
1.48031167874459));
#64458=CARTESIAN_POINT('Ctrl Pts',(-5.89669956056473,-1.39397979824229,
0.569005434320529));
#64459=CARTESIAN_POINT('Ctrl Pts',(-5.81715593334767,-1.23234007347556,
-0.865034568962549));
#64460=CARTESIAN_POINT('Ctrl Pts',(-5.73761230613061,0.0614254974524097,
-1.50438484785532));
#64461=CARTESIAN_POINT('Ctrl Pts',(-5.65806867891355,1.29876070895606,-0.761687260669268));
#64462=CARTESIAN_POINT('Ctrl Pts',(-5.5785250516965,1.34295078281849,0.680756973611814));
#64463=CARTESIAN_POINT('Ctrl Pts',(-5.49898142447944,0.153399193908172,
1.49780357507327));
#64464=CARTESIAN_POINT('Ctrl Pts',(-5.41943779726237,-1.1770771250679,0.938848392359403));
#64465=CARTESIAN_POINT('Ctrl Pts',(-5.33989417004532,-1.42619654841353,
-0.482607778104791));
#64466=CARTESIAN_POINT('Ctrl Pts',(-5.26035054282825,-0.36509811151294,
-1.46070196520837));
#64467=CARTESIAN_POINT('Ctrl Pts',(-5.1808069156112,1.03140855995292,-1.09687886507572));
#64468=CARTESIAN_POINT('Ctrl Pts',(-5.10126328839413,1.48038109388043,0.274624614838766));
#64469=CARTESIAN_POINT('Ctrl Pts',(-5.02171966117708,0.569357523953502,
1.3938360276989));
#64470=CARTESIAN_POINT('Ctrl Pts',(-4.94217603396002,-0.8647232624414,1.23255853475063));
#64471=CARTESIAN_POINT('Ctrl Pts',(-4.86263240674296,-1.50440031543688,
-0.0610455003040735));
#64472=CARTESIAN_POINT('Ctrl Pts',(-4.7830887795259,-0.762015292599876,
-1.29856827161219));
#64473=CARTESIAN_POINT('Ctrl Pts',(-4.70354515230884,0.680417733617677,
-1.34312269356619));
#64474=CARTESIAN_POINT('Ctrl Pts',(-4.62400152509178,1.49776477992184,-0.15377752182816));
#64475=CARTESIAN_POINT('Ctrl Pts',(-4.54445789787472,0.939145682369963,
1.17683994216708));
#64476=CARTESIAN_POINT('Ctrl Pts',(-4.46491427065766,-0.482247517238938,
1.42631840565522));
#64477=CARTESIAN_POINT('Ctrl Pts',(-4.3853706434406,-1.46060969784225,0.365467061119176));
#64478=CARTESIAN_POINT('Ctrl Pts',(-4.30582701622354,-1.09713935536833,
-1.03113146450678));
#64479=CARTESIAN_POINT('Ctrl Pts',(-4.22628338900648,0.274250674039124,
-1.48045041456411));
#64480=CARTESIAN_POINT('Ctrl Pts',(-4.14673976178942,1.39369216822517,-0.569709577260021));
#64481=CARTESIAN_POINT('Ctrl Pts',(-4.06719613457236,1.23277691738527,0.864411900748698));
#64482=CARTESIAN_POINT('Ctrl Pts',(-3.9876525073553,-0.0606654992609097,
1.5044156870338));
#64483=CARTESIAN_POINT('Ctrl Pts',(-3.90810888013824,-1.29837575141631,
0.762343275911907));
#64484=CARTESIAN_POINT('Ctrl Pts',(-3.82856525292117,-1.34329451861918,
-0.680078450211127));
#64485=CARTESIAN_POINT('Ctrl Pts',(-3.74902162570413,-0.154155839936718,
-1.49772588920915));
#64486=CARTESIAN_POINT('Ctrl Pts',(-3.66947799848706,1.17660268418084,-0.939442912460569));
#64487=CARTESIAN_POINT('Ctrl Pts',(-3.58993437127,1.42644017189407,0.481887225604464));
#64488=CARTESIAN_POINT('Ctrl Pts',(-3.51039074405294,0.365835987407674,
1.46051733728545));
#64489=CARTESIAN_POINT('Ctrl Pts',(-3.43084711683588,-1.03085430327181,
1.09739977566059));
#64490=CARTESIAN_POINT('Ctrl Pts',(-3.35130348961882,-1.48051964079121,
-0.2738767157416));
#64491=CARTESIAN_POINT('Ctrl Pts',(-3.27175986240177,-0.570061594217579,
-1.39354821983028));
#64492=CARTESIAN_POINT('Ctrl Pts',(-3.1922162351847,0.864100483904304,-1.23299522136551));
#64493=CARTESIAN_POINT('Ctrl Pts',(-3.11267260796765,1.50443096264505,0.0602854943470151));
#64494=CARTESIAN_POINT('Ctrl Pts',(-3.03312898075058,0.762671210584582,
1.29818314838084));
#64495=CARTESIAN_POINT('Ctrl Pts',(-2.95358535353353,-0.679739123413961,
1.34346625796621));
#64496=CARTESIAN_POINT('Ctrl Pts',(-2.87404172631646,-1.49768690293735,
0.154534148210354));
#64497=CARTESIAN_POINT('Ctrl Pts',(-2.79449809909941,-0.939740082612886,
-1.17636535112546));
#64498=CARTESIAN_POINT('Ctrl Pts',(-2.71495447188235,0.481526903225423,
-1.42656184712011));
#64499=CARTESIAN_POINT('Ctrl Pts',(-2.63541084466529,1.46042488354174,-0.366204890359183));
#64500=CARTESIAN_POINT('Ctrl Pts',(-2.55586721744823,1.09766012593993,1.03057707627376));
#64501=CARTESIAN_POINT('Ctrl Pts',(-2.47632359023116,-0.273502739977664,
1.48058877254194));
#64502=CARTESIAN_POINT('Ctrl Pts',(-2.39677996301411,-1.39340418250887,
0.570413574832941));
#64503=CARTESIAN_POINT('Ctrl Pts',(-2.31723633579704,-1.23321344670508,
-0.863789011983425));
#64504=CARTESIAN_POINT('Ctrl Pts',(-2.23769270857999,0.0599054856391566,
-1.50444614216461));
#64505=CARTESIAN_POINT('Ctrl Pts',(-2.15814908136293,1.2979904624185,-0.76299909679633));
#64506=CARTESIAN_POINT('Ctrl Pts',(-2.07860545414587,1.34363791178529,0.679399753626298));
#64507=CARTESIAN_POINT('Ctrl Pts',(-1.99906182692881,0.154912446266186,
1.4976478203906));
#64508=CARTESIAN_POINT('Ctrl Pts',(-1.91951819971175,-1.17612794233516,
0.940037194171402));
#64509=CARTESIAN_POINT('Ctrl Pts',(-1.83997457249469,-1.42668343261808,
-0.481166552712769));
#64510=CARTESIAN_POINT('Ctrl Pts',(-1.76043094527763,-0.366573767496878,
-1.46033233170502));
#64511=CARTESIAN_POINT('Ctrl Pts',(-1.68088731806057,1.03029977887392,-1.09792041551294));
#64512=CARTESIAN_POINT('Ctrl Pts',(-1.60134369084351,1.48065781864995,0.27312876446696));
#64513=CARTESIAN_POINT('Ctrl Pts',(-1.52180006362645,0.570765502308645,
1.3932600226829));
#64514=CARTESIAN_POINT('Ctrl Pts',(-1.44225643640939,-0.863477453166383,
1.23343165713992));
#64515=CARTESIAN_POINT('Ctrl Pts',(-1.36271280919234,-1.50446128602429,
-0.0595255941614048));
#64516=CARTESIAN_POINT('Ctrl Pts',(-1.28316918197527,-0.76332681982241,
-1.29779746387891));
#64517=CARTESIAN_POINT('Ctrl Pts',(-1.20362555475822,0.679060123157279,
-1.34380991597466));
#64518=CARTESIAN_POINT('Ctrl Pts',(-1.12408192754115,1.49760905479862,-0.155289906706672));
#64519=CARTESIAN_POINT('Ctrl Pts',(-1.04453830032409,0.94033346279502,1.17588888743665));
#64520=CARTESIAN_POINT('Ctrl Pts',(-0.964994673107034,-0.480804685414002,
1.4268079090415));
#64521=CARTESIAN_POINT('Ctrl Pts',(-0.885451045889976,-1.46024250734839,
0.366936961380079));
#64522=CARTESIAN_POINT('Ctrl Pts',(-0.805907418672918,-1.09817528131783,
-1.03001167307692));
#64523=CARTESIAN_POINT('Ctrl Pts',(-0.726363791455856,0.272744609926045,
-1.48074716033771));
#64524=CARTESIAN_POINT('Ctrl Pts',(-0.646820164238799,1.3931350613471,-0.571078691880378));
#64525=CARTESIAN_POINT('Ctrl Pts',(-0.567276537021739,1.23361317856029,
0.86309237935622));
#64526=CARTESIAN_POINT('Ctrl Pts',(-0.487732909804683,-0.0590761934204603,
1.50461578833112));
#64527=CARTESIAN_POINT('Ctrl Pts',(-0.408189282587616,-1.29773645562838,
0.763389596137374));
#64528=CARTESIAN_POINT('Ctrl Pts',(-0.328645655370557,-1.34372989411186,
-0.678215903148311));
#64529=CARTESIAN_POINT('Ctrl Pts',(-0.249102028153499,-0.15615620871939,
-1.49854272923124));
#64530=CARTESIAN_POINT('Ctrl Pts',(-0.169558400936439,1.17666683856934,
-0.938658107396819));
#64531=CARTESIAN_POINT('Ctrl Pts',(-0.116529316125066,1.34179608678025,
0.00423245967186979));
#64532=CARTESIAN_POINT('Ctrl Pts',(-0.0900147737193787,1.20644987911676,
0.406211384846794));
#64533=CARTESIAN_POINT('Ctrl Pts',(-34.6365,0.684664424539256,-0.958295198918542));
#64534=CARTESIAN_POINT('Ctrl Pts',(-34.6099854575943,1.00396030307469,-0.7301707867521));
#64535=CARTESIAN_POINT('Ctrl Pts',(-34.556956372783,1.39099115610471,0.0663998364373292));
#64536=CARTESIAN_POINT('Ctrl Pts',(-34.4774127455658,0.694817159188923,
1.20840932237519));
#64537=CARTESIAN_POINT('Ctrl Pts',(-34.3978691183489,-0.640240458638742,
1.23665911837698));
#64538=CARTESIAN_POINT('Ctrl Pts',(-34.3183254911317,-1.38682292844981,
0.130635890290045));
#64539=CARTESIAN_POINT('Ctrl Pts',(-34.2387818639147,-0.859516886189572,
-1.09634891418097));
#64540=CARTESIAN_POINT('Ctrl Pts',(-34.1592382366976,0.457492926185055,
-1.31564139210814));
#64541=CARTESIAN_POINT('Ctrl Pts',(-34.0796946094806,1.3541695165413,-0.326543447000047));
#64542=CARTESIAN_POINT('Ctrl Pts',(-34.0001509822635,1.00682106773482,0.962681709799215));
#64543=CARTESIAN_POINT('Ctrl Pts',(-33.9206073550465,-0.265485630343504,
1.36743779586005));
#64544=CARTESIAN_POINT('Ctrl Pts',(-33.8410637278294,-1.29388966381863,
0.515994903012744));
#64545=CARTESIAN_POINT('Ctrl Pts',(-33.7615201006123,-1.13362686059144,
-0.809502282827959));
#64546=CARTESIAN_POINT('Ctrl Pts',(-33.6819764733953,0.0680777368036397,
-1.39131546907066));
#64547=CARTESIAN_POINT('Ctrl Pts',(-33.6024328461782,1.20723976173548,-0.694960952389941));
#64548=CARTESIAN_POINT('Ctrl Pts',(-33.5228892189612,1.23733558104474,0.639843063744817));
#64549=CARTESIAN_POINT('Ctrl Pts',(-33.4433455917441,0.130716022946506,
1.38683466763195));
#64550=CARTESIAN_POINT('Ctrl Pts',(-33.3638019645271,-1.09598955901368,
0.859770194715907));
#64551=CARTESIAN_POINT('Ctrl Pts',(-33.2842583373099,-1.31583182073299,
-0.457148161455002));
#64552=CARTESIAN_POINT('Ctrl Pts',(-33.204714710093,-0.326846022470247,
-1.35409354000658));
#64553=CARTESIAN_POINT('Ctrl Pts',(-33.1251710828758,0.962406571507915,
-1.00706075074908));
#64554=CARTESIAN_POINT('Ctrl Pts',(-33.0456274556588,1.36751576661517,0.26513840054929));
#64555=CARTESIAN_POINT('Ctrl Pts',(-32.9660838284418,0.516315940709615,
1.29376024423113));
#64556=CARTESIAN_POINT('Ctrl Pts',(-32.8865402012247,-0.809212871355991,
1.13383079342446));
#64557=CARTESIAN_POINT('Ctrl Pts',(-32.8069965740076,-1.39133422266715,
-0.0677260339843446));
#64558=CARTESIAN_POINT('Ctrl Pts',(-32.7274529467905,-0.69526502492905,
-1.20706432189118));
#64559=CARTESIAN_POINT('Ctrl Pts',(-32.6479093195736,0.639530057869942,
-1.23749708685117));
#64560=CARTESIAN_POINT('Ctrl Pts',(-32.5683656923564,1.38680183990368,-0.131066360639972));
#64561=CARTESIAN_POINT('Ctrl Pts',(-32.4888220651394,0.860046881755779,
1.09577237368332));
#64562=CARTESIAN_POINT('Ctrl Pts',(-32.4092784379223,-0.456815713582613,
1.31594723981434));
#64563=CARTESIAN_POINT('Ctrl Pts',(-32.3297348107053,-1.35401097246879,
0.327188050574965));
#64564=CARTESIAN_POINT('Ctrl Pts',(-32.2501911834881,-1.00730379652143,
-0.962152168572661));
#64565=CARTESIAN_POINT('Ctrl Pts',(-32.1706475562712,0.264792959390405,
-1.3675826931817));
#64566=CARTESIAN_POINT('Ctrl Pts',(-32.0911039290541,1.29362979082703,-0.516642718223328));
#64567=CARTESIAN_POINT('Ctrl Pts',(-32.011560301837,1.1340351551021,0.808926449684369));
#64568=CARTESIAN_POINT('Ctrl Pts',(-31.93201667462,-0.0673745908983318,
1.39135128508784));
#64569=CARTESIAN_POINT('Ctrl Pts',(-31.8524730474029,-1.20688866591361,
0.695569897350098));
#64570=CARTESIAN_POINT('Ctrl Pts',(-31.7729294201859,-1.23765858699842,
-0.639217455987783));
#64571=CARTESIAN_POINT('Ctrl Pts',(-31.6933857929688,-0.131416651354211,
-1.38676868934885));
#64572=CARTESIAN_POINT('Ctrl Pts',(-31.6138421657517,1.09555509809422,-0.860323637389223));
#64573=CARTESIAN_POINT('Ctrl Pts',(-31.5342985385347,1.31606258565414,0.45648330161381));
#64574=CARTESIAN_POINT('Ctrl Pts',(-31.4547549113176,0.327530052156675,
1.35392828426963));
#64575=CARTESIAN_POINT('Ctrl Pts',(-31.3752112841005,-0.961897701274149,
1.00754679608168));
#64576=CARTESIAN_POINT('Ctrl Pts',(-31.2956676568835,-1.36764953406056,
-0.264447510850282));
#64577=CARTESIAN_POINT('Ctrl Pts',(-31.2161240296664,-0.516969461947962,
-1.29349924987385));
#64578=CARTESIAN_POINT('Ctrl Pts',(-31.1365804024493,0.808639975965988,
-1.13423944706605));
#64579=CARTESIAN_POINT('Ctrl Pts',(-31.0570367752323,1.39136825896598,0.067023144904906));
#64580=CARTESIAN_POINT('Ctrl Pts',(-30.9774931480152,0.695874725271205,
1.20671293220041));
#64581=CARTESIAN_POINT('Ctrl Pts',(-30.8979495207982,-0.638904813258247,
1.23782000856604));
#64582=CARTESIAN_POINT('Ctrl Pts',(-30.8184058935811,-1.38673545034811,
0.131766933480272));
#64583=CARTESIAN_POINT('Ctrl Pts',(-30.7388622663641,-0.860600338114134,
-1.09533775249866));
#64584=CARTESIAN_POINT('Ctrl Pts',(-30.659318639147,0.456150860510873,-1.31617784758222));
#64585=CARTESIAN_POINT('Ctrl Pts',(-30.57977501193,1.35384550969123,-0.327872032811375));
#64586=CARTESIAN_POINT('Ctrl Pts',(-30.5002313847129,1.00778973135526,0.961643172588391));
#64587=CARTESIAN_POINT('Ctrl Pts',(-30.4206877574958,-0.264102045436351,
1.3677162876881));
#64588=CARTESIAN_POINT('Ctrl Pts',(-30.3411441302788,-1.2933686263928,0.517296172684261));
#64589=CARTESIAN_POINT('Ctrl Pts',(-30.2616005030617,-1.13444366666221,
-0.808353450651991));
#64590=CARTESIAN_POINT('Ctrl Pts',(-30.1820568758447,0.0666716946350309,
-1.39138514407244));
#64591=CARTESIAN_POINT('Ctrl Pts',(-30.1025132486276,1.2065371214959,-0.696179508793066));
#64592=CARTESIAN_POINT('Ctrl Pts',(-30.0229696214105,1.23798135115748,0.638592129764595));
#64593=CARTESIAN_POINT('Ctrl Pts',(-29.9434259941935,0.132117207199287,
1.38670212287024));
#64594=CARTESIAN_POINT('Ctrl Pts',(-29.8638823669764,-1.09512033701773,
0.860876983930424));
#64595=CARTESIAN_POINT('Ctrl Pts',(-29.7843387397594,-1.31629302553474,
-0.455818390304285));
#64596=CARTESIAN_POINT('Ctrl Pts',(-29.7047951125423,-0.328213992546994,
-1.35376264873402));
#64597=CARTESIAN_POINT('Ctrl Pts',(-29.6252514853253,0.96138858254731,-1.00803260232924));
#64598=CARTESIAN_POINT('Ctrl Pts',(-29.5457078581082,1.3677829540518,0.263756563172021));
#64599=CARTESIAN_POINT('Ctrl Pts',(-29.4661642308912,0.517622850415724,
1.29323792039148));
#64600=CARTESIAN_POINT('Ctrl Pts',(-29.386620603674,-0.808066873762948,
1.13464781387793));
#64601=CARTESIAN_POINT('Ctrl Pts',(-29.3070769764571,-1.39140194040491,
-0.066320240111329));
#64602=CARTESIAN_POINT('Ctrl Pts',(-29.2275333492399,-0.696484247896873,
-1.20636123381121));
#64603=CARTESIAN_POINT('Ctrl Pts',(-29.1479897220229,0.638279405527112,
-1.23814261476251));
#64604=CARTESIAN_POINT('Ctrl Pts',(-29.0684460948058,1.38666870691719,-0.132467472488888));
#64605=CARTESIAN_POINT('Ctrl Pts',(-28.9889024675888,0.86115357482053,1.0949028516653));
#64606=CARTESIAN_POINT('Ctrl Pts',(-28.9093588403717,-0.455485891015299,
1.31640811950435));
#64607=CARTESIAN_POINT('Ctrl Pts',(-28.8298152131546,-1.35367970140324,
0.328555931341711));
#64608=CARTESIAN_POINT('Ctrl Pts',(-28.7502715859376,-1.00827540898812,
-0.961133931167149));
#64609=CARTESIAN_POINT('Ctrl Pts',(-28.6707279587205,0.26341106407934,-1.3678495331474));
#64610=CARTESIAN_POINT('Ctrl Pts',(-28.5911843315035,1.29310713187823,-0.517949495121513));
#64611=CARTESIAN_POINT('Ctrl Pts',(-28.5116407042864,1.13485188870017,0.807780245317151));
#64612=CARTESIAN_POINT('Ctrl Pts',(-28.4320970770694,-0.0659687813562216,
1.39141864796234));
#64613=CARTESIAN_POINT('Ctrl Pts',(-28.3525534498523,-1.20618526915755,
0.696788942563181));
#64614=CARTESIAN_POINT('Ctrl Pts',(-28.2730098226353,-1.23830379937083,
-0.637966640565749));
#64615=CARTESIAN_POINT('Ctrl Pts',(-28.1934661954182,-0.132817729326718,
-1.38663520249108));
#64616=CARTESIAN_POINT('Ctrl Pts',(-28.1139225682011,1.09468529645522,-0.861430110766812));
#64617=CARTESIAN_POINT('Ctrl Pts',(-28.0343789409841,1.31652312948372,0.455153362665139));
#64618=CARTESIAN_POINT('Ctrl Pts',(-27.954835313767,0.32889784917371,1.35359666770419));
#64619=CARTESIAN_POINT('Ctrl Pts',(-27.8752916865499,-0.960879218464155,
1.00851815131642));
#64620=CARTESIAN_POINT('Ctrl Pts',(-27.7957480593329,-1.36791602497067,
-0.26306554818035));
#64621=CARTESIAN_POINT('Ctrl Pts',(-27.7162044321158,-0.51827610678078,
-1.2929762608614));
#64622=CARTESIAN_POINT('Ctrl Pts',(-27.6366608048988,0.807493565332879,
-1.13505589111593));
#64623=CARTESIAN_POINT('Ctrl Pts',(-27.5571171776817,1.39143526674366,0.0656173183921381));
#64624=CARTESIAN_POINT('Ctrl Pts',(-27.4775735504646,0.697093592772551,
1.20600922754614));
#64625=CARTESIAN_POINT('Ctrl Pts',(-27.3980299232476,-0.637653834900464,
1.23846490497216));
#64626=CARTESIAN_POINT('Ctrl Pts',(-27.3184862960305,-1.38660160959405,
0.133167977690434));
#64627=CARTESIAN_POINT('Ctrl Pts',(-27.2389426688135,-0.861706591751621,
-1.09446767140139));
#64628=CARTESIAN_POINT('Ctrl Pts',(-27.1593990415964,0.454820805275012,
-1.3166380554655));
#64629=CARTESIAN_POINT('Ctrl Pts',(-27.0798554143794,1.35351354764217,-0.329239746021173));
#64630=CARTESIAN_POINT('Ctrl Pts',(-27.0003117871623,1.00876082929865,0.960624444454579));
#64631=CARTESIAN_POINT('Ctrl Pts',(-26.9207681599452,-0.262720015497096,
1.36798242951735));
#64632=CARTESIAN_POINT('Ctrl Pts',(-26.8412245327282,-1.29284530734934,
0.518602685372692));
#64633=CARTESIAN_POINT('Ctrl Pts',(-26.761680905511,-1.13525982111218,-0.807206833828431));
#64634=CARTESIAN_POINT('Ctrl Pts',(-26.6821372782941,0.065265851241496,
-1.39145179674781));
#64635=CARTESIAN_POINT('Ctrl Pts',(-26.6025936510769,1.20583310898822,-0.697398198505544));
#64636=CARTESIAN_POINT('Ctrl Pts',(-26.52305002386,1.23862593155623,0.637340988551213));
#64637=CARTESIAN_POINT('Ctrl Pts',(-26.4435063966428,0.133518217557687,
1.38656792822826));
#64638=CARTESIAN_POINT('Ctrl Pts',(-26.3639627694258,-1.09424997651769,
0.861983017757319));
#64639=CARTESIAN_POINT('Ctrl Pts',(-26.2844191422087,-1.31675289744237,
-0.454488218866141));
#64640=CARTESIAN_POINT('Ctrl Pts',(-26.2048755149917,-0.329581621862289,
-1.35343034122248));
#64641=CARTESIAN_POINT('Ctrl Pts',(-26.1253318877746,0.960369609154678,
-1.00900344291933));
#64642=CARTESIAN_POINT('Ctrl Pts',(-26.0457882605576,1.36804874678321,0.262374466051626));
#64643=CARTESIAN_POINT('Ctrl Pts',(-25.9662446333405,0.518929230876408,
1.2927142713504));
#64644=CARTESIAN_POINT('Ctrl Pts',(-25.8867010061234,-0.806920050822095,
1.13546367867592));
#64645=CARTESIAN_POINT('Ctrl Pts',(-25.8071573789064,-1.39146823797373,
-0.0649143799267269));
#64646=CARTESIAN_POINT('Ctrl Pts',(-25.7276137516893,-0.697702759742729,
-1.20565691349503));
#64647=CARTESIAN_POINT('Ctrl Pts',(-25.6480701244723,0.637028101537958,
-1.23878687911276));
#64648=CARTESIAN_POINT('Ctrl Pts',(-25.5685264972552,1.38653415839583,-0.133868448906134));
#64649=CARTESIAN_POINT('Ctrl Pts',(-25.4889828700381,0.862259388766268,
1.09403221181801));
#64650=CARTESIAN_POINT('Ctrl Pts',(-25.4094392428211,-0.454155603459752,
1.31686765540699));
#64651=CARTESIAN_POINT('Ctrl Pts',(-25.329895615604,-1.35334704845044,0.329923476675237));
#64652=CARTESIAN_POINT('Ctrl Pts',(-25.250351988387,-1.00924599216297,-0.960114712580717));
#64653=CARTESIAN_POINT('Ctrl Pts',(-25.1708083611699,0.262028899865992,
-1.36811497676401));
#64654=CARTESIAN_POINT('Ctrl Pts',(-25.0912647339529,1.29258315287295,-0.519255743271084));
#64655=CARTESIAN_POINT('Ctrl Pts',(-25.0117211067357,1.13566746379413,0.806633216332175));
#64656=CARTESIAN_POINT('Ctrl Pts',(-24.9321774795188,-0.0645629044702633,
1.39148459042037));
#64657=CARTESIAN_POINT('Ctrl Pts',(-24.8526338523016,-1.20548064107781,
0.698007276464662));
#64658=CARTESIAN_POINT('Ctrl Pts',(-24.7730902250846,-1.23894774763147,
-0.63671517388067));
#64659=CARTESIAN_POINT('Ctrl Pts',(-24.6935465978676,-0.134218671713418,
-1.38650030009895));
#64660=CARTESIAN_POINT('Ctrl Pts',(-24.6140029706505,1.09381437731624,-0.862535704760827));
#64661=CARTESIAN_POINT('Ctrl Pts',(-24.5344593434334,1.31698232935204,0.453822959077054));
#64662=CARTESIAN_POINT('Ctrl Pts',(-24.4549157162164,0.330265310438215,
1.35326366933134));
#64663=CARTESIAN_POINT('Ctrl Pts',(-24.3753720889993,-0.959859754748951,
1.00948847701412));
#64664=CARTESIAN_POINT('Ctrl Pts',(-24.2958284617822,-1.36818111945554,
-0.261683316962251));
#64665=CARTESIAN_POINT('Ctrl Pts',(-24.2162848345652,-0.519582222535895,
-1.29245195192535));
#64666=CARTESIAN_POINT('Ctrl Pts',(-24.1367412073481,0.806346330376981,
-1.13587117645381));
#64667=CARTESIAN_POINT('Ctrl Pts',(-24.057197580131,1.39150085408669,0.0642114248945288));
#64668=CARTESIAN_POINT('Ctrl Pts',(-23.977653952914,0.698311748651915,1.20530429174781));
#64669=CARTESIAN_POINT('Ctrl Pts',(-23.8981103256969,-0.636402205599313,
1.2391085371021));
#64670=CARTESIAN_POINT('Ctrl Pts',(-23.8185666984799,-1.38646635333975,
0.134568885957192));
#64671=CARTESIAN_POINT('Ctrl Pts',(-23.7390230712628,-0.862811965723368,
-1.0935964730263));
#64672=CARTESIAN_POINT('Ctrl Pts',(-23.6594794440458,0.453490285739293,
-1.31709691927021));
#64673=CARTESIAN_POINT('Ctrl Pts',(-23.5799358168287,1.35318020387053,-0.330607123129397));
#64674=CARTESIAN_POINT('Ctrl Pts',(-23.5003921896117,1.00973089745727,0.959604735675643));
#64675=CARTESIAN_POINT('Ctrl Pts',(-23.4208485623946,-0.261337717362417,
1.36824717485357));
#64676=CARTESIAN_POINT('Ctrl Pts',(-23.3413049351776,-1.29232066851596,
0.519908668650037));
#64677=CARTESIAN_POINT('Ctrl Pts',(-23.2617613079605,-1.13607481664197,
-0.806059392974791));
#64678=CARTESIAN_POINT('Ctrl Pts',(-23.1822176807434,0.063859941221911,
-1.39151702897166));
#64679=CARTESIAN_POINT('Ctrl Pts',(-23.1026740535264,1.20512786551627,-0.698616176285083));
#64680=CARTESIAN_POINT('Ctrl Pts',(-23.0231304263093,1.23926924751441,0.636089196713827));
#64681=CARTESIAN_POINT('Ctrl Pts',(-22.9435867990922,0.134919091615136,
1.38643231812041));
#64682=CARTESIAN_POINT('Ctrl Pts',(-22.8640431718752,-1.09337849896205,
0.863088171636293));
#64683=CARTESIAN_POINT('Ctrl Pts',(-22.7844995446581,-1.31721142515419,
-0.453157583467666));
#64684=CARTESIAN_POINT('Ctrl Pts',(-22.7049559174411,-0.330948914727013,
-1.35309665207331));
#64685=CARTESIAN_POINT('Ctrl Pts',(-22.625412290224,0.959349655377068,-1.00997325347698));
#64686=CARTESIAN_POINT('Ctrl Pts',(-22.5458686630069,1.36831314295389,0.260992101088554));
#64687=CARTESIAN_POINT('Ctrl Pts',(-22.4663250357899,0.520235081592649,
1.29218930265316));
#64688=CARTESIAN_POINT('Ctrl Pts',(-22.3867814085728,-0.805772404143914,
1.13627838434563));
#64689=CARTESIAN_POINT('Ctrl Pts',(-22.3072377813558,-1.39153311507424,
-0.0635084534748757));
#64690=CARTESIAN_POINT('Ctrl Pts',(-22.2276941541387,-0.69892055934474,
-1.20495136239444));
#64691=CARTESIAN_POINT('Ctrl Pts',(-22.1481505269216,0.635776147244211,
-1.23942987885813));
#64692=CARTESIAN_POINT('Ctrl Pts',(-22.0686068997046,1.38639819444309,-0.135269288664905));
#64693=CARTESIAN_POINT('Ctrl Pts',(-21.9890632724875,0.863364322481949,
1.09316045513743));
#64694=CARTESIAN_POINT('Ctrl Pts',(-21.9095196452704,-0.4528248522834,1.31732584699667));
#64695=CARTESIAN_POINT('Ctrl Pts',(-21.8299760180534,-1.35301301394502,
0.331290685209222));
#64696=CARTESIAN_POINT('Ctrl Pts',(-21.7504323908363,-1.01021554505779,
-0.959094513869495));
#64697=CARTESIAN_POINT('Ctrl Pts',(-21.6708887636193,0.260646468162729,
-1.36837902375229));
#64698=CARTESIAN_POINT('Ctrl Pts',(-21.5913451364022,1.29205785434534,-0.520561461342927));
#64699=CARTESIAN_POINT('Ctrl Pts',(-21.5118015091852,1.13648187955178,0.805485363902682));
#64700=CARTESIAN_POINT('Ctrl Pts',(-21.4322578819681,-0.0631569616758272,
1.3915491123934));
#64701=CARTESIAN_POINT('Ctrl Pts',(-21.352714254751,-1.2047747823936,0.699224897811445));
#64702=CARTESIAN_POINT('Ctrl Pts',(-21.273170627534,-1.23959043112302,-0.635463057210422));
#64703=CARTESIAN_POINT('Ctrl Pts',(-21.1936270003169,-0.135619477084131,
-1.38636398230999));
#64704=CARTESIAN_POINT('Ctrl Pts',(-21.1140833730999,1.09294234156633,-0.863640418242735));
#64705=CARTESIAN_POINT('Ctrl Pts',(-21.0345397458828,1.31744018479035,0.452492092207748));
#64706=CARTESIAN_POINT('Ctrl Pts',(-20.9549961186657,0.331632434554235,
1.352929289491));
#64707=CARTESIAN_POINT('Ctrl Pts',(-20.8754524914487,-0.958839311169214,
1.01045777218423));
#64708=CARTESIAN_POINT('Ctrl Pts',(-20.7959088642316,-1.36844481724457,
-0.260300818606975));
#64709=CARTESIAN_POINT('Ctrl Pts',(-20.7163652370146,-0.520887807880025,
-1.29192632360089));
#64710=CARTESIAN_POINT('Ctrl Pts',(-20.6368216097975,0.80519827226939,-1.13668530224745));
#64711=CARTESIAN_POINT('Ctrl Pts',(-20.5572779825804,1.39156502092812,0.06280546584721));
#64712=CARTESIAN_POINT('Ctrl Pts',(-20.4777343553634,0.699529191665802,
1.20459812552501));
#64713=CARTESIAN_POINT('Ctrl Pts',(-20.3981907281463,-0.635149926632454,
1.23975090429883));
#64714=CARTESIAN_POINT('Ctrl Pts',(-20.3186471009293,-1.38632968172327,
0.135969656850494));
#64715=CARTESIAN_POINT('Ctrl Pts',(-20.2391034737122,-0.863916458901017,
-1.09272415826269));
#64716=CARTESIAN_POINT('Ctrl Pts',(-20.1595598464952,0.452159303261918,
-1.31755443852794));
#64717=CARTESIAN_POINT('Ctrl Pts',(-20.0800162192781,1.35284547871658,-0.331974162740232));
#64718=CARTESIAN_POINT('Ctrl Pts',(-20.0004725920611,1.01069993484086,0.958584047292498));
#64719=CARTESIAN_POINT('Ctrl Pts',(-19.920928964844,-0.259955152443364,
1.36851052342652));
#64720=CARTESIAN_POINT('Ctrl Pts',(-19.8413853376269,-1.29179471042819,
0.521214121183144));
#64721=CARTESIAN_POINT('Ctrl Pts',(-19.7618417104099,-1.13688865241964,
-0.804911129262371));
#64722=CARTESIAN_POINT('Ctrl Pts',(-19.6822980831928,0.0624539660114313,
-1.3915808406774));
#64723=CARTESIAN_POINT('Ctrl Pts',(-19.6027544559757,1.20442139179994,-0.699833440888375));
#64724=CARTESIAN_POINT('Ctrl Pts',(-19.5232108287587,1.23991129837533,0.634836755530266));
#64725=CARTESIAN_POINT('Ctrl Pts',(-19.4436672015416,0.13631982794163,1.38629529268513));
#64726=CARTESIAN_POINT('Ctrl Pts',(-19.3641235743245,-1.09250590524041,
0.864192444439202));
#64727=CARTESIAN_POINT('Ctrl Pts',(-19.2845799471075,-1.31766860820214,
-0.451826485467164));
#64728=CARTESIAN_POINT('Ctrl Pts',(-19.2050363198904,-0.332315869745427,
-1.35276158162712));
#64729=CARTESIAN_POINT('Ctrl Pts',(-19.1254926926734,0.958328722255644,
-1.0109420330122));
#64730=CARTESIAN_POINT('Ctrl Pts',(-19.0459490654563,1.36857614229396,0.25960946969393));
#64731=CARTESIAN_POINT('Ctrl Pts',(-18.9664054382392,0.521540401231442,
1.29166301483565));
#64732=CARTESIAN_POINT('Ctrl Pts',(-18.8868618110222,-0.804623934899931,
1.13709193005541));
#64733=CARTESIAN_POINT('Ctrl Pts',(-18.8073181838051,-1.39159657164021,
-0.0621024621909377));
#64734=CARTESIAN_POINT('Ctrl Pts',(-18.7277745565881,-0.700137645459773,
-1.20424458122967));
#64735=CARTESIAN_POINT('Ctrl Pts',(-18.648230929371,0.63452354392386,-1.24007161334226));
#64736=CARTESIAN_POINT('Ctrl Pts',(-18.5686873021539,1.38626081519776,-0.136669990335221));
#64737=CARTESIAN_POINT('Ctrl Pts',(-18.4891436749369,0.864468374839663,
1.09228758251344));
#64738=CARTESIAN_POINT('Ctrl Pts',(-18.4096000477198,-0.451493638844702,
1.31778269380568));
#64739=CARTESIAN_POINT('Ctrl Pts',(-18.3300564205028,-1.35267759822798,
0.332657555548002));
#64740=CARTESIAN_POINT('Ctrl Pts',(-18.2505127932857,-1.01118406668283,
-0.958073336074932));
#64741=CARTESIAN_POINT('Ctrl Pts',(-18.1709691660687,0.259263770380752,
-1.36864167384269));
#64742=CARTESIAN_POINT('Ctrl Pts',(-18.0914255388516,1.29153123683166,-0.521866648004122));
#64743=CARTESIAN_POINT('Ctrl Pts',(-18.0118819116345,1.13729513514176,0.804336689200407));
#64744=CARTESIAN_POINT('Ctrl Pts',(-17.9323382844175,-0.0617509544081363,
1.39161221381557));
#64745=CARTESIAN_POINT('Ctrl Pts',(-17.8527946572004,-1.20406769382548,
0.700441805360565));
#64746=CARTESIAN_POINT('Ctrl Pts',(-17.7732510299834,-1.24023184918943,
-0.634210291833199));
#64747=CARTESIAN_POINT('Ctrl Pts',(-17.6937074027663,-0.137020144008901,
-1.38622624926336));
#64748=CARTESIAN_POINT('Ctrl Pts',(-17.6141637755493,1.09206919009568,-0.864744250084811));
#64749=CARTESIAN_POINT('Ctrl Pts',(-17.5346201483322,1.31789669533126,0.451160763415784));
#64750=CARTESIAN_POINT('Ctrl Pts',(-17.4550765211151,0.332999220126171,
1.35259352852449));
#64751=CARTESIAN_POINT('Ctrl Pts',(-17.3755328938981,-0.957817888766664,
1.0114260358373));
#64752=CARTESIAN_POINT('Ctrl Pts',(-17.295989266681,-1.36870711806855,-0.258918054525863));
#64753=CARTESIAN_POINT('Ctrl Pts',(-17.2164456394639,-0.522192861480347,
-1.29139937642464));
#64754=CARTESIAN_POINT('Ctrl Pts',(-17.1369020122469,0.804049392182112,
-1.13749826766574));
#64755=CARTESIAN_POINT('Ctrl Pts',(-17.0573583850298,1.39162776720246,0.0613994426854746));
#64756=CARTESIAN_POINT('Ctrl Pts',(-16.9778147578128,0.700745920571368,
1.20389072959865));
#64757=CARTESIAN_POINT('Ctrl Pts',(-16.8982711305957,-0.63389699927829,
1.24039200590658));
#64758=CARTESIAN_POINT('Ctrl Pts',(-16.8187275033786,-1.38619159488414,
0.137370288940351));
#64759=CARTESIAN_POINT('Ctrl Pts',(-16.7391838761616,-0.865020070157029,
-1.09185072800109));
#64760=CARTESIAN_POINT('Ctrl Pts',(-16.6596402489445,0.450827859201633,
-1.31801061277163));
#64761=CARTESIAN_POINT('Ctrl Pts',(-16.5800966217275,1.35250937252205,-0.333340863458119));
#64762=CARTESIAN_POINT('Ctrl Pts',(-16.5005529945104,1.01166794046017,0.957562380347131));
#64763=CARTESIAN_POINT('Ctrl Pts',(-16.4210093672934,-0.258572322151341,
1.36877247496735));
#64764=CARTESIAN_POINT('Ctrl Pts',(-16.3414657400763,-1.29126743362299,
0.522519041639328));
#64765=CARTESIAN_POINT('Ctrl Pts',(-16.2619221128592,-1.13770132761438,
-0.803762043863395));
#64766=CARTESIAN_POINT('Ctrl Pts',(-16.1823784856422,0.061047927045359,
-1.39164323179989));
#64767=CARTESIAN_POINT('Ctrl Pts',(-16.1028348584251,1.20371368856048,-0.701049991072757));
#64768=CARTESIAN_POINT('Ctrl Pts',(-16.0232912312081,1.24055208348352,0.633583666279101));
#64769=CARTESIAN_POINT('Ctrl Pts',(-15.943747603991,0.13772042510721,1.3861568520623));
#64770=CARTESIAN_POINT('Ctrl Pts',(-15.8642039767739,-1.09163219624359,
0.865295835038735));
#64771=CARTESIAN_POINT('Ctrl Pts',(-15.7846603495569,-1.31812444611951,
-0.450494926223506));
#64772=CARTESIAN_POINT('Ctrl Pts',(-15.7051167223398,-0.333682485522065,
-1.352425130226));
#64773=CARTESIAN_POINT('Ctrl Pts',(-15.6255730951227,0.957306810832643,
-1.011909780536));
#64774=CARTESIAN_POINT('Ctrl Pts',(-15.5460294679057,1.36883774453492,0.258226573279226));
#64775=CARTESIAN_POINT('Ctrl Pts',(-15.4664858406886,0.52284518846023,1.29113540843514));
#64776=CARTESIAN_POINT('Ctrl Pts',(-15.3869422134716,-0.803474644262568,
1.13790431497473));
#64777=CARTESIAN_POINT('Ctrl Pts',(-15.3073985862545,-1.39165860760688,
-0.0606964075102383));
#64778=CARTESIAN_POINT('Ctrl Pts',(-15.2278549590375,-0.70135401684535,
-1.20353657072225));
#64779=CARTESIAN_POINT('Ctrl Pts',(-15.1483113318204,0.633270292855629,
-1.24071208191002));
#64780=CARTESIAN_POINT('Ctrl Pts',(-15.0687677046033,1.38612202080006,-0.138070552487189));
#64781=CARTESIAN_POINT('Ctrl Pts',(-14.9892240773863,0.865571544712346,
1.09141359483712));
#64782=CARTESIAN_POINT('Ctrl Pts',(-14.9096804501692,-0.45016196450262,
1.31823819536764));
#64783=CARTESIAN_POINT('Ctrl Pts',(-14.8301368229522,-1.35234080164171,
0.334024086296205));
#64784=CARTESIAN_POINT('Ctrl Pts',(-14.7505931957351,-1.01215155604939,
-0.957051180239471));
#64785=CARTESIAN_POINT('Ctrl Pts',(-14.6710495685181,0.25788080793157,-1.36890292676711));
#64786=CARTESIAN_POINT('Ctrl Pts',(-14.591505941301,1.2910033008695,-0.523171301922277));
#64787=CARTESIAN_POINT('Ctrl Pts',(-14.5119623140839,1.13810722973384,0.803187193397973));
#64788=CARTESIAN_POINT('Ctrl Pts',(-14.4324186868668,-0.0603448841024907,
1.39167389462245));
#64789=CARTESIAN_POINT('Ctrl Pts',(-14.3528750596498,-1.20335937609527,
0.701657997869762));
#64790=CARTESIAN_POINT('Ctrl Pts',(-14.2733314324327,-1.2408720011759,-0.632956879027886));
#64791=CARTESIAN_POINT('Ctrl Pts',(-14.1937878052157,-0.138420671057853,
-1.38608710109966));
#64792=CARTESIAN_POINT('Ctrl Pts',(-14.1142441779986,1.09119492379563,-0.865847199160223));
#64793=CARTESIAN_POINT('Ctrl Pts',(-14.0347005507816,1.31835186050876,0.449828974060237));
#64794=CARTESIAN_POINT('Ctrl Pts',(-13.9551569235645,0.334365665758747,
1.3522563867746));
#64795=CARTESIAN_POINT('Ctrl Pts',(-13.8756132963474,-0.956795488584001,
1.01239326698485));
#64796=CARTESIAN_POINT('Ctrl Pts',(-13.7960696691304,-1.36896802165973,
-0.257535026130468));
#64797=CARTESIAN_POINT('Ctrl Pts',(-13.7165260419133,-0.523497382004637,
-1.29087111093451));
#64798=CARTESIAN_POINT('Ctrl Pts',(-13.6369824146963,0.802899691287971,
-1.13831007187878));
#64799=CARTESIAN_POINT('Ctrl Pts',(-13.5574387874792,1.39168909284562,0.05999335684464));
#64800=CARTESIAN_POINT('Ctrl Pts',(-13.4778951602621,0.701961934126549,
1.20318210469084));
#64801=CARTESIAN_POINT('Ctrl Pts',(-13.3983515330451,-0.632643424815839,
1.24103184127092));
#64802=CARTESIAN_POINT('Ctrl Pts',(-13.318807905828,-1.38605209296332,0.138770780796948));
#64803=CARTESIAN_POINT('Ctrl Pts',(-13.2392642786109,-0.866122798364796,
-1.09097618313311));
#64804=CARTESIAN_POINT('Ctrl Pts',(-13.1597206513939,0.449495954917602,
-1.3184654415356));
#64805=CARTESIAN_POINT('Ctrl Pts',(-13.0801770241768,1.35217188563002,-0.334707223887899));
#64806=CARTESIAN_POINT('Ctrl Pts',(-13.0006333969598,1.01263491332703,0.956539735882493));
#64807=CARTESIAN_POINT('Ctrl Pts',(-12.9210897697427,-0.25718922789799,
1.36903302920864));
#64808=CARTESIAN_POINT('Ctrl Pts',(-12.8415461425257,-1.29073883863859,
0.523823428686496));
#64809=CARTESIAN_POINT('Ctrl Pts',(-12.7620025153086,-1.13851284139658,
-0.802612137950876));
#64810=CARTESIAN_POINT('Ctrl Pts',(-12.6824588880915,0.0596418257590296,
-1.39170420227544));
#64811=CARTESIAN_POINT('Ctrl Pts',(-12.6029152608745,1.2030047565203,-0.702265825596333));
#64812=CARTESIAN_POINT('Ctrl Pts',(-12.5233716336574,1.24119160218488,0.632329930239507));
#64813=CARTESIAN_POINT('Ctrl Pts',(-12.4438280064404,0.139120881682115,
1.38601699639326));
#64814=CARTESIAN_POINT('Ctrl Pts',(-12.3642843792233,-1.09075737286348,
0.86639834230852));
#64815=CARTESIAN_POINT('Ctrl Pts',(-12.2847407520063,-1.31857893844094,
-0.449162907095992));
#64816=CARTESIAN_POINT('Ctrl Pts',(-12.2051971247892,-0.335048760661853,
-1.35208729821336));
#64817=CARTESIAN_POINT('Ctrl Pts',(-12.1256534975721,0.956283922151258,
-1.01287649506048));
#64818=CARTESIAN_POINT('Ctrl Pts',(-12.0461098703551,1.36909794940973,0.256843413256152));
#64819=CARTESIAN_POINT('Ctrl Pts',(-11.966566243138,0.524149441947044,1.29060648399021));
#64820=CARTESIAN_POINT('Ctrl Pts',(-11.887022615921,-0.802324533405046,
1.1387155382743));
#64821=CARTESIAN_POINT('Ctrl Pts',(-11.8074789887039,-1.39171922291092,
-0.0592902908681086));
#64822=CARTESIAN_POINT('Ctrl Pts',(-11.7279353614868,-0.702569672259767,
-1.20282733159494));
#64823=CARTESIAN_POINT('Ctrl Pts',(-11.6483917342698,0.632016395318918,
-1.2413512839076));
#64824=CARTESIAN_POINT('Ctrl Pts',(-11.5688481070527,1.38598181139171,-0.139470973691));
#64825=CARTESIAN_POINT('Ctrl Pts',(-11.4893044798357,0.866673830973786,
1.09053849300069));
#64826=CARTESIAN_POINT('Ctrl Pts',(-11.4097608526186,-0.448829830616605,
1.31869235121755));
#64827=CARTESIAN_POINT('Ctrl Pts',(-11.3302172254015,-1.35200262453006,
0.335390276058804));
#64828=CARTESIAN_POINT('Ctrl Pts',(-11.2506735981845,-1.01311801216977,
-0.956028047406628));
#64829=CARTESIAN_POINT('Ctrl Pts',(-11.1711299709674,0.256497582227027,
-1.36916278225881));
#64830=CARTESIAN_POINT('Ctrl Pts',(-11.0915863437504,1.2904740469978,-0.52447542176553));
#64831=CARTESIAN_POINT('Ctrl Pts',(-11.0120427165333,1.13891816249902,0.802036877668863));
#64832=CARTESIAN_POINT('Ctrl Pts',(-10.9324990893162,-0.0589387521943207,
1.39173415475109));
#64833=CARTESIAN_POINT('Ctrl Pts',(-10.8529554620992,-1.20264982992607,
0.702873474097439));
#64834=CARTESIAN_POINT('Ctrl Pts',(-10.7734118348821,-1.24151088642892,
-0.631702820074028));
#64835=CARTESIAN_POINT('Ctrl Pts',(-10.6938682076651,-0.139821056801252,
-1.38594653796095));
#64836=CARTESIAN_POINT('Ctrl Pts',(-10.614324580448,1.09031954355872,-0.866949264343001));
#64837=CARTESIAN_POINT('Ctrl Pts',(-10.534780953231,1.31880567985816,0.4484967255007));
#64838=CARTESIAN_POINT('Ctrl Pts',(-10.4552373260139,0.335731770057017,
1.35191786458549));
#64839=CARTESIAN_POINT('Ctrl Pts',(-10.3756936987968,-0.955772111664961,
1.0133594646395));
#64840=CARTESIAN_POINT('Ctrl Pts',(-10.2961500715798,-1.36922752775175,
-0.256151734832699));
#64841=CARTESIAN_POINT('Ctrl Pts',(-10.2166064443627,-0.524801368121128,
-1.29034152766978));
#64842=CARTESIAN_POINT('Ctrl Pts',(-10.1370628171456,0.801749170760637,
-1.13912071405783));
#64843=CARTESIAN_POINT('Ctrl Pts',(-10.0575191899286,1.39174899779504,0.0585872097601163));
#64844=CARTESIAN_POINT('Ctrl Pts',(-9.97797556271153,0.703177231089948,
1.20247225152501));
#64845=CARTESIAN_POINT('Ctrl Pts',(-9.89843193549446,-0.63138920452485,
1.24167040973862));
#64846=CARTESIAN_POINT('Ctrl Pts',(-9.8188883082774,-1.38591117610322,0.140171130990584));
#64847=CARTESIAN_POINT('Ctrl Pts',(-9.73934468106035,-0.867224642398599,
-1.09010052455156));
#64848=CARTESIAN_POINT('Ctrl Pts',(-9.65980105384327,0.448163591769547,
-1.31891892435554));
#64849=CARTESIAN_POINT('Ctrl Pts',(-9.58025742662623,1.35183301838504,-0.33607324263468));
#64850=CARTESIAN_POINT('Ctrl Pts',(-9.50071379940917,1.0136008524543,0.955516114942553));
#64851=CARTESIAN_POINT('Ctrl Pts',(-9.42117017219209,-0.255805871095256,
1.36929218588443));
#64852=CARTESIAN_POINT('Ctrl Pts',(-9.34162654497505,-1.29020892601463,
0.525127280993029));
#64853=CARTESIAN_POINT('Ctrl Pts',(-9.26208291775799,-1.13932319293779,
-0.801461412698725));
#64854=CARTESIAN_POINT('Ctrl Pts',(-9.18253929054092,0.0582356635878705,
-1.3917637520418));
#64855=CARTESIAN_POINT('Ctrl Pts',(-9.10299566332388,1.20229459640314,-0.703480943217913));
#64856=CARTESIAN_POINT('Ctrl Pts',(-9.02345203610679,1.24182985382652,0.631075548691406));
#64857=CARTESIAN_POINT('Ctrl Pts',(-8.94390840888976,0.140521196236644,
1.38587572582076));
#64858=CARTESIAN_POINT('Ctrl Pts',(-8.86436478167268,-1.08988143599316,
0.867499965123046));
#64859=CARTESIAN_POINT('Ctrl Pts',(-8.78482115445563,-1.31903208470249,
-0.447830429444425));
#64860=CARTESIAN_POINT('Ctrl Pts',(-8.70527752723856,-0.336414693769986,
-1.35174808593414));
#64861=CARTESIAN_POINT('Ctrl Pts',(-8.62573390002151,0.955260057255724,
-1.01384217559874));
#64862=CARTESIAN_POINT('Ctrl Pts',(-8.54619027280444,1.36935675665274,0.255459991036712));
#64863=CARTESIAN_POINT('Ctrl Pts',(-8.46664664558739,0.525453160360428,
1.29007624204083));
#64864=CARTESIAN_POINT('Ctrl Pts',(-8.38710301837033,-0.801173603501495,
1.13952559912596));
#64865=CARTESIAN_POINT('Ctrl Pts',(-8.30755939115328,-1.39177841749043,
-0.0578841137000273));
#64866=CARTESIAN_POINT('Ctrl Pts',(-8.2280157639362,-0.703784610462002,
-1.20211686457176));
#64867=CARTESIAN_POINT('Ctrl Pts',(-8.14847213671916,0.630761852593739,
-1.24198921868246));
#64868=CARTESIAN_POINT('Ctrl Pts',(-8.06892850950209,1.38584018711583,-0.140871252517076));
#64869=CARTESIAN_POINT('Ctrl Pts',(-7.98938488228504,0.867775232498749,
1.08966227789749));
#64870=CARTESIAN_POINT('Ctrl Pts',(-7.90984125506796,-0.447497238546542,
1.31914516089179));
#64871=CARTESIAN_POINT('Ctrl Pts',(-7.83029762785092,-1.35166306723823,
0.336756123441143));
#64872=CARTESIAN_POINT('Ctrl Pts',(-7.75075400063385,-1.01408343405741,
-0.955003938620828));
#64873=CARTESIAN_POINT('Ctrl Pts',(-7.6712103734168,0.255114094679148,-1.36942124005254));
#64874=CARTESIAN_POINT('Ctrl Pts',(-7.59166674619974,1.28994347575683,-0.525779006202587));
#64875=CARTESIAN_POINT('Ctrl Pts',(-7.51212311898267,1.13972793260945,0.800885743187348));
#64876=CARTESIAN_POINT('Ctrl Pts',(-7.43257949176562,-0.0575325601190364,
1.39179299413997));
#64877=CARTESIAN_POINT('Ctrl Pts',(-7.35303586454856,-1.2019390560422,0.704088232802815));
#64878=CARTESIAN_POINT('Ctrl Pts',(-7.27349223733148,-1.2421485042963,-0.630448116251818));
#64879=CARTESIAN_POINT('Ctrl Pts',(-7.19394861011444,-0.141221299809534,
-1.38580455999072));
#64880=CARTESIAN_POINT('Ctrl Pts',(-7.11440498289737,1.08944305027853,-0.868050444508131));
#64881=CARTESIAN_POINT('Ctrl Pts',(-7.03486135568032,1.3192581529162,0.447164019097165));
#64882=CARTESIAN_POINT('Ctrl Pts',(-6.95531772846325,0.337097531626415,
1.35157796230272));
#64883=CARTESIAN_POINT('Ctrl Pts',(-6.8757741012462,-0.954747759054236,
1.01432462781492));
#64884=CARTESIAN_POINT('Ctrl Pts',(-6.79623047402913,-1.3694856360797,-0.254768182044651));
#64885=CARTESIAN_POINT('Ctrl Pts',(-6.71668684681209,-0.526104818498686,
-1.28981062717108));
#64886=CARTESIAN_POINT('Ctrl Pts',(-6.63714321959501,0.800597831774603,
-1.13993019337537));
#64887=CARTESIAN_POINT('Ctrl Pts',(-6.55759959237797,1.39180748198953,0.0571810028673485));
#64888=CARTESIAN_POINT('Ctrl Pts',(-6.47805596516089,0.704391810220957,
1.2017611708258));
#64889=CARTESIAN_POINT('Ctrl Pts',(-6.39851233794385,-0.630134339685656,
1.24230771065784));
#64890=CARTESIAN_POINT('Ctrl Pts',(-6.31896871072677,-1.3857688444477,0.141571338091734));
#64891=CARTESIAN_POINT('Ctrl Pts',(-6.23942508350973,-0.868325601133633,
-1.08922375315032));
#64892=CARTESIAN_POINT('Ctrl Pts',(-6.15988145629266,0.446830771117568,
-1.31937106076852));
#64893=CARTESIAN_POINT('Ctrl Pts',(-6.08033782907561,1.35149277113303,-0.337438918303999));
#64894=CARTESIAN_POINT('Ctrl Pts',(-6.00079420185854,1.01456575685592,0.954491518572258));
#64895=CARTESIAN_POINT('Ctrl Pts',(-5.92125057464148,-0.254422253155312,
1.36954994473014));
#64896=CARTESIAN_POINT('Ctrl Pts',(-5.84170694742441,-1.28967769629207,
0.526430597227924));
#64897=CARTESIAN_POINT('Ctrl Pts',(-5.76216332020736,-1.14013238141078,
-0.80030986928163));
#64898=CARTESIAN_POINT('Ctrl Pts',(-5.68261969299031,0.0568294419673366,
-1.39182188103819));
#64899=CARTESIAN_POINT('Ctrl Pts',(-5.60307606577323,1.20158320893396,-0.704695342697066));
#64900=CARTESIAN_POINT('Ctrl Pts',(-5.52353243855619,1.24246683775691,0.629820522915297));
#64901=CARTESIAN_POINT('Ctrl Pts',(-5.44398881133912,0.141921367341324,
1.38573304048903));
#64902=CARTESIAN_POINT('Ctrl Pts',(-5.36444518412207,-1.08900438652681,
0.868600702357744));
#64903=CARTESIAN_POINT('Ctrl Pts',(-5.284901556905,-1.31948388444155,-0.446497494629042));
#64904=CARTESIAN_POINT('Ctrl Pts',(-5.20535792968794,-0.337780283452094,
-1.35140749373458));
#64905=CARTESIAN_POINT('Ctrl Pts',(-5.12581430247089,0.954235217191234,
-1.01480682116499));
#64906=CARTESIAN_POINT('Ctrl Pts',(-5.04627067525382,1.36961416599977,0.254076308033152));
#64907=CARTESIAN_POINT('Ctrl Pts',(-4.96672704803676,0.526756342369506,
1.2895446831283));
#64908=CARTESIAN_POINT('Ctrl Pts',(-4.88718342081971,-0.800021855726812,
1.14033449670278));
#64909=CARTESIAN_POINT('Ctrl Pts',(-4.80763979360265,-1.39183619128499,
-0.0564778774414496));
#64910=CARTESIAN_POINT('Ctrl Pts',(-4.72809616638559,-0.704998830211815,
-1.20140517037799));
#64911=CARTESIAN_POINT('Ctrl Pts',(-4.64855253916853,0.629506665960787,
-1.24262588558339));
#64912=CARTESIAN_POINT('Ctrl Pts',(-4.56900891195147,1.38569714811699,-0.142271387535955));
#64913=CARTESIAN_POINT('Ctrl Pts',(-4.48946528473441,0.868875748162881,
1.08878495042198));
#64914=CARTESIAN_POINT('Ctrl Pts',(-4.40992165751735,-0.446164189652799,
1.31959662392811));
#64915=CARTESIAN_POINT('Ctrl Pts',(-4.33037803030028,-1.35132213011286,
0.338121627048909));
#64916=CARTESIAN_POINT('Ctrl Pts',(-4.25083440308323,-1.01504782072675,
-0.953978854927527));
#64917=CARTESIAN_POINT('Ctrl Pts',(-4.17129077586617,0.253730346700255,
-1.36967829988445));
#64918=CARTESIAN_POINT('Ctrl Pts',(-4.09174714864911,1.28941158768824,-0.527082053902699));
#64919=CARTESIAN_POINT('Ctrl Pts',(-4.01220352143205,1.14053653923849,0.799733791128557));
#64920=CARTESIAN_POINT('Ctrl Pts',(-3.93265989421499,-0.0561263093121601,
1.39185041272904));
#64921=CARTESIAN_POINT('Ctrl Pts',(-3.85311626699793,-1.20122705516927,
0.705302272745785));
#64922=CARTESIAN_POINT('Ctrl Pts',(-3.77357263978087,-1.24278485412711,
-0.629192768842119));
#64923=CARTESIAN_POINT('Ctrl Pts',(-3.69402901256381,-0.142621398653279,
-1.3856611673339));
#64924=CARTESIAN_POINT('Ctrl Pts',(-3.61448538534675,1.08856544484988,-0.869150738531468));
#64925=CARTESIAN_POINT('Ctrl Pts',(-3.53494175812969,1.31970927922097,0.445830856210143));
#64926=CARTESIAN_POINT('Ctrl Pts',(-3.45539813091263,0.338462949072693,
1.35123668027329));
#64927=CARTESIAN_POINT('Ctrl Pts',(-3.37585450369557,-0.95372243179753,
1.01528875552582));
#64928=CARTESIAN_POINT('Ctrl Pts',(-3.29631087647852,-1.36974234638011,
-0.253384369178725));
#64929=CARTESIAN_POINT('Ctrl Pts',(-3.21676724926146,-0.527407731806677,
-1.28927840998041));
#64930=CARTESIAN_POINT('Ctrl Pts',(-3.13722362204439,0.799445675505238,
-1.14073850900496));
#64931=CARTESIAN_POINT('Ctrl Pts',(-3.05767999482733,1.39186454536937,0.0557747376017607));
#64932=CARTESIAN_POINT('Ctrl Pts',(-2.97813636761027,0.705605670279753,
1.20104886331929));
#64933=CARTESIAN_POINT('Ctrl Pts',(-2.89859274039321,-0.62887883157946,
1.24294374337767));
#64934=CARTESIAN_POINT('Ctrl Pts',(-2.81904911317616,-1.38562509814175,
0.142971400671562));
#64935=CARTESIAN_POINT('Ctrl Pts',(-2.7395054859591,-0.869425673446542,
-1.08834586982554));
#64936=CARTESIAN_POINT('Ctrl Pts',(-2.65996185874204,0.445497494323327,
-1.31982185031089));
#64937=CARTESIAN_POINT('Ctrl Pts',(-2.58041823152498,1.35115114421937,-0.338804249505638));
#64938=CARTESIAN_POINT('Ctrl Pts',(-2.50087460430792,1.01552962555056,0.953465947825067));
#64939=CARTESIAN_POINT('Ctrl Pts',(-2.42133097709085,-0.253038375497675,
1.36980630546842));
#64940=CARTESIAN_POINT('Ctrl Pts',(-2.3417873498738,-1.28914514999981,0.527733376087698));
#64941=CARTESIAN_POINT('Ctrl Pts',(-2.26224372265673,-1.14094040601493,
-0.799157508926434));
#64942=CARTESIAN_POINT('Ctrl Pts',(-2.18270009543968,0.0554231623812737,
-1.39187858910792));
#64943=CARTESIAN_POINT('Ctrl Pts',(-2.10315646822262,1.2008705947473,-0.7059090229788));
#64944=CARTESIAN_POINT('Ctrl Pts',(-2.02361284100557,1.24310255349976,0.628564854542996));
#64945=CARTESIAN_POINT('Ctrl Pts',(-1.9440692137885,0.143321393236571,1.38558893987825));
#64946=CARTESIAN_POINT('Ctrl Pts',(-1.86452558657144,-1.08812622473303,
0.869700554151995));
#64947=CARTESIAN_POINT('Ctrl Pts',(-1.78498195935438,-1.31993433838648,
-0.445164106407946));
#64948=CARTESIAN_POINT('Ctrl Pts',(-1.70543833213732,-0.339145526056245,
-1.35106551741206));
#64949=CARTESIAN_POINT('Ctrl Pts',(-1.62589470492026,0.9532093987185,-1.01577043941121));
#64950=CARTESIAN_POINT('Ctrl Pts',(-1.5463510777032,1.36987018532208,0.25269238205091));
#64951=CARTESIAN_POINT('Ctrl Pts',(-1.46680745048614,0.528058971205146,
1.28901177668085));
#64952=CARTESIAN_POINT('Ctrl Pts',(-1.38726382326908,-0.798869261953324,
1.14114228923538));
#64953=CARTESIAN_POINT('Ctrl Pts',(-1.30772019605202,-1.39189259985476,
-0.0550716956193558));
#64954=CARTESIAN_POINT('Ctrl Pts',(-1.22817656883496,-0.70621222470226,
-1.20069203698611));
#64955=CARTESIAN_POINT('Ctrl Pts',(-1.14863294161791,0.628250636330202,
-1.24326168777629));
#64956=CARTESIAN_POINT('Ctrl Pts',(-1.06908931440084,1.38555307485394,-0.143670610859339));
#64957=CARTESIAN_POINT('Ctrl Pts',(-0.989545687183782,0.869974654993682,
1.08790505669946));
#64958=CARTESIAN_POINT('Ctrl Pts',(-0.910002059966723,-0.444829315197323,
1.32004950107908));
#64959=CARTESIAN_POINT('Ctrl Pts',(-0.830458432749666,-1.35098241400592,
0.33948154459194));
#64960=CARTESIAN_POINT('Ctrl Pts',(-0.750914805532605,-1.01600623532771,
-0.952942849934193));
#64961=CARTESIAN_POINT('Ctrl Pts',(-0.671371178315547,0.252336971202078,
-1.36995284217421));
#64962=CARTESIAN_POINT('Ctrl Pts',(-0.591827551098487,1.28889616535859,
-0.528348726914579));
#64963=CARTESIAN_POINT('Ctrl Pts',(-0.512283923881428,1.14131022863273,
0.798513000617958));
#64964=CARTESIAN_POINT('Ctrl Pts',(-0.432740296664372,-0.0546559205033708,
1.39203554179653));
#64965=CARTESIAN_POINT('Ctrl Pts',(-0.353196669447305,-1.20063559357129,
0.70627030388918));
#64966=CARTESIAN_POINT('Ctrl Pts',(-0.273653042230246,-1.24318765340952,
-0.627469583607843));
#64967=CARTESIAN_POINT('Ctrl Pts',(-0.194109415013188,-0.144472093338112,
-1.38641688872905));
#64968=CARTESIAN_POINT('Ctrl Pts',(-0.114565787796129,1.08862479899838,
-0.868424655134898));
#64969=CARTESIAN_POINT('Ctrl Pts',(-0.0615367029847556,1.24139853983146,
0.00391577327447434));
#64970=CARTESIAN_POINT('Ctrl Pts',(-0.0350221605790679,1.11617937559294,
0.375817327967939));
#64971=CARTESIAN_POINT('Ctrl Pts',(-0.200000000000004,1.38699088616444,
0.466999498604424));
#64972=CARTESIAN_POINT('Ctrl Pts',(-0.22651454240569,1.54259118067784,0.00486583246659934));
#64973=CARTESIAN_POINT('Ctrl Pts',(-0.253029084811376,1.44767104919453,
-0.537129589727037));
#64974=CARTESIAN_POINT('Ctrl Pts',(-0.279543627217062,1.14483175725401,
-0.915405533876346));
#64975=CARTESIAN_POINT('Ctrl Pts',(-0.306058169622748,0.841992465313498,
-1.29368147802566));
#64976=CARTESIAN_POINT('Ctrl Pts',(-0.332572712028434,0.331234012915777,
-1.50823794413064));
#64977=CARTESIAN_POINT('Ctrl Pts',(-0.35908725443412,-0.151693535955519,
-1.45833519918207));
#64978=CARTESIAN_POINT('Ctrl Pts',(-0.385601796839806,-0.634621084826815,
-1.4084324542335));
#64979=CARTESIAN_POINT('Ctrl Pts',(-0.412116339245492,-1.08971773017168,
-1.09407049823137));
#64980=CARTESIAN_POINT('Ctrl Pts',(-0.438630881651178,-1.30845335354846,
-0.660666733086481));
#64981=CARTESIAN_POINT('Ctrl Pts',(-0.451035572486509,-1.41078767790324,
-0.457901034503743));
#64982=CARTESIAN_POINT('Ctrl Pts',(-0.463440263321839,-1.46138759520564,
-0.229079612523116));
#64983=CARTESIAN_POINT('Ctrl Pts',(-0.47584495415717,-1.4610556053668,-0.000134560743048767));
#64984=CARTESIAN_POINT('Origin',(-0.2,0.,0.));
#64985=CARTESIAN_POINT('',(0.,-2.03719995038162E-16,1.6635));
#64986=CARTESIAN_POINT('Origin',(-0.2,-2.03719995038162E-16,1.6635));
#64987=CARTESIAN_POINT('Origin',(0.,0.,0.));
#64988=CARTESIAN_POINT('Origin',(-0.2,0.,0.));
#64989=CARTESIAN_POINT('Origin',(-17.3,0.,0.));
#64990=CARTESIAN_POINT('Origin',(0.,2.75,0.));
#64991=CARTESIAN_POINT('',(0.,-2.75,-3.36777869765522E-16));
#64992=CARTESIAN_POINT('Origin',(0.,0.,0.));
#64993=CARTESIAN_POINT('Origin',(0.3,2.77916773064255,-0.363113928340879));
#64994=CARTESIAN_POINT('',(2.6,2.72200415854531,-0.391399234621183));
#64995=CARTESIAN_POINT('',(0.3,2.72200415854531,-0.391399234621183));
#64996=CARTESIAN_POINT('',(1.35,2.72200415854531,-0.391399234621183));
#64997=CARTESIAN_POINT('',(2.6,2.59004439042211,-0.456694707264027));
#64998=CARTESIAN_POINT('',(2.6,2.77916773064255,-0.363113928340879));
#64999=CARTESIAN_POINT('',(0.3,2.59004439042211,-0.456694707264027));
#65000=CARTESIAN_POINT('',(0.3,2.59004439042211,-0.456694707264027));
#65001=CARTESIAN_POINT('',(0.3,2.77916773064255,-0.363113928340879));
#65002=CARTESIAN_POINT('Origin',(0.3,2.67375304942814,-0.471454802365716));
#65003=CARTESIAN_POINT('',(0.3,2.69171364385628,-0.563185279883955));
#65004=CARTESIAN_POINT('Origin',(0.3,0.,0.));
#65005=CARTESIAN_POINT('',(0.3,2.59004439042211,-0.456694707264027));
#65006=CARTESIAN_POINT('Origin',(0.3,2.59004439042211,-0.456694707264027));
#65007=CARTESIAN_POINT('',(2.6,2.69171364385628,-0.563185279883955));
#65008=CARTESIAN_POINT('',(1.35,2.69171364385628,-0.563185279883955));
#65009=CARTESIAN_POINT('',(2.6,2.59004439042211,-0.456694707264027));
#65010=CARTESIAN_POINT('Origin',(2.6,2.67375304942814,-0.471454802365716));
#65011=CARTESIAN_POINT('Origin',(2.6,0.,0.));
#65012=CARTESIAN_POINT('Origin',(0.3,2.67389185611625,-0.840194823713636));
#65013=CARTESIAN_POINT('',(2.6,2.61268503523469,-0.858124062511185));
#65014=CARTESIAN_POINT('',(0.3,2.61268503523469,-0.858124062511185));
#65015=CARTESIAN_POINT('',(1.35,2.61268503523469,-0.858124062511185));
#65016=CARTESIAN_POINT('',(2.6,2.47139159266694,-0.899512976946511));
#65017=CARTESIAN_POINT('',(2.6,2.67389185611625,-0.840194823713636));
#65018=CARTESIAN_POINT('',(0.3,2.47139159266694,-0.899512976946511));
#65019=CARTESIAN_POINT('',(0.3,2.47139159266694,-0.899512976946511));
#65020=CARTESIAN_POINT('',(0.3,2.67389185611625,-0.840194823713636));
#65021=CARTESIAN_POINT('Origin',(0.3,2.55126546543374,-0.928584689129192));
#65022=CARTESIAN_POINT('',(0.3,2.55302436781771,-1.02204039906893));
#65023=CARTESIAN_POINT('Origin',(0.3,0.,0.));
#65024=CARTESIAN_POINT('',(0.3,2.47139159266694,-0.899512976946511));
#65025=CARTESIAN_POINT('Origin',(0.3,2.47139159266694,-0.899512976946511));
#65026=CARTESIAN_POINT('',(2.6,2.55302436781771,-1.02204039906893));
#65027=CARTESIAN_POINT('',(1.35,2.55302436781771,-1.02204039906893));
#65028=CARTESIAN_POINT('',(2.6,2.47139159266694,-0.899512976946511));
#65029=CARTESIAN_POINT('Origin',(2.6,2.55126546543374,-0.928584689129192));
#65030=CARTESIAN_POINT('Origin',(2.6,0.,0.));
#65031=CARTESIAN_POINT('Origin',(0.3,2.48737113059643,-1.29174682452695));
#65032=CARTESIAN_POINT('',(2.6,2.42398079921089,-1.29877522499351));
#65033=CARTESIAN_POINT('',(0.3,2.42398079921089,-1.29877522499351));
#65034=CARTESIAN_POINT('',(1.35,2.42398079921089,-1.29877522499351));
#65035=CARTESIAN_POINT('',(2.6,2.27764681195307,-1.315));
#65036=CARTESIAN_POINT('',(2.6,2.48737113059643,-1.29174682452695));
#65037=CARTESIAN_POINT('',(0.3,2.27764681195307,-1.315));
#65038=CARTESIAN_POINT('',(0.3,2.27764681195307,-1.315));
#65039=CARTESIAN_POINT('',(0.3,2.48737113059643,-1.29174682452695));
#65040=CARTESIAN_POINT('Origin',(0.3,2.35125897127475,-1.3575));
#65041=CARTESIAN_POINT('',(0.3,2.33676273825567,-1.44984133790558));
#65042=CARTESIAN_POINT('Origin',(0.3,0.,0.));
#65043=CARTESIAN_POINT('',(0.3,2.27764681195307,-1.315));
#65044=CARTESIAN_POINT('Origin',(0.3,2.27764681195307,-1.315));
#65045=CARTESIAN_POINT('',(2.6,2.33676273825567,-1.44984133790558));
#65046=CARTESIAN_POINT('',(1.35,2.33676273825567,-1.44984133790558));
#65047=CARTESIAN_POINT('',(2.6,2.27764681195307,-1.315));
#65048=CARTESIAN_POINT('Origin',(2.6,2.35125897127475,-1.3575));
#65049=CARTESIAN_POINT('Origin',(2.6,0.,0.));
#65050=CARTESIAN_POINT('Origin',(0.3,2.22527289194396,-1.70404975173244));
#65051=CARTESIAN_POINT('',(2.6,2.16162513319653,-1.69996375947638));
#65052=CARTESIAN_POINT('',(0.3,2.16162513319653,-1.69996375947638));
#65053=CARTESIAN_POINT('',(1.35,2.16162513319653,-1.69996375947638));
#65054=CARTESIAN_POINT('',(2.6,2.01469688540291,-1.6905314134756));
#65055=CARTESIAN_POINT('',(2.6,2.22527289194396,-1.70404975173244));
#65056=CARTESIAN_POINT('',(0.3,2.01469688540291,-1.6905314134756));
#65057=CARTESIAN_POINT('',(0.3,2.01469688540291,-1.6905314134756));
#65058=CARTESIAN_POINT('',(0.3,2.22527289194396,-1.70404975173244));
#65059=CARTESIAN_POINT('Origin',(0.3,2.07981066306802,-1.74516836029895));
#65060=CARTESIAN_POINT('',(0.3,2.04949975535074,-1.83358958134509));
#65061=CARTESIAN_POINT('Origin',(0.3,0.,0.));
#65062=CARTESIAN_POINT('',(0.3,2.01469688540291,-1.6905314134756));
#65063=CARTESIAN_POINT('Origin',(0.3,2.01469688540291,-1.6905314134756));
#65064=CARTESIAN_POINT('',(2.6,2.04949975535074,-1.83358958134509));
#65065=CARTESIAN_POINT('',(1.35,2.04949975535074,-1.83358958134509));
#65066=CARTESIAN_POINT('',(2.6,2.01469688540291,-1.6905314134756));
#65067=CARTESIAN_POINT('Origin',(2.6,2.07981066306802,-1.74516836029895));
#65068=CARTESIAN_POINT('Origin',(2.6,0.,0.));
#65069=CARTESIAN_POINT('Origin',(0.3,1.89556086251218,-2.06457598952232));
#65070=CARTESIAN_POINT('',(2.6,1.83358958134509,-2.04949975535074));
#65071=CARTESIAN_POINT('',(0.3,1.83358958134509,-2.04949975535074));
#65072=CARTESIAN_POINT('',(1.35,1.83358958134509,-2.04949975535074));
#65073=CARTESIAN_POINT('',(2.6,1.6905314134756,-2.01469688540291));
#65074=CARTESIAN_POINT('',(2.6,1.89556086251218,-2.06457598952232));
#65075=CARTESIAN_POINT('',(0.3,1.6905314134756,-2.01469688540291));
#65076=CARTESIAN_POINT('',(0.3,1.6905314134756,-2.01469688540291));
#65077=CARTESIAN_POINT('',(0.3,1.89556086251218,-2.06457598952232));
#65078=CARTESIAN_POINT('Origin',(0.3,1.74516836029895,-2.07981066306803));
#65079=CARTESIAN_POINT('',(0.3,1.69996375947638,-2.16162513319653));
#65080=CARTESIAN_POINT('Origin',(0.3,0.,0.));
#65081=CARTESIAN_POINT('',(0.3,1.6905314134756,-2.01469688540291));
#65082=CARTESIAN_POINT('Origin',(0.3,1.6905314134756,-2.01469688540291));
#65083=CARTESIAN_POINT('',(2.6,1.69996375947638,-2.16162513319653));
#65084=CARTESIAN_POINT('',(1.35,1.69996375947638,-2.16162513319653));
#65085=CARTESIAN_POINT('',(2.6,1.6905314134756,-2.01469688540291));
#65086=CARTESIAN_POINT('Origin',(2.6,1.74516836029895,-2.07981066306803));
#65087=CARTESIAN_POINT('Origin',(2.6,0.,0.));
#65088=CARTESIAN_POINT('Origin',(0.3,1.50825317547306,-2.36237113059643));
#65089=CARTESIAN_POINT('',(2.6,1.44984133790558,-2.33676273825567));
#65090=CARTESIAN_POINT('',(0.3,1.44984133790558,-2.33676273825567));
#65091=CARTESIAN_POINT('',(1.35,1.44984133790558,-2.33676273825567));
#65092=CARTESIAN_POINT('',(2.6,1.315,-2.27764681195307));
#65093=CARTESIAN_POINT('',(2.6,1.50825317547306,-2.36237113059643));
#65094=CARTESIAN_POINT('',(0.3,1.315,-2.27764681195307));
#65095=CARTESIAN_POINT('',(0.3,1.315,-2.27764681195307));
#65096=CARTESIAN_POINT('',(0.3,1.50825317547306,-2.36237113059643));
#65097=CARTESIAN_POINT('Origin',(0.3,1.3575,-2.35125897127475));
#65098=CARTESIAN_POINT('',(0.3,1.29877522499351,-2.42398079921089));
#65099=CARTESIAN_POINT('Origin',(0.3,0.,0.));
#65100=CARTESIAN_POINT('',(0.3,1.315,-2.27764681195307));
#65101=CARTESIAN_POINT('Origin',(0.3,1.315,-2.27764681195307));
#65102=CARTESIAN_POINT('',(2.6,1.29877522499351,-2.42398079921089));
#65103=CARTESIAN_POINT('',(1.35,1.29877522499351,-2.42398079921089));
#65104=CARTESIAN_POINT('',(2.6,1.315,-2.27764681195307));
#65105=CARTESIAN_POINT('Origin',(2.6,1.3575,-2.35125897127475));
#65106=CARTESIAN_POINT('Origin',(2.6,0.,0.));
#65107=CARTESIAN_POINT('Origin',(0.3,1.07511797891011,-2.58838682028484));
#65108=CARTESIAN_POINT('',(2.6,1.02204039906892,-2.55302436781771));
#65109=CARTESIAN_POINT('',(0.3,1.02204039906892,-2.55302436781771));
#65110=CARTESIAN_POINT('',(1.35,1.02204039906892,-2.55302436781771));
#65111=CARTESIAN_POINT('',(2.6,0.899512976946507,-2.47139159266694));
#65112=CARTESIAN_POINT('',(2.6,1.07511797891011,-2.58838682028484));
#65113=CARTESIAN_POINT('',(0.3,0.899512976946507,-2.47139159266694));
#65114=CARTESIAN_POINT('',(0.3,0.899512976946507,-2.47139159266694));
#65115=CARTESIAN_POINT('',(0.3,1.07511797891011,-2.58838682028484));
#65116=CARTESIAN_POINT('Origin',(0.3,0.928584689129189,-2.55126546543374));
#65117=CARTESIAN_POINT('',(0.3,0.858124062511182,-2.61268503523469));
#65118=CARTESIAN_POINT('Origin',(0.3,0.,0.));
#65119=CARTESIAN_POINT('',(0.3,0.899512976946507,-2.47139159266694));
#65120=CARTESIAN_POINT('Origin',(0.3,0.899512976946507,-2.47139159266694));
#65121=CARTESIAN_POINT('',(2.6,0.858124062511182,-2.61268503523469));
#65122=CARTESIAN_POINT('',(1.35,0.858124062511182,-2.61268503523469));
#65123=CARTESIAN_POINT('',(2.6,0.899512976946507,-2.47139159266694));
#65124=CARTESIAN_POINT('Origin',(2.6,0.928584689129189,-2.55126546543374));
#65125=CARTESIAN_POINT('Origin',(2.6,0.,0.));
#65126=CARTESIAN_POINT('Origin',(0.3,0.60931586659393,-2.73575568622582));
#65127=CARTESIAN_POINT('',(2.6,0.563185279883954,-2.69171364385628));
#65128=CARTESIAN_POINT('',(0.3,0.563185279883954,-2.69171364385628));
#65129=CARTESIAN_POINT('',(1.35,0.563185279883954,-2.69171364385628));
#65130=CARTESIAN_POINT('',(2.6,0.456694707264026,-2.59004439042211));
#65131=CARTESIAN_POINT('',(2.6,0.60931586659393,-2.73575568622582));
#65132=CARTESIAN_POINT('',(0.3,0.456694707264026,-2.59004439042211));
#65133=CARTESIAN_POINT('',(0.3,0.456694707264026,-2.59004439042211));
#65134=CARTESIAN_POINT('',(0.3,0.60931586659393,-2.73575568622582));
#65135=CARTESIAN_POINT('Origin',(0.3,0.471454802365715,-2.67375304942814));
#65136=CARTESIAN_POINT('',(0.3,0.391399234621181,-2.72200415854531));
#65137=CARTESIAN_POINT('Origin',(0.3,0.,0.));
#65138=CARTESIAN_POINT('',(0.3,0.456694707264026,-2.59004439042211));
#65139=CARTESIAN_POINT('Origin',(0.3,0.456694707264026,-2.59004439042211));
#65140=CARTESIAN_POINT('',(2.6,0.391399234621181,-2.72200415854531));
#65141=CARTESIAN_POINT('',(1.35,0.391399234621181,-2.72200415854531));
#65142=CARTESIAN_POINT('',(2.6,0.456694707264026,-2.59004439042211));
#65143=CARTESIAN_POINT('Origin',(2.6,0.471454802365715,-2.67375304942814));
#65144=CARTESIAN_POINT('Origin',(2.6,0.,0.));
#65145=CARTESIAN_POINT('Origin',(0.3,0.124999999999999,-2.8));
#65146=CARTESIAN_POINT('',(2.6,0.0872180609552139,-2.74861656289909));
#65147=CARTESIAN_POINT('',(0.3,0.0872180609552139,-2.74861656289909));
#65148=CARTESIAN_POINT('',(1.35,0.0872180609552139,-2.74861656289909));
#65149=CARTESIAN_POINT('',(2.6,-4.83123162263631E-16,-2.63));
#65150=CARTESIAN_POINT('',(2.6,0.124999999999999,-2.8));
#65151=CARTESIAN_POINT('',(0.3,-4.83123162263631E-16,-2.63));
#65152=CARTESIAN_POINT('',(0.3,-4.83123162263631E-16,-2.63));
#65153=CARTESIAN_POINT('',(0.3,0.124999999999999,-2.8));
#65154=CARTESIAN_POINT('Origin',(0.3,-4.9873740895276E-16,-2.715));
#65155=CARTESIAN_POINT('',(0.3,-0.0872180609552148,-2.74861656289909));
#65156=CARTESIAN_POINT('Origin',(0.3,0.,0.));
#65157=CARTESIAN_POINT('',(0.3,-4.83123162263631E-16,-2.63));
#65158=CARTESIAN_POINT('Origin',(0.3,-4.83123162263631E-16,-2.63));
#65159=CARTESIAN_POINT('',(2.6,-0.0872180609552148,-2.74861656289909));
#65160=CARTESIAN_POINT('',(1.35,-0.0872180609552148,-2.74861656289909));
#65161=CARTESIAN_POINT('',(2.6,-4.83123162263631E-16,-2.63));
#65162=CARTESIAN_POINT('Origin',(2.6,-4.9873740895276E-16,-2.715));
#65163=CARTESIAN_POINT('Origin',(2.6,0.,0.));
#65164=CARTESIAN_POINT('Origin',(0.3,-0.363113928340879,-2.77916773064255));
#65165=CARTESIAN_POINT('',(2.6,-0.391399234621183,-2.72200415854531));
#65166=CARTESIAN_POINT('',(0.3,-0.391399234621183,-2.72200415854531));
#65167=CARTESIAN_POINT('',(1.35,-0.391399234621183,-2.72200415854531));
#65168=CARTESIAN_POINT('',(2.6,-0.456694707264027,-2.59004439042211));
#65169=CARTESIAN_POINT('',(2.6,-0.363113928340879,-2.77916773064255));
#65170=CARTESIAN_POINT('',(0.3,-0.456694707264027,-2.59004439042211));
#65171=CARTESIAN_POINT('',(0.3,-0.456694707264027,-2.59004439042211));
#65172=CARTESIAN_POINT('',(0.3,-0.363113928340879,-2.77916773064255));
#65173=CARTESIAN_POINT('Origin',(0.3,-0.471454802365716,-2.67375304942814));
#65174=CARTESIAN_POINT('',(0.3,-0.563185279883955,-2.69171364385628));
#65175=CARTESIAN_POINT('Origin',(0.3,0.,0.));
#65176=CARTESIAN_POINT('',(0.3,-0.456694707264027,-2.59004439042211));
#65177=CARTESIAN_POINT('Origin',(0.3,-0.456694707264027,-2.59004439042211));
#65178=CARTESIAN_POINT('',(2.6,-0.563185279883955,-2.69171364385628));
#65179=CARTESIAN_POINT('',(1.35,-0.563185279883955,-2.69171364385628));
#65180=CARTESIAN_POINT('',(2.6,-0.456694707264027,-2.59004439042211));
#65181=CARTESIAN_POINT('Origin',(2.6,-0.471454802365716,-2.67375304942814));
#65182=CARTESIAN_POINT('Origin',(2.6,0.,0.));
#65183=CARTESIAN_POINT('Origin',(0.3,-0.840194823713636,-2.67389185611625));
#65184=CARTESIAN_POINT('',(2.6,-0.858124062511185,-2.61268503523469));
#65185=CARTESIAN_POINT('',(0.3,-0.858124062511185,-2.61268503523469));
#65186=CARTESIAN_POINT('',(1.35,-0.858124062511185,-2.61268503523469));
#65187=CARTESIAN_POINT('',(2.6,-0.89951297694651,-2.47139159266694));
#65188=CARTESIAN_POINT('',(2.6,-0.840194823713636,-2.67389185611625));
#65189=CARTESIAN_POINT('',(0.3,-0.89951297694651,-2.47139159266694));
#65190=CARTESIAN_POINT('',(0.3,-0.89951297694651,-2.47139159266694));
#65191=CARTESIAN_POINT('',(0.3,-0.840194823713636,-2.67389185611625));
#65192=CARTESIAN_POINT('Origin',(0.3,-0.928584689129192,-2.55126546543374));
#65193=CARTESIAN_POINT('',(0.3,-1.02204039906893,-2.55302436781771));
#65194=CARTESIAN_POINT('Origin',(0.3,0.,0.));
#65195=CARTESIAN_POINT('',(0.3,-0.89951297694651,-2.47139159266694));
#65196=CARTESIAN_POINT('Origin',(0.3,-0.89951297694651,-2.47139159266694));
#65197=CARTESIAN_POINT('',(2.6,-1.02204039906893,-2.55302436781771));
#65198=CARTESIAN_POINT('',(1.35,-1.02204039906893,-2.55302436781771));
#65199=CARTESIAN_POINT('',(2.6,-0.89951297694651,-2.47139159266694));
#65200=CARTESIAN_POINT('Origin',(2.6,-0.928584689129192,-2.55126546543374));
#65201=CARTESIAN_POINT('Origin',(2.6,0.,0.));
#65202=CARTESIAN_POINT('Origin',(0.3,-1.29174682452695,-2.48737113059643));
#65203=CARTESIAN_POINT('',(2.6,-1.29877522499351,-2.42398079921089));
#65204=CARTESIAN_POINT('',(0.3,-1.29877522499351,-2.42398079921089));
#65205=CARTESIAN_POINT('',(1.35,-1.29877522499351,-2.42398079921089));
#65206=CARTESIAN_POINT('',(2.6,-1.315,-2.27764681195307));
#65207=CARTESIAN_POINT('',(2.6,-1.29174682452695,-2.48737113059643));
#65208=CARTESIAN_POINT('',(0.3,-1.315,-2.27764681195307));
#65209=CARTESIAN_POINT('',(0.3,-1.315,-2.27764681195307));
#65210=CARTESIAN_POINT('',(0.3,-1.29174682452695,-2.48737113059643));
#65211=CARTESIAN_POINT('Origin',(0.3,-1.3575,-2.35125897127475));
#65212=CARTESIAN_POINT('',(0.3,-1.44984133790558,-2.33676273825567));
#65213=CARTESIAN_POINT('Origin',(0.3,0.,0.));
#65214=CARTESIAN_POINT('',(0.3,-1.315,-2.27764681195307));
#65215=CARTESIAN_POINT('Origin',(0.3,-1.315,-2.27764681195307));
#65216=CARTESIAN_POINT('',(2.6,-1.44984133790558,-2.33676273825567));
#65217=CARTESIAN_POINT('',(1.35,-1.44984133790558,-2.33676273825567));
#65218=CARTESIAN_POINT('',(2.6,-1.315,-2.27764681195307));
#65219=CARTESIAN_POINT('Origin',(2.6,-1.3575,-2.35125897127475));
#65220=CARTESIAN_POINT('Origin',(2.6,0.,0.));
#65221=CARTESIAN_POINT('Origin',(0.3,-1.70404975173244,-2.22527289194396));
#65222=CARTESIAN_POINT('',(2.6,-1.69996375947638,-2.16162513319653));
#65223=CARTESIAN_POINT('',(0.3,-1.69996375947638,-2.16162513319653));
#65224=CARTESIAN_POINT('',(1.35,-1.69996375947638,-2.16162513319653));
#65225=CARTESIAN_POINT('',(2.6,-1.6905314134756,-2.01469688540291));
#65226=CARTESIAN_POINT('',(2.6,-1.70404975173244,-2.22527289194396));
#65227=CARTESIAN_POINT('',(0.3,-1.6905314134756,-2.01469688540291));
#65228=CARTESIAN_POINT('',(0.3,-1.6905314134756,-2.01469688540291));
#65229=CARTESIAN_POINT('',(0.3,-1.70404975173244,-2.22527289194396));
#65230=CARTESIAN_POINT('Origin',(0.3,-1.74516836029895,-2.07981066306802));
#65231=CARTESIAN_POINT('',(0.3,-1.83358958134509,-2.04949975535074));
#65232=CARTESIAN_POINT('Origin',(0.3,0.,0.));
#65233=CARTESIAN_POINT('',(0.3,-1.6905314134756,-2.01469688540291));
#65234=CARTESIAN_POINT('Origin',(0.3,-1.6905314134756,-2.01469688540291));
#65235=CARTESIAN_POINT('',(2.6,-1.83358958134509,-2.04949975535074));
#65236=CARTESIAN_POINT('',(1.35,-1.83358958134509,-2.04949975535074));
#65237=CARTESIAN_POINT('',(2.6,-1.6905314134756,-2.01469688540291));
#65238=CARTESIAN_POINT('Origin',(2.6,-1.74516836029895,-2.07981066306802));
#65239=CARTESIAN_POINT('Origin',(2.6,0.,0.));
#65240=CARTESIAN_POINT('Origin',(0.3,-2.06457598952232,-1.89556086251218));
#65241=CARTESIAN_POINT('',(2.6,-2.04949975535074,-1.83358958134509));
#65242=CARTESIAN_POINT('',(0.3,-2.04949975535074,-1.83358958134509));
#65243=CARTESIAN_POINT('',(1.35,-2.04949975535074,-1.83358958134509));
#65244=CARTESIAN_POINT('',(2.6,-2.01469688540291,-1.6905314134756));
#65245=CARTESIAN_POINT('',(2.6,-2.06457598952232,-1.89556086251218));
#65246=CARTESIAN_POINT('',(0.3,-2.01469688540291,-1.6905314134756));
#65247=CARTESIAN_POINT('',(0.3,-2.01469688540291,-1.6905314134756));
#65248=CARTESIAN_POINT('',(0.3,-2.06457598952232,-1.89556086251218));
#65249=CARTESIAN_POINT('Origin',(0.3,-2.07981066306803,-1.74516836029895));
#65250=CARTESIAN_POINT('',(0.3,-2.16162513319653,-1.69996375947638));
#65251=CARTESIAN_POINT('Origin',(0.3,0.,0.));
#65252=CARTESIAN_POINT('',(0.3,-2.01469688540291,-1.6905314134756));
#65253=CARTESIAN_POINT('Origin',(0.3,-2.01469688540291,-1.6905314134756));
#65254=CARTESIAN_POINT('',(2.6,-2.16162513319653,-1.69996375947638));
#65255=CARTESIAN_POINT('',(1.35,-2.16162513319653,-1.69996375947638));
#65256=CARTESIAN_POINT('',(2.6,-2.01469688540291,-1.6905314134756));
#65257=CARTESIAN_POINT('Origin',(2.6,-2.07981066306803,-1.74516836029895));
#65258=CARTESIAN_POINT('Origin',(2.6,0.,0.));
#65259=CARTESIAN_POINT('Origin',(0.3,-2.36237113059643,-1.50825317547305));
#65260=CARTESIAN_POINT('',(2.6,-2.33676273825568,-1.44984133790558));
#65261=CARTESIAN_POINT('',(0.3,-2.33676273825568,-1.44984133790558));
#65262=CARTESIAN_POINT('',(1.35,-2.33676273825567,-1.44984133790558));
#65263=CARTESIAN_POINT('',(2.6,-2.27764681195307,-1.315));
#65264=CARTESIAN_POINT('',(2.6,-2.36237113059643,-1.50825317547305));
#65265=CARTESIAN_POINT('',(0.3,-2.27764681195307,-1.315));
#65266=CARTESIAN_POINT('',(0.3,-2.27764681195307,-1.315));
#65267=CARTESIAN_POINT('',(0.3,-2.36237113059643,-1.50825317547305));
#65268=CARTESIAN_POINT('Origin',(0.3,-2.35125897127475,-1.3575));
#65269=CARTESIAN_POINT('',(0.3,-2.42398079921089,-1.29877522499351));
#65270=CARTESIAN_POINT('Origin',(0.3,0.,0.));
#65271=CARTESIAN_POINT('',(0.3,-2.27764681195307,-1.315));
#65272=CARTESIAN_POINT('Origin',(0.3,-2.27764681195307,-1.315));
#65273=CARTESIAN_POINT('',(2.6,-2.42398079921089,-1.29877522499351));
#65274=CARTESIAN_POINT('',(1.35,-2.42398079921089,-1.29877522499351));
#65275=CARTESIAN_POINT('',(2.6,-2.27764681195307,-1.315));
#65276=CARTESIAN_POINT('Origin',(2.6,-2.35125897127475,-1.3575));
#65277=CARTESIAN_POINT('Origin',(2.6,0.,0.));
#65278=CARTESIAN_POINT('Origin',(0.3,-2.58838682028483,-1.07511797891011));
#65279=CARTESIAN_POINT('',(2.6,-2.55302436781771,-1.02204039906892));
#65280=CARTESIAN_POINT('',(0.3,-2.55302436781771,-1.02204039906892));
#65281=CARTESIAN_POINT('',(1.35,-2.55302436781771,-1.02204039906892));
#65282=CARTESIAN_POINT('',(2.6,-2.47139159266694,-0.899512976946509));
#65283=CARTESIAN_POINT('',(2.6,-2.58838682028483,-1.07511797891011));
#65284=CARTESIAN_POINT('',(0.3,-2.47139159266694,-0.899512976946509));
#65285=CARTESIAN_POINT('',(0.3,-2.47139159266694,-0.899512976946509));
#65286=CARTESIAN_POINT('',(0.3,-2.58838682028483,-1.07511797891011));
#65287=CARTESIAN_POINT('Origin',(0.3,-2.55126546543374,-0.92858468912919));
#65288=CARTESIAN_POINT('',(0.3,-2.61268503523469,-0.858124062511184));
#65289=CARTESIAN_POINT('Origin',(0.3,0.,0.));
#65290=CARTESIAN_POINT('',(0.3,-2.47139159266694,-0.899512976946509));
#65291=CARTESIAN_POINT('Origin',(0.3,-2.47139159266694,-0.899512976946509));
#65292=CARTESIAN_POINT('',(2.6,-2.61268503523469,-0.858124062511184));
#65293=CARTESIAN_POINT('',(1.35,-2.61268503523469,-0.858124062511184));
#65294=CARTESIAN_POINT('',(2.6,-2.47139159266694,-0.899512976946509));
#65295=CARTESIAN_POINT('Origin',(2.6,-2.55126546543374,-0.92858468912919));
#65296=CARTESIAN_POINT('Origin',(2.6,0.,0.));
#65297=CARTESIAN_POINT('Origin',(0.3,-2.73575568622582,-0.60931586659393));
#65298=CARTESIAN_POINT('',(2.6,-2.69171364385628,-0.563185279883954));
#65299=CARTESIAN_POINT('',(0.3,-2.69171364385628,-0.563185279883954));
#65300=CARTESIAN_POINT('',(1.35,-2.69171364385628,-0.563185279883954));
#65301=CARTESIAN_POINT('',(2.6,-2.59004439042211,-0.456694707264026));
#65302=CARTESIAN_POINT('',(2.6,-2.73575568622582,-0.60931586659393));
#65303=CARTESIAN_POINT('',(0.3,-2.59004439042211,-0.456694707264026));
#65304=CARTESIAN_POINT('',(0.3,-2.59004439042211,-0.456694707264026));
#65305=CARTESIAN_POINT('',(0.3,-2.73575568622582,-0.60931586659393));
#65306=CARTESIAN_POINT('Origin',(0.3,-2.67375304942814,-0.471454802365715));
#65307=CARTESIAN_POINT('',(0.3,-2.72200415854531,-0.391399234621182));
#65308=CARTESIAN_POINT('Origin',(0.3,0.,0.));
#65309=CARTESIAN_POINT('',(0.3,-2.59004439042211,-0.456694707264026));
#65310=CARTESIAN_POINT('Origin',(0.3,-2.59004439042211,-0.456694707264026));
#65311=CARTESIAN_POINT('',(2.6,-2.72200415854531,-0.391399234621182));
#65312=CARTESIAN_POINT('',(1.35,-2.72200415854531,-0.391399234621182));
#65313=CARTESIAN_POINT('',(2.6,-2.59004439042211,-0.456694707264026));
#65314=CARTESIAN_POINT('Origin',(2.6,-2.67375304942814,-0.471454802365715));
#65315=CARTESIAN_POINT('Origin',(2.6,0.,0.));
#65316=CARTESIAN_POINT('Origin',(0.3,-2.8,-0.125));
#65317=CARTESIAN_POINT('',(2.6,-2.74861656289909,-0.0872180609552139));
#65318=CARTESIAN_POINT('',(0.3,-2.74861656289909,-0.0872180609552139));
#65319=CARTESIAN_POINT('',(1.35,-2.74861656289909,-0.0872180609552139));
#65320=CARTESIAN_POINT('',(2.6,-2.63,3.22082108175754E-16));
#65321=CARTESIAN_POINT('',(2.6,-2.8,-0.125));
#65322=CARTESIAN_POINT('',(0.3,-2.63,3.22082108175754E-16));
#65323=CARTESIAN_POINT('',(0.3,-2.63,3.22082108175754E-16));
#65324=CARTESIAN_POINT('',(0.3,-2.8,-0.125));
#65325=CARTESIAN_POINT('Origin',(0.3,-2.715,3.32491605968506E-16));
#65326=CARTESIAN_POINT('',(0.3,-2.75,-3.36777869765522E-16));
#65327=CARTESIAN_POINT('Origin',(0.3,0.,0.));
#65328=CARTESIAN_POINT('',(0.3,-2.74861656289909,0.0872180609552148));
#65329=CARTESIAN_POINT('',(0.3,-2.63,3.22082108175754E-16));
#65330=CARTESIAN_POINT('Origin',(0.3,0.,0.));
#65331=CARTESIAN_POINT('Origin',(0.3,-2.63,3.22082108175754E-16));
#65332=CARTESIAN_POINT('',(2.6,-2.74861656289909,0.0872180609552148));
#65333=CARTESIAN_POINT('',(1.35,-2.74861656289909,0.0872180609552148));
#65334=CARTESIAN_POINT('',(2.6,-2.63,3.22082108175754E-16));
#65335=CARTESIAN_POINT('Origin',(2.6,-2.715,3.32491605968506E-16));
#65336=CARTESIAN_POINT('',(2.6,-2.75,-3.36777869765522E-16));
#65337=CARTESIAN_POINT('Origin',(2.6,0.,0.));
#65338=CARTESIAN_POINT('Origin',(2.6,0.,0.));
#65339=CARTESIAN_POINT('Origin',(0.3,-2.77916773064255,0.36311392834088));
#65340=CARTESIAN_POINT('',(2.6,-2.72200415854531,0.391399234621184));
#65341=CARTESIAN_POINT('',(0.3,-2.72200415854531,0.391399234621184));
#65342=CARTESIAN_POINT('',(1.35,-2.72200415854531,0.391399234621184));
#65343=CARTESIAN_POINT('',(2.6,-2.59004439042211,0.456694707264028));
#65344=CARTESIAN_POINT('',(2.6,-2.77916773064255,0.36311392834088));
#65345=CARTESIAN_POINT('',(0.3,-2.59004439042211,0.456694707264028));
#65346=CARTESIAN_POINT('',(0.3,-2.59004439042211,0.456694707264028));
#65347=CARTESIAN_POINT('',(0.3,-2.77916773064255,0.36311392834088));
#65348=CARTESIAN_POINT('Origin',(0.3,-2.67375304942814,0.471454802365717));
#65349=CARTESIAN_POINT('',(0.3,-2.69171364385628,0.563185279883956));
#65350=CARTESIAN_POINT('Origin',(0.3,0.,0.));
#65351=CARTESIAN_POINT('',(0.3,-2.59004439042211,0.456694707264028));
#65352=CARTESIAN_POINT('Origin',(0.3,-2.59004439042211,0.456694707264028));
#65353=CARTESIAN_POINT('',(2.6,-2.69171364385628,0.563185279883956));
#65354=CARTESIAN_POINT('',(1.35,-2.69171364385628,0.563185279883956));
#65355=CARTESIAN_POINT('',(2.6,-2.59004439042211,0.456694707264028));
#65356=CARTESIAN_POINT('Origin',(2.6,-2.67375304942814,0.471454802365717));
#65357=CARTESIAN_POINT('Origin',(2.6,0.,0.));
#65358=CARTESIAN_POINT('Origin',(0.3,-2.67389185611625,0.840194823713635));
#65359=CARTESIAN_POINT('',(2.6,-2.61268503523469,0.858124062511184));
#65360=CARTESIAN_POINT('',(0.3,-2.61268503523469,0.858124062511184));
#65361=CARTESIAN_POINT('',(1.35,-2.61268503523469,0.858124062511184));
#65362=CARTESIAN_POINT('',(2.6,-2.47139159266694,0.899512976946509));
#65363=CARTESIAN_POINT('',(2.6,-2.67389185611625,0.840194823713635));
#65364=CARTESIAN_POINT('',(0.3,-2.47139159266694,0.899512976946509));
#65365=CARTESIAN_POINT('',(0.3,-2.47139159266694,0.899512976946509));
#65366=CARTESIAN_POINT('',(0.3,-2.67389185611625,0.840194823713635));
#65367=CARTESIAN_POINT('Origin',(0.3,-2.55126546543374,0.928584689129191));
#65368=CARTESIAN_POINT('',(0.3,-2.55302436781771,1.02204039906892));
#65369=CARTESIAN_POINT('Origin',(0.3,0.,0.));
#65370=CARTESIAN_POINT('',(0.3,-2.47139159266694,0.899512976946509));
#65371=CARTESIAN_POINT('Origin',(0.3,-2.47139159266694,0.899512976946509));
#65372=CARTESIAN_POINT('',(2.6,-2.55302436781771,1.02204039906892));
#65373=CARTESIAN_POINT('',(1.35,-2.55302436781771,1.02204039906893));
#65374=CARTESIAN_POINT('',(2.6,-2.47139159266694,0.899512976946509));
#65375=CARTESIAN_POINT('Origin',(2.6,-2.55126546543374,0.928584689129191));
#65376=CARTESIAN_POINT('Origin',(2.6,0.,0.));
#65377=CARTESIAN_POINT('Origin',(0.3,-2.48737113059643,1.29174682452694));
#65378=CARTESIAN_POINT('',(2.6,-2.42398079921089,1.29877522499351));
#65379=CARTESIAN_POINT('',(0.3,-2.42398079921089,1.29877522499351));
#65380=CARTESIAN_POINT('',(1.35,-2.42398079921089,1.29877522499351));
#65381=CARTESIAN_POINT('',(2.6,-2.27764681195307,1.315));
#65382=CARTESIAN_POINT('',(2.6,-2.48737113059643,1.29174682452694));
#65383=CARTESIAN_POINT('',(0.3,-2.27764681195307,1.315));
#65384=CARTESIAN_POINT('',(0.3,-2.27764681195307,1.315));
#65385=CARTESIAN_POINT('',(0.3,-2.48737113059643,1.29174682452694));
#65386=CARTESIAN_POINT('Origin',(0.3,-2.35125897127475,1.3575));
#65387=CARTESIAN_POINT('',(0.3,-2.33676273825567,1.44984133790558));
#65388=CARTESIAN_POINT('Origin',(0.3,0.,0.));
#65389=CARTESIAN_POINT('',(0.3,-2.27764681195307,1.315));
#65390=CARTESIAN_POINT('Origin',(0.3,-2.27764681195307,1.315));
#65391=CARTESIAN_POINT('',(2.6,-2.33676273825567,1.44984133790558));
#65392=CARTESIAN_POINT('',(1.35,-2.33676273825567,1.44984133790558));
#65393=CARTESIAN_POINT('',(2.6,-2.27764681195307,1.315));
#65394=CARTESIAN_POINT('Origin',(2.6,-2.35125897127475,1.3575));
#65395=CARTESIAN_POINT('Origin',(2.6,0.,0.));
#65396=CARTESIAN_POINT('Origin',(0.3,-2.22527289194396,1.70404975173244));
#65397=CARTESIAN_POINT('',(2.6,-2.16162513319653,1.69996375947638));
#65398=CARTESIAN_POINT('',(0.3,-2.16162513319653,1.69996375947638));
#65399=CARTESIAN_POINT('',(1.35,-2.16162513319653,1.69996375947638));
#65400=CARTESIAN_POINT('',(2.6,-2.01469688540291,1.6905314134756));
#65401=CARTESIAN_POINT('',(2.6,-2.22527289194396,1.70404975173244));
#65402=CARTESIAN_POINT('',(0.3,-2.01469688540291,1.6905314134756));
#65403=CARTESIAN_POINT('',(0.3,-2.01469688540291,1.6905314134756));
#65404=CARTESIAN_POINT('',(0.3,-2.22527289194396,1.70404975173244));
#65405=CARTESIAN_POINT('Origin',(0.3,-2.07981066306802,1.74516836029895));
#65406=CARTESIAN_POINT('',(0.3,-2.04949975535074,1.83358958134509));
#65407=CARTESIAN_POINT('Origin',(0.3,0.,0.));
#65408=CARTESIAN_POINT('',(0.3,-2.01469688540291,1.6905314134756));
#65409=CARTESIAN_POINT('Origin',(0.3,-2.01469688540291,1.6905314134756));
#65410=CARTESIAN_POINT('',(2.6,-2.04949975535074,1.83358958134509));
#65411=CARTESIAN_POINT('',(1.35,-2.04949975535074,1.83358958134509));
#65412=CARTESIAN_POINT('',(2.6,-2.01469688540291,1.6905314134756));
#65413=CARTESIAN_POINT('Origin',(2.6,-2.07981066306802,1.74516836029895));
#65414=CARTESIAN_POINT('Origin',(2.6,0.,0.));
#65415=CARTESIAN_POINT('Origin',(0.3,-1.89556086251218,2.06457598952232));
#65416=CARTESIAN_POINT('',(2.6,-1.83358958134509,2.04949975535074));
#65417=CARTESIAN_POINT('',(0.3,-1.83358958134509,2.04949975535074));
#65418=CARTESIAN_POINT('',(1.35,-1.83358958134509,2.04949975535074));
#65419=CARTESIAN_POINT('',(2.6,-1.6905314134756,2.01469688540291));
#65420=CARTESIAN_POINT('',(2.6,-1.89556086251218,2.06457598952232));
#65421=CARTESIAN_POINT('',(0.3,-1.6905314134756,2.01469688540291));
#65422=CARTESIAN_POINT('',(0.3,-1.6905314134756,2.01469688540291));
#65423=CARTESIAN_POINT('',(0.3,-1.89556086251218,2.06457598952232));
#65424=CARTESIAN_POINT('Origin',(0.3,-1.74516836029895,2.07981066306803));
#65425=CARTESIAN_POINT('',(0.3,-1.69996375947638,2.16162513319653));
#65426=CARTESIAN_POINT('Origin',(0.3,0.,0.));
#65427=CARTESIAN_POINT('',(0.3,-1.6905314134756,2.01469688540291));
#65428=CARTESIAN_POINT('Origin',(0.3,-1.6905314134756,2.01469688540291));
#65429=CARTESIAN_POINT('',(2.6,-1.69996375947638,2.16162513319653));
#65430=CARTESIAN_POINT('',(1.35,-1.69996375947638,2.16162513319653));
#65431=CARTESIAN_POINT('',(2.6,-1.6905314134756,2.01469688540291));
#65432=CARTESIAN_POINT('Origin',(2.6,-1.74516836029895,2.07981066306803));
#65433=CARTESIAN_POINT('Origin',(2.6,0.,0.));
#65434=CARTESIAN_POINT('Origin',(0.3,-1.50825317547305,2.36237113059643));
#65435=CARTESIAN_POINT('',(2.6,-1.44984133790558,2.33676273825568));
#65436=CARTESIAN_POINT('',(0.3,-1.44984133790558,2.33676273825568));
#65437=CARTESIAN_POINT('',(1.35,-1.44984133790558,2.33676273825568));
#65438=CARTESIAN_POINT('',(2.6,-1.315,2.27764681195307));
#65439=CARTESIAN_POINT('',(2.6,-1.50825317547305,2.36237113059643));
#65440=CARTESIAN_POINT('',(0.3,-1.315,2.27764681195307));
#65441=CARTESIAN_POINT('',(0.3,-1.315,2.27764681195307));
#65442=CARTESIAN_POINT('',(0.3,-1.50825317547305,2.36237113059643));
#65443=CARTESIAN_POINT('Origin',(0.3,-1.3575,2.35125897127475));
#65444=CARTESIAN_POINT('',(0.3,-1.29877522499351,2.42398079921089));
#65445=CARTESIAN_POINT('Origin',(0.3,0.,0.));
#65446=CARTESIAN_POINT('',(0.3,-1.315,2.27764681195307));
#65447=CARTESIAN_POINT('Origin',(0.3,-1.315,2.27764681195307));
#65448=CARTESIAN_POINT('',(2.6,-1.29877522499351,2.42398079921089));
#65449=CARTESIAN_POINT('',(1.35,-1.29877522499351,2.42398079921089));
#65450=CARTESIAN_POINT('',(2.6,-1.315,2.27764681195307));
#65451=CARTESIAN_POINT('Origin',(2.6,-1.3575,2.35125897127475));
#65452=CARTESIAN_POINT('Origin',(2.6,0.,0.));
#65453=CARTESIAN_POINT('Origin',(0.3,-1.07511797891011,2.58838682028483));
#65454=CARTESIAN_POINT('',(2.6,-1.02204039906892,2.55302436781771));
#65455=CARTESIAN_POINT('',(0.3,-1.02204039906892,2.55302436781771));
#65456=CARTESIAN_POINT('',(1.35,-1.02204039906892,2.55302436781771));
#65457=CARTESIAN_POINT('',(2.6,-0.899512976946509,2.47139159266694));
#65458=CARTESIAN_POINT('',(2.6,-1.07511797891011,2.58838682028483));
#65459=CARTESIAN_POINT('',(0.3,-0.899512976946509,2.47139159266694));
#65460=CARTESIAN_POINT('',(0.3,-0.899512976946509,2.47139159266694));
#65461=CARTESIAN_POINT('',(0.3,-1.07511797891011,2.58838682028483));
#65462=CARTESIAN_POINT('Origin',(0.3,-0.92858468912919,2.55126546543374));
#65463=CARTESIAN_POINT('',(0.3,-0.858124062511184,2.61268503523469));
#65464=CARTESIAN_POINT('Origin',(0.3,0.,0.));
#65465=CARTESIAN_POINT('',(0.3,-0.899512976946509,2.47139159266694));
#65466=CARTESIAN_POINT('Origin',(0.3,-0.899512976946509,2.47139159266694));
#65467=CARTESIAN_POINT('',(2.6,-0.858124062511184,2.61268503523469));
#65468=CARTESIAN_POINT('',(1.35,-0.858124062511184,2.61268503523469));
#65469=CARTESIAN_POINT('',(2.6,-0.899512976946509,2.47139159266694));
#65470=CARTESIAN_POINT('Origin',(2.6,-0.92858468912919,2.55126546543374));
#65471=CARTESIAN_POINT('Origin',(2.6,0.,0.));
#65472=CARTESIAN_POINT('Origin',(0.3,-0.609315866593931,2.73575568622582));
#65473=CARTESIAN_POINT('',(2.6,-0.563185279883955,2.69171364385628));
#65474=CARTESIAN_POINT('',(0.3,-0.563185279883955,2.69171364385628));
#65475=CARTESIAN_POINT('',(1.35,-0.563185279883955,2.69171364385628));
#65476=CARTESIAN_POINT('',(2.6,-0.456694707264027,2.59004439042211));
#65477=CARTESIAN_POINT('',(2.6,-0.609315866593931,2.73575568622582));
#65478=CARTESIAN_POINT('',(0.3,-0.456694707264027,2.59004439042211));
#65479=CARTESIAN_POINT('',(0.3,-0.456694707264027,2.59004439042211));
#65480=CARTESIAN_POINT('',(0.3,-0.609315866593931,2.73575568622582));
#65481=CARTESIAN_POINT('Origin',(0.3,-0.471454802365716,2.67375304942814));
#65482=CARTESIAN_POINT('',(0.3,-0.391399234621183,2.72200415854531));
#65483=CARTESIAN_POINT('Origin',(0.3,0.,0.));
#65484=CARTESIAN_POINT('',(0.3,-0.456694707264027,2.59004439042211));
#65485=CARTESIAN_POINT('Origin',(0.3,-0.456694707264027,2.59004439042211));
#65486=CARTESIAN_POINT('',(2.6,-0.391399234621183,2.72200415854531));
#65487=CARTESIAN_POINT('',(1.35,-0.391399234621183,2.72200415854531));
#65488=CARTESIAN_POINT('',(2.6,-0.456694707264027,2.59004439042211));
#65489=CARTESIAN_POINT('Origin',(2.6,-0.471454802365716,2.67375304942814));
#65490=CARTESIAN_POINT('Origin',(2.6,0.,0.));
#65491=CARTESIAN_POINT('Origin',(0.3,-0.125,2.8));
#65492=CARTESIAN_POINT('',(2.6,-0.0872180609552139,2.74861656289909));
#65493=CARTESIAN_POINT('',(0.3,-0.0872180609552139,2.74861656289909));
#65494=CARTESIAN_POINT('',(1.35,-0.0872180609552139,2.74861656289909));
#65495=CARTESIAN_POINT('',(2.6,1.61041054087877E-16,2.63));
#65496=CARTESIAN_POINT('',(2.6,-0.125,2.8));
#65497=CARTESIAN_POINT('',(0.3,1.61041054087877E-16,2.63));
#65498=CARTESIAN_POINT('',(0.3,1.61041054087877E-16,2.63));
#65499=CARTESIAN_POINT('',(0.3,-0.125,2.8));
#65500=CARTESIAN_POINT('Origin',(0.3,1.66245802984253E-16,2.715));
#65501=CARTESIAN_POINT('',(0.3,0.0872180609552142,2.74861656289909));
#65502=CARTESIAN_POINT('Origin',(0.3,0.,0.));
#65503=CARTESIAN_POINT('',(0.3,1.61041054087877E-16,2.63));
#65504=CARTESIAN_POINT('Origin',(0.3,1.61041054087877E-16,2.63));
#65505=CARTESIAN_POINT('',(2.6,0.0872180609552142,2.74861656289909));
#65506=CARTESIAN_POINT('',(1.35,0.0872180609552142,2.74861656289909));
#65507=CARTESIAN_POINT('',(2.6,1.61041054087877E-16,2.63));
#65508=CARTESIAN_POINT('Origin',(2.6,1.66245802984253E-16,2.715));
#65509=CARTESIAN_POINT('Origin',(2.6,0.,0.));
#65510=CARTESIAN_POINT('Origin',(0.3,0.363113928340879,2.77916773064255));
#65511=CARTESIAN_POINT('',(2.6,0.391399234621183,2.72200415854531));
#65512=CARTESIAN_POINT('',(0.3,0.391399234621183,2.72200415854531));
#65513=CARTESIAN_POINT('',(1.35,0.391399234621183,2.72200415854531));
#65514=CARTESIAN_POINT('',(2.6,0.456694707264027,2.59004439042211));
#65515=CARTESIAN_POINT('',(2.6,0.363113928340879,2.77916773064255));
#65516=CARTESIAN_POINT('',(0.3,0.456694707264027,2.59004439042211));
#65517=CARTESIAN_POINT('',(0.3,0.456694707264027,2.59004439042211));
#65518=CARTESIAN_POINT('',(0.3,0.363113928340879,2.77916773064255));
#65519=CARTESIAN_POINT('Origin',(0.3,0.471454802365716,2.67375304942814));
#65520=CARTESIAN_POINT('',(0.3,0.563185279883955,2.69171364385628));
#65521=CARTESIAN_POINT('Origin',(0.3,0.,0.));
#65522=CARTESIAN_POINT('',(0.3,0.456694707264027,2.59004439042211));
#65523=CARTESIAN_POINT('Origin',(0.3,0.456694707264027,2.59004439042211));
#65524=CARTESIAN_POINT('',(2.6,0.563185279883955,2.69171364385628));
#65525=CARTESIAN_POINT('',(1.35,0.563185279883955,2.69171364385628));
#65526=CARTESIAN_POINT('',(2.6,0.456694707264027,2.59004439042211));
#65527=CARTESIAN_POINT('Origin',(2.6,0.471454802365716,2.67375304942814));
#65528=CARTESIAN_POINT('Origin',(2.6,0.,0.));
#65529=CARTESIAN_POINT('Origin',(0.3,0.840194823713634,2.67389185611625));
#65530=CARTESIAN_POINT('',(2.6,0.858124062511184,2.61268503523469));
#65531=CARTESIAN_POINT('',(0.3,0.858124062511184,2.61268503523469));
#65532=CARTESIAN_POINT('',(1.35,0.858124062511184,2.61268503523469));
#65533=CARTESIAN_POINT('',(2.6,0.899512976946509,2.47139159266694));
#65534=CARTESIAN_POINT('',(2.6,0.840194823713634,2.67389185611625));
#65535=CARTESIAN_POINT('',(0.3,0.899512976946509,2.47139159266694));
#65536=CARTESIAN_POINT('',(0.3,0.899512976946509,2.47139159266694));
#65537=CARTESIAN_POINT('',(0.3,0.840194823713634,2.67389185611625));
#65538=CARTESIAN_POINT('Origin',(0.3,0.928584689129191,2.55126546543374));
#65539=CARTESIAN_POINT('',(0.3,1.02204039906892,2.55302436781771));
#65540=CARTESIAN_POINT('Origin',(0.3,0.,0.));
#65541=CARTESIAN_POINT('',(0.3,0.899512976946509,2.47139159266694));
#65542=CARTESIAN_POINT('Origin',(0.3,0.899512976946509,2.47139159266694));
#65543=CARTESIAN_POINT('',(2.6,1.02204039906892,2.55302436781771));
#65544=CARTESIAN_POINT('',(1.35,1.02204039906892,2.55302436781771));
#65545=CARTESIAN_POINT('',(2.6,0.899512976946509,2.47139159266694));
#65546=CARTESIAN_POINT('Origin',(2.6,0.928584689129191,2.55126546543374));
#65547=CARTESIAN_POINT('Origin',(2.6,0.,0.));
#65548=CARTESIAN_POINT('Origin',(0.3,1.29174682452695,2.48737113059643));
#65549=CARTESIAN_POINT('',(2.6,1.29877522499351,2.42398079921089));
#65550=CARTESIAN_POINT('',(0.3,1.29877522499351,2.42398079921089));
#65551=CARTESIAN_POINT('',(1.35,1.29877522499351,2.42398079921089));
#65552=CARTESIAN_POINT('',(2.6,1.315,2.27764681195307));
#65553=CARTESIAN_POINT('',(2.6,1.29174682452695,2.48737113059643));
#65554=CARTESIAN_POINT('',(0.3,1.315,2.27764681195307));
#65555=CARTESIAN_POINT('',(0.3,1.315,2.27764681195307));
#65556=CARTESIAN_POINT('',(0.3,1.29174682452695,2.48737113059643));
#65557=CARTESIAN_POINT('Origin',(0.3,1.3575,2.35125897127475));
#65558=CARTESIAN_POINT('',(0.3,1.44984133790558,2.33676273825567));
#65559=CARTESIAN_POINT('Origin',(0.3,0.,0.));
#65560=CARTESIAN_POINT('',(0.3,1.315,2.27764681195307));
#65561=CARTESIAN_POINT('Origin',(0.3,1.315,2.27764681195307));
#65562=CARTESIAN_POINT('',(2.6,1.44984133790558,2.33676273825567));
#65563=CARTESIAN_POINT('',(1.35,1.44984133790558,2.33676273825567));
#65564=CARTESIAN_POINT('',(2.6,1.315,2.27764681195307));
#65565=CARTESIAN_POINT('Origin',(2.6,1.3575,2.35125897127475));
#65566=CARTESIAN_POINT('Origin',(2.6,0.,0.));
#65567=CARTESIAN_POINT('Origin',(0.3,1.70404975173244,2.22527289194396));
#65568=CARTESIAN_POINT('',(2.6,1.69996375947638,2.16162513319653));
#65569=CARTESIAN_POINT('',(0.3,1.69996375947638,2.16162513319653));
#65570=CARTESIAN_POINT('',(1.35,1.69996375947638,2.16162513319653));
#65571=CARTESIAN_POINT('',(2.6,1.6905314134756,2.01469688540291));
#65572=CARTESIAN_POINT('',(2.6,1.70404975173244,2.22527289194396));
#65573=CARTESIAN_POINT('',(0.3,1.6905314134756,2.01469688540291));
#65574=CARTESIAN_POINT('',(0.3,1.6905314134756,2.01469688540291));
#65575=CARTESIAN_POINT('',(0.3,1.70404975173244,2.22527289194396));
#65576=CARTESIAN_POINT('Origin',(0.3,1.74516836029895,2.07981066306803));
#65577=CARTESIAN_POINT('',(0.3,1.83358958134509,2.04949975535074));
#65578=CARTESIAN_POINT('Origin',(0.3,0.,0.));
#65579=CARTESIAN_POINT('',(0.3,1.6905314134756,2.01469688540291));
#65580=CARTESIAN_POINT('Origin',(0.3,1.6905314134756,2.01469688540291));
#65581=CARTESIAN_POINT('',(2.6,1.83358958134509,2.04949975535074));
#65582=CARTESIAN_POINT('',(1.35,1.83358958134509,2.04949975535074));
#65583=CARTESIAN_POINT('',(2.6,1.6905314134756,2.01469688540291));
#65584=CARTESIAN_POINT('Origin',(2.6,1.74516836029895,2.07981066306803));
#65585=CARTESIAN_POINT('Origin',(2.6,0.,0.));
#65586=CARTESIAN_POINT('Origin',(0.3,2.06457598952232,1.89556086251218));
#65587=CARTESIAN_POINT('',(2.6,2.04949975535074,1.83358958134509));
#65588=CARTESIAN_POINT('',(0.3,2.04949975535074,1.83358958134509));
#65589=CARTESIAN_POINT('',(1.35,2.04949975535074,1.83358958134509));
#65590=CARTESIAN_POINT('',(2.6,2.01469688540291,1.6905314134756));
#65591=CARTESIAN_POINT('',(2.6,2.06457598952232,1.89556086251218));
#65592=CARTESIAN_POINT('',(0.3,2.01469688540291,1.6905314134756));
#65593=CARTESIAN_POINT('',(0.3,2.01469688540291,1.6905314134756));
#65594=CARTESIAN_POINT('',(0.3,2.06457598952232,1.89556086251218));
#65595=CARTESIAN_POINT('Origin',(0.3,2.07981066306803,1.74516836029895));
#65596=CARTESIAN_POINT('',(0.3,2.16162513319653,1.69996375947638));
#65597=CARTESIAN_POINT('Origin',(0.3,0.,0.));
#65598=CARTESIAN_POINT('',(0.3,2.01469688540291,1.6905314134756));
#65599=CARTESIAN_POINT('Origin',(0.3,2.01469688540291,1.6905314134756));
#65600=CARTESIAN_POINT('',(2.6,2.16162513319653,1.69996375947638));
#65601=CARTESIAN_POINT('',(1.35,2.16162513319653,1.69996375947638));
#65602=CARTESIAN_POINT('',(2.6,2.01469688540291,1.6905314134756));
#65603=CARTESIAN_POINT('Origin',(2.6,2.07981066306803,1.74516836029895));
#65604=CARTESIAN_POINT('Origin',(2.6,0.,0.));
#65605=CARTESIAN_POINT('Origin',(0.3,2.36237113059643,1.50825317547305));
#65606=CARTESIAN_POINT('',(2.6,2.33676273825567,1.44984133790558));
#65607=CARTESIAN_POINT('',(0.3,2.33676273825567,1.44984133790558));
#65608=CARTESIAN_POINT('',(1.35,2.33676273825567,1.44984133790558));
#65609=CARTESIAN_POINT('',(2.6,2.27764681195307,1.315));
#65610=CARTESIAN_POINT('',(2.6,2.36237113059643,1.50825317547305));
#65611=CARTESIAN_POINT('',(0.3,2.27764681195307,1.315));
#65612=CARTESIAN_POINT('',(0.3,2.27764681195307,1.315));
#65613=CARTESIAN_POINT('',(0.3,2.36237113059643,1.50825317547305));
#65614=CARTESIAN_POINT('Origin',(0.3,2.35125897127475,1.3575));
#65615=CARTESIAN_POINT('',(0.3,2.42398079921089,1.29877522499351));
#65616=CARTESIAN_POINT('Origin',(0.3,0.,0.));
#65617=CARTESIAN_POINT('',(0.3,2.27764681195307,1.315));
#65618=CARTESIAN_POINT('Origin',(0.3,2.27764681195307,1.315));
#65619=CARTESIAN_POINT('',(2.6,2.42398079921089,1.29877522499351));
#65620=CARTESIAN_POINT('',(1.35,2.42398079921089,1.29877522499351));
#65621=CARTESIAN_POINT('',(2.6,2.27764681195307,1.315));
#65622=CARTESIAN_POINT('Origin',(2.6,2.35125897127475,1.3575));
#65623=CARTESIAN_POINT('Origin',(2.6,0.,0.));
#65624=CARTESIAN_POINT('Origin',(0.3,2.58838682028483,1.07511797891011));
#65625=CARTESIAN_POINT('',(2.6,2.55302436781771,1.02204039906892));
#65626=CARTESIAN_POINT('',(0.3,2.55302436781771,1.02204039906892));
#65627=CARTESIAN_POINT('',(1.35,2.55302436781771,1.02204039906892));
#65628=CARTESIAN_POINT('',(2.6,2.47139159266694,0.899512976946509));
#65629=CARTESIAN_POINT('',(2.6,2.58838682028483,1.07511797891011));
#65630=CARTESIAN_POINT('',(0.3,2.47139159266694,0.899512976946509));
#65631=CARTESIAN_POINT('',(0.3,2.47139159266694,0.899512976946509));
#65632=CARTESIAN_POINT('',(0.3,2.58838682028483,1.07511797891011));
#65633=CARTESIAN_POINT('Origin',(0.3,2.55126546543374,0.92858468912919));
#65634=CARTESIAN_POINT('',(0.3,2.61268503523469,0.858124062511184));
#65635=CARTESIAN_POINT('Origin',(0.3,0.,0.));
#65636=CARTESIAN_POINT('',(0.3,2.47139159266694,0.899512976946509));
#65637=CARTESIAN_POINT('Origin',(0.3,2.47139159266694,0.899512976946509));
#65638=CARTESIAN_POINT('',(2.6,2.61268503523469,0.858124062511184));
#65639=CARTESIAN_POINT('',(1.35,2.61268503523469,0.858124062511184));
#65640=CARTESIAN_POINT('',(2.6,2.47139159266694,0.899512976946509));
#65641=CARTESIAN_POINT('Origin',(2.6,2.55126546543374,0.92858468912919));
#65642=CARTESIAN_POINT('Origin',(2.6,0.,0.));
#65643=CARTESIAN_POINT('Origin',(0.3,2.73575568622582,0.609315866593931));
#65644=CARTESIAN_POINT('',(2.6,2.69171364385628,0.563185279883955));
#65645=CARTESIAN_POINT('',(0.3,2.69171364385628,0.563185279883955));
#65646=CARTESIAN_POINT('',(1.35,2.69171364385628,0.563185279883955));
#65647=CARTESIAN_POINT('',(2.6,2.59004439042211,0.456694707264027));
#65648=CARTESIAN_POINT('',(2.6,2.73575568622582,0.609315866593931));
#65649=CARTESIAN_POINT('',(0.3,2.59004439042211,0.456694707264027));
#65650=CARTESIAN_POINT('',(0.3,2.59004439042211,0.456694707264027));
#65651=CARTESIAN_POINT('',(0.3,2.73575568622582,0.609315866593931));
#65652=CARTESIAN_POINT('Origin',(0.3,2.67375304942814,0.471454802365716));
#65653=CARTESIAN_POINT('',(0.3,2.72200415854531,0.391399234621183));
#65654=CARTESIAN_POINT('Origin',(0.3,0.,0.));
#65655=CARTESIAN_POINT('',(0.3,2.59004439042211,0.456694707264027));
#65656=CARTESIAN_POINT('Origin',(0.3,2.59004439042211,0.456694707264027));
#65657=CARTESIAN_POINT('',(2.6,2.72200415854531,0.391399234621183));
#65658=CARTESIAN_POINT('',(1.35,2.72200415854531,0.391399234621183));
#65659=CARTESIAN_POINT('',(2.6,2.59004439042211,0.456694707264027));
#65660=CARTESIAN_POINT('Origin',(2.6,2.67375304942814,0.471454802365716));
#65661=CARTESIAN_POINT('Origin',(2.6,0.,0.));
#65662=CARTESIAN_POINT('Origin',(0.3,2.8,0.125));
#65663=CARTESIAN_POINT('',(2.6,2.74861656289909,0.0872180609552145));
#65664=CARTESIAN_POINT('',(0.3,2.74861656289909,0.0872180609552145));
#65665=CARTESIAN_POINT('',(1.35,2.74861656289909,0.0872180609552145));
#65666=CARTESIAN_POINT('',(2.6,2.63,0.));
#65667=CARTESIAN_POINT('',(2.6,2.8,0.125));
#65668=CARTESIAN_POINT('',(0.3,2.63,0.));
#65669=CARTESIAN_POINT('',(0.3,2.63,0.));
#65670=CARTESIAN_POINT('',(0.3,2.8,0.125));
#65671=CARTESIAN_POINT('Origin',(0.3,2.715,0.));
#65672=CARTESIAN_POINT('',(0.3,2.74861656289909,-0.0872180609552142));
#65673=CARTESIAN_POINT('Origin',(0.3,0.,0.));
#65674=CARTESIAN_POINT('',(0.3,2.63,0.));
#65675=CARTESIAN_POINT('Origin',(0.3,2.63,0.));
#65676=CARTESIAN_POINT('',(2.6,2.74861656289909,-0.0872180609552142));
#65677=CARTESIAN_POINT('',(1.35,2.74861656289909,-0.0872180609552142));
#65678=CARTESIAN_POINT('',(2.6,2.63,0.));
#65679=CARTESIAN_POINT('Origin',(2.6,2.715,0.));
#65680=CARTESIAN_POINT('Origin',(2.6,0.,0.));
#65681=CARTESIAN_POINT('Origin',(1.32946211310777,0.,0.));
#65682=CARTESIAN_POINT('',(0.94892422621555,0.,0.));
#65683=CARTESIAN_POINT('',(1.7,-1.23357587978679,1.51069475268627E-16));
#65684=CARTESIAN_POINT('',(1.32946211310777,-0.625,-7.65404249467096E-17));
#65685=CARTESIAN_POINT('Origin',(1.7,0.,0.));
#65686=CARTESIAN_POINT('Origin',(3.,0.,1.44337567297406));
#65687=CARTESIAN_POINT('',(3.,8.83812698937422E-17,1.44337567297406));
#65688=CARTESIAN_POINT('',(3.,1.25,0.721687836487032));
#65689=CARTESIAN_POINT('',(3.,0.3125,1.26295371385231));
#65690=CARTESIAN_POINT('',(1.7,1.38777878078145E-16,1.44337567297406));
#65691=CARTESIAN_POINT('',(3.,8.83812698937422E-17,1.44337567297406));
#65692=CARTESIAN_POINT('',(1.7,1.25,0.721687836487032));
#65693=CARTESIAN_POINT('',(1.7,1.25,0.721687836487032));
#65694=CARTESIAN_POINT('',(3.,1.25,0.721687836487032));
#65695=CARTESIAN_POINT('Origin',(3.,-1.25,0.721687836487032));
#65696=CARTESIAN_POINT('',(3.,-1.25,0.721687836487032));
#65697=CARTESIAN_POINT('',(3.,-0.9375,0.90210979560879));
#65698=CARTESIAN_POINT('',(1.7,-1.25,0.721687836487032));
#65699=CARTESIAN_POINT('',(3.,-1.25,0.721687836487032));
#65700=CARTESIAN_POINT('',(1.7,8.83812698937422E-17,1.44337567297406));
#65701=CARTESIAN_POINT('Origin',(3.,-1.25,-0.721687836487032));
#65702=CARTESIAN_POINT('',(3.,-1.25,-0.721687836487032));
#65703=CARTESIAN_POINT('',(3.,-1.25,-0.360843918243516));
#65704=CARTESIAN_POINT('',(1.7,-1.25,-0.721687836487032));
#65705=CARTESIAN_POINT('',(3.,-1.25,-0.721687836487032));
#65706=CARTESIAN_POINT('',(1.7,-1.25,0.721687836487032));
#65707=CARTESIAN_POINT('Origin',(3.,-2.77555756156289E-16,-1.44337567297406));
#65708=CARTESIAN_POINT('',(3.,-2.65143809681227E-16,-1.44337567297406));
#65709=CARTESIAN_POINT('',(3.,-0.3125,-1.26295371385231));
#65710=CARTESIAN_POINT('',(1.7,-2.77555756156289E-16,-1.44337567297406));
#65711=CARTESIAN_POINT('',(3.,-2.65143809681227E-16,-1.44337567297406));
#65712=CARTESIAN_POINT('',(1.7,-1.25,-0.721687836487032));
#65713=CARTESIAN_POINT('Origin',(3.,1.25,-0.721687836487033));
#65714=CARTESIAN_POINT('',(3.,1.25,-0.721687836487033));
#65715=CARTESIAN_POINT('',(3.,0.9375,-0.902109795608791));
#65716=CARTESIAN_POINT('',(1.7,1.25,-0.721687836487033));
#65717=CARTESIAN_POINT('',(3.,1.25,-0.721687836487033));
#65718=CARTESIAN_POINT('',(1.7,-2.65143809681227E-16,-1.44337567297406));
#65719=CARTESIAN_POINT('Origin',(3.,1.25,0.721687836487032));
#65720=CARTESIAN_POINT('',(3.,1.25,0.360843918243516));
#65721=CARTESIAN_POINT('',(1.7,1.25,-0.721687836487033));
#65722=CARTESIAN_POINT('Origin',(1.7,0.,0.));
#65723=CARTESIAN_POINT('Origin',(-35.,1.1,0.));
#65724=CARTESIAN_POINT('',(-35.,-1.1,-1.34711147906209E-16));
#65725=CARTESIAN_POINT('Origin',(-35.,0.,0.));
#65726=CARTESIAN_POINT('Origin',(-34.8,0.,0.));
#65727=CARTESIAN_POINT('',(-34.8,-1.3,-1.59204083889156E-16));
#65728=CARTESIAN_POINT('Origin',(1.35,0.,0.));
#65729=CARTESIAN_POINT('',(2.7,-2.75,-3.36777869765522E-16));
#65730=CARTESIAN_POINT('Origin',(2.7,0.,0.));
#65731=CARTESIAN_POINT('',(1.35,-2.75,-3.36777869765522E-16));
#65732=CARTESIAN_POINT('',(1.35,-2.75,-3.36777869765522E-16));
#65733=CARTESIAN_POINT('Origin',(2.85,0.,0.));
#65734=CARTESIAN_POINT('',(3.,-2.45,-3.00038465791102E-16));
#65735=CARTESIAN_POINT('Origin',(3.,0.,0.));
#65736=CARTESIAN_POINT('',(2.85,-2.6,-3.18408167778312E-16));
#65737=CARTESIAN_POINT('Origin',(3.,0.,0.));
#65738=CARTESIAN_POINT('',(0.,0.,0.));
#65739=CARTESIAN_POINT('Origin',(5.88,10.38,0.75));
#65740=CARTESIAN_POINT('',(6.,10.26,-1.5));
#65741=CARTESIAN_POINT('',(5.76,10.5,-1.5));
#65742=CARTESIAN_POINT('',(4.38,11.88,-1.5));
#65743=CARTESIAN_POINT('',(5.76,10.5,1.5));
#65744=CARTESIAN_POINT('',(5.76,10.5,0.75));
#65745=CARTESIAN_POINT('',(6.,10.26,1.5));
#65746=CARTESIAN_POINT('',(3.88,12.38,1.5));
#65747=CARTESIAN_POINT('',(6.,10.26,0.75));
#65748=CARTESIAN_POINT('Origin',(0.,10.5,1.5));
#65749=CARTESIAN_POINT('',(0.24,10.5,-1.5));
#65750=CARTESIAN_POINT('',(0.,10.5,-1.5));
#65751=CARTESIAN_POINT('',(0.24,10.5,1.5));
#65752=CARTESIAN_POINT('',(0.24,10.5,0.75));
#65753=CARTESIAN_POINT('',(0.,10.5,1.5));
#65754=CARTESIAN_POINT('Origin',(3.,11.7696910617194,-1.61890285590863));
#65755=CARTESIAN_POINT('',(5.73807935887593,11.6658808997907,-1.5));
#65756=CARTESIAN_POINT('',(5.5,11.8735012236482,-1.73780571181725));
#65757=CARTESIAN_POINT('Ctrl Pts',(5.73807935887593,11.6658808997907,-1.5));
#65758=CARTESIAN_POINT('Ctrl Pts',(5.62113668491351,11.768650949805,-1.61771152478273));
#65759=CARTESIAN_POINT('Ctrl Pts',(5.5,11.8735012236482,-1.73780571181725));
#65760=CARTESIAN_POINT('',(0.5,11.8735012236482,-1.73780571181725));
#65761=CARTESIAN_POINT('',(3.,11.8735012236482,-1.73780571181725));
#65762=CARTESIAN_POINT('',(0.261920641124074,11.6658808997907,-1.5));
#65763=CARTESIAN_POINT('Ctrl Pts',(0.5,11.8735012236482,-1.73780571181725));
#65764=CARTESIAN_POINT('Ctrl Pts',(0.378863315084015,11.7686509498028,-1.6177115247802));
#65765=CARTESIAN_POINT('Ctrl Pts',(0.261920641124074,11.6658808997907,-1.5));
#65766=CARTESIAN_POINT('',(3.,11.6658808997907,-1.5));
#65767=CARTESIAN_POINT('Origin',(3.,0.,0.));
#65768=CARTESIAN_POINT('',(5.5,1.73780571181725,-11.8735012236482));
#65769=CARTESIAN_POINT('Origin',(5.5,0.,0.));
#65770=CARTESIAN_POINT('',(0.5,1.73780571181725,-11.8735012236482));
#65771=CARTESIAN_POINT('',(3.,1.73780571181725,-11.8735012236482));
#65772=CARTESIAN_POINT('Origin',(0.5,0.,0.));
#65773=CARTESIAN_POINT('Origin',(5.75,0.,0.));
#65774=CARTESIAN_POINT('',(6.,11.4017542509914,-1.5));
#65775=CARTESIAN_POINT('Ctrl Pts',(5.73807935887593,11.6658808997907,-1.5));
#65776=CARTESIAN_POINT('Ctrl Pts',(5.87053918780798,11.5323305910383,-1.5));
#65777=CARTESIAN_POINT('Ctrl Pts',(6.,11.4017542509914,-1.5));
#65778=CARTESIAN_POINT('',(6.,1.5,-11.4017542509914));
#65779=CARTESIAN_POINT('Origin',(6.,0.,0.));
#65780=CARTESIAN_POINT('',(5.73807935887592,1.5,-11.6658808997907));
#65781=CARTESIAN_POINT('Ctrl Pts',(6.,1.5,-11.4017542509914));
#65782=CARTESIAN_POINT('Ctrl Pts',(5.87053918781806,1.5,-11.5323305910281));
#65783=CARTESIAN_POINT('Ctrl Pts',(5.73807935887592,1.5,-11.6658808997907));
#65784=CARTESIAN_POINT('Ctrl Pts',(5.5,1.73780571181725,-11.8735012236482));
#65785=CARTESIAN_POINT('Ctrl Pts',(5.62113668491587,1.61771152478031,-11.7686509498029));
#65786=CARTESIAN_POINT('Ctrl Pts',(5.73807935887592,1.5,-11.6658808997907));
#65787=CARTESIAN_POINT('Origin',(3.,11.7696910617194,1.61890285590863));
#65788=CARTESIAN_POINT('',(0.261920641124074,11.6658808997907,1.5));
#65789=CARTESIAN_POINT('',(0.5,11.8735012236482,1.73780571181725));
#65790=CARTESIAN_POINT('Ctrl Pts',(0.261920641124074,11.6658808997907,1.5));
#65791=CARTESIAN_POINT('Ctrl Pts',(0.378863315086433,11.7686509498049,1.61771152478267));
#65792=CARTESIAN_POINT('Ctrl Pts',(0.5,11.8735012236482,1.73780571181725));
#65793=CARTESIAN_POINT('',(5.5,11.8735012236482,1.73780571181725));
#65794=CARTESIAN_POINT('',(3.,11.8735012236482,1.73780571181725));
#65795=CARTESIAN_POINT('',(5.73807935887593,11.6658808997907,1.5));
#65796=CARTESIAN_POINT('Ctrl Pts',(5.5,11.8735012236482,1.73780571181725));
#65797=CARTESIAN_POINT('Ctrl Pts',(5.62113668491577,11.768650949803,1.61771152478042));
#65798=CARTESIAN_POINT('Ctrl Pts',(5.73807935887593,11.6658808997907,1.5));
#65799=CARTESIAN_POINT('',(3.,11.6658808997907,1.5));
#65800=CARTESIAN_POINT('Origin',(0.,12.5,1.5));
#65801=CARTESIAN_POINT('',(6.,11.4017542509914,1.5));
#65802=CARTESIAN_POINT('Ctrl Pts',(6.,11.4017542509914,1.5));
#65803=CARTESIAN_POINT('Ctrl Pts',(5.87053918780798,11.5323305910383,1.5));
#65804=CARTESIAN_POINT('Ctrl Pts',(5.73807935887593,11.6658808997907,1.5));
#65805=CARTESIAN_POINT('',(6.,9.775,1.5));
#65806=CARTESIAN_POINT('',(0.,10.26,1.5));
#65807=CARTESIAN_POINT('',(0.619999999999999,10.88,1.5));
#65808=CARTESIAN_POINT('',(0.,11.4017542509914,1.5));
#65809=CARTESIAN_POINT('',(0.,12.,1.5));
#65810=CARTESIAN_POINT('Ctrl Pts',(0.261920641124074,11.6658808997907,1.5));
#65811=CARTESIAN_POINT('Ctrl Pts',(0.129460812179182,11.5323305910253,1.5));
#65812=CARTESIAN_POINT('Ctrl Pts',(3.46944695195361E-17,11.4017542509914,
1.5));
#65813=CARTESIAN_POINT('Origin',(5.75,0.,0.));
#65814=CARTESIAN_POINT('',(5.5,1.73780571181725,11.8735012236482));
#65815=CARTESIAN_POINT('Origin',(5.5,0.,0.));
#65816=CARTESIAN_POINT('',(5.73807935887592,1.5,11.6658808997907));
#65817=CARTESIAN_POINT('Ctrl Pts',(5.73807935887592,1.5,11.6658808997907));
#65818=CARTESIAN_POINT('Ctrl Pts',(5.6211366849136,1.61771152478264,11.7686509498049));
#65819=CARTESIAN_POINT('Ctrl Pts',(5.5,1.73780571181725,11.8735012236482));
#65820=CARTESIAN_POINT('',(6.,1.5,11.4017542509914));
#65821=CARTESIAN_POINT('Ctrl Pts',(5.73807935887592,1.5,11.6658808997907));
#65822=CARTESIAN_POINT('Ctrl Pts',(5.87053918781908,1.5,11.5323305910271));
#65823=CARTESIAN_POINT('Ctrl Pts',(6.,1.5,11.4017542509914));
#65824=CARTESIAN_POINT('Origin',(6.,0.,0.));
#65825=CARTESIAN_POINT('Origin',(5.88,2.775,10.38));
#65826=CARTESIAN_POINT('',(6.,1.5,10.26));
#65827=CARTESIAN_POINT('',(5.76,1.5,10.5));
#65828=CARTESIAN_POINT('',(4.38,1.5,11.88));
#65829=CARTESIAN_POINT('',(5.76,-1.5,10.5));
#65830=CARTESIAN_POINT('',(5.76,2.775,10.5));
#65831=CARTESIAN_POINT('',(6.,-1.5,10.26));
#65832=CARTESIAN_POINT('',(3.88,-1.5,12.38));
#65833=CARTESIAN_POINT('',(6.,2.775,10.26));
#65834=CARTESIAN_POINT('Origin',(0.,-1.5,10.5));
#65835=CARTESIAN_POINT('',(0.24,1.5,10.5));
#65836=CARTESIAN_POINT('',(0.,1.5,10.5));
#65837=CARTESIAN_POINT('',(0.24,-1.5,10.5));
#65838=CARTESIAN_POINT('',(0.24,5.,10.5));
#65839=CARTESIAN_POINT('',(0.,-1.5,10.5));
#65840=CARTESIAN_POINT('Origin',(3.,1.61890285590863,11.7696910617194));
#65841=CARTESIAN_POINT('',(0.5,1.73780571181725,11.8735012236482));
#65842=CARTESIAN_POINT('',(3.,1.73780571181725,11.8735012236482));
#65843=CARTESIAN_POINT('',(0.261920641124077,1.5,11.6658808997907));
#65844=CARTESIAN_POINT('Ctrl Pts',(0.500000000000001,1.73780571181725,11.8735012236482));
#65845=CARTESIAN_POINT('Ctrl Pts',(0.378863315084023,1.61771152478021,11.7686509498028));
#65846=CARTESIAN_POINT('Ctrl Pts',(0.261920641124077,1.5,11.6658808997907));
#65847=CARTESIAN_POINT('',(3.,1.5,11.6658808997907));
#65848=CARTESIAN_POINT('Origin',(0.,1.5,10.5));
#65849=CARTESIAN_POINT('',(0.,1.5,11.4017542509914));
#65850=CARTESIAN_POINT('Ctrl Pts',(3.46944695195361E-17,1.5,11.4017542509914));
#65851=CARTESIAN_POINT('Ctrl Pts',(0.129460812178863,1.5,11.532330591025));
#65852=CARTESIAN_POINT('Ctrl Pts',(0.261920641124077,1.5,11.6658808997907));
#65853=CARTESIAN_POINT('',(0.,1.5,10.26));
#65854=CARTESIAN_POINT('',(0.,1.5,5.25));
#65855=CARTESIAN_POINT('',(0.12,1.5,10.38));
#65856=CARTESIAN_POINT('',(6.,1.5,5.25));
#65857=CARTESIAN_POINT('Origin',(3.,-1.61890285590862,11.7696910617194));
#65858=CARTESIAN_POINT('',(0.261920641124075,-1.5,11.6658808997907));
#65859=CARTESIAN_POINT('',(0.5,-1.73780571181725,11.8735012236482));
#65860=CARTESIAN_POINT('Ctrl Pts',(0.261920641124075,-1.5,11.6658808997907));
#65861=CARTESIAN_POINT('Ctrl Pts',(0.378863315086399,-1.61771152478264,
11.7686509498049));
#65862=CARTESIAN_POINT('Ctrl Pts',(0.5,-1.73780571181725,11.8735012236482));
#65863=CARTESIAN_POINT('',(5.5,-1.73780571181725,11.8735012236482));
#65864=CARTESIAN_POINT('',(3.,-1.73780571181725,11.8735012236482));
#65865=CARTESIAN_POINT('',(5.73807935887593,-1.5,11.6658808997907));
#65866=CARTESIAN_POINT('Ctrl Pts',(5.5,-1.73780571181725,11.8735012236482));
#65867=CARTESIAN_POINT('Ctrl Pts',(5.62113668491568,-1.61771152478051,11.7686509498031));
#65868=CARTESIAN_POINT('Ctrl Pts',(5.73807935887593,-1.5,11.6658808997907));
#65869=CARTESIAN_POINT('',(3.,-1.5,11.6658808997907));
#65870=CARTESIAN_POINT('Origin',(3.,0.,0.));
#65871=CARTESIAN_POINT('',(0.5,-11.8735012236482,1.73780571181725));
#65872=CARTESIAN_POINT('Origin',(0.5,0.,0.));
#65873=CARTESIAN_POINT('',(5.5,-11.8735012236482,1.73780571181725));
#65874=CARTESIAN_POINT('',(3.,-11.8735012236482,1.73780571181725));
#65875=CARTESIAN_POINT('Origin',(5.5,0.,0.));
#65876=CARTESIAN_POINT('Origin',(0.25,0.,0.));
#65877=CARTESIAN_POINT('',(0.,-1.5,11.4017542509914));
#65878=CARTESIAN_POINT('Ctrl Pts',(0.261920641124075,-1.5,11.6658808997907));
#65879=CARTESIAN_POINT('Ctrl Pts',(0.129460812179394,-1.5,11.5323305910256));
#65880=CARTESIAN_POINT('Ctrl Pts',(3.46944695195361E-17,-1.5,11.4017542509914));
#65881=CARTESIAN_POINT('',(3.46944695195361E-17,-11.4017542509914,1.5));
#65882=CARTESIAN_POINT('Origin',(0.,0.,0.));
#65883=CARTESIAN_POINT('',(0.261920641124076,-11.6658808997907,1.5));
#65884=CARTESIAN_POINT('Ctrl Pts',(3.46944695195361E-17,-11.4017542509914,
1.5));
#65885=CARTESIAN_POINT('Ctrl Pts',(0.129460812178545,-11.5323305910247,
1.5));
#65886=CARTESIAN_POINT('Ctrl Pts',(0.261920641124076,-11.6658808997907,
1.5));
#65887=CARTESIAN_POINT('Ctrl Pts',(0.5,-11.8735012236482,1.73780571181725));
#65888=CARTESIAN_POINT('Ctrl Pts',(0.378863315084097,-11.7686509498029,
1.61771152478029));
#65889=CARTESIAN_POINT('Ctrl Pts',(0.261920641124076,-11.6658808997907,
1.5));
#65890=CARTESIAN_POINT('Origin',(5.88,-10.38,-0.749999999999998));
#65891=CARTESIAN_POINT('',(6.,-10.26,1.5));
#65892=CARTESIAN_POINT('',(5.76,-10.5,1.5));
#65893=CARTESIAN_POINT('',(4.38,-11.88,1.5));
#65894=CARTESIAN_POINT('',(5.76,-10.5,-1.5));
#65895=CARTESIAN_POINT('',(5.76,-10.5,-0.749999999999998));
#65896=CARTESIAN_POINT('',(6.,-10.26,-1.5));
#65897=CARTESIAN_POINT('',(3.88,-12.38,-1.5));
#65898=CARTESIAN_POINT('',(6.,-10.26,-0.749999999999998));
#65899=CARTESIAN_POINT('Origin',(0.,-10.5,-1.5));
#65900=CARTESIAN_POINT('',(0.24,-10.5,1.5));
#65901=CARTESIAN_POINT('',(0.,-10.5,1.5));
#65902=CARTESIAN_POINT('',(0.24,-10.5,-1.5));
#65903=CARTESIAN_POINT('',(0.24,-10.5,-0.749999999999998));
#65904=CARTESIAN_POINT('',(0.,-10.5,-1.5));
#65905=CARTESIAN_POINT('Origin',(3.,-11.7696910617194,1.61890285590863));
#65906=CARTESIAN_POINT('',(5.73807935887592,-11.6658808997907,1.5));
#65907=CARTESIAN_POINT('Ctrl Pts',(5.73807935887592,-11.6658808997907,1.5));
#65908=CARTESIAN_POINT('Ctrl Pts',(5.6211366849137,-11.7686509498048,1.61771152478254));
#65909=CARTESIAN_POINT('Ctrl Pts',(5.5,-11.8735012236482,1.73780571181725));
#65910=CARTESIAN_POINT('',(3.,-11.6658808997907,1.5));
#65911=CARTESIAN_POINT('Origin',(5.75,0.,0.));
#65912=CARTESIAN_POINT('',(6.,-11.4017542509914,1.5));
#65913=CARTESIAN_POINT('Ctrl Pts',(5.73807935887592,-11.6658808997907,1.5));
#65914=CARTESIAN_POINT('Ctrl Pts',(5.8705391878194,-11.5323305910268,1.5));
#65915=CARTESIAN_POINT('Ctrl Pts',(6.,-11.4017542509914,1.5));
#65916=CARTESIAN_POINT('',(6.,-1.5,11.4017542509914));
#65917=CARTESIAN_POINT('Origin',(6.,0.,0.));
#65918=CARTESIAN_POINT('Ctrl Pts',(6.,-1.5,11.4017542509914));
#65919=CARTESIAN_POINT('Ctrl Pts',(5.87053918781854,-1.5,11.5323305910276));
#65920=CARTESIAN_POINT('Ctrl Pts',(5.73807935887593,-1.5,11.6658808997907));
#65921=CARTESIAN_POINT('Origin',(0.,-10.5,1.5));
#65922=CARTESIAN_POINT('',(0.,-10.26,1.5));
#65923=CARTESIAN_POINT('',(0.,0.499999999999999,1.5));
#65924=CARTESIAN_POINT('',(0.119999999999999,-10.38,1.5));
#65925=CARTESIAN_POINT('',(6.,-1.725,1.5));
#65926=CARTESIAN_POINT('Origin',(3.,-11.7696910617194,-1.61890285590862));
#65927=CARTESIAN_POINT('',(0.261920641124079,-11.6658808997907,-1.5));
#65928=CARTESIAN_POINT('',(0.5,-11.8735012236482,-1.73780571181725));
#65929=CARTESIAN_POINT('Ctrl Pts',(0.261920641124079,-11.6658808997907,
-1.5));
#65930=CARTESIAN_POINT('Ctrl Pts',(0.378863315086326,-11.7686509498049,
-1.61771152478256));
#65931=CARTESIAN_POINT('Ctrl Pts',(0.5,-11.8735012236482,-1.73780571181725));
#65932=CARTESIAN_POINT('',(5.5,-11.8735012236482,-1.73780571181725));
#65933=CARTESIAN_POINT('',(3.,-11.8735012236482,-1.73780571181725));
#65934=CARTESIAN_POINT('',(5.73807935887592,-11.6658808997907,-1.5));
#65935=CARTESIAN_POINT('Ctrl Pts',(5.5,-11.8735012236482,-1.73780571181725));
#65936=CARTESIAN_POINT('Ctrl Pts',(5.62113668491587,-11.7686509498029,-1.61771152478031));
#65937=CARTESIAN_POINT('Ctrl Pts',(5.73807935887592,-11.6658808997907,-1.5));
#65938=CARTESIAN_POINT('',(3.,-11.6658808997907,-1.5));
#65939=CARTESIAN_POINT('Origin',(3.,0.,0.));
#65940=CARTESIAN_POINT('',(0.5,-1.73780571181725,-11.8735012236482));
#65941=CARTESIAN_POINT('Origin',(0.5,0.,0.));
#65942=CARTESIAN_POINT('',(5.5,-1.73780571181725,-11.8735012236482));
#65943=CARTESIAN_POINT('',(3.,-1.73780571181725,-11.8735012236482));
#65944=CARTESIAN_POINT('Origin',(5.5,0.,0.));
#65945=CARTESIAN_POINT('Origin',(0.25,0.,0.));
#65946=CARTESIAN_POINT('',(0.,-11.4017542509914,-1.5));
#65947=CARTESIAN_POINT('Ctrl Pts',(0.261920641124079,-11.6658808997907,
-1.5));
#65948=CARTESIAN_POINT('Ctrl Pts',(0.129460812178151,-11.5323305910243,
-1.5));
#65949=CARTESIAN_POINT('Ctrl Pts',(6.93889390390723E-17,-11.4017542509914,
-1.5));
#65950=CARTESIAN_POINT('',(0.,-1.5,-11.4017542509914));
#65951=CARTESIAN_POINT('Origin',(0.,0.,0.));
#65952=CARTESIAN_POINT('',(0.261920641124077,-1.5,-11.6658808997907));
#65953=CARTESIAN_POINT('Ctrl Pts',(-3.46944695195361E-17,-1.5,-11.4017542509914));
#65954=CARTESIAN_POINT('Ctrl Pts',(0.129460812179839,-1.5,-11.532330591026));
#65955=CARTESIAN_POINT('Ctrl Pts',(0.261920641124077,-1.5,-11.6658808997907));
#65956=CARTESIAN_POINT('Ctrl Pts',(0.5,-1.73780571181725,-11.8735012236482));
#65957=CARTESIAN_POINT('Ctrl Pts',(0.378863315084089,-1.61771152478028,
-11.7686509498029));
#65958=CARTESIAN_POINT('Ctrl Pts',(0.261920641124077,-1.5,-11.6658808997907));
#65959=CARTESIAN_POINT('Origin',(0.12,10.38,0.75));
#65960=CARTESIAN_POINT('',(0.,10.26,-1.5));
#65961=CARTESIAN_POINT('',(0.119999999999999,10.38,-1.5));
#65962=CARTESIAN_POINT('',(0.,10.26,0.75));
#65963=CARTESIAN_POINT('Origin',(0.12,5.,10.38));
#65964=CARTESIAN_POINT('',(0.,-1.5,10.26));
#65965=CARTESIAN_POINT('',(0.62,-1.5,10.88));
#65966=CARTESIAN_POINT('',(0.,5.,10.26));
#65967=CARTESIAN_POINT('Origin',(0.12,-10.38,-0.749999999999998));
#65968=CARTESIAN_POINT('',(0.,-10.26,-1.5));
#65969=CARTESIAN_POINT('',(0.619999999999999,-10.88,-1.5));
#65970=CARTESIAN_POINT('',(0.,-10.26,-0.749999999999998));
#65971=CARTESIAN_POINT('Origin',(5.88,4.275,-10.38));
#65972=CARTESIAN_POINT('',(6.,-1.5,-10.26));
#65973=CARTESIAN_POINT('',(5.76,-1.5,-10.5));
#65974=CARTESIAN_POINT('',(4.38,-1.5,-11.88));
#65975=CARTESIAN_POINT('',(5.76,1.5,-10.5));
#65976=CARTESIAN_POINT('',(5.76,4.275,-10.5));
#65977=CARTESIAN_POINT('',(6.,1.5,-10.26));
#65978=CARTESIAN_POINT('',(3.88,1.5,-12.38));
#65979=CARTESIAN_POINT('',(6.,4.275,-10.26));
#65980=CARTESIAN_POINT('Origin',(0.,1.5,-10.5));
#65981=CARTESIAN_POINT('',(0.24,-1.5,-10.5));
#65982=CARTESIAN_POINT('',(0.,-1.5,-10.5));
#65983=CARTESIAN_POINT('',(0.24,1.5,-10.5));
#65984=CARTESIAN_POINT('',(0.24,6.5,-10.5));
#65985=CARTESIAN_POINT('',(0.,1.5,-10.5));
#65986=CARTESIAN_POINT('Origin',(0.12,6.5,-10.38));
#65987=CARTESIAN_POINT('',(0.,1.5,-10.26));
#65988=CARTESIAN_POINT('',(0.619999999999999,1.5,-10.88));
#65989=CARTESIAN_POINT('',(0.,-1.5,-10.26));
#65990=CARTESIAN_POINT('',(0.12,-1.5,-10.38));
#65991=CARTESIAN_POINT('',(0.,6.5,-10.26));
#65992=CARTESIAN_POINT('Origin',(3.,1.61890285590862,-11.7696910617194));
#65993=CARTESIAN_POINT('',(0.261920641124076,1.5,-11.6658808997907));
#65994=CARTESIAN_POINT('Ctrl Pts',(0.261920641124076,1.5,-11.6658808997907));
#65995=CARTESIAN_POINT('Ctrl Pts',(0.378863315086346,1.61771152478258,-11.7686509498049));
#65996=CARTESIAN_POINT('Ctrl Pts',(0.500000000000001,1.73780571181725,-11.8735012236482));
#65997=CARTESIAN_POINT('',(3.,1.5,-11.6658808997907));
#65998=CARTESIAN_POINT('Origin',(0.25,0.,0.));
#65999=CARTESIAN_POINT('',(0.,1.5,-11.4017542509914));
#66000=CARTESIAN_POINT('Ctrl Pts',(0.261920641124076,1.5,-11.6658808997907));
#66001=CARTESIAN_POINT('Ctrl Pts',(0.129460812180139,1.5,-11.5323305910263));
#66002=CARTESIAN_POINT('Ctrl Pts',(3.46944695195361E-17,1.5,-11.4017542509914));
#66003=CARTESIAN_POINT('',(0.,11.4017542509914,-1.5));
#66004=CARTESIAN_POINT('Origin',(0.,0.,0.));
#66005=CARTESIAN_POINT('Ctrl Pts',(3.46944695195361E-17,11.4017542509914,
-1.5));
#66006=CARTESIAN_POINT('Ctrl Pts',(0.129460812179182,11.5323305910253,-1.5));
#66007=CARTESIAN_POINT('Ctrl Pts',(0.261920641124074,11.6658808997907,-1.5));
#66008=CARTESIAN_POINT('Origin',(0.,1.5,-12.5));
#66009=CARTESIAN_POINT('',(6.,1.5,-6.25));
#66010=CARTESIAN_POINT('',(0.,1.5,-6.25));
#66011=CARTESIAN_POINT('Origin',(3.,-1.61890285590863,-11.7696910617194));
#66012=CARTESIAN_POINT('',(5.73807935887592,-1.5,-11.6658808997907));
#66013=CARTESIAN_POINT('Ctrl Pts',(5.73807935887592,-1.5,-11.6658808997907));
#66014=CARTESIAN_POINT('Ctrl Pts',(5.62113668491346,-1.61771152478279,-11.768650949805));
#66015=CARTESIAN_POINT('Ctrl Pts',(5.5,-1.73780571181725,-11.8735012236482));
#66016=CARTESIAN_POINT('',(3.,-1.5,-11.6658808997907));
#66017=CARTESIAN_POINT('Origin',(5.75,0.,0.));
#66018=CARTESIAN_POINT('',(6.,-1.5,-11.4017542509914));
#66019=CARTESIAN_POINT('Ctrl Pts',(5.73807935887592,-1.5,-11.6658808997907));
#66020=CARTESIAN_POINT('Ctrl Pts',(5.87053918781962,-1.5,-11.5323305910266));
#66021=CARTESIAN_POINT('Ctrl Pts',(6.,-1.5,-11.4017542509914));
#66022=CARTESIAN_POINT('',(6.,-11.4017542509914,-1.5));
#66023=CARTESIAN_POINT('Origin',(6.,0.,0.));
#66024=CARTESIAN_POINT('Ctrl Pts',(6.,-11.4017542509914,-1.5));
#66025=CARTESIAN_POINT('Ctrl Pts',(5.87053918781838,-11.5323305910278,-1.5));
#66026=CARTESIAN_POINT('Ctrl Pts',(5.73807935887592,-11.6658808997907,-1.5));
#66027=CARTESIAN_POINT('Origin',(0.,-1.5,-10.5));
#66028=CARTESIAN_POINT('',(0.,-1.5,-5.25));
#66029=CARTESIAN_POINT('',(6.,-1.5,-5.25));
#66030=CARTESIAN_POINT('Origin',(0.,11.5,0.));
#66031=CARTESIAN_POINT('',(0.,11.,-1.5));
#66032=CARTESIAN_POINT('',(0.,-0.500000000000001,-1.5));
#66033=CARTESIAN_POINT('',(0.,-1.5,6.25));
#66034=CARTESIAN_POINT('Origin',(0.,0.,0.));
#66035=CARTESIAN_POINT('',(0.,-7.05,-8.63375993398884E-16));
#66036=CARTESIAN_POINT('Origin',(0.,0.,0.));
#66037=CARTESIAN_POINT('Origin',(0.,-12.5,-1.5));
#66038=CARTESIAN_POINT('',(6.,-2.725,-1.5));
#66039=CARTESIAN_POINT('Origin',(0.,-1.5,12.5));
#66040=CARTESIAN_POINT('',(6.,-1.5,6.25));
#66041=CARTESIAN_POINT('Origin',(3.,0.,0.));
#66042=CARTESIAN_POINT('Origin',(0.5,0.,0.));
#66043=CARTESIAN_POINT('Origin',(0.25,0.,0.));
#66044=CARTESIAN_POINT('Origin',(0.,10.5,-1.5));
#66045=CARTESIAN_POINT('',(6.,8.775,-1.5));
#66046=CARTESIAN_POINT('Origin',(3.,0.,0.));
#66047=CARTESIAN_POINT('',(6.,-7.05,-8.63375993398884E-16));
#66048=CARTESIAN_POINT('Origin',(6.,0.,0.));
#66049=CARTESIAN_POINT('',(3.,-7.05,-8.63375993398884E-16));
#66050=CARTESIAN_POINT('Origin',(6.,7.05,0.));
#66051=CARTESIAN_POINT('',(0.,0.,0.));
#66052=CARTESIAN_POINT('Origin',(-3.775,0.,0.));
#66053=CARTESIAN_POINT('',(-13.2148283363937,-6.93306764378165,0.000177865042129965));
#66054=CARTESIAN_POINT('',(-13.3941716636063,-6.93294642624908,0.000111209669744707));
#66055=CARTESIAN_POINT('',(-3.775,-6.933,-8.4904762584886E-16));
#66056=CARTESIAN_POINT('',(-13.617,3.02035542106413,6.24066579987949));
#66057=CARTESIAN_POINT('Ctrl Pts',(-13.2148283363937,-6.93306764378165,
0.000177865042129965));
#66058=CARTESIAN_POINT('Ctrl Pts',(-13.2218364625447,-6.93331928540806,
0.244392711657743));
#66059=CARTESIAN_POINT('Ctrl Pts',(-13.2288445886957,-6.92066616143694,
0.488581520566852));
#66060=CARTESIAN_POINT('Ctrl Pts',(-13.2358527148466,-6.89491117443486,
0.731380409494485));
#66061=CARTESIAN_POINT('Ctrl Pts',(-13.2689040081711,-6.77344708950859,
1.87645358939269));
#66062=CARTESIAN_POINT('Ctrl Pts',(-13.3019553014956,-6.36057186435389,
2.99061222182));
#66063=CARTESIAN_POINT('Ctrl Pts',(-13.33500659482,-5.70651333434507,3.93832482936462));
#66064=CARTESIAN_POINT('Ctrl Pts',(-13.3680578881445,-5.05245480433625,
4.88603743690924));
#66065=CARTESIAN_POINT('Ctrl Pts',(-13.401109181469,-4.15721296947331,5.66730401957118));
#66066=CARTESIAN_POINT('Ctrl Pts',(-13.4341604747935,-3.12969490598308,
6.18706519987829));
#66067=CARTESIAN_POINT('Ctrl Pts',(-13.467211768118,-2.10217684249286,6.7068263801854));
#66068=CARTESIAN_POINT('Ctrl Pts',(-13.5002630614424,-0.942382550375355,
6.96508215813768));
#66069=CARTESIAN_POINT('Ctrl Pts',(-13.5333143547669,0.208594027287818,
6.93044705647606));
#66070=CARTESIAN_POINT('Ctrl Pts',(-13.5612095698446,1.18001559521549,6.90121511082712));
#66071=CARTESIAN_POINT('Ctrl Pts',(-13.5891047849223,2.14515602214522,6.66334759170891));
#66072=CARTESIAN_POINT('Ctrl Pts',(-13.617,3.02048254223755,6.24076191290031));
#66073=CARTESIAN_POINT('',(-13.617,-3.02022829989073,6.24056968685866));
#66074=CARTESIAN_POINT('Origin',(-13.617,0.,0.));
#66075=CARTESIAN_POINT('Ctrl Pts',(-13.617,-3.0202282998907,6.24056968685867));
#66076=CARTESIAN_POINT('Ctrl Pts',(-13.5839487066755,-4.0569986079954,5.73880731865404));
#66077=CARTESIAN_POINT('Ctrl Pts',(-13.550897413351,-4.96580358103262,4.97396809622495));
#66078=CARTESIAN_POINT('Ctrl Pts',(-13.5178461200266,-5.63641088424476,
4.03806620002614));
#66079=CARTESIAN_POINT('Ctrl Pts',(-13.4847948267021,-6.30701818745691,
3.10216430382733));
#66080=CARTESIAN_POINT('Ctrl Pts',(-13.4517435333776,-6.73942782084398,
1.9951997338588));
#66081=CARTESIAN_POINT('Ctrl Pts',(-13.4186922400531,-6.8809997664126,0.852378123583212));
#66082=CARTESIAN_POINT('Ctrl Pts',(-13.4105187145708,-6.91601025430248,
0.569760391756853));
#66083=CARTESIAN_POINT('Ctrl Pts',(-13.4023451890886,-6.93323415571197,
0.284949772367894));
#66084=CARTESIAN_POINT('Ctrl Pts',(-13.3941716636063,-6.93294642624908,
0.000111209669744707));
#66085=CARTESIAN_POINT('Origin',(-3.775,0.,0.));
#66086=CARTESIAN_POINT('',(-11.9648283363937,-6.93317898118896,-0.000167065473373196));
#66087=CARTESIAN_POINT('',(-12.1441716636063,-6.93330133372241,-0.00014816709062256));
#66088=CARTESIAN_POINT('',(-3.775,-6.933,-8.4904762584886E-16));
#66089=CARTESIAN_POINT('Ctrl Pts',(-11.9648283363937,-6.93317898118896,
-0.000167065473373196));
#66090=CARTESIAN_POINT('Ctrl Pts',(-11.9918876093176,-6.93222498183581,
0.942733971459933));
#66091=CARTESIAN_POINT('Ctrl Pts',(-12.0189468822415,-6.7384283406596,1.88601512439082));
#66092=CARTESIAN_POINT('Ctrl Pts',(-12.0460061551654,-6.36433591287228,
2.75135297573217));
#66093=CARTESIAN_POINT('Ctrl Pts',(-12.0790574484899,-5.90740425044193,
3.80831172070338));
#66094=CARTESIAN_POINT('Ctrl Pts',(-12.1121087418143,-5.18148623385836,
4.74898552680103));
#66095=CARTESIAN_POINT('Ctrl Pts',(-12.1451600351388,-4.27489147628079,
5.45893924348122));
#66096=CARTESIAN_POINT('Ctrl Pts',(-12.1782113284633,-3.36829671870322,
6.16889296016141));
#66097=CARTESIAN_POINT('Ctrl Pts',(-12.2112626217878,-2.28102522013168,
6.64812658742415));
#66098=CARTESIAN_POINT('Ctrl Pts',(-12.2443139151122,-1.14534608355589,
6.83834023540624));
#66099=CARTESIAN_POINT('Ctrl Pts',(-12.2773652084367,-0.00966694698010501,
7.02855388338833));
#66100=CARTESIAN_POINT('Ctrl Pts',(-12.3104165017612,1.17441982759993,6.92974755208976));
#66101=CARTESIAN_POINT('Ctrl Pts',(-12.3434677950857,2.26286733274423,6.55394127266096));
#66102=CARTESIAN_POINT('Ctrl Pts',(-12.3765190884102,3.35131483788853,6.17813499323216));
#66103=CARTESIAN_POINT('Ctrl Pts',(-12.4095703817346,4.34412307359712,5.52532876567314));
#66104=CARTESIAN_POINT('Ctrl Pts',(-12.4426216750591,5.12051461339035,4.67493796181516));
#66105=CARTESIAN_POINT('Ctrl Pts',(-12.4756729683836,5.89690615318357,3.82454715795718));
#66106=CARTESIAN_POINT('Ctrl Pts',(-12.5087242617081,6.45688099706144,2.77657177780023));
#66107=CARTESIAN_POINT('Ctrl Pts',(-12.5417755550326,6.73231690145685,1.65850050356931));
#66108=CARTESIAN_POINT('Ctrl Pts',(-12.574826848357,7.00775280585226,0.540429229338383));
#66109=CARTESIAN_POINT('Ctrl Pts',(-12.6078781416815,6.99864977076521,-0.647737938966518));
#66110=CARTESIAN_POINT('Ctrl Pts',(-12.640929435006,6.7061152074704,-1.7614577884509));
#66111=CARTESIAN_POINT('Ctrl Pts',(-12.6739807283305,6.41358064417558,-2.87517763793529));
#66112=CARTESIAN_POINT('Ctrl Pts',(-12.707032021655,5.83761455267299,-3.91445016859917));
#66113=CARTESIAN_POINT('Ctrl Pts',(-12.7400833149794,5.04828453444703,-4.75284530198096));
#66114=CARTESIAN_POINT('Ctrl Pts',(-12.7731346083039,4.25895451622106,-5.59124043536275));
#66115=CARTESIAN_POINT('Ctrl Pts',(-12.8061859016284,3.25626057127172,-6.22875817146247));
#66116=CARTESIAN_POINT('Ctrl Pts',(-12.8392371949529,2.16218276932853,-6.5878433086778));
#66117=CARTESIAN_POINT('Ctrl Pts',(-12.8722884882773,1.06810496738535,-6.94692844589313));
#66118=CARTESIAN_POINT('Ctrl Pts',(-12.9053397816018,-0.117356691551664,
-7.02758098422409));
#66119=CARTESIAN_POINT('Ctrl Pts',(-12.9383910749263,-1.24998808595104,
-6.81998875087525));
#66120=CARTESIAN_POINT('Ctrl Pts',(-12.9714423682508,-2.38261948035043,
-6.6123965175264));
#66121=CARTESIAN_POINT('Ctrl Pts',(-13.0044936615752,-3.46242061021218,
-6.11655951249774));
#66122=CARTESIAN_POINT('Ctrl Pts',(-13.0375449548997,-4.35803107659019,
-5.39279862959555));
#66123=CARTESIAN_POINT('Ctrl Pts',(-13.0705962482242,-5.25364154296821,
-4.66903774669337));
#66124=CARTESIAN_POINT('Ctrl Pts',(-13.1036475415487,-5.96506134586249,
-3.71735298591766));
#66125=CARTESIAN_POINT('Ctrl Pts',(-13.1366988348732,-6.40574477496072,
-2.65351674184525));
#66126=CARTESIAN_POINT('Ctrl Pts',(-13.1627420020467,-6.75298662422614,
-1.81525407909162));
#66127=CARTESIAN_POINT('Ctrl Pts',(-13.1887851692202,-6.93213250865378,
-0.907358320760865));
#66128=CARTESIAN_POINT('Ctrl Pts',(-13.2148283363937,-6.93306764378165,
0.000177865042129965));
#66129=CARTESIAN_POINT('Ctrl Pts',(-13.3941716636063,-6.93294642624908,
0.000111209669744707));
#66130=CARTESIAN_POINT('Ctrl Pts',(-13.3692938957641,-6.93207066378957,
-0.866852213967783));
#66131=CARTESIAN_POINT('Ctrl Pts',(-13.3444161279219,-6.76896512341342,
-1.73407450766015));
#66132=CARTESIAN_POINT('Ctrl Pts',(-13.3195383600797,-6.45138278311444,
-2.54051030748334));
#66133=CARTESIAN_POINT('Ctrl Pts',(-13.2864870667552,-6.02945959649748,
-3.61189847769166));
#66134=CARTESIAN_POINT('Ctrl Pts',(-13.2534357734307,-5.33487896551338,
-4.57599616752565));
#66135=CARTESIAN_POINT('Ctrl Pts',(-13.2203844801063,-4.45212669250648,
-5.31539786545727));
#66136=CARTESIAN_POINT('Ctrl Pts',(-13.1873331867818,-3.56937441949959,
-6.05479956338889));
#66137=CARTESIAN_POINT('Ctrl Pts',(-13.1542818934573,-2.49845050446989,
-6.56950526941814));
#66138=CARTESIAN_POINT('Ctrl Pts',(-13.1212306001328,-1.36964132464014,
-6.79696181781881));
#66139=CARTESIAN_POINT('Ctrl Pts',(-13.0881793068083,-0.240832144810394,
-7.02441836621948));
#66140=CARTESIAN_POINT('Ctrl Pts',(-13.0551280134839,0.945862299819417,
-6.96462575699158));
#66141=CARTESIAN_POINT('Ctrl Pts',(-13.0220767201594,2.04608097294984,-6.62482593361867));
#66142=CARTESIAN_POINT('Ctrl Pts',(-12.9890254268349,3.14629964608026,-6.28502611024576));
#66143=CARTESIAN_POINT('Ctrl Pts',(-12.9559741335104,4.1600425477113,-5.66521907272784));
#66144=CARTESIAN_POINT('Ctrl Pts',(-12.922922840186,4.96398389811699,-4.84082229058768));
#66145=CARTESIAN_POINT('Ctrl Pts',(-12.8898715468615,5.76792524852269,-4.01642550844751));
#66146=CARTESIAN_POINT('Ctrl Pts',(-12.856820253537,6.36206504770304,-2.9874389816851));
#66147=CARTESIAN_POINT('Ctrl Pts',(-12.8237689602125,6.67412563574283,-1.87903278923947));
#66148=CARTESIAN_POINT('Ctrl Pts',(-12.790717666888,6.98618622378262,-0.77062659679384));
#66149=CARTESIAN_POINT('Ctrl Pts',(-12.7576663735636,7.01616760068184,0.417199261334988));
#66150=CARTESIAN_POINT('Ctrl Pts',(-12.7246150802391,6.7604220353384,1.53993860937376));
#66151=CARTESIAN_POINT('Ctrl Pts',(-12.6915637869146,6.50467646999496,2.66267795741254));
#66152=CARTESIAN_POINT('Ctrl Pts',(-12.6585124935901,5.96320396240885,3.72033079536126));
#66153=CARTESIAN_POINT('Ctrl Pts',(-12.6254612002656,5.2018761213938,4.58423347136944));
#66154=CARTESIAN_POINT('Ctrl Pts',(-12.5924099069412,4.44054828037874,5.44813614737763));
#66155=CARTESIAN_POINT('Ctrl Pts',(-12.5593586136167,3.45936510593474,6.11828866144528));
#66156=CARTESIAN_POINT('Ctrl Pts',(-12.5263073202922,2.37768969654824,6.51316422990427));
#66157=CARTESIAN_POINT('Ctrl Pts',(-12.4932560269677,1.29601428716175,6.90803979836326));
#66158=CARTESIAN_POINT('Ctrl Pts',(-12.4602047336432,0.113846642832758,
7.02763842121359));
#66159=CARTESIAN_POINT('Ctrl Pts',(-12.4271534403188,-1.02499973766536,
6.85741125425395));
#66160=CARTESIAN_POINT('Ctrl Pts',(-12.3941021469943,-2.16384611816347,
6.68718408729431));
#66161=CARTESIAN_POINT('Ctrl Pts',(-12.3610508536698,-3.25937123483072,
6.2271311305247));
#66162=CARTESIAN_POINT('Ctrl Pts',(-12.3279995603453,-4.17830194280872,
5.53321858179927));
#66163=CARTESIAN_POINT('Ctrl Pts',(-12.2949482670209,-5.09723265078673,
4.83930603307384));
#66164=CARTESIAN_POINT('Ctrl Pts',(-12.2618969736964,-5.8395689500755,3.91153389239259));
#66165=CARTESIAN_POINT('Ctrl Pts',(-12.2288456803719,-6.31500388982293,
2.86276795740906));
#66166=CARTESIAN_POINT('Ctrl Pts',(-12.2006210081167,-6.72100904130986,
1.96715777669006));
#66167=CARTESIAN_POINT('Ctrl Pts',(-12.1723963358615,-6.93237437728127,
0.983311965242192));
#66168=CARTESIAN_POINT('Ctrl Pts',(-12.1441716636063,-6.93330133372241,
-0.00014816709062256));
#66169=CARTESIAN_POINT('Origin',(-3.775,0.,0.));
#66170=CARTESIAN_POINT('',(-10.7148283363937,-6.93246113187516,7.73909840809384E-5));
#66171=CARTESIAN_POINT('',(-10.8941716636063,-6.93242320179691,4.17880428927411E-5));
#66172=CARTESIAN_POINT('',(-3.775,-6.933,-8.4904762584886E-16));
#66173=CARTESIAN_POINT('Ctrl Pts',(-10.7148283363937,-6.93246113187516,
7.73909840809384E-5));
#66174=CARTESIAN_POINT('Ctrl Pts',(-10.7288874627661,-6.93265361386657,
0.490124109213171));
#66175=CARTESIAN_POINT('Ctrl Pts',(-10.7429465891384,-6.88142264742765,
0.980131164451067));
#66176=CARTESIAN_POINT('Ctrl Pts',(-10.7570057155107,-6.77835452257098,
1.45898073080005));
#66177=CARTESIAN_POINT('Ctrl Pts',(-10.7900570088352,-6.53605391748161,
2.58469772462808));
#66178=CARTESIAN_POINT('Ctrl Pts',(-10.8231083021597,-6.00726861161217,
3.64875142588059));
#66179=CARTESIAN_POINT('Ctrl Pts',(-10.8561595954841,-5.25632656572988,
4.52169723012369));
#66180=CARTESIAN_POINT('Ctrl Pts',(-10.8892108888086,-4.50538451984759,
5.3946430343668));
#66181=CARTESIAN_POINT('Ctrl Pts',(-10.9222621821331,-3.53228573395244,
6.07648094160049));
#66182=CARTESIAN_POINT('Ctrl Pts',(-10.9553134754576,-2.45540993574669,
6.48426378657882));
#66183=CARTESIAN_POINT('Ctrl Pts',(-10.9883647687821,-1.37853413754095,
6.89204663155715));
#66184=CARTESIAN_POINT('Ctrl Pts',(-11.0214160621065,-0.197881327024614,
7.02577441428012));
#66185=CARTESIAN_POINT('Ctrl Pts',(-11.054467355431,0.942919338880705,6.86917883934291));
#66186=CARTESIAN_POINT('Ctrl Pts',(-11.0875186487555,2.08372000478602,6.7125832644057));
#66187=CARTESIAN_POINT('Ctrl Pts',(-11.12056994208,3.18466852608032,6.2656643318083));
#66188=CARTESIAN_POINT('Ctrl Pts',(-11.1536212354045,4.1118319577694,5.58279076784725));
#66189=CARTESIAN_POINT('Ctrl Pts',(-11.1866725287289,5.03899538945848,4.89991720388618));
#66190=CARTESIAN_POINT('Ctrl Pts',(-11.2197238220534,5.79237373154235,3.98108900856145));
#66191=CARTESIAN_POINT('Ctrl Pts',(-11.2527751153779,6.28031675869468,2.93808376615998));
#66192=CARTESIAN_POINT('Ctrl Pts',(-11.2858264087024,6.76825978584702,1.89507852375851));
#66193=CARTESIAN_POINT('Ctrl Pts',(-11.3188777020268,6.99076749806784,0.727896234280309));
#66194=CARTESIAN_POINT('Ctrl Pts',(-11.3519289953513,6.9207713153042,-0.421472665512276));
#66195=CARTESIAN_POINT('Ctrl Pts',(-11.3849802886758,6.85077513254057,-1.57084156530486));
#66196=CARTESIAN_POINT('Ctrl Pts',(-11.4180315820003,6.48827505479248,-2.70239707541183));
#66197=CARTESIAN_POINT('Ctrl Pts',(-11.4510828753248,5.87737005856666,-3.67848283958341));
#66198=CARTESIAN_POINT('Ctrl Pts',(-11.4841341686492,5.26646506234084,-4.65456860375499));
#66199=CARTESIAN_POINT('Ctrl Pts',(-11.5171854619737,4.40715514763729,-5.47518462199118));
#66200=CARTESIAN_POINT('Ctrl Pts',(-11.5502367552982,3.40397736165498,-6.04050104941805));
#66201=CARTESIAN_POINT('Ctrl Pts',(-11.5832880486227,2.40079957567267,-6.60581747684491));
#66202=CARTESIAN_POINT('Ctrl Pts',(-11.6163393419471,1.25375391841161,-6.91583431346245));
#66203=CARTESIAN_POINT('Ctrl Pts',(-11.6493906352716,0.102381158542403,
-6.93283729107388));
#66204=CARTESIAN_POINT('Ctrl Pts',(-11.6824419285961,-1.0489916013268,-6.94984026868531));
#66205=CARTESIAN_POINT('Ctrl Pts',(-11.7154932219206,-2.20469146380415,
-6.67382938729065));
#66206=CARTESIAN_POINT('Ctrl Pts',(-11.7485445152451,-3.22412485607506,
-6.13838201153716));
#66207=CARTESIAN_POINT('Ctrl Pts',(-11.7815958085695,-4.24355824834597,
-5.60293463578368));
#66208=CARTESIAN_POINT('Ctrl Pts',(-11.814647101894,-5.12672517041044,-4.80805076567137));
#66209=CARTESIAN_POINT('Ctrl Pts',(-11.8476983952185,-5.76618631467301,
-3.85042987084347));
#66210=CARTESIAN_POINT('Ctrl Pts',(-11.880749688543,-6.40564745893558,-2.89280897601557));
#66211=CARTESIAN_POINT('Ctrl Pts',(-11.9138009818675,-6.80140282539625,
-1.77245105647208));
#66212=CARTESIAN_POINT('Ctrl Pts',(-11.9468522751919,-6.90530785448801,
-0.625650254777943));
#66213=CARTESIAN_POINT('Ctrl Pts',(-11.9528442955925,-6.9241452732822,-0.417741483048112));
#66214=CARTESIAN_POINT('Ctrl Pts',(-11.9588363159931,-6.93339023533471,
-0.20896359392941));
#66215=CARTESIAN_POINT('Ctrl Pts',(-11.9648283363937,-6.93317898118896,
-0.000167065473373196));
#66216=CARTESIAN_POINT('Ctrl Pts',(-12.1441716636063,-6.93330133372241,
-0.00014816709062256));
#66217=CARTESIAN_POINT('Ctrl Pts',(-12.139345042537,-6.93345984991167,-0.168326892164513));
#66218=CARTESIAN_POINT('Ctrl Pts',(-12.1345184214677,-6.92746442206593,
-0.336494338650843));
#66219=CARTESIAN_POINT('Ctrl Pts',(-12.1296918003985,-6.91523604410695,
-0.504207325629335));
#66220=CARTESIAN_POINT('Ctrl Pts',(-12.096640507074,-6.83149967843746,-1.6526569443984));
#66221=CARTESIAN_POINT('Ctrl Pts',(-12.0635892137495,-6.45549336689239,
-2.77979645265072));
#66222=CARTESIAN_POINT('Ctrl Pts',(-12.030537920425,-5.83295914650944,-3.74850666788663));
#66223=CARTESIAN_POINT('Ctrl Pts',(-11.9974866271005,-5.2104249261265,-4.71721688312255));
#66224=CARTESIAN_POINT('Ctrl Pts',(-11.9644353337761,-4.3413627969057,-5.52749780534206));
#66225=CARTESIAN_POINT('Ctrl Pts',(-11.9313840404516,-3.3314961877589,-6.08077690042575));
#66226=CARTESIAN_POINT('Ctrl Pts',(-11.8983327471271,-2.32162957861211,
-6.63405599550944));
#66227=CARTESIAN_POINT('Ctrl Pts',(-11.8652814538026,-1.17095848953932,
-6.9303332634573));
#66228=CARTESIAN_POINT('Ctrl Pts',(-11.8322301604781,-0.0194647302894101,
-6.93356587491011));
#66229=CARTESIAN_POINT('Ctrl Pts',(-11.7991788671537,1.13202902896051,-6.93679848636293));
#66230=CARTESIAN_POINT('Ctrl Pts',(-11.7661275738292,2.28434545838755,-6.6469864413207));
#66231=CARTESIAN_POINT('Ctrl Pts',(-11.7330762805047,3.29730258707578,-6.09938605419939));
#66232=CARTESIAN_POINT('Ctrl Pts',(-11.7000249871802,4.310259715764,-5.55178566707809));
#66233=CARTESIAN_POINT('Ctrl Pts',(-11.6669736938558,5.18385754371339,-4.7463969378777));
#66234=CARTESIAN_POINT('Ctrl Pts',(-11.6339224005313,5.81182086618272,-3.7811972732666));
#66235=CARTESIAN_POINT('Ctrl Pts',(-11.6008711072068,6.43978418865204,-2.81599760865551));
#66236=CARTESIAN_POINT('Ctrl Pts',(-11.5678198138823,6.82211300564129,-1.69098700863372));
#66237=CARTESIAN_POINT('Ctrl Pts',(-11.5347685205578,6.91229612830372,-0.543025627548823));
#66238=CARTESIAN_POINT('Ctrl Pts',(-11.5017172272334,7.00247925096614,0.604935753536091));
#66239=CARTESIAN_POINT('Ctrl Pts',(-11.4686659339089,6.80051667930173,1.77584791568409));
#66240=CARTESIAN_POINT('Ctrl Pts',(-11.4356146405844,6.3309776293689,2.82726667529135));
#66241=CARTESIAN_POINT('Ctrl Pts',(-11.4025633472599,5.86143857943607,3.8786854348986));
#66242=CARTESIAN_POINT('Ctrl Pts',(-11.3695120539354,5.12432305123482,4.8106107919651));
#66243=CARTESIAN_POINT('Ctrl Pts',(-11.336460760611,4.20930286096558,5.50967186162471));
#66244=CARTESIAN_POINT('Ctrl Pts',(-11.3034094672865,3.29428267069634,6.20873293128433));
#66245=CARTESIAN_POINT('Ctrl Pts',(-11.270358173962,2.2013578183591,6.67492971353706));
#66246=CARTESIAN_POINT('Ctrl Pts',(-11.2373068806375,1.06348515100223,6.85154828711766));
#66247=CARTESIAN_POINT('Ctrl Pts',(-11.2042555873131,-0.0743875163546409,
7.02816686069827));
#66248=CARTESIAN_POINT('Ctrl Pts',(-11.1712042939886,-1.25720799873115,
6.91520722560674));
#66249=CARTESIAN_POINT('Ctrl Pts',(-11.1381530006641,-2.3410834368994,6.5264111837318));
#66250=CARTESIAN_POINT('Ctrl Pts',(-11.1051017073396,-3.42495887506765,
6.13761514185686));
#66251=CARTESIAN_POINT('Ctrl Pts',(-11.0720504140151,-4.40988926902763,
5.47298269319852));
#66252=CARTESIAN_POINT('Ctrl Pts',(-11.0389991206907,-5.17605554846697,
4.61336791905991));
#66253=CARTESIAN_POINT('Ctrl Pts',(-11.0059478273662,-5.94222182790631,
3.75375314492132));
#66254=CARTESIAN_POINT('Ctrl Pts',(-10.9728965340417,-6.489623992825,2.69915604530247));
#66255=CARTESIAN_POINT('Ctrl Pts',(-10.9398452407172,-6.75166929831051,
1.57787080705134));
#66256=CARTESIAN_POINT('Ctrl Pts',(-10.9246207150136,-6.87237608729205,
1.061369508198));
#66257=CARTESIAN_POINT('Ctrl Pts',(-10.9093961893099,-6.93253499603995,
0.530718118686483));
#66258=CARTESIAN_POINT('Ctrl Pts',(-10.8941716636063,-6.93242320179691,
4.17880428927411E-5));
#66259=CARTESIAN_POINT('Origin',(-3.775,0.,0.));
#66260=CARTESIAN_POINT('',(-9.46482833639373,-6.9335752955847,3.8715574435539E-5));
#66261=CARTESIAN_POINT('',(-9.64417166360628,-6.93351961894304,7.87873629847102E-5));
#66262=CARTESIAN_POINT('',(-3.775,-6.933,-8.4904762584886E-16));
#66263=CARTESIAN_POINT('Ctrl Pts',(-9.46482833639373,-6.9335752955847,3.8715574435539E-5));
#66264=CARTESIAN_POINT('Ctrl Pts',(-9.46588731621449,-6.93358665184356,
0.0369335697061642));
#66265=CARTESIAN_POINT('Ctrl Pts',(-9.46694629603526,-6.93329830646238,
0.0738282457414585));
#66266=CARTESIAN_POINT('Ctrl Pts',(-9.46800527585603,-6.9327091605576,0.11071811787296));
#66267=CARTESIAN_POINT('Ctrl Pts',(-9.50105656918051,-6.91432162027785,
1.26206959843057));
#66268=CARTESIAN_POINT('Ctrl Pts',(-9.534107862505,-6.60292563630512,2.40874161780564));
#66269=CARTESIAN_POINT('Ctrl Pts',(-9.56715915582948,-6.03640325342724,
3.41123886125227));
#66270=CARTESIAN_POINT('Ctrl Pts',(-9.60021044915396,-5.46988087054935,
4.4137361046989));
#66271=CARTESIAN_POINT('Ctrl Pts',(-9.63326174247843,-4.6482320887663,5.27205857221708));
#66272=CARTESIAN_POINT('Ctrl Pts',(-9.66631303580291,-3.67141239097886,
5.88178934184756));
#66273=CARTESIAN_POINT('Ctrl Pts',(-9.69936432912738,-2.69459269319141,
6.49152011147804));
#66274=CARTESIAN_POINT('Ctrl Pts',(-9.73241562245186,-1.56260207939957,
6.85265918322081));
#66275=CARTESIAN_POINT('Ctrl Pts',(-9.76546691577634,-0.413149837256818,
6.9212731501133));
#66276=CARTESIAN_POINT('Ctrl Pts',(-9.79851820910082,0.736302404885922,
6.98988711700579));
#66277=CARTESIAN_POINT('Ctrl Pts',(-9.8315695024253,1.90321627537957,6.76597597904801));
#66278=CARTESIAN_POINT('Ctrl Pts',(-9.86462079574978,2.94563399127012,6.27677904629267));
#66279=CARTESIAN_POINT('Ctrl Pts',(-9.89767208907426,3.98805170716067,5.78758211353733));
#66280=CARTESIAN_POINT('Ctrl Pts',(-9.93072338239874,4.90597326844813,5.03309938598441));
#66281=CARTESIAN_POINT('Ctrl Pts',(-9.96377467572322,5.58773138497425,4.1051154400185));
#66282=CARTESIAN_POINT('Ctrl Pts',(-9.99682596904769,6.26948950150039,3.17713149405257));
#66283=CARTESIAN_POINT('Ctrl Pts',(-10.0298772623722,6.71508417326519,2.07564632967368));
#66284=CARTESIAN_POINT('Ctrl Pts',(-10.0629285556967,6.87030777338264,0.934658175753425));
#66285=CARTESIAN_POINT('Ctrl Pts',(-10.0959798490211,7.02553137350009,-0.206329978166798));
#66286=CARTESIAN_POINT('Ctrl Pts',(-10.1290311423456,6.89038390197017,-1.38682112162837));
#66287=CARTESIAN_POINT('Ctrl Pts',(-10.1620824356701,6.48130636263677,-2.46320576488217));
#66288=CARTESIAN_POINT('Ctrl Pts',(-10.1951337289946,6.07222882330335,-3.53959040813599));
#66289=CARTESIAN_POINT('Ctrl Pts',(-10.228185022319,5.38922121616644,-4.51186855118207));
#66290=CARTESIAN_POINT('Ctrl Pts',(-10.2612363156435,4.51537300318336,-5.26176029942713));
#66291=CARTESIAN_POINT('Ctrl Pts',(-10.294287608968,3.64152479020029,-6.01165204767217));
#66292=CARTESIAN_POINT('Ctrl Pts',(-10.3273389022925,2.57683597137107,-6.53915740111618));
#66293=CARTESIAN_POINT('Ctrl Pts',(-10.360390195617,1.45082841465755,-6.78010410817761));
#66294=CARTESIAN_POINT('Ctrl Pts',(-10.3934414889414,0.32482085794402,-7.02105081523904));
#66295=CARTESIAN_POINT('Ctrl Pts',(-10.4264927822659,-0.862505436653806,
-6.9754388759179));
#66296=CARTESIAN_POINT('Ctrl Pts',(-10.4595440755904,-1.9667094673739,-6.64881708858398));
#66297=CARTESIAN_POINT('Ctrl Pts',(-10.4925953689149,-3.070913498094,-6.32219530125007));
#66298=CARTESIAN_POINT('Ctrl Pts',(-10.5256466622394,-4.09199526493636,
-5.71456366590338));
#66299=CARTESIAN_POINT('Ctrl Pts',(-10.5586979555638,-4.90573779910758,
-4.89984198244309));
#66300=CARTESIAN_POINT('Ctrl Pts',(-10.5917492488883,-5.7194803332788,-4.0851202989828));
#66301=CARTESIAN_POINT('Ctrl Pts',(-10.6248005422128,-6.32588363477888,
-3.0633085674089));
#66302=CARTESIAN_POINT('Ctrl Pts',(-10.6578518355373,-6.65117733337426,
-1.95871255842018));
#66303=CARTESIAN_POINT('Ctrl Pts',(-10.6768440024894,-6.83809988952223,
-1.32398182000576));
#66304=CARTESIAN_POINT('Ctrl Pts',(-10.6958361694416,-6.9322011121542,-0.661916024572997));
#66305=CARTESIAN_POINT('Ctrl Pts',(-10.7148283363937,-6.93246113187516,
7.73909840809384E-5));
#66306=CARTESIAN_POINT('Ctrl Pts',(-10.8941716636063,-6.93242320179691,
4.17880428927411E-5));
#66307=CARTESIAN_POINT('Ctrl Pts',(-10.8763448959854,-6.93229229919733,
-0.621340041014074));
#66308=CARTESIAN_POINT('Ctrl Pts',(-10.8585181283646,-6.8495264177626,-1.24275606595426));
#66309=CARTESIAN_POINT('Ctrl Pts',(-10.8406913607438,-6.68457054115384,
-1.8415296027582));
#66310=CARTESIAN_POINT('Ctrl Pts',(-10.8076400674193,-6.37873803245931,
-2.95167139743321));
#66311=CARTESIAN_POINT('Ctrl Pts',(-10.7745887740948,-5.79038456901791,
-3.98398160989983));
#66312=CARTESIAN_POINT('Ctrl Pts',(-10.7415374807704,-4.99108471633639,
-4.81287730488004));
#66313=CARTESIAN_POINT('Ctrl Pts',(-10.7084861874459,-4.19178486365487,
-5.64177299986026));
#66314=CARTESIAN_POINT('Ctrl Pts',(-10.6754348941214,-3.18153862173323,
-6.26725417735407));
#66315=CARTESIAN_POINT('Ctrl Pts',(-10.6423836007969,-2.08324479258817,
-6.61322959919343));
#66316=CARTESIAN_POINT('Ctrl Pts',(-10.6093323074724,-0.984950963443121,
-6.9592050210328));
#66317=CARTESIAN_POINT('Ctrl Pts',(-10.576281014148,0.201390452925348,-7.02567468721771));
#66318=CARTESIAN_POINT('Ctrl Pts',(-10.5432297208235,1.33145826747934,-6.80455240845744));
#66319=CARTESIAN_POINT('Ctrl Pts',(-10.510178427499,2.46152608203333,-6.58343012969718));
#66320=CARTESIAN_POINT('Ctrl Pts',(-10.4771271341745,3.53532029477285,-6.07471590599172));
#66321=CARTESIAN_POINT('Ctrl Pts',(-10.44407584085,4.42221134541617,-5.34029600433914));
#66322=CARTESIAN_POINT('Ctrl Pts',(-10.4110245475256,5.30910239605948,-4.60587610268656));
#66323=CARTESIAN_POINT('Ctrl Pts',(-10.3779732542011,6.0090902846066,-3.64575052308685));
#66324=CARTESIAN_POINT('Ctrl Pts',(-10.3449219608766,6.4370198584233,-2.57672077256163));
#66325=CARTESIAN_POINT('Ctrl Pts',(-10.3118706675521,6.86494943223999,-1.50769102203641));
#66326=CARTESIAN_POINT('Ctrl Pts',(-10.2788193742277,7.02082069132626,-0.329757100585688));
#66327=CARTESIAN_POINT('Ctrl Pts',(-10.2457680809032,6.88567153494304,0.813782594039565));
#66328=CARTESIAN_POINT('Ctrl Pts',(-10.2127167875787,6.75052237855983,1.95732228866483));
#66329=CARTESIAN_POINT('Ctrl Pts',(-10.1796654942542,6.32435280670714,3.0664677564646));
#66330=CARTESIAN_POINT('Ctrl Pts',(-10.1466142009297,5.65900733774437,4.0062888748619));
#66331=CARTESIAN_POINT('Ctrl Pts',(-10.1135629076053,4.99366186878161,4.9461099932592));
#66332=CARTESIAN_POINT('Ctrl Pts',(-10.0805116142808,4.08914050270877,5.71660676225401));
#66333=CARTESIAN_POINT('Ctrl Pts',(-10.0474603209563,3.05548036480908,6.22404646012164));
#66334=CARTESIAN_POINT('Ctrl Pts',(-10.0144090276318,2.0218202269094,6.73148615798928));
#66335=CARTESIAN_POINT('Ctrl Pts',(-9.98135773430734,0.859021317182861,
6.97586878472975));
#66336=CARTESIAN_POINT('Ctrl Pts',(-9.94830644098286,-0.291459175952402,
6.92746462612693));
#66337=CARTESIAN_POINT('Ctrl Pts',(-9.91525514765838,-1.44193966908766,
6.87906046752411));
#66338=CARTESIAN_POINT('Ctrl Pts',(-9.8822038543339,-2.58010174563166,6.537869523578));
#66339=CARTESIAN_POINT('Ctrl Pts',(-9.84915256100942,-3.56748534515149,
5.94539846516749));
#66340=CARTESIAN_POINT('Ctrl Pts',(-9.81610126768494,-4.55486894467133,
5.35292740675699));
#66341=CARTESIAN_POINT('Ctrl Pts',(-9.78304997436047,-5.39147406716701,
4.5091762338821));
#66342=CARTESIAN_POINT('Ctrl Pts',(-9.74999868103599,-5.97552575614819,
3.51678923666124));
#66343=CARTESIAN_POINT('Ctrl Pts',(-9.71694738771152,-6.55957744512937,
2.52440223944039));
#66344=CARTESIAN_POINT('Ctrl Pts',(-9.68389609438704,-6.89107570059605,
1.38337941787357));
#66345=CARTESIAN_POINT('Ctrl Pts',(-9.65084480106256,-6.9296929897379,0.232528848670892));
#66346=CARTESIAN_POINT('Ctrl Pts',(-9.64862042191046,-6.93229196497418,
0.155075661342478));
#66347=CARTESIAN_POINT('Ctrl Pts',(-9.64639604275837,-6.93356436504135,
0.0775779602098864));
#66348=CARTESIAN_POINT('Ctrl Pts',(-9.64417166360628,-6.93351961894304,
7.87873629847102E-5));
#66349=CARTESIAN_POINT('Origin',(-3.775,0.,0.));
#66350=CARTESIAN_POINT('',(-8.21482833639373,-6.93258532737551,-0.000132552009395881));
#66351=CARTESIAN_POINT('',(-8.39417166360628,-6.93268012709199,-0.00015517830160834));
#66352=CARTESIAN_POINT('',(-3.775,-6.933,-8.4904762584886E-16));
#66353=CARTESIAN_POINT('Ctrl Pts',(-8.21482833639373,-6.93258532737551,
-0.000132552009395881));
#66354=CARTESIAN_POINT('Ctrl Pts',(-8.23593846298743,-6.93207868762057,
0.735646992959097));
#66355=CARTESIAN_POINT('Ctrl Pts',(-8.25704858958112,-6.81542918802548,
1.47158339831407));
#66356=CARTESIAN_POINT('Ctrl Pts',(-8.27815871617481,-6.58523850360685,
2.17010337475394));
#66357=CARTESIAN_POINT('Ctrl Pts',(-8.31121000949928,-6.22483802009874,
3.26374857540489));
#66358=CARTESIAN_POINT('Ctrl Pts',(-8.34426130282376,-5.58611481446254,
4.26567514229184));
#66359=CARTESIAN_POINT('Ctrl Pts',(-8.37731259614824,-4.74677104834537,
5.0539963811913));
#66360=CARTESIAN_POINT('Ctrl Pts',(-8.41036388947272,-3.90742728222822,
5.84231762009076));
#66361=CARTESIAN_POINT('Ctrl Pts',(-8.44341518279719,-2.86746295563012,
6.41703353100273));
#66362=CARTESIAN_POINT('Ctrl Pts',(-8.47646647612167,-1.75339214460081,
6.70822858836495));
#66363=CARTESIAN_POINT('Ctrl Pts',(-8.50951776944615,-0.639321333571469,
6.99942364572718));
#66364=CARTESIAN_POINT('Ctrl Pts',(-8.54256906277064,0.548855961889083,
7.00709784953965));
#66365=CARTESIAN_POINT('Ctrl Pts',(-8.57562035609511,1.66659521378707,6.73031761508226));
#66366=CARTESIAN_POINT('Ctrl Pts',(-8.60867164941959,2.78433446568503,6.45353738062489));
#66367=CARTESIAN_POINT('Ctrl Pts',(-8.64172294274407,3.83163567402044,5.89230270789768));
#66368=CARTESIAN_POINT('Ctrl Pts',(-8.67477423606855,4.68109221403745,5.11488909852233));
#66369=CARTESIAN_POINT('Ctrl Pts',(-8.70782552939302,5.53054875405448,4.33747548914697));
#66370=CARTESIAN_POINT('Ctrl Pts',(-8.7408768227175,6.18216062575312,3.34388294312347));
#66371=CARTESIAN_POINT('Ctrl Pts',(-8.77392811604198,6.55665773132082,2.25498430167829));
#66372=CARTESIAN_POINT('Ctrl Pts',(-8.80697940936646,6.93115483688851,1.16608566023314));
#66373=CARTESIAN_POINT('Ctrl Pts',(-8.84003070269094,7.02853717632526,-0.018119076633696));
#66374=CARTESIAN_POINT('Ctrl Pts',(-8.87308199601542,6.83695796183047,-1.15356865190917));
#66375=CARTESIAN_POINT('Ctrl Pts',(-8.9061332893399,6.64537874733568,-2.28901822718469));
#66376=CARTESIAN_POINT('Ctrl Pts',(-8.93918458266438,6.16483797890932,-3.37571264086885));
#66377=CARTESIAN_POINT('Ctrl Pts',(-8.97223587598886,5.45379455727212,-4.28145299326918));
#66378=CARTESIAN_POINT('Ctrl Pts',(-9.00528716931333,4.74275113563496,-5.18719334566947));
#66379=CARTESIAN_POINT('Ctrl Pts',(-9.03833846263781,3.80120506078698,-5.91197963678595));
#66380=CARTESIAN_POINT('Ctrl Pts',(-9.07138975596229,2.7436975998381,-6.36763993070802));
#66381=CARTESIAN_POINT('Ctrl Pts',(-9.10444104928677,1.68619013888922,-6.82330022463009));
#66382=CARTESIAN_POINT('Ctrl Pts',(-9.13749234261125,0.512721291839444,
-7.00983452135775));
#66383=CARTESIAN_POINT('Ctrl Pts',(-9.17054363593573,-0.6339537302327,-6.90455049039608));
#66384=CARTESIAN_POINT('Ctrl Pts',(-9.20359492926021,-1.78062875230486,
-6.79926645943441));
#66385=CARTESIAN_POINT('Ctrl Pts',(-9.23664622258468,-2.90050994939938,
-6.40216410078339));
#66386=CARTESIAN_POINT('Ctrl Pts',(-9.26969751590916,-3.85736117253282,
-5.76155183879664));
#66387=CARTESIAN_POINT('Ctrl Pts',(-9.30274880923364,-4.81421239566625,
-5.12093957680988));
#66388=CARTESIAN_POINT('Ctrl Pts',(-9.33580010255813,-5.60803364483859,
-4.23681741148739));
#66389=CARTESIAN_POINT('Ctrl Pts',(-9.3688513958826,-6.14225472113137,-3.21674085795608));
#66390=CARTESIAN_POINT('Ctrl Pts',(-9.40084370938631,-6.65935908934048,
-2.22934806282485));
#66391=CARTESIAN_POINT('Ctrl Pts',(-9.43283602289002,-6.93323221728751,
-1.11457340158659));
#66392=CARTESIAN_POINT('Ctrl Pts',(-9.46482833639373,-6.9335752955847,3.8715574435539E-5));
#66393=CARTESIAN_POINT('Ctrl Pts',(-9.64417166360628,-6.93351961894304,
7.87873629847102E-5));
#66394=CARTESIAN_POINT('Ctrl Pts',(-9.61334474943389,-6.93289949798433,
-1.07395589217263));
#66395=CARTESIAN_POINT('Ctrl Pts',(-9.5825178352615,-6.67930505166503,-2.14827323277089));
#66396=CARTESIAN_POINT('Ctrl Pts',(-9.55169092108911,-6.19783372514389,
-3.10830688847735));
#66397=CARTESIAN_POINT('Ctrl Pts',(-9.51863962776464,-5.68162084859103,
-4.13761373958437));
#66398=CARTESIAN_POINT('Ctrl Pts',(-9.48558833444016,-4.9034587726683,-5.03554912495985));
#66399=CARTESIAN_POINT('Ctrl Pts',(-9.45253704111568,-3.95801272149387,
-5.69287711917089));
#66400=CARTESIAN_POINT('Ctrl Pts',(-9.4194857477912,-3.01256667031946,-6.35020511338191));
#66401=CARTESIAN_POINT('Ctrl Pts',(-9.38643445446672,-1.89983664389337,
-6.76692571642851));
#66402=CARTESIAN_POINT('Ctrl Pts',(-9.35338316114224,-0.755188834675868,
-6.8923438989554));
#66403=CARTESIAN_POINT('Ctrl Pts',(-9.32033186781776,0.389458974541642,
-7.01776208148228));
#66404=CARTESIAN_POINT('Ctrl Pts',(-9.28728057449329,1.56602456655058,-6.85187784348945));
#66405=CARTESIAN_POINT('Ctrl Pts',(-9.25422928116881,2.6313760040547,-6.41487138785898));
#66406=CARTESIAN_POINT('Ctrl Pts',(-9.22117798784433,3.69672744155883,-5.97786493222852));
#66407=CARTESIAN_POINT('Ctrl Pts',(-9.18812669451985,4.65086472455815,-5.26973625896042));
#66408=CARTESIAN_POINT('Ctrl Pts',(-9.15507540119538,5.3777148362232,-4.37663086606029));
#66409=CARTESIAN_POINT('Ctrl Pts',(-9.1220241078709,6.10456494788824,-3.48352547316016));
#66410=CARTESIAN_POINT('Ctrl Pts',(-9.08897281454642,6.60412788821901,-2.405443360628));
#66411=CARTESIAN_POINT('Ctrl Pts',(-9.05592152122194,6.81563066509628,-1.27353572171572));
#66412=CARTESIAN_POINT('Ctrl Pts',(-9.02287022789746,7.02713344197355,-0.141628082803403));
#66413=CARTESIAN_POINT('Ctrl Pts',(-8.98981893457298,6.95057605539729,1.04410508248903));
#66414=CARTESIAN_POINT('Ctrl Pts',(-8.9567676412485,6.59527188927863,2.13941658028022));
#66415=CARTESIAN_POINT('Ctrl Pts',(-8.92371634792402,6.23996772315997,3.23472807807139));
#66416=CARTESIAN_POINT('Ctrl Pts',(-8.89066505459954,5.60591677749891,4.2396179083613));
#66417=CARTESIAN_POINT('Ctrl Pts',(-8.85761376127506,4.77025282266349,5.03183888905018));
#66418=CARTESIAN_POINT('Ctrl Pts',(-8.82456246795059,3.93458886782808,5.82405986973906));
#66419=CARTESIAN_POINT('Ctrl Pts',(-8.79151117462611,2.89731190381832,6.4036120008269));
#66420=CARTESIAN_POINT('Ctrl Pts',(-8.75845988130163,1.78460908278264,6.69999141933305));
#66421=CARTESIAN_POINT('Ctrl Pts',(-8.72540858797715,0.671906261746978,
6.99637083783919));
#66422=CARTESIAN_POINT('Ctrl Pts',(-8.69235729465267,-0.516222416314614,
7.00957754376366));
#66423=CARTESIAN_POINT('Ctrl Pts',(-8.65930600132819,-1.63523833782786,
6.73800491065306));
#66424=CARTESIAN_POINT('Ctrl Pts',(-8.62625470800371,-2.75425425934114,
6.46643227754245));
#66425=CARTESIAN_POINT('Ctrl Pts',(-8.59320341467923,-3.80415742430608,
5.91008030539675));
#66426=CARTESIAN_POINT('Ctrl Pts',(-8.56015212135476,-4.65722467389882,
5.13663050396997));
#66427=CARTESIAN_POINT('Ctrl Pts',(-8.52710082803028,-5.51029192349154,
4.36318070254321));
#66428=CARTESIAN_POINT('Ctrl Pts',(-8.4940495347058,-6.16652325771206,3.37263307183539));
#66429=CARTESIAN_POINT('Ctrl Pts',(-8.46099824138132,-6.54608661040156,
2.28549003205181));
#66430=CARTESIAN_POINT('Ctrl Pts',(-8.43872271545631,-6.80190030035354,
1.55279002152113));
#66431=CARTESIAN_POINT('Ctrl Pts',(-8.41644718953129,-6.93204216650887,
0.776213154833276));
#66432=CARTESIAN_POINT('Ctrl Pts',(-8.39417166360628,-6.93268012709199,
-0.00015517830160834));
#66433=CARTESIAN_POINT('Origin',(-3.775,0.,0.));
#66434=CARTESIAN_POINT('',(-6.96482833639374,-6.93294662844253,0.000179318065722245));
#66435=CARTESIAN_POINT('',(-7.14417166360628,-6.93282359318651,0.000173910073648998));
#66436=CARTESIAN_POINT('',(-3.775,-6.933,-8.4904762584886E-16));
#66437=CARTESIAN_POINT('Ctrl Pts',(-6.96482833639374,-6.93294662844253,
0.000179318065722245));
#66438=CARTESIAN_POINT('Ctrl Pts',(-6.97293831643587,-6.93323237473856,
0.282805046459917));
#66439=CARTESIAN_POINT('Ctrl Pts',(-6.981048296478,-6.91627613789149,0.565396712104997));
#66440=CARTESIAN_POINT('Ctrl Pts',(-6.98915827652014,-6.88180763536459,
0.845835963022602));
#66441=CARTESIAN_POINT('Ctrl Pts',(-7.02220956984461,-6.74133520737417,
1.98873395951844));
#66442=CARTESIAN_POINT('Ctrl Pts',(-7.05526086316909,-6.31000567023157,
3.09588300514889));
#66443=CARTESIAN_POINT('Ctrl Pts',(-7.08831215649357,-5.64029126405976,
4.03259584673145));
#66444=CARTESIAN_POINT('Ctrl Pts',(-7.12136344981805,-4.97057685788794,
4.96930868831402));
#66445=CARTESIAN_POINT('Ctrl Pts',(-7.15441474314253,-4.06247758268689,
5.73558532584869));
#66446=CARTESIAN_POINT('Ctrl Pts',(-7.18746603646701,-3.02646582469637,
6.23820642640571));
#66447=CARTESIAN_POINT('Ctrl Pts',(-7.22051732979149,-1.99045406670588,
6.74082752696272));
#66448=CARTESIAN_POINT('Ctrl Pts',(-7.25356862311596,-0.826529825925916,
6.97979309054209));
#66449=CARTESIAN_POINT('Ctrl Pts',(-7.28661991644044,0.323712810088738,
6.92603240124453));
#66450=CARTESIAN_POINT('Ctrl Pts',(-7.31967120976492,1.47395544610341,6.87227171194696));
#66451=CARTESIAN_POINT('Ctrl Pts',(-7.3527225030894,2.61051647735277,6.52578476977245));
#66452=CARTESIAN_POINT('Ctrl Pts',(-7.38577379641388,3.59513061428307,5.92872251608635));
#66453=CARTESIAN_POINT('Ctrl Pts',(-7.41882508973836,4.57974475121336,5.33166026240026));
#66454=CARTESIAN_POINT('Ctrl Pts',(-7.45187638306283,5.4124119938246,4.48402269720259));
#66455=CARTESIAN_POINT('Ctrl Pts',(-7.48492767638731,5.99183643786163,3.48892689926549));
#66456=CARTESIAN_POINT('Ctrl Pts',(-7.51797896971179,6.57126088189867,2.49383110132837));
#66457=CARTESIAN_POINT('Ctrl Pts',(-7.55103026303627,6.89744252736151,1.3512770706518));
#66458=CARTESIAN_POINT('Ctrl Pts',(-7.58408155636075,6.93070061939663,0.200259159090933));
#66459=CARTESIAN_POINT('Ctrl Pts',(-7.61713284968523,6.96395871143175,-0.950758752469911));
#66460=CARTESIAN_POINT('Ctrl Pts',(-7.6501841430097,6.70429325003918,-2.11024054491504));
#66461=CARTESIAN_POINT('Ctrl Pts',(-7.68323543633418,6.18329314177072,-3.13713256484896));
#66462=CARTESIAN_POINT('Ctrl Pts',(-7.71628672965866,5.66229303350226,-4.16402458478286));
#66463=CARTESIAN_POINT('Ctrl Pts',(-7.74933802298314,4.8799582783579,-5.05832683220554));
#66464=CARTESIAN_POINT('Ctrl Pts',(-7.78238931630762,3.9314617165758,-5.7112453613554));
#66465=CARTESIAN_POINT('Ctrl Pts',(-7.81544060963211,2.98296515479368,-6.36416389050527));
#66466=CARTESIAN_POINT('Ctrl Pts',(-7.84849190295658,1.8683067863738,-6.77569870138231));
#66467=CARTESIAN_POINT('Ctrl Pts',(-7.88154319628106,0.723087391059321,
-6.89578562829469));
#66468=CARTESIAN_POINT('Ctrl Pts',(-7.91459448960554,-0.422132004255161,
-7.01587255520707));
#66469=CARTESIAN_POINT('Ctrl Pts',(-7.94764578293001,-1.59791242646425,
-6.84451159815479));
#66470=CARTESIAN_POINT('Ctrl Pts',(-7.98069707625449,-2.66121745600175,
-6.40254921561531));
#66471=CARTESIAN_POINT('Ctrl Pts',(-8.01374836957897,-3.72452248553925,
-5.96058683307582));
#66472=CARTESIAN_POINT('Ctrl Pts',(-8.04679966290345,-4.67535212240517,
-5.24802302504913));
#66473=CARTESIAN_POINT('Ctrl Pts',(-8.07985095622793,-5.39803573260544,
-4.35154283398653));
#66474=CARTESIAN_POINT('Ctrl Pts',(-8.11290224955241,-6.1207193428057,-3.45506264292393));
#66475=CARTESIAN_POINT('Ctrl Pts',(-8.14595354287689,-6.61525692634032,
-2.37466606882542));
#66476=CARTESIAN_POINT('Ctrl Pts',(-8.17900483620136,-6.82148683741763,
-1.24178586456869));
#66477=CARTESIAN_POINT('Ctrl Pts',(-8.19094600293215,-6.89599604735606,
-0.832485348784596));
#66478=CARTESIAN_POINT('Ctrl Pts',(-8.20288716966294,-6.93287191351981,
-0.416334045855466));
#66479=CARTESIAN_POINT('Ctrl Pts',(-8.21482833639373,-6.93258532737551,
-0.000132552009395881));
#66480=CARTESIAN_POINT('Ctrl Pts',(-8.39417166360628,-6.93268012709199,
-0.00015517830160834));
#66481=CARTESIAN_POINT('Ctrl Pts',(-8.38339589620681,-6.93298874000092,
-0.37572272280464));
#66482=CARTESIAN_POINT('Ctrl Pts',(-8.37262012880735,-6.90299172060379,
-0.751241467689222));
#66483=CARTESIAN_POINT('Ctrl Pts',(-8.36184436140789,-6.8422552629613,-1.12172078253239));
#66484=CARTESIAN_POINT('Ctrl Pts',(-8.32879306808341,-6.65596519167306,
-2.25805010847369));
#66485=CARTESIAN_POINT('Ctrl Pts',(-8.29574177475893,-6.1804896779381,-3.34697031149697));
#66486=CARTESIAN_POINT('Ctrl Pts',(-8.26269048143445,-5.47367142247792,
-4.25601171946639));
#66487=CARTESIAN_POINT('Ctrl Pts',(-8.22963918810997,-4.76685316701774,
-5.16505312743582));
#66488=CARTESIAN_POINT('Ctrl Pts',(-8.19658789478549,-3.82869216983234,
-5.89421574035139));
#66489=CARTESIAN_POINT('Ctrl Pts',(-8.16353660146101,-2.77331789547083,
-6.35479523258995));
#66490=CARTESIAN_POINT('Ctrl Pts',(-8.13048530813654,-1.71794362110932,
-6.81537472482851));
#66491=CARTESIAN_POINT('Ctrl Pts',(-8.09743401481205,-0.545356069571706,
-7.00737109639006));
#66492=CARTESIAN_POINT('Ctrl Pts',(-8.06438272148757,0.601796759709674,
-6.90742754268835));
#66493=CARTESIAN_POINT('Ctrl Pts',(-8.03133142816309,1.74894958899105,-6.80748398898665));
#66494=CARTESIAN_POINT('Ctrl Pts',(-7.99828013483862,2.87066769601621,-6.41560051002169));
#66495=CARTESIAN_POINT('Ctrl Pts',(-7.96522884151414,3.83049146744168,-5.7794506413104));
#66496=CARTESIAN_POINT('Ctrl Pts',(-7.93217754818967,4.79031523886716,-5.14330077259911));
#66497=CARTESIAN_POINT('Ctrl Pts',(-7.89912625486518,5.58824467469295,-4.26288451414151));
#66498=CARTESIAN_POINT('Ctrl Pts',(-7.8660749615407,6.12720980555135,-3.24530654888596));
#66499=CARTESIAN_POINT('Ctrl Pts',(-7.83302366821622,6.66617493640975,-2.22772858363043));
#66500=CARTESIAN_POINT('Ctrl Pts',(-7.79997237489175,6.94617576230075,-1.07298891157697));
#66501=CARTESIAN_POINT('Ctrl Pts',(-7.76692108156727,6.93314953234458,0.0784357038399208));
#66502=CARTESIAN_POINT('Ctrl Pts',(-7.73386978824279,6.92012330238841,1.22986031925681));
#66503=CARTESIAN_POINT('Ctrl Pts',(-7.7008184949183,6.61407001658507,2.37796987803714));
#66504=CARTESIAN_POINT('Ctrl Pts',(-7.66776720159383,6.05222176807958,3.38309418542708));
#66505=CARTESIAN_POINT('Ctrl Pts',(-7.63471590826935,5.49037351957408,4.38821849281703));
#66506=CARTESIAN_POINT('Ctrl Pts',(-7.60166461494488,4.67273030836643,5.25035754881659));
#66507=CARTESIAN_POINT('Ctrl Pts',(-7.5686133216204,3.69876033039241,5.86463013461226));
#66508=CARTESIAN_POINT('Ctrl Pts',(-7.53556202829592,2.72479035241839,6.47890272040792));
#66509=CARTESIAN_POINT('Ctrl Pts',(-7.50251073497143,1.594493607678,6.8453088359997));
#66510=CARTESIAN_POINT('Ctrl Pts',(-7.46945944164695,0.445373320719949,
6.91927432630602));
#66511=CARTESIAN_POINT('Ctrl Pts',(-7.43640814832247,-0.703746966238116,
6.99323981661234));
#66512=CARTESIAN_POINT('Ctrl Pts',(-7.403356854998,-1.87169079541385,6.77476468163321));
#66513=CARTESIAN_POINT('Ctrl Pts',(-7.37030556167353,-2.91637508698706,
6.29042692903177));
#66514=CARTESIAN_POINT('Ctrl Pts',(-7.33725426834905,-3.96105937856024,
5.80608917643034));
#66515=CARTESIAN_POINT('Ctrl Pts',(-7.30420297502456,-4.8824841325309,5.05588880620663));
#66516=CARTESIAN_POINT('Ctrl Pts',(-7.27115168170009,-5.56855588721342,
4.13108943602865));
#66517=CARTESIAN_POINT('Ctrl Pts',(-7.23810038837561,-6.25462764189595,
3.20629006585067));
#66518=CARTESIAN_POINT('Ctrl Pts',(-7.20504909505113,-6.70534639729033,
2.1068916957184));
#66519=CARTESIAN_POINT('Ctrl Pts',(-7.17199780172665,-6.86588116983432,
0.966638691136082));
#66520=CARTESIAN_POINT('Ctrl Pts',(-7.1627224223532,-6.91093298984508,0.646642765548731));
#66521=CARTESIAN_POINT('Ctrl Pts',(-7.15344704297974,-6.9331309329507,0.323429271653318));
#66522=CARTESIAN_POINT('Ctrl Pts',(-7.14417166360628,-6.93282359318651,
0.000173910073648998));
#66523=CARTESIAN_POINT('Origin',(-3.775,0.,0.));
#66524=CARTESIAN_POINT('',(-5.71482833639373,-6.9332949284688,-0.000149415166278977));
#66525=CARTESIAN_POINT('',(-5.89417166360628,-6.93340591766582,-0.000122946964495745));
#66526=CARTESIAN_POINT('',(-3.775,-6.933,-8.4904762584886E-16));
#66527=CARTESIAN_POINT('Ctrl Pts',(-5.71482833639373,-6.9332949284688,-0.000149415166278977));
#66528=CARTESIAN_POINT('Ctrl Pts',(-5.74298946320879,-6.9323649764916,0.981099183034019));
#66529=CARTESIAN_POINT('Ctrl Pts',(-5.77115059002384,-6.72197882763447,
1.96273382210663));
#66530=CARTESIAN_POINT('Ctrl Pts',(-5.7993117168389,-6.31774422827313,2.85671536429974));
#66531=CARTESIAN_POINT('Ctrl Pts',(-5.83236301016338,-5.84331447966477,
3.90593638346357));
#66532=CARTESIAN_POINT('Ctrl Pts',(-5.86541430348786,-5.10186755766788,
4.83441936161318));
#66533=CARTESIAN_POINT('Ctrl Pts',(-5.89846559681234,-4.18360220264049,
5.52921218769603));
#66534=CARTESIAN_POINT('Ctrl Pts',(-5.93151689013682,-3.26533684761313,
6.22400501377885));
#66535=CARTESIAN_POINT('Ctrl Pts',(-5.96456818346129,-2.17025305955524,
6.68510768779497));
#66536=CARTESIAN_POINT('Ctrl Pts',(-5.99761947678577,-1.03157032503942,
6.85642599836115));
#66537=CARTESIAN_POINT('Ctrl Pts',(-6.03067077011025,0.10711240947641,7.02774430892733));
#66538=CARTESIAN_POINT('Ctrl Pts',(-6.06372206343474,1.28939409045018,6.90927825604357));
#66539=CARTESIAN_POINT('Ctrl Pts',(-6.09677335675921,2.37144740508529,6.51543951022638));
#66540=CARTESIAN_POINT('Ctrl Pts',(-6.12982465008369,3.45350071972041,6.12160076440917));
#66541=CARTESIAN_POINT('Ctrl Pts',(-6.16287594340816,4.43532566801688,5.45238932565852));
#66542=CARTESIAN_POINT('Ctrl Pts',(-6.19592723673264,5.1974809643465,4.58921632000066));
#66543=CARTESIAN_POINT('Ctrl Pts',(-6.22897853005712,5.95963626067613,3.7260433143428));
#66544=CARTESIAN_POINT('Ctrl Pts',(-6.2620298233816,6.50212190503891,2.66890874177771));
#66545=CARTESIAN_POINT('Ctrl Pts',(-6.29508111670608,6.75894325866555,1.54641547866158));
#66546=CARTESIAN_POINT('Ctrl Pts',(-6.32813241003056,7.01576461229219,0.423922215545444));
#66547=CARTESIAN_POINT('Ctrl Pts',(-6.36118370335504,6.98692167518268,-0.763929738121745));
#66548=CARTESIAN_POINT('Ctrl Pts',(-6.39423499667951,6.67592325763527,-1.87263543293112));
#66549=CARTESIAN_POINT('Ctrl Pts',(-6.42728629000399,6.36492484008786,-2.9813411277405));
#66550=CARTESIAN_POINT('Ctrl Pts',(-6.46033758332848,5.77177094210252,-4.01090056369207));
#66551=CARTESIAN_POINT('Ctrl Pts',(-6.49338887665296,4.96862011319837,-4.8360654438526));
#66552=CARTESIAN_POINT('Ctrl Pts',(-6.52644016997744,4.16546928429424,-5.66123032401311));
#66553=CARTESIAN_POINT('Ctrl Pts',(-6.55949146330191,3.1523215244713,-6.28200064838259));
#66554=CARTESIAN_POINT('Ctrl Pts',(-6.59254275662639,2.05242861213926,-6.62285826502249));
#66555=CARTESIAN_POINT('Ctrl Pts',(-6.62559404995086,0.95253569980721,-6.9637158816624));
#66556=CARTESIAN_POINT('Ctrl Pts',(-6.65864534327534,-0.234102365033948,
-7.02466079057273));
#66557=CARTESIAN_POINT('Ctrl Pts',(-6.69169663659982,-1.36312830537076,
-6.79827890201643));
#66558=CARTESIAN_POINT('Ctrl Pts',(-6.7247479299243,-2.49215424570755,-6.57189701346013));
#66559=CARTESIAN_POINT('Ctrl Pts',(-6.75779922324879,-3.56356806153999,
-6.05818832743721));
#66560=CARTESIAN_POINT('Ctrl Pts',(-6.79085051657326,-4.44702977339938,
-5.31964669888933));
#66561=CARTESIAN_POINT('Ctrl Pts',(-6.82390180989774,-5.33049148525877,
-4.58110507034144));
#66562=CARTESIAN_POINT('Ctrl Pts',(-6.85695310322222,-6.02600109314511,
-3.61773049926859));
#66563=CARTESIAN_POINT('Ctrl Pts',(-6.89000439654669,-6.44894823766917,
-2.54671974005156));
#66564=CARTESIAN_POINT('Ctrl Pts',(-6.91494570982904,-6.76811448420257,
-1.73850885970419));
#66565=CARTESIAN_POINT('Ctrl Pts',(-6.93988702311139,-6.93206784848853,
-0.869003688169781));
#66566=CARTESIAN_POINT('Ctrl Pts',(-6.96482833639374,-6.93294662844253,
0.000179318065722245));
#66567=CARTESIAN_POINT('Ctrl Pts',(-7.14417166360628,-6.93282359318651,
0.000173910073648998));
#66568=CARTESIAN_POINT('Ctrl Pts',(-7.12039574965526,-6.93203577810175,
-0.828438198571558));
#66569=CARTESIAN_POINT('Ctrl Pts',(-7.09661983570424,-6.78337269219751,
-1.65732540685377));
#66570=CARTESIAN_POINT('Ctrl Pts',(-7.07284392175322,-6.4927056665093,-2.43299973809386));
#66571=CARTESIAN_POINT('Ctrl Pts',(-7.03979262842874,-6.08864460094668,
-3.51127752370906));
#66572=CARTESIAN_POINT('Ctrl Pts',(-7.00674133510426,-5.41017168012784,
-4.48672545590704));
#66573=CARTESIAN_POINT('Ctrl Pts',(-6.97369004177978,-4.53982471088598,
-5.24067802788111));
#66574=CARTESIAN_POINT('Ctrl Pts',(-6.9406387484553,-3.66947774164411,-5.99463059985517));
#66575=CARTESIAN_POINT('Ctrl Pts',(-6.90758745513082,-2.60725672397922,
-6.52708781160532));
#66576=CARTESIAN_POINT('Ctrl Pts',(-6.87453616180634,-1.48238331210909,
-6.77327500648447));
#66577=CARTESIAN_POINT('Ctrl Pts',(-6.84148486848186,-0.357509900238965,
-7.01946220136363));
#66578=CARTESIAN_POINT('Ctrl Pts',(-6.80843357515739,0.830015905836396,
-6.97937937937179));
#66579=CARTESIAN_POINT('Ctrl Pts',(-6.77538228183291,1.93572883332028,-6.65790270891211));
#66580=CARTESIAN_POINT('Ctrl Pts',(-6.74233098850843,3.04144176080416,-6.33642603845244));
#66581=CARTESIAN_POINT('Ctrl Pts',(-6.70927969518395,4.06534180969655,-5.73355551952493));
#66582=CARTESIAN_POINT('Ctrl Pts',(-6.67622840185947,4.8828691606461,-4.92263175115689));
#66583=CARTESIAN_POINT('Ctrl Pts',(-6.64317710853499,5.70039651159566,-4.11170798278886));
#66584=CARTESIAN_POINT('Ctrl Pts',(-6.61012581521051,6.31155116460237,-3.09273096498031));
#66585=CARTESIAN_POINT('Ctrl Pts',(-6.57707452188604,6.64198473648509,-1.98966161891559));
#66586=CARTESIAN_POINT('Ctrl Pts',(-6.54402322856156,6.97241830836781,-0.886592272850891));
#66587=CARTESIAN_POINT('Ctrl Pts',(-6.51097193523707,7.02213079912654,0.300569401470009));
#66588=CARTESIAN_POINT('Ctrl Pts',(-6.4779206419126,6.785074568784,1.42740242872407));
#66589=CARTESIAN_POINT('Ctrl Pts',(-6.44486934858812,6.54801833844146,2.55423545597816));
#66590=CARTESIAN_POINT('Ctrl Pts',(-6.41181805526364,6.02419338699765,3.62073983616544));
#66591=CARTESIAN_POINT('Ctrl Pts',(-6.37876676193916,5.27732423658162,4.49717283406753));
#66592=CARTESIAN_POINT('Ctrl Pts',(-6.34571546861469,4.53045508616559,5.37360583196962));
#66593=CARTESIAN_POINT('Ctrl Pts',(-6.31266417529021,3.56054173677734,6.05996744758651));
#66594=CARTESIAN_POINT('Ctrl Pts',(-6.27961288196573,2.48557640036856,6.47276019603829));
#66595=CARTESIAN_POINT('Ctrl Pts',(-6.24656158864125,1.41061106395978,6.88555294449007));
#66596=CARTESIAN_POINT('Ctrl Pts',(-6.21351029531677,0.230593740530481,
7.02477682577673));
#66597=CARTESIAN_POINT('Ctrl Pts',(-6.18045900199229,-0.91092372147787,
6.87349493133847));
#66598=CARTESIAN_POINT('Ctrl Pts',(-6.14740770866781,-2.05244118348622,
6.72221303690022));
#66599=CARTESIAN_POINT('Ctrl Pts',(-6.11435641534333,-3.15545878407361,
6.28042536673705));
#66600=CARTESIAN_POINT('Ctrl Pts',(-6.08130512201885,-4.08579186994391,
5.60187641714693));
#66601=CARTESIAN_POINT('Ctrl Pts',(-6.04825382869438,-5.0161249558142,4.92332746755682));
#66602=CARTESIAN_POINT('Ctrl Pts',(-6.0152025353699,-5.7737735269674,4.00801723853978));
#66603=CARTESIAN_POINT('Ctrl Pts',(-5.98215124204542,-6.26656787479109,
2.96729534561747));
#66604=CARTESIAN_POINT('Ctrl Pts',(-5.95282471589904,-6.70382599308494,
2.04385923362447));
#66605=CARTESIAN_POINT('Ctrl Pts',(-5.92349818975266,-6.93256242451305,
1.02168559205232));
#66606=CARTESIAN_POINT('Ctrl Pts',(-5.89417166360628,-6.93340591766582,
-0.000122946964495745));
#66607=CARTESIAN_POINT('Origin',(-3.775,0.,0.));
#66608=CARTESIAN_POINT('',(-4.46482833639373,-6.93242469144749,4.3789760074131E-5));
#66609=CARTESIAN_POINT('',(-4.64417166360628,-6.93240876118694,6.45577665183761E-6));
#66610=CARTESIAN_POINT('',(-3.775,-6.933,-8.4904762584886E-16));
#66611=CARTESIAN_POINT('Ctrl Pts',(-4.46482833639373,-6.93242469144749,
4.3789760074131E-5));
#66612=CARTESIAN_POINT('Ctrl Pts',(-4.47998931665723,-6.9325413820039,0.528504817274455));
#66613=CARTESIAN_POINT('Ctrl Pts',(-4.49515029692073,-6.87288824602125,
1.05693991976439));
#66614=CARTESIAN_POINT('Ctrl Pts',(-4.51031127718423,-6.75317819609387,
1.57140034946762));
#66615=CARTESIAN_POINT('Ctrl Pts',(-4.54336257050871,-6.49220747353687,
2.69293617831474));
#66616=CARTESIAN_POINT('Ctrl Pts',(-4.57641386383319,-5.94581611852691,
3.74805734008833));
#66617=CARTESIAN_POINT('Ctrl Pts',(-4.60946515715767,-5.18047390860605,
4.60840589453192));
#66618=CARTESIAN_POINT('Ctrl Pts',(-4.64251645048215,-4.41513169868519,
5.46875444897552));
#66619=CARTESIAN_POINT('Ctrl Pts',(-4.67556774380662,-3.43083863385344,
6.13433039608913));
#66620=CARTESIAN_POINT('Ctrl Pts',(-4.7086190371311,-2.34733625184864,6.524164875849));
#66621=CARTESIAN_POINT('Ctrl Pts',(-4.74167033045558,-1.26383386984384,
6.91399935560887));
#66622=CARTESIAN_POINT('Ctrl Pts',(-4.77472162378006,-0.0811221706659873,
7.028092368015));
#66623=CARTESIAN_POINT('Ctrl Pts',(-4.80777291710454,1.05691922017489,6.85256423308308));
#66624=CARTESIAN_POINT('Ctrl Pts',(-4.84082421042902,2.19496061101574,6.67703609815116));
#66625=CARTESIAN_POINT('Ctrl Pts',(-4.87387550375349,3.28833169351963,6.2118868158812));
#66626=CARTESIAN_POINT('Ctrl Pts',(-4.90692679707797,4.20402133572304,5.51370287695031));
#66627=CARTESIAN_POINT('Ctrl Pts',(-4.93997809040245,5.11971097792649,4.81551893801939));
#66628=CARTESIAN_POINT('Ctrl Pts',(-4.97302938372693,5.85771917982946,3.88430034242751));
#66629=CARTESIAN_POINT('Ctrl Pts',(-5.00608067705141,6.32826552936115,2.83333199544354));
#66630=CARTESIAN_POINT('Ctrl Pts',(-5.03913197037589,6.79881187889281,1.78236364845962));
#66631=CARTESIAN_POINT('Ctrl Pts',(-5.07218326370037,7.00189637605322,0.611645550083625));
#66632=CARTESIAN_POINT('Ctrl Pts',(-5.10523455702485,6.91281332002058,-0.536401723571765));
#66633=CARTESIAN_POINT('Ctrl Pts',(-5.13828585034933,6.82373026398793,-1.68444899722717));
#66634=CARTESIAN_POINT('Ctrl Pts',(-5.17133714367381,6.44247965476221,-2.80982544616197));
#66635=CARTESIAN_POINT('Ctrl Pts',(-5.20438843699828,5.81544151455764,-3.77562641124148));
#66636=CARTESIAN_POINT('Ctrl Pts',(-5.23743973032276,5.18840337435306,-4.74142737632099));
#66637=CARTESIAN_POINT('Ctrl Pts',(-5.27049102364724,4.31557770316962,-5.54765285754521));
#66638=CARTESIAN_POINT('Ctrl Pts',(-5.30354231697172,3.30314577138174,-6.09622365235295));
#66639=CARTESIAN_POINT('Ctrl Pts',(-5.3365936102962,2.29071383959387,-6.64479444716068));
#66640=CARTESIAN_POINT('Ctrl Pts',(-5.36964490362068,1.13867564720158,-6.93571055555193));
#66641=CARTESIAN_POINT('Ctrl Pts',(-5.40269619694516,-0.0128206836366791,
-6.9335813571758));
#66642=CARTESIAN_POINT('Ctrl Pts',(-5.43574749026964,-1.16431701447495,
-6.93145215879967));
#66643=CARTESIAN_POINT('Ctrl Pts',(-5.46879878359411,-2.31527148375918,
-6.63627765365614));
#66644=CARTESIAN_POINT('Ctrl Pts',(-5.50185007691859,-3.32566780676435,
-6.08396650595282));
#66645=CARTESIAN_POINT('Ctrl Pts',(-5.53490137024307,-4.33606412976952,
-5.5316553582495));
#66646=CARTESIAN_POINT('Ctrl Pts',(-5.56795266356755,-5.20590230649563,
-4.72220756798638));
#66647=CARTESIAN_POINT('Ctrl Pts',(-5.60100395689203,-5.8293645022086,-3.75409433910429));
#66648=CARTESIAN_POINT('Ctrl Pts',(-5.63405525021651,-6.45282669792157,
-2.78598111022221));
#66649=CARTESIAN_POINT('Ctrl Pts',(-5.66710654354098,-6.8299129126214,-1.65920244272117));
#66650=CARTESIAN_POINT('Ctrl Pts',(-5.70015783686546,-6.91474973236137,
-0.510833578881621));
#66651=CARTESIAN_POINT('Ctrl Pts',(-5.70504800337488,-6.92730192421013,
-0.34092449534652));
#66652=CARTESIAN_POINT('Ctrl Pts',(-5.70993816988431,-6.933456414195,-0.17054277562555));
#66653=CARTESIAN_POINT('Ctrl Pts',(-5.71482833639373,-6.9332949284688,-0.000149415166278977));
#66654=CARTESIAN_POINT('Ctrl Pts',(-5.89417166360628,-6.93340591766582,
-0.000122946964495745));
#66655=CARTESIAN_POINT('Ctrl Pts',(-5.89044689642818,-6.93351304987762,
-0.129903026931444));
#66656=CARTESIAN_POINT('Ctrl Pts',(-5.88672212925008,-6.92994390796523,
-0.259677217215776));
#66657=CARTESIAN_POINT('Ctrl Pts',(-5.88299736207198,-6.92265880264989,
-0.389242468881223));
#66658=CARTESIAN_POINT('Ctrl Pts',(-5.8499460687475,-6.85801525819082,-1.53892483363012));
#66659=CARTESIAN_POINT('Ctrl Pts',(-5.81689477542302,-6.50078804477848,
-2.67215600630032));
#66660=CARTESIAN_POINT('Ctrl Pts',(-5.78384348209855,-5.89443468272273,
-3.65107578236909));
#66661=CARTESIAN_POINT('Ctrl Pts',(-5.75079218877407,-5.288081320667,-4.62999555843786));
#66662=CARTESIAN_POINT('Ctrl Pts',(-5.71774089544959,-4.43260180996788,
-5.45460393790521));
#66663=CARTESIAN_POINT('Ctrl Pts',(-5.68468960212511,-3.43206722028373,
-6.02458539593727));
#66664=CARTESIAN_POINT('Ctrl Pts',(-5.65163830880063,-2.43153263059957,
-6.59456685396934));
#66665=CARTESIAN_POINT('Ctrl Pts',(-5.61858701547615,-1.28594296193037,
-6.90992139056613));
#66666=CARTESIAN_POINT('Ctrl Pts',(-5.58553572215167,-0.134661858544509,
-6.93228539381783));
#66667=CARTESIAN_POINT('Ctrl Pts',(-5.55248442882719,1.01661924484135,-6.95464939706954));
#66668=CARTESIAN_POINT('Ctrl Pts',(-5.51943313550271,2.17359178294388,-6.68402286697617));
#66669=CARTESIAN_POINT('Ctrl Pts',(-5.48638184217824,3.19550735898701,-6.1533281495583));
#66670=CARTESIAN_POINT('Ctrl Pts',(-5.45333054885376,4.21742293503015,-5.62263343214043));
#66671=CARTESIAN_POINT('Ctrl Pts',(-5.42027925552928,5.10428154901389,-4.83187052739805));
#66672=CARTESIAN_POINT('Ctrl Pts',(-5.3872279622048,5.74819479047523,-3.87723757954555));
#66673=CARTESIAN_POINT('Ctrl Pts',(-5.35417666888032,6.39210803193656,-2.92260463169304));
#66674=CARTESIAN_POINT('Ctrl Pts',(-5.32112537555584,6.79307590087549,-1.80410164073041));
#66675=CARTESIAN_POINT('Ctrl Pts',(-5.28807408223136,6.90231972463275,-0.657797093663752));
#66676=CARTESIAN_POINT('Ctrl Pts',(-5.25502278890689,7.01156354839,0.488507453402909));
#66677=CARTESIAN_POINT('Ctrl Pts',(-5.22197149558241,6.82908332696558,1.6626135565736));
#66678=CARTESIAN_POINT('Ctrl Pts',(-5.18892020225793,6.3770782031766,2.7216884810824));
#66679=CARTESIAN_POINT('Ctrl Pts',(-5.15586890893345,5.92507307938763,3.7807634055912));
#66680=CARTESIAN_POINT('Ctrl Pts',(-5.12281761560897,5.2035430532341,4.72480715143811));
#66681=CARTESIAN_POINT('Ctrl Pts',(-5.08976632228449,4.30026392842995,5.43897460403438));
#66682=CARTESIAN_POINT('Ctrl Pts',(-5.05671502896001,3.3969848036258,6.15314205663066));
#66683=CARTESIAN_POINT('Ctrl Pts',(-5.02366373563553,2.31195658017102,6.6374332159763));
#66684=CARTESIAN_POINT('Ctrl Pts',(-4.99061244231105,1.1771754618463,6.83293293758352));
#66685=CARTESIAN_POINT('Ctrl Pts',(-4.95756114898658,0.0423943435215721,
7.02843265919073));
#66686=CARTESIAN_POINT('Ctrl Pts',(-4.9245098556621,-1.1421396696731,6.93514094305953));
#66687=CARTESIAN_POINT('Ctrl Pts',(-4.89145856233762,-2.23232526349452,
6.56440694316333));
#66688=CARTESIAN_POINT('Ctrl Pts',(-4.85840726901314,-3.32251085731596,
6.19367294326712));
#66689=CARTESIAN_POINT('Ctrl Pts',(-4.82535597568866,-4.31834803176415,
5.54549665960591));
#66690=CARTESIAN_POINT('Ctrl Pts',(-4.79230468236418,-5.09869088135075,
4.69873024272701));
#66691=CARTESIAN_POINT('Ctrl Pts',(-4.7592533890397,-5.87903373093732,3.85196382584815));
#66692=CARTESIAN_POINT('Ctrl Pts',(-4.72620209571523,-6.44388225566231,
2.80660727575161));
#66693=CARTESIAN_POINT('Ctrl Pts',(-4.69315080239075,-6.72452132041392,
1.68983064500126));
#66694=CARTESIAN_POINT('Ctrl Pts',(-4.67682442279593,-6.86314887290602,
1.13817540363875));
#66695=CARTESIAN_POINT('Ctrl Pts',(-4.6604980432011,-6.93242723552036,0.569093139492368));
#66696=CARTESIAN_POINT('Ctrl Pts',(-4.64417166360628,-6.93240876118694,
6.45577665183761E-6));
#66697=CARTESIAN_POINT('Origin',(-3.775,0.,0.));
#66698=CARTESIAN_POINT('',(-3.21482833639373,-6.93352350063866,7.67097482256771E-5));
#66699=CARTESIAN_POINT('',(-3.39417166360628,-6.93343988028234,0.000112224652378165));
#66700=CARTESIAN_POINT('',(-3.775,-6.933,-8.4904762584886E-16));
#66701=CARTESIAN_POINT('Ctrl Pts',(-3.21482833639373,-6.93352350063866,
7.67097482256771E-5));
#66702=CARTESIAN_POINT('Ctrl Pts',(-3.21698917010567,-6.93356599650761,
0.0753617861455037));
#66703=CARTESIAN_POINT('Ctrl Pts',(-3.21915000381762,-6.93236527092446,
0.150645504658142));
#66704=CARTESIAN_POINT('Ctrl Pts',(-3.22131083752956,-6.92991264230934,
0.225888415961884));
#66705=CARTESIAN_POINT('Ctrl Pts',(-3.25436213085404,-6.89239816476019,
1.37677546402265));
#66706=CARTESIAN_POINT('Ctrl Pts',(-3.28741342417851,-6.56199343734975,
2.51811541993279));
#66707=CARTESIAN_POINT('Ctrl Pts',(-3.320464717503,-5.97889296266017,3.51106162685268));
#66708=CARTESIAN_POINT('Ctrl Pts',(-3.35351601082748,-5.3957924879706,4.50400783377254));
#66709=CARTESIAN_POINT('Ctrl Pts',(-3.38656730415196,-4.55999626600192,
5.34856029170215));
#66710=CARTESIAN_POINT('Ctrl Pts',(-3.41961859747644,-3.57318084861636,
5.94197723233487));
#66711=CARTESIAN_POINT('Ctrl Pts',(-3.45266989080091,-2.5863654312308,6.53539417296759));
#66712=CARTESIAN_POINT('Ctrl Pts',(-3.48572118412539,-1.44853081842837,
6.87767559630342));
#66713=CARTESIAN_POINT('Ctrl Pts',(-3.51877247744987,-0.298097233917136,
6.92718217211267));
#66714=CARTESIAN_POINT('Ctrl Pts',(-3.55182377077435,0.852336350594116,
6.97668874792192));
#66715=CARTESIAN_POINT('Ctrl Pts',(-3.58487506409883,2.01536890681417,6.73342047620457));
#66716=CARTESIAN_POINT('Ctrl Pts',(-3.61792635742331,3.04951482268625,6.22697150729964));
#66717=CARTESIAN_POINT('Ctrl Pts',(-3.65097765074779,4.08366073855829,5.72052253839471));
#66718=CARTESIAN_POINT('Ctrl Pts',(-3.68402894407227,4.98892001408236,4.95089287230221));
#66719=CARTESIAN_POINT('Ctrl Pts',(-3.71708023739674,5.65516575557641,4.01170974566463));
#66720=CARTESIAN_POINT('Ctrl Pts',(-3.75013153072122,6.32141149707046,3.07252661902703));
#66721=CARTESIAN_POINT('Ctrl Pts',(-3.7831828240457,6.74864370453449,1.96379003184436));
#66722=CARTESIAN_POINT('Ctrl Pts',(-3.81623411737018,6.88488858751857,0.820380365416631));
#66723=CARTESIAN_POINT('Ctrl Pts',(-3.84928541069466,7.02113347050265,-0.32302930101107));
#66724=CARTESIAN_POINT('Ctrl Pts',(-3.88233670401913,6.86639102900679,-1.50111204668383));
#66725=CARTESIAN_POINT('Ctrl Pts',(-3.91538799734361,6.4394860404881,-2.57055136903808));
#66726=CARTESIAN_POINT('Ctrl Pts',(-3.94843929066809,6.01258105196939,-3.63999069139237));
#66727=CARTESIAN_POINT('Ctrl Pts',(-3.98149058399257,5.31351351642781,-4.60078659042814));
#66728=CARTESIAN_POINT('Ctrl Pts',(-4.01454187731705,4.42732662341655,-5.33605601320785));
#66729=CARTESIAN_POINT('Ctrl Pts',(-4.04759317064153,3.54113973040531,-6.07132543598754));
#66730=CARTESIAN_POINT('Ctrl Pts',(-4.080644463966,2.4678334799244,-6.58106838251119));
#66731=CARTESIAN_POINT('Ctrl Pts',(-4.11369575729048,1.3379780705134,-6.80327343925921));
#66732=CARTESIAN_POINT('Ctrl Pts',(-4.14674705061496,0.208122661102384,
-7.02547849600723));
#66733=CARTESIAN_POINT('Ctrl Pts',(-4.17979834393945,-0.978281907238725,
-6.9601456629796));
#66734=CARTESIAN_POINT('Ctrl Pts',(-4.21284963726393,-2.07690676288808,
-6.61522283107489));
#66735=CARTESIAN_POINT('Ctrl Pts',(-4.2459009305884,-3.17553161853743,-6.27029999917018));
#66736=CARTESIAN_POINT('Ctrl Pts',(-4.27895222391288,-4.18637676149503,
-5.64578716838837));
#66737=CARTESIAN_POINT('Ctrl Pts',(-4.31200351723736,-4.98647053204155,
-4.81765777526651));
#66738=CARTESIAN_POINT('Ctrl Pts',(-4.34505481056184,-5.78656430258806,
-3.98952838214466));
#66739=CARTESIAN_POINT('Ctrl Pts',(-4.37810610388631,-6.37590670072351,
-2.95778242668277));
#66740=CARTESIAN_POINT('Ctrl Pts',(-4.41115739721079,-6.68280285473921,
-1.8479342009915));
#66741=CARTESIAN_POINT('Ctrl Pts',(-4.42904771027177,-6.84892247428479,
-1.24718517695605));
#66742=CARTESIAN_POINT('Ctrl Pts',(-4.44693802333275,-6.93228699384818,
-0.623552643876927));
#66743=CARTESIAN_POINT('Ctrl Pts',(-4.46482833639373,-6.93242469144749,
4.3789760074131E-5));
#66744=CARTESIAN_POINT('Ctrl Pts',(-4.64417166360628,-6.93240876118694,
6.45577665183761E-6));
#66745=CARTESIAN_POINT('Ctrl Pts',(-4.62744674987662,-6.93238983588688,
-0.5829718851691));
#66746=CARTESIAN_POINT('Ctrl Pts',(-4.61072183614696,-6.85964964898072,
-1.16595486408495));
#66747=CARTESIAN_POINT('Ctrl Pts',(-4.59399692241731,-6.71424448162094,
-1.73021259922285));
#66748=CARTESIAN_POINT('Ctrl Pts',(-4.56094562909283,-6.42689897329813,
-2.84528250129246));
#66749=CARTESIAN_POINT('Ctrl Pts',(-4.52789433576836,-5.85577835187427,
-3.88722559402747));
#66750=CARTESIAN_POINT('Ctrl Pts',(-4.49484304244388,-5.07036076759396,
-4.72928707988114));
#66751=CARTESIAN_POINT('Ctrl Pts',(-4.4617917491194,-4.28494318331366,-5.5713485657348));
#66752=CARTESIAN_POINT('Ctrl Pts',(-4.42874045579492,-3.28522863617693,
-6.21352844470713));
#66753=CARTESIAN_POINT('Ctrl Pts',(-4.39568916247044,-2.19283472306634,
-6.57770404281017));
#66754=CARTESIAN_POINT('Ctrl Pts',(-4.36263786914596,-1.10044080995574,
-6.94187964091322));
#66755=CARTESIAN_POINT('Ctrl Pts',(-4.32958657582149,0.0846324691287112,
-7.02805095814698));
#66756=CARTESIAN_POINT('Ctrl Pts',(-4.29653528249701,1.21821819699567,-6.82573505360377));
#66757=CARTESIAN_POINT('Ctrl Pts',(-4.26348398917253,2.35180392486264,-6.62341914906057));
#66758=CARTESIAN_POINT('Ctrl Pts',(-4.23043269584805,3.43390210151211,-6.1326160227404));
#66759=CARTESIAN_POINT('Ctrl Pts',(-4.19738140252357,4.33287297016345,-5.41303301504006));
#66760=CARTESIAN_POINT('Ctrl Pts',(-4.16433010919909,5.23184383881479,-4.69345000733972));
#66761=CARTESIAN_POINT('Ctrl Pts',(-4.13127881587461,5.947687399468,-3.74508711825922));
#66762=CARTESIAN_POINT('Ctrl Pts',(-4.09822752255013,6.39331962014627,-2.68331489619455));
#66763=CARTESIAN_POINT('Ctrl Pts',(-4.06517622922565,6.83895184082454,-1.62154267412987));
#66764=CARTESIAN_POINT('Ctrl Pts',(-4.03212493590118,7.01437272152787,-0.446361119081015));
#66765=CARTESIAN_POINT('Ctrl Pts',(-3.9990736425767,6.89824190463591,0.69926620296696));
#66766=CARTESIAN_POINT('Ctrl Pts',(-3.96602234925222,6.78211108774396,1.84489352501493));
#66767=CARTESIAN_POINT('Ctrl Pts',(-3.93297105592774,6.37442857325671,2.96096661406203));
#66768=CARTESIAN_POINT('Ctrl Pts',(-3.89991976260326,5.72478988606175,3.91171258631457));
#66769=CARTESIAN_POINT('Ctrl Pts',(-3.86686846927878,5.0751511988668,4.8624585585671));
#66770=CARTESIAN_POINT('Ctrl Pts',(-3.8338171759543,4.18355633896413,5.64787741402508));
#66771=CARTESIAN_POINT('Ctrl Pts',(-3.80076588262982,3.15846989213457,6.17242112448318));
#66772=CARTESIAN_POINT('Ctrl Pts',(-3.76771458930535,2.133383445305,6.69696483494128));
#66773=CARTESIAN_POINT('Ctrl Pts',(-3.73466329598087,0.974805411548551,
6.96063340039951));
#66774=CARTESIAN_POINT('Ctrl Pts',(-3.70161200265639,-0.17632050008306,
6.93135092739772));
#66775=CARTESIAN_POINT('Ctrl Pts',(-3.66856070933191,-1.32744641171467,
6.90206845439593));
#66776=CARTESIAN_POINT('Ctrl Pts',(-3.63550941600743,-2.4711202012214,6.57983494293414));
#66777=CARTESIAN_POINT('Ctrl Pts',(-3.60245812268295,-3.46821129548542,
6.00385084819352));
#66778=CARTESIAN_POINT('Ctrl Pts',(-3.56940682935847,-4.46530238974945,
5.42786675345291));
#66779=CARTESIAN_POINT('Ctrl Pts',(-3.53635553603399,-5.31581078877077,
4.59813207543344));
#66780=CARTESIAN_POINT('Ctrl Pts',(-3.50330424270951,-5.91627017017391,
3.61558596509572));
#66781=CARTESIAN_POINT('Ctrl Pts',(-3.47025294938503,-6.51672955157704,
2.633039854758));
#66782=CARTESIAN_POINT('Ctrl Pts',(-3.43720165606056,-6.86713991536202,
1.49768231210201));
#66783=CARTESIAN_POINT('Ctrl Pts',(-3.40415036273608,-6.92487302681091,
0.347632219498546));
#66784=CARTESIAN_POINT('Ctrl Pts',(-3.40082412969281,-6.93068320135103,
0.231892887246826));
#66785=CARTESIAN_POINT('Ctrl Pts',(-3.39749789664954,-6.9335291083434,0.116004747225949));
#66786=CARTESIAN_POINT('Ctrl Pts',(-3.39417166360628,-6.93343988028234,
0.000112224652378165));
#66787=CARTESIAN_POINT('Origin',(-3.775,0.,0.));
#66788=CARTESIAN_POINT('',(-1.96482833639373,-6.93267455605571,-0.000154115015024714));
#66789=CARTESIAN_POINT('',(-2.14417166360627,-6.93278353301175,-0.000170174852231984));
#66790=CARTESIAN_POINT('',(-3.775,-6.933,-8.4904762584886E-16));
#66791=CARTESIAN_POINT('Ctrl Pts',(-1.96482833639373,-6.93267455605571,
-0.000154115015024714));
#66792=CARTESIAN_POINT('Ctrl Pts',(-1.9870403168786,-6.93204351043128,0.774001260964231));
#66793=CARTESIAN_POINT('Ctrl Pts',(-2.00925229736346,-6.80265738467977,
1.5483623151292));
#66794=CARTESIAN_POINT('Ctrl Pts',(-2.03146427784833,-6.54827367295132,
2.27921624920437));
#66795=CARTESIAN_POINT('Ctrl Pts',(-2.06451557117281,-6.1697522403832,3.36672250597088));
#66796=CARTESIAN_POINT('Ctrl Pts',(-2.09756686449728,-5.51447039087689,
4.35789851282317));
#66797=CARTESIAN_POINT('Ctrl Pts',(-2.13061815782176,-4.66214468357019,
5.13216540613831));
#66798=CARTESIAN_POINT('Ctrl Pts',(-2.16366945114624,-3.8098189762635,5.90643229945344));
#66799=CARTESIAN_POINT('Ctrl Pts',(-2.19672074447072,-2.76044941115642,
6.46379007923142));
#66800=CARTESIAN_POINT('Ctrl Pts',(-2.2297720377952,-1.64169423341061,6.73643487688339));
#66801=CARTESIAN_POINT('Ctrl Pts',(-2.26282333111968,-0.522939055664844,
7.00907967453536));
#66802=CARTESIAN_POINT('Ctrl Pts',(-2.29587462444416,0.665201734719648,
6.99701149006133));
#66803=CARTESIAN_POINT('Ctrl Pts',(-2.32892591776863,1.77818805067639,6.7016984461356));
#66804=CARTESIAN_POINT('Ctrl Pts',(-2.36197721109311,2.89117436663317,6.40638540220986));
#66805=CARTESIAN_POINT('Ctrl Pts',(-2.39502850441759,3.92900620816221,5.8278274988324));
#66806=CARTESIAN_POINT('Ctrl Pts',(-2.42807979774207,4.76542892097592,5.03640764887344));
#66807=CARTESIAN_POINT('Ctrl Pts',(-2.46113109106655,5.60185163378963,4.24498779891447));
#66808=CARTESIAN_POINT('Ctrl Pts',(-2.49418238439103,6.23686521788803,3.24070600237399));
#66809=CARTESIAN_POINT('Ctrl Pts',(-2.52723367771551,6.59321879570106,2.14573547263377));
#66810=CARTESIAN_POINT('Ctrl Pts',(-2.56028497103999,6.9495723735141,1.05076494289354));
#66811=CARTESIAN_POINT('Ctrl Pts',(-2.59333626436446,7.02726594504176,-0.134894320046401));
#66812=CARTESIAN_POINT('Ctrl Pts',(-2.62638755768894,6.81684790683436,-1.26700411269759));
#66813=CARTESIAN_POINT('Ctrl Pts',(-2.65943885101342,6.60642986862698,-2.39911390534872));
#66814=CARTESIAN_POINT('Ctrl Pts',(-2.6924901443379,6.1079002206845,-3.47767422771116));
#66815=CARTESIAN_POINT('Ctrl Pts',(-2.72554143766238,5.38190625270701,-4.37147571119614));
#66816=CARTESIAN_POINT('Ctrl Pts',(-2.75859273098686,4.65591228472947,-5.26527719468117));
#66817=CARTESIAN_POINT('Ctrl Pts',(-2.79164402431133,3.70245399671694,-5.97431983928876));
#66818=CARTESIAN_POINT('Ctrl Pts',(-2.82469531763581,2.63752180418136,-6.41234696027691));
#66819=CARTESIAN_POINT('Ctrl Pts',(-2.85774661096029,1.57258961164582,-6.85037408126505));
#66820=CARTESIAN_POINT('Ctrl Pts',(-2.89079790428477,0.396183514587305,
-7.01738567863371));
#66821=CARTESIAN_POINT('Ctrl Pts',(-2.92384919760925,-0.74858395262916,
-6.89306440361402));
#66822=CARTESIAN_POINT('Ctrl Pts',(-2.95690049093373,-1.89335141984563,
-6.76874312859432));
#66823=CARTESIAN_POINT('Ctrl Pts',(-2.98995178425821,-3.00648025722006,
-6.35308898118627));
#66824=CARTESIAN_POINT('Ctrl Pts',(-3.02300307758269,-3.9525557560139,-5.69666725393945));
#66825=CARTESIAN_POINT('Ctrl Pts',(-3.05605437090717,-4.89863125480775,
-5.04024552669263));
#66826=CARTESIAN_POINT('Ctrl Pts',(-3.08910566423165,-5.67765341502102,
-4.14305621960703));
#66827=CARTESIAN_POINT('Ctrl Pts',(-3.12215695755613,-6.1948523812837,-3.11424449595857));
#66828=CARTESIAN_POINT('Ctrl Pts',(-3.15304741716866,-6.67823781561858,
-2.15269461994424));
#66829=CARTESIAN_POINT('Ctrl Pts',(-3.1839378767812,-6.93291599580554,-1.07617020320189));
#66830=CARTESIAN_POINT('Ctrl Pts',(-3.21482833639373,-6.93352350063866,
7.67097482256771E-5));
#66831=CARTESIAN_POINT('Ctrl Pts',(-3.39417166360628,-6.93343988028234,
0.000112224652378165));
#66832=CARTESIAN_POINT('Ctrl Pts',(-3.36444660332506,-6.93264248892117,
-1.03556752924019));
#66833=CARTESIAN_POINT('Ctrl Pts',(-3.33472154304385,-6.69743936418148,
-2.07159728252277));
#66834=CARTESIAN_POINT('Ctrl Pts',(-3.30499648276264,-6.24862210463677,
-3.004902060123));
#66835=CARTESIAN_POINT('Ctrl Pts',(-3.27194518943816,-5.74958221190098,
-4.04264360459012));
#66836=CARTESIAN_POINT('Ctrl Pts',(-3.23889389611369,-4.98644656731659,
-4.95338405097345));
#66837=CARTESIAN_POINT('Ctrl Pts',(-3.20584260278921,-4.05205239472479,
-5.62632970842377));
#66838=CARTESIAN_POINT('Ctrl Pts',(-3.17279130946473,-3.11765822213298,
-6.29927536587409));
#66839=CARTESIAN_POINT('Ctrl Pts',(-3.13974001614025,-2.01200552153376,
-6.7344262343914));
#66840=CARTESIAN_POINT('Ctrl Pts',(-3.10668872281577,-0.869599512260727,
-6.87884520001451));
#66841=CARTESIAN_POINT('Ctrl Pts',(-3.07363742949129,0.272806497012319,
-7.02326416563761));
#66842=CARTESIAN_POINT('Ctrl Pts',(-3.04058613616681,1.45196581495916,-6.8769512283665));
#66843=CARTESIAN_POINT('Ctrl Pts',(-3.00753484284234,2.52443097149833,-6.45770569688855));
#66844=CARTESIAN_POINT('Ctrl Pts',(-2.97448354951786,3.59689612803748,-6.03846016541059));
#66845=CARTESIAN_POINT('Ctrl Pts',(-2.94143225619338,4.56266712316898,-5.34628203972578));
#66846=CARTESIAN_POINT('Ctrl Pts',(-2.9083809628689,5.30425567195863,-4.46537639667492));
#66847=CARTESIAN_POINT('Ctrl Pts',(-2.87532966954442,6.04584422074829,-3.58447075362404));
#66848=CARTESIAN_POINT('Ctrl Pts',(-2.84227837621994,6.56325032319611,-2.51483759320713));
#66849=CARTESIAN_POINT('Ctrl Pts',(-2.80922708289546,6.79353032506368,-1.38660027402525));
#66850=CARTESIAN_POINT('Ctrl Pts',(-2.77617578957098,7.02381032693125,-0.258362954843403));
#66851=CARTESIAN_POINT('Ctrl Pts',(-2.7431244962465,6.96696422821857,0.928478523103413));
#66852=CARTESIAN_POINT('Ctrl Pts',(-2.71007320292203,6.62990748888108,2.02954213712485));
#66853=CARTESIAN_POINT('Ctrl Pts',(-2.67702190959755,6.29285074954358,3.13060575114631));
#66854=CARTESIAN_POINT('Ctrl Pts',(-2.64397061627307,5.67558336958127,4.14589150124242));
#66855=CARTESIAN_POINT('Ctrl Pts',(-2.61091932294859,4.8531973596086,4.95188751752045));
#66856=CARTESIAN_POINT('Ctrl Pts',(-2.57786802962411,4.03081134963592,5.7578835337985));
#66857=CARTESIAN_POINT('Ctrl Pts',(-2.54481673629963,3.00330670965288,6.35458981625845));
#66858=CARTESIAN_POINT('Ctrl Pts',(-2.51176544297515,1.89568176589007,6.66941565955809));
#66859=CARTESIAN_POINT('Ctrl Pts',(-2.47871414965067,0.788056822127327,
6.9842415028577));
#66860=CARTESIAN_POINT('Ctrl Pts',(-2.4456628563262,-0.399688425415167,
7.01718690699704));
#66861=CARTESIAN_POINT('Ctrl Pts',(-2.41261156300172,-1.52306200837649,
6.7642439870341));
#66862=CARTESIAN_POINT('Ctrl Pts',(-2.37956026967724,-2.64643559133784,
6.51130106707115));
#66863=CARTESIAN_POINT('Ctrl Pts',(-2.34650897635276,-3.70543750971801,
5.97246982300591));
#66864=CARTESIAN_POINT('Ctrl Pts',(-2.31345768302828,-4.57123772020481,
5.21330032732275));
#66865=CARTESIAN_POINT('Ctrl Pts',(-2.2804063897038,-5.4370379306916,4.45413083163958));
#66866=CARTESIAN_POINT('Ctrl Pts',(-2.24735509637932,-6.10963643328502,
3.47462308433849));
#66867=CARTESIAN_POINT('Ctrl Pts',(-2.21430380305484,-6.50721005777458,
2.39393647816395));
#66868=CARTESIAN_POINT('Ctrl Pts',(-2.19092642323865,-6.78841628874856,
1.62956030060298));
#66869=CARTESIAN_POINT('Ctrl Pts',(-2.16754904342246,-6.93203256432842,
0.814566176130428));
#66870=CARTESIAN_POINT('Ctrl Pts',(-2.14417166360627,-6.93278353301175,
-0.000170174852231984));
#66871=CARTESIAN_POINT('Origin',(-3.775,0.,0.));
#66872=CARTESIAN_POINT('',(-0.714828336393731,-6.93283010606057,0.00017441890636849));
#66873=CARTESIAN_POINT('',(-0.894171663606273,-6.9327161513647,0.000161366341133071));
#66874=CARTESIAN_POINT('',(-3.775,-6.933,-8.4904762584886E-16));
#66875=CARTESIAN_POINT('Ctrl Pts',(-0.714828336393731,-6.93283010606057,
0.00017441890636849));
#66876=CARTESIAN_POINT('Ctrl Pts',(-0.72404017032704,-6.93313670432102,
0.321214300938314));
#66877=CARTESIAN_POINT('Ctrl Pts',(-0.733252004260348,-6.91124292430801,
0.642212700743149));
#66878=CARTESIAN_POINT('Ctrl Pts',(-0.742463838193657,-6.86680430682767,
0.960059070181433));
#66879=CARTESIAN_POINT('Ctrl Pts',(-0.775515131518135,-6.70736224654842,
2.10046538498052));
#66880=CARTESIAN_POINT('Ctrl Pts',(-0.808566424842613,-6.25769718736783,
3.200295150628));
#66881=CARTESIAN_POINT('Ctrl Pts',(-0.841617718167092,-5.57251192825613,
4.12575152135315));
#66882=CARTESIAN_POINT('Ctrl Pts',(-0.874669011491571,-4.88732666914443,
5.05120789207829));
#66883=CARTESIAN_POINT('Ctrl Pts',(-0.90772030481605,-3.96662121010161,
5.8022908678811));
#66884=CARTESIAN_POINT('Ctrl Pts',(-0.940771598140529,-2.9224015089145,
6.28762946007467));
#66885=CARTESIAN_POINT('Ctrl Pts',(-0.973822891465008,-1.87818180772739,
6.77296805226824));
#66886=CARTESIAN_POINT('Ctrl Pts',(-1.00687418478949,-0.710447864395994,
6.99256226085256));
#66887=CARTESIAN_POINT('Ctrl Pts',(-1.03992547811396,0.438742774360017,
6.91969794026094));
#66888=CARTESIAN_POINT('Ctrl Pts',(-1.07297677143844,1.58793341311603,6.84683361966932));
#66889=CARTESIAN_POINT('Ctrl Pts',(-1.10602806476292,2.71858074729665,6.48151076990174));
#66890=CARTESIAN_POINT('Ctrl Pts',(-1.1390793580874,3.69313890233341,5.86817176423596));
#66891=CARTESIAN_POINT('Ctrl Pts',(-1.17213065141188,4.66769705737016,5.25483275857018));
#66892=CARTESIAN_POINT('Ctrl Pts',(-1.20518194473636,5.48616603326304,4.39347759700619));
#66893=CARTESIAN_POINT('Ctrl Pts',(-1.23823323806084,6.04897717788414,3.38889213577852));
#66894=CARTESIAN_POINT('Ctrl Pts',(-1.27128453138532,6.61178832250524,2.38430667455085));
#66895=CARTESIAN_POINT('Ctrl Pts',(-1.3043358247098,6.91894163585457,1.23649091365949));
#66896=CARTESIAN_POINT('Ctrl Pts',(-1.33738711803427,6.93307120388089,0.0850793066626232));
#66897=CARTESIAN_POINT('Ctrl Pts',(-1.37043841135875,6.94720077190721,-1.06633230033425));
#66898=CARTESIAN_POINT('Ctrl Pts',(-1.40348970468323,6.66830659461054,-2.22133975343664));
#66899=CARTESIAN_POINT('Ctrl Pts',(-1.43654099800771,6.13031679649852,-3.23943371302343));
#66900=CARTESIAN_POINT('Ctrl Pts',(-1.46959229133219,5.5923269983865,-4.25752767261022));
#66901=CARTESIAN_POINT('Ctrl Pts',(-1.50264358465667,4.79524157945913,-5.13870813868142));
#66902=CARTESIAN_POINT('Ctrl Pts',(-1.53569487798115,3.83602783246789,-5.77577746065725));
#66903=CARTESIAN_POINT('Ctrl Pts',(-1.56874617130562,2.87681408547664,-6.41284678263308));
#66904=CARTESIAN_POINT('Ctrl Pts',(-1.6017974646301,1.75547201042152,-6.80580496051356));
#66905=CARTESIAN_POINT('Ctrl Pts',(-1.63484875795458,0.608415475483342,
-6.90684771916227));
#66906=CARTESIAN_POINT('Ctrl Pts',(-1.66790005127906,-0.53864105945484,
-7.00789047781097));
#66907=CARTESIAN_POINT('Ctrl Pts',(-1.70095134460354,-1.71141205427608,
-6.81701781722792));
#66908=CARTESIAN_POINT('Ctrl Pts',(-1.73400263792802,-2.76722719324648,
-6.35744983994855));
#66909=CARTESIAN_POINT('Ctrl Pts',(-1.7670539312525,-3.82304233221688,-5.89788186266918));
#66910=CARTESIAN_POINT('Ctrl Pts',(-1.80010522457698,-4.76190161533643,
-5.1696185686935));
#66911=CARTESIAN_POINT('Ctrl Pts',(-1.83315651790145,-5.46959062995009,
-4.26125487940662));
#66912=CARTESIAN_POINT('Ctrl Pts',(-1.86620781122593,-6.17727964456378,
-3.35289119011972));
#66913=CARTESIAN_POINT('Ctrl Pts',(-1.89925910455042,-6.65379839067156,
-2.26442710552161));
#66914=CARTESIAN_POINT('Ctrl Pts',(-1.9323103978749,-6.84117725591047,-1.12827680988217));
#66915=CARTESIAN_POINT('Ctrl Pts',(-1.94314971071451,-6.90262895524085,
-0.755671466837037));
#66916=CARTESIAN_POINT('Ctrl Pts',(-1.95398902355412,-6.93298250252378,
-0.377937280835089));
#66917=CARTESIAN_POINT('Ctrl Pts',(-1.96482833639373,-6.93267455605571,
-0.000154115015024714));
#66918=CARTESIAN_POINT('Ctrl Pts',(-2.14417166360627,-6.93278353301175,
-0.000170174852231984));
#66919=CARTESIAN_POINT('Ctrl Pts',(-2.13449775009798,-6.93309429521638,
-0.337320405264556));
#66920=CARTESIAN_POINT('Ctrl Pts',(-2.12482383658969,-6.90894037892185,
-0.674426493780623));
#66921=CARTESIAN_POINT('Ctrl Pts',(-2.11514992308141,-6.8599479572671,-1.00788323781755));
#66922=CARTESIAN_POINT('Ctrl Pts',(-2.08209862975693,-6.69256348588433,
-2.14715088257655));
#66923=CARTESIAN_POINT('Ctrl Pts',(-2.04904733643245,-6.23524579673307,
-3.24382070704658));
#66924=CARTESIAN_POINT('Ctrl Pts',(-2.01599604310797,-5.54362864899564,
-4.16448027964133));
#66925=CARTESIAN_POINT('Ctrl Pts',(-1.98294474978349,-4.85201150125823,
-5.08513985223605));
#66926=CARTESIAN_POINT('Ctrl Pts',(-1.94989345645902,-3.92609489493467,
-5.82978917295552));
#66927=CARTESIAN_POINT('Ctrl Pts',(-1.91684216313454,-2.8785187359834,-6.30783992219835));
#66928=CARTESIAN_POINT('Ctrl Pts',(-1.88379086981006,-1.83094257703207,
-6.78589067144121));
#66929=CARTESIAN_POINT('Ctrl Pts',(-1.85073957648558,-0.661706865453005,
-6.9973428492074));
#66930=CARTESIAN_POINT('Ctrl Pts',(-1.8176882831611,0.48694815843834,-6.91647280689227));
#66931=CARTESIAN_POINT('Ctrl Pts',(-1.78463698983662,1.63560318232962,-6.83560276457714));
#66932=CARTESIAN_POINT('Ctrl Pts',(-1.75158569651214,2.76367751853319,-6.46241050218072));
#66933=CARTESIAN_POINT('Ctrl Pts',(-1.71853440318767,3.73393830366126,-5.84229572530679));
#66934=CARTESIAN_POINT('Ctrl Pts',(-1.68548310986319,4.70419908878935,-5.22218094843285));
#66935=CARTESIAN_POINT('Ctrl Pts',(-1.65243181653871,5.51664632284193,-4.35514365708138));
#66936=CARTESIAN_POINT('Ctrl Pts',(-1.61938052321423,6.07244391257379,-3.34666095177451));
#66937=CARTESIAN_POINT('Ctrl Pts',(-1.58632922988975,6.62824150230566,-2.33817824646763));
#66938=CARTESIAN_POINT('Ctrl Pts',(-1.55327793656527,6.92738944771679,-1.18825012720539));
#66939=CARTESIAN_POINT('Ctrl Pts',(-1.52022664324079,6.93349570636123,-0.0367680208484475));
#66940=CARTESIAN_POINT('Ctrl Pts',(-1.48717534991632,6.93960196500567,1.11471408550848));
#66941=CARTESIAN_POINT('Ctrl Pts',(-1.45412405659184,6.6526665368834,2.26775017896005));
#66942=CARTESIAN_POINT('Ctrl Pts',(-1.42107276326736,6.10759578334394,3.28207074036592));
#66943=CARTESIAN_POINT('Ctrl Pts',(-1.38802146994288,5.56252502980449,4.29639130177176));
#66944=CARTESIAN_POINT('Ctrl Pts',(-1.3549701766184,4.75931895084777,5.17199633113198));
#66945=CARTESIAN_POINT('Ctrl Pts',(-1.32191888329392,3.79568943173556,5.80236644269368));
#66946=CARTESIAN_POINT('Ctrl Pts',(-1.28886758996944,2.83205991262329,6.43273655425541));
#66947=CARTESIAN_POINT('Ctrl Pts',(-1.25581629664496,1.70800695335555,6.81787174801864));
#66948=CARTESIAN_POINT('Ctrl Pts',(-1.22276500332048,0.560274207474504,
6.9109194330368));
#66949=CARTESIAN_POINT('Ctrl Pts',(-1.18971370999601,-0.587458538406507,
7.00396711805494));
#66950=CARTESIAN_POINT('Ctrl Pts',(-1.15666241667153,-1.75887107090073,
6.80492729432799));
#66951=CARTESIAN_POINT('Ctrl Pts',(-1.12361112334705,-2.81145833437188,
6.33801361875924));
#66952=CARTESIAN_POINT('Ctrl Pts',(-1.09055983002257,-3.86404559784306,
5.87109994319048));
#66953=CARTESIAN_POINT('Ctrl Pts',(-1.05750853669809,-4.79780759229117,
5.13631241577991));
#66954=CARTESIAN_POINT('Ctrl Pts',(-1.02445724337361,-5.49915000206846,
4.22303964606504));
#66955=CARTESIAN_POINT('Ctrl Pts',(-0.99140595004913,-6.20049241184572,
3.30976687635023));
#66956=CARTESIAN_POINT('Ctrl Pts',(-0.958354656724652,-6.66941523695218,
2.21800886433114));
#66957=CARTESIAN_POINT('Ctrl Pts',(-0.925303363400175,-6.84887292645916,
1.08058050819984));
#66958=CARTESIAN_POINT('Ctrl Pts',(-0.914926130135541,-6.90521790173331,
0.723458042294939));
#66959=CARTESIAN_POINT('Ctrl Pts',(-0.904548896870907,-6.9330275729645,
0.361833420535273));
#66960=CARTESIAN_POINT('Ctrl Pts',(-0.894171663606273,-6.9327161513647,
0.000161366341133071));
#66961=CARTESIAN_POINT('Origin',(-3.775,0.,0.));
#66962=CARTESIAN_POINT('',(0.535171663606277,-6.9334003037143,-0.000124581990723627));
#66963=CARTESIAN_POINT('',(0.355828336393729,-6.93349343740785,-9.14711828918373E-5));
#66964=CARTESIAN_POINT('',(-3.775,-6.933,-8.4904762584886E-16));
#66965=CARTESIAN_POINT('Ctrl Pts',(0.535171663606277,-6.9334003037143,-0.000124581990723627));
#66966=CARTESIAN_POINT('Ctrl Pts',(0.505908682900044,-6.93255028157601,
1.01947227644454));
#66967=CARTESIAN_POINT('Ctrl Pts',(0.476645702193811,-6.7048358987811,2.03943623973099));
#66968=CARTESIAN_POINT('Ctrl Pts',(0.447382721487578,-6.26940839990456,
2.96128909796236));
#66969=CARTESIAN_POINT('Ctrl Pts',(0.414331428163099,-5.77761154122546,
4.00248273183317));
#66970=CARTESIAN_POINT('Ctrl Pts',(0.381280134838622,-5.02084040545093,
4.91851855368217));
#66971=CARTESIAN_POINT('Ctrl Pts',(0.348228841514143,-4.09115795914137,
5.5979586779342));
#66972=CARTESIAN_POINT('Ctrl Pts',(0.315177548189664,-3.16147551283182,
6.27739880218624));
#66973=CARTESIAN_POINT('Ctrl Pts',(0.282126254865185,-2.05888175598725,
6.72024322884129));
#66974=CARTESIAN_POINT('Ctrl Pts',(0.249074961540705,-0.917509780327954,
6.87261890471945));
#66975=CARTESIAN_POINT('Ctrl Pts',(0.216023668216227,0.223862195331312,
7.0249945805976));
#66976=CARTESIAN_POINT('Ctrl Pts',(0.182972374891749,1.40401238980529,6.88690150569888));
#66977=CARTESIAN_POINT('Ctrl Pts',(0.149921081567271,2.47937279058131,6.47513902335924));
#66978=CARTESIAN_POINT('Ctrl Pts',(0.116869788242791,3.55473319135739,6.06337654101958));
#66979=CARTESIAN_POINT('Ctrl Pts',(0.0838184949183126,4.52530379843548,
5.37794465123898));
#66980=CARTESIAN_POINT('Ctrl Pts',(0.0507672015938329,5.27301244293917,
4.50222773558971));
#66981=CARTESIAN_POINT('Ctrl Pts',(0.0177159082693552,6.02072108744283,
3.6265108199405));
#66982=CARTESIAN_POINT('Ctrl Pts',(-0.0153353850551226,6.54556776937211,
2.56050887842267));
#66983=CARTESIAN_POINT('Ctrl Pts',(-0.0483866783796008,6.78370367071106,
1.43390352342335));
#66984=CARTESIAN_POINT('Ctrl Pts',(-0.0814379717040799,7.02183957205002,
0.307298168423996));
#66985=CARTESIAN_POINT('Ctrl Pts',(-0.114489265028562,6.97326469279862,
-0.879910600056927));
#66986=CARTESIAN_POINT('Ctrl Pts',(-0.14754055835304,6.64388827985173,-1.98329607758234));
#66987=CARTESIAN_POINT('Ctrl Pts',(-0.180591851677519,6.31451186690483,
-3.08668155510775));
#66988=CARTESIAN_POINT('Ctrl Pts',(-0.213643145001997,5.70433392026246,
-4.10624374167772));
#66989=CARTESIAN_POINT('Ctrl Pts',(-0.246694438326475,4.88758400450776,
-4.91795052896881));
#66990=CARTESIAN_POINT('Ctrl Pts',(-0.279745731650954,4.07083408875305,
-5.72965731625989));
#66991=CARTESIAN_POINT('Ctrl Pts',(-0.312797024975433,3.04751220388602,
-6.33350870427208));
#66992=CARTESIAN_POINT('Ctrl Pts',(-0.345848318299913,1.94210783426131,
-6.65604476897545));
#66993=CARTESIAN_POINT('Ctrl Pts',(-0.378899611624392,0.836703464636607,
-6.97858083367883));
#66994=CARTESIAN_POINT('Ctrl Pts',(-0.411950904948871,-0.350783389745759,
-7.01980157507339));
#66995=CARTESIAN_POINT('Ctrl Pts',(-0.44500219827335,-1.47589219465302,
-6.77469239421739));
#66996=CARTESIAN_POINT('Ctrl Pts',(-0.47805349159783,-2.60100099956031,
-6.52958321336138));
#66997=CARTESIAN_POINT('Ctrl Pts',(-0.511104784922308,-3.66373175499246,
-5.99814411025479));
#66998=CARTESIAN_POINT('Ctrl Pts',(-0.544156078246788,-4.53480079594826,
-5.24502588626326));
#66999=CARTESIAN_POINT('Ctrl Pts',(-0.577207371571265,-5.40586983690397,
-4.49190766227179));
#67000=CARTESIAN_POINT('Ctrl Pts',(-0.610258664895742,-6.08527716338335,
-3.51711031739542));
#67001=CARTESIAN_POINT('Ctrl Pts',(-0.643309958220219,-6.49037129593408,
-2.43922021298191));
#67002=CARTESIAN_POINT('Ctrl Pts',(-0.66714941761139,-6.78256031945386,
-1.66175238078425));
#67003=CARTESIAN_POINT('Ctrl Pts',(-0.690988877002561,-6.93203665528496,
-0.830650071206651));
#67004=CARTESIAN_POINT('Ctrl Pts',(-0.714828336393731,-6.93283010606057,
0.00017441890636849));
#67005=CARTESIAN_POINT('Ctrl Pts',(-0.894171663606273,-6.9327161513647,
0.000161366341133071));
#67006=CARTESIAN_POINT('Ctrl Pts',(-0.871497603546429,-6.93203570100982,
-0.790085288970428));
#67007=CARTESIAN_POINT('Ctrl Pts',(-0.848823543486585,-6.79710113099127,
-1.58055839350899));
#67008=CARTESIAN_POINT('Ctrl Pts',(-0.826149483426741,-6.53223324953361,
-2.32478888744209));
#67009=CARTESIAN_POINT('Ctrl Pts',(-0.793098190102262,-6.14614332919358,
-3.40963122670925));
#67010=CARTESIAN_POINT('Ctrl Pts',(-0.760046896777782,-5.48397093460601,
-4.396217205));
#67011=CARTESIAN_POINT('Ctrl Pts',(-0.726995603453304,-4.62627087572379,
-5.16452634632805));
#67012=CARTESIAN_POINT('Ctrl Pts',(-0.693944310128825,-3.76857081684157,
-5.9328354876561));
#67013=CARTESIAN_POINT('Ctrl Pts',(-0.660893016804347,-2.7153430936647,
-6.48286779202144));
#67014=CARTESIAN_POINT('Ctrl Pts',(-0.627841723479869,-1.5947153052461,
-6.74771055193542));
#67015=CARTESIAN_POINT('Ctrl Pts',(-0.59479043015539,-0.474087516827503,
-7.01255331184939));
#67016=CARTESIAN_POINT('Ctrl Pts',(-0.561739136830911,0.713940336832824,
-6.992206527312));
#67017=CARTESIAN_POINT('Ctrl Pts',(-0.528687843506432,1.82484190768325,
-6.68914543192549));
#67018=CARTESIAN_POINT('Ctrl Pts',(-0.495636550181953,2.93574347853367,
-6.38608433653898));
#67019=CARTESIAN_POINT('Ctrl Pts',(-0.462585256857474,3.96951876657419,
-5.80030893030336));
#67020=CARTESIAN_POINT('Ctrl Pts',(-0.429533963532995,4.80040660667202,
-5.00308015207695));
#67021=CARTESIAN_POINT('Ctrl Pts',(-0.396482670208517,5.63129444676985,
-4.20585137385055));
#67022=CARTESIAN_POINT('Ctrl Pts',(-0.363431376884039,6.259294838925,-3.19716922363337));
#67023=CARTESIAN_POINT('Ctrl Pts',(-0.330380083559561,6.60801007665816,
-2.09974222805347));
#67024=CARTESIAN_POINT('Ctrl Pts',(-0.297328790235082,6.95672531439132,
-1.00231523247358));
#67025=CARTESIAN_POINT('Ctrl Pts',(-0.264277496910602,7.02615539770249,
0.183856608469029));
#67026=CARTESIAN_POINT('Ctrl Pts',(-0.231226203586123,6.80785399567866,
1.31447273498114));
#67027=CARTESIAN_POINT('Ctrl Pts',(-0.198174910261644,6.58955259365484,
2.44508886149324));
#67028=CARTESIAN_POINT('Ctrl Pts',(-0.165123616937165,6.08351970629602,
3.52014927357485));
#67029=CARTESIAN_POINT('Ctrl Pts',(-0.132072323612686,5.35131540980637,
4.40887037485291));
#67030=CARTESIAN_POINT('Ctrl Pts',(-0.0990210302882075,4.61911111331672,
5.29759147613098));
#67031=CARTESIAN_POINT('Ctrl Pts',(-0.0659697369637293,3.66073540769622,
5.9999732666055));
#67032=CARTESIAN_POINT('Ctrl Pts',(-0.0329184436392508,2.59277692373161,
6.43056936991209));
#67033=CARTESIAN_POINT('Ctrl Pts',(0.000132849685227725,1.524818439767,
6.86116547321868));
#67034=CARTESIAN_POINT('Ctrl Pts',(0.0331841430097067,0.347277177458266,
7.01997588935733));
#67035=CARTESIAN_POINT('Ctrl Pts',(0.0662354363341857,-0.796596233340036,
6.8876809623062));
#67036=CARTESIAN_POINT('Ctrl Pts',(0.0992867296586647,-1.94046964413834,
6.75538603525507));
#67037=CARTESIAN_POINT('Ctrl Pts',(0.132338022983144,-3.05067520342622,
6.33198576501416));
#67038=CARTESIAN_POINT('Ctrl Pts',(0.165389316307622,-3.99215382603479,
5.66898777796905));
#67039=CARTESIAN_POINT('Ctrl Pts',(0.198440609632101,-4.93363244864337,
5.00598979092394));
#67040=CARTESIAN_POINT('Ctrl Pts',(0.231491902956579,-5.70638413457265,
4.10339408707464));
#67041=CARTESIAN_POINT('Ctrl Pts',(0.264543196281057,-6.21640184621488,
3.07100353042177));
#67042=CARTESIAN_POINT('Ctrl Pts',(0.294971576318614,-6.68594512863285,
2.12054232163898));
#67043=CARTESIAN_POINT('Ctrl Pts',(0.325399956356172,-6.93280032536449,
1.06006957977906));
#67044=CARTESIAN_POINT('Ctrl Pts',(0.355828336393729,-6.93349343740785,
-9.14711828918373E-5));
#67045=CARTESIAN_POINT('Origin',(-3.775,0.,0.));
#67046=CARTESIAN_POINT('',(1.78517166360628,-6.93240903352825,8.51318353534136E-6));
#67047=CARTESIAN_POINT('',(1.60582833639373,-6.93241554159061,-2.91227924267906E-5));
#67048=CARTESIAN_POINT('',(-3.775,-6.933,-8.4904762584886E-16));
#67049=CARTESIAN_POINT('Ctrl Pts',(1.78517166360628,-6.93240903352825,8.51318353534136E-6));
#67050=CARTESIAN_POINT('Ctrl Pts',(1.7689088294516,-6.93243330175633,0.566880142059182));
#67051=CARTESIAN_POINT('Ctrl Pts',(1.75264599529692,-6.86369887729813,1.13374598789551));
#67052=CARTESIAN_POINT('Ctrl Pts',(1.73638316114225,-6.72613751527892,1.68338615060896));
#67053=CARTESIAN_POINT('Ctrl Pts',(1.70333186781777,-6.446568721613,2.8004311913427));
#67054=CARTESIAN_POINT('Ctrl Pts',(1.67028057449329,-5.88272216008265,3.84632852564582));
#67055=CARTESIAN_POINT('Ctrl Pts',(1.63722928116881,-5.10319107464959,4.69384231329956));
#67056=CARTESIAN_POINT('Ctrl Pts',(1.60417798784433,-4.32365998921648,5.54135610095335));
#67057=CARTESIAN_POINT('Ctrl Pts',(1.57112669451985,-3.32844437988063,6.19048634195776));
#67058=CARTESIAN_POINT('Ctrl Pts',(1.53807540119537,-2.23861453729065,6.56226483463869));
#67059=CARTESIAN_POINT('Ctrl Pts',(1.50502410787089,-1.14878469470068,6.93404332731963));
#67060=CARTESIAN_POINT('Ctrl Pts',(1.47197281454642,0.0356593811433296,
7.02847007167711));
#67061=CARTESIAN_POINT('Ctrl Pts',(1.43892152122194,1.17062731708598,6.83405783491746));
#67062=CARTESIAN_POINT('Ctrl Pts',(1.40587022789746,2.30559525302856,6.63964559815781));
#67063=CARTESIAN_POINT('Ctrl Pts',(1.37281893457298,3.39108704906978,6.156394380281));
#67064=CARTESIAN_POINT('Ctrl Pts',(1.3397676412485,4.29505010674682,5.44309281447954));
#67065=CARTESIAN_POINT('Ctrl Pts',(1.30671634792402,5.19901316442391,4.72979124867803));
#67066=CARTESIAN_POINT('Ctrl Pts',(1.27366505459954,5.92144748373691,3.7864393349518));
#67067=CARTESIAN_POINT('Ctrl Pts',(1.24061376127506,6.37446725160844,2.72779802490509));
#67068=CARTESIAN_POINT('Ctrl Pts',(1.20756246795058,6.82748701947995,1.66915671485844));
#67069=CARTESIAN_POINT('Ctrl Pts',(1.17451117462611,7.01109223591004,0.495226008491308));
#67070=CARTESIAN_POINT('Ctrl Pts',(1.14145988130163,6.90294689982591,-0.65118269685897));
#67071=CARTESIAN_POINT('Ctrl Pts',(1.10840858797715,6.79480156374177,-1.79759140220928));
#67072=CARTESIAN_POINT('Ctrl Pts',(1.07535729465267,6.39490567514344,-2.91647810654265));
#67073=CARTESIAN_POINT('Ctrl Pts',(1.0423060013282,5.7519074977916,-3.87172764323028));
#67074=CARTESIAN_POINT('Ctrl Pts',(1.00925470800372,5.10890932043973,-4.82697717991793));
#67075=CARTESIAN_POINT('Ctrl Pts',(0.976203414679236,4.22280885433436,-5.61858954895975));
#67076=CARTESIAN_POINT('Ctrl Pts',(0.943152121354756,3.20140227948802,-6.1502632668361));
#67077=CARTESIAN_POINT('Ctrl Pts',(0.910100828030278,2.17999570464171,-6.68193698471244));
#67078=CARTESIAN_POINT('Ctrl Pts',(0.877049534705799,1.02328302105442,-6.95367205142334));
#67079=CARTESIAN_POINT('Ctrl Pts',(0.843998241381321,-0.128018986403163,
-6.93241126489369));
#67080=CARTESIAN_POINT('Ctrl Pts',(0.810946948056843,-1.27932099386075,
-6.91115047836404));
#67081=CARTESIAN_POINT('Ctrl Pts',(0.777895654732364,-2.42521232518865,
-6.59689383859384));
#67082=CARTESIAN_POINT('Ctrl Pts',(0.744844361407885,-3.42629263815531,
-6.02787139579365));
#67083=CARTESIAN_POINT('Ctrl Pts',(0.711793068083405,-4.42737295112197,
-5.45884895299347));
#67084=CARTESIAN_POINT('Ctrl Pts',(0.678741774758925,-5.2836422457274,-4.63506070716328));
#67085=CARTESIAN_POINT('Ctrl Pts',(0.645690481434447,-5.89093337326648,
-3.65672241197494));
#67086=CARTESIAN_POINT('Ctrl Pts',(0.612639188109969,-6.49822450080554,
-2.67838411678662));
#67087=CARTESIAN_POINT('Ctrl Pts',(0.579587894785492,-6.85653746127826,
-1.54549577224014));
#67088=CARTESIAN_POINT('Ctrl Pts',(0.546536601461015,-6.92228265072279,
-0.395875877020612));
#67089=CARTESIAN_POINT('Ctrl Pts',(0.542748288842769,-6.92981831137959,
-0.26410737064204));
#67090=CARTESIAN_POINT('Ctrl Pts',(0.538959976224523,-6.9335103454638,-0.132119052516801));
#67091=CARTESIAN_POINT('Ctrl Pts',(0.535171663606277,-6.9334003037143,-0.000124581990723627));
#67092=CARTESIAN_POINT('Ctrl Pts',(0.355828336393729,-6.93349343740785,
-9.14711828918373E-5));
#67093=CARTESIAN_POINT('Ctrl Pts',(0.358451249680651,-6.93355318336822,
-0.0914768983207502));
#67094=CARTESIAN_POINT('Ctrl Pts',(0.361074162967572,-6.9317838549599,-0.182860009481177));
#67095=CARTESIAN_POINT('Ctrl Pts',(0.363697076254494,-6.92817041721913,
-0.27417014326238));
#67096=CARTESIAN_POINT('Ctrl Pts',(0.396748369578973,-6.88263753922595,
-1.42476785083719));
#67097=CARTESIAN_POINT('Ctrl Pts',(0.42979966290345,-6.54428804588444,-2.56377785653038));
#67098=CARTESIAN_POINT('Ctrl Pts',(0.462850956227928,-5.95428293900704,
-3.55263694735846));
#67099=CARTESIAN_POINT('Ctrl Pts',(0.495902249552406,-5.36427783212963,
-4.54149603818656));
#67100=CARTESIAN_POINT('Ctrl Pts',(0.528953542876885,-4.52261711171632,
-5.38020421414952));
#67101=CARTESIAN_POINT('Ctrl Pts',(0.562004836201364,-3.53169075948771,
-5.96673067741756));
#67102=CARTESIAN_POINT('Ctrl Pts',(0.595056129525843,-2.54076440725911,
-6.55325714068561));
#67103=CARTESIAN_POINT('Ctrl Pts',(0.628107422850322,-1.40057242321521,
-6.88760189125872));
#67104=CARTESIAN_POINT('Ctrl Pts',(0.661158716174801,-0.249821810751499,
-6.92909111358478));
#67105=CARTESIAN_POINT('Ctrl Pts',(0.69421000949928,0.900928801712209,-6.97058033591085));
#67106=CARTESIAN_POINT('Ctrl Pts',(0.727261302823757,2.0622380425957,-6.71921402998986));
#67107=CARTESIAN_POINT('Ctrl Pts',(0.760312596148236,3.09282994515598,-6.20557149083251));
#67108=CARTESIAN_POINT('Ctrl Pts',(0.793363889472715,4.12342184771625,-5.69192895167516));
#67109=CARTESIAN_POINT('Ctrl Pts',(0.826415182797194,5.02329641195328,-4.91601017928145));
#67110=CARTESIAN_POINT('Ctrl Pts',(0.859466476121673,5.68298180682118,-3.9722074946843));
#67111=CARTESIAN_POINT('Ctrl Pts',(0.892517769446152,6.34266720168907,-3.02840481008717));
#67112=CARTESIAN_POINT('Ctrl Pts',(0.925569062770629,6.76216342718784,-1.91671821328664));
#67113=CARTESIAN_POINT('Ctrl Pts',(0.958620356095107,6.89043779304345,-0.772386961105221));
#67114=CARTESIAN_POINT('Ctrl Pts',(0.991671649419586,7.01871215889905,0.371944291076227));
#67115=CARTESIAN_POINT('Ctrl Pts',(1.02472294274407,6.85576466511146,1.54892019863863));
#67116=CARTESIAN_POINT('Ctrl Pts',(1.05777423606855,6.42141825280848,2.61535890844541));
#67117=CARTESIAN_POINT('Ctrl Pts',(1.09082552939302,5.98707184050551,3.68179761825219));
#67118=CARTESIAN_POINT('Ctrl Pts',(1.1238768227175,5.28132650968716,4.63769913030343));
#67119=CARTESIAN_POINT('Ctrl Pts',(1.15692811604198,4.39003781921376,5.36677580520741));
#67120=CARTESIAN_POINT('Ctrl Pts',(1.18997940936646,3.49874912874037,6.09585248011138));
#67121=CARTESIAN_POINT('Ctrl Pts',(1.22303070269094,2.42191707861195,6.59810431786807));
#67122=CARTESIAN_POINT('Ctrl Pts',(1.25608199601542,1.29054078908523,6.81243121574038));
#67123=CARTESIAN_POINT('Ctrl Pts',(1.2891332893399,0.159164499558506,7.02675811361269));
#67124=CARTESIAN_POINT('Ctrl Pts',(1.32218458266438,-1.02675602936649,6.95316007160062));
#67125=CARTESIAN_POINT('Ctrl Pts',(1.35523587598886,-2.12295081058728,6.60059046247482));
#67126=CARTESIAN_POINT('Ctrl Pts',(1.38828716931333,-3.21914559180807,6.24802085334902));
#67127=CARTESIAN_POINT('Ctrl Pts',(1.42133846263781,-4.22561462532463,5.6164796771095));
#67128=CARTESIAN_POINT('Ctrl Pts',(1.45438975596229,-5.01991861529638,4.78279538484427));
#67129=CARTESIAN_POINT('Ctrl Pts',(1.48744104928677,-5.81422260526812,3.94911109257903));
#67130=CARTESIAN_POINT('Ctrl Pts',(1.52049234261125,-6.39636155169502,2.91328368428809));
#67131=CARTESIAN_POINT('Ctrl Pts',(1.55354363593573,-6.69551689950157,1.80132397029951));
#67132=CARTESIAN_POINT('Ctrl Pts',(1.57097186942173,-6.85326410772647,1.21497797372492));
#67133=CARTESIAN_POINT('Ctrl Pts',(1.58840010290773,-6.93232647210883,0.607463052115828));
#67134=CARTESIAN_POINT('Ctrl Pts',(1.60582833639373,-6.93241554159061,-2.91227924267906E-5));
#67135=CARTESIAN_POINT('Origin',(-3.775,0.,0.));
#67136=CARTESIAN_POINT('',(3.03517166360627,-6.93344508439855,0.000110442622268392));
#67137=CARTESIAN_POINT('',(2.85582833639373,-6.93334073279147,0.000139834461613099));
#67138=CARTESIAN_POINT('',(-3.775,-6.933,-8.4904762584886E-16));
#67139=CARTESIAN_POINT('Ctrl Pts',(3.03517166360627,-6.93344508439855,0.000110442622268392));
#67140=CARTESIAN_POINT('Ctrl Pts',(3.03190897600315,-6.93353152368877,0.113788670324413));
#67141=CARTESIAN_POINT('Ctrl Pts',(3.02864628840003,-6.93079336343887,0.227462733245047));
#67142=CARTESIAN_POINT('Ctrl Pts',(3.02538360079691,-6.92520297852914,0.340996352887752));
#67143=CARTESIAN_POINT('Ctrl Pts',(2.99233230747244,-6.86857192035748,1.49110124230881));
#67144=CARTESIAN_POINT('Ctrl Pts',(2.95928101414796,-6.51924966455837,2.62679404428279));
#67145=CARTESIAN_POINT('Ctrl Pts',(2.92622972082349,-5.91973207498778,3.60991509136462));
#67146=CARTESIAN_POINT('Ctrl Pts',(2.89317842749901,-5.32021448541714,4.59303613844651));
#67147=CARTESIAN_POINT('Ctrl Pts',(2.86012713417452,-4.470501562075,5.42358543063623));
#67148=CARTESIAN_POINT('Ctrl Pts',(2.82707584085004,-3.47396285587152,6.0005247172669));
#67149=CARTESIAN_POINT('Ctrl Pts',(2.79402454752556,-2.47742414966807,6.57746400389754));
#67150=CARTESIAN_POINT('Ctrl Pts',(2.76097325420109,-1.3340596606033,6.90079328496915));
#67151=CARTESIAN_POINT('Ctrl Pts',(2.72792196087661,-0.182962334678425,
6.93117880238228));
#67152=CARTESIAN_POINT('Ctrl Pts',(2.69487066755213,0.968134991246454,6.9615643197954));
#67153=CARTESIAN_POINT('Ctrl Pts',(2.66181937422765,2.12696515403145,6.69900607355004));
#67154=CARTESIAN_POINT('Ctrl Pts',(2.62876808090317,3.15255377254311,6.17544488419488));
#67155=CARTESIAN_POINT('Ctrl Pts',(2.59571678757869,4.17814239105477,5.65188369483972));
#67156=CARTESIAN_POINT('Ctrl Pts',(2.56266549425421,5.07048946529311,4.86731956237475));
#67157=CARTESIAN_POINT('Ctrl Pts',(2.52961420092973,5.72103890085591,3.91719653596781));
#67158=CARTESIAN_POINT('Ctrl Pts',(2.49656290760526,6.37158833641871,2.96707350956087));
#67159=CARTESIAN_POINT('Ctrl Pts',(2.46351161428078,6.78034013330596,1.85139158921196));
#67160=CARTESIAN_POINT('Ctrl Pts',(2.4304603209563,6.8975686859424,0.705876072133954));
#67161=CARTESIAN_POINT('Ctrl Pts',(2.39740902763182,7.01479723857884,-0.43963944494405));
#67162=CARTESIAN_POINT('Ctrl Pts',(2.36435773430734,6.84050254696446,-1.61498855875114));
#67163=CARTESIAN_POINT('Ctrl Pts',(2.33130644098286,6.39588796520089,-2.6771873193901));
#67164=CARTESIAN_POINT('Ctrl Pts',(2.29825514765838,5.95127338343732,-3.73938608002905));
#67165=CARTESIAN_POINT('Ctrl Pts',(2.26520385433391,5.23633891152456,-4.68843448749987));
#67166=CARTESIAN_POINT('Ctrl Pts',(2.23215256100943,4.33805798868245,-5.408878598502));
#67167=CARTESIAN_POINT('Ctrl Pts',(2.19910126768495,3.43977706584034,-6.12932270950414));
#67168=CARTESIAN_POINT('Ctrl Pts',(2.16604997436047,2.35814969206887,-6.62116252403759));
#67169=CARTESIAN_POINT('Ctrl Pts',(2.13299868103599,1.22475834988496,-6.8245645861763));
#67170=CARTESIAN_POINT('Ctrl Pts',(2.09994738771151,0.0913670077010516,
-7.02796664831501));
#67171=CARTESIAN_POINT('Ctrl Pts',(2.06689609438703,-1.09378830289531,-6.94293095805898));
#67172=CARTESIAN_POINT('Ctrl Pts',(2.03384480106255,-2.1865306853888,-6.57980230465611));
#67173=CARTESIAN_POINT('Ctrl Pts',(2.00079350773808,-3.27927306788225,-6.21667365125325));
#67174=CARTESIAN_POINT('Ctrl Pts',(1.9677422144136,-4.27960252227285,-5.57545203470356));
#67175=CARTESIAN_POINT('Ctrl Pts',(1.93469092108912,-5.0658266467822,-4.73414355414536));
#67176=CARTESIAN_POINT('Ctrl Pts',(1.90163962776464,-5.85205077129157,-3.89283507358712));
#67177=CARTESIAN_POINT('Ctrl Pts',(1.86858833444016,-6.42416956591969,-2.85143972902036));
#67178=CARTESIAN_POINT('Ctrl Pts',(1.83553704111568,-6.71258345033301,-1.73664568315478));
#67179=CARTESIAN_POINT('Ctrl Pts',(1.81874858194588,-6.85908376047037,-1.17038420170491));
#67180=CARTESIAN_POINT('Ctrl Pts',(1.80196012277608,-6.9323839809358,-0.585184762809014));
#67181=CARTESIAN_POINT('Ctrl Pts',(1.78517166360628,-6.93240903352825,8.51318353534136E-6));
#67182=CARTESIAN_POINT('Ctrl Pts',(1.60582833639373,-6.93241554159061,-2.91227924267906E-5));
#67183=CARTESIAN_POINT('Ctrl Pts',(1.62145139623221,-6.93249538547409,-0.544598749290784));
#67184=CARTESIAN_POINT('Ctrl Pts',(1.63707445607069,-6.86911440472784,-1.08915009714958));
#67185=CARTESIAN_POINT('Ctrl Pts',(1.65269751590916,-6.74206481620649,-1.61841793476135));
#67186=CARTESIAN_POINT('Ctrl Pts',(1.68574880923364,-6.47328563591869,-2.73810810614741));
#67187=CARTESIAN_POINT('Ctrl Pts',(1.71880010255812,-5.91955552615691,-3.78939642923338));
#67188=CARTESIAN_POINT('Ctrl Pts',(1.7518513958826,-5.14823704102586,-4.64439123749239));
#67189=CARTESIAN_POINT('Ctrl Pts',(1.78490268920708,-4.37691855589478,-5.49938604575143));
#67190=CARTESIAN_POINT('Ctrl Pts',(1.81795398253156,-3.38801169539442,-6.15808733918351));
#67191=CARTESIAN_POINT('Ctrl Pts',(1.85100527585604,-2.30181927622303,-6.54036257535428));
#67192=CARTESIAN_POINT('Ctrl Pts',(1.88405656918051,-1.21562685705165,-6.92263781152505));
#67193=CARTESIAN_POINT('Ctrl Pts',(1.91710786250499,-0.0321488792092285,
-7.02848699043451));
#67194=CARTESIAN_POINT('Ctrl Pts',(1.95015915582947,1.10464181221467,-6.8450333135927));
#67195=CARTESIAN_POINT('Ctrl Pts',(1.98321044915395,2.24143250363856,-6.66157963675089));
#67196=CARTESIAN_POINT('Ctrl Pts',(2.01626174247843,3.33153590864396,-6.1888231041578));
#67197=CARTESIAN_POINT('Ctrl Pts',(2.04931303580291,4.24233841582545,-5.48427564616316));
#67198=CARTESIAN_POINT('Ctrl Pts',(2.08236432912739,5.15314092300694,-4.77972818816852));
#67199=CARTESIAN_POINT('Ctrl Pts',(2.11541562245186,5.88464253236454,-3.84338980477231));
#67200=CARTESIAN_POINT('Ctrl Pts',(2.14846691577634,6.34785437392469,-2.78916823532248));
#67201=CARTESIAN_POINT('Ctrl Pts',(2.18151820910082,6.81106621548483,-1.73494666587266));
#67202=CARTESIAN_POINT('Ctrl Pts',(2.2145695024253,7.00598828924752,-0.562841910369289));
#67203=CARTESIAN_POINT('Ctrl Pts',(2.24762079574978,6.90890787215769,0.584556765014494));
#67204=CARTESIAN_POINT('Ctrl Pts',(2.28067208907426,6.81182745506786,1.73195544039831));
#67205=CARTESIAN_POINT('Ctrl Pts',(2.31372338239873,6.42274454712547,2.85464803566247));
#67206=CARTESIAN_POINT('Ctrl Pts',(2.34677467572321,5.78899198787716,3.81605638870559));
#67207=CARTESIAN_POINT('Ctrl Pts',(2.37982596904769,5.15523942862888,4.77746474174866));
#67208=CARTESIAN_POINT('Ctrl Pts',(2.41287726237217,4.2768172180747,5.57758885257073));
#67209=CARTESIAN_POINT('Ctrl Pts',(2.44592855569665,3.26058745860362,6.11909176449279));
#67210=CARTESIAN_POINT('Ctrl Pts',(2.47897984902113,2.24435769913248,6.66059467641489));
#67211=CARTESIAN_POINT('Ctrl Pts',(2.51203114234561,1.09032039074442,6.94347638943696));
#67212=CARTESIAN_POINT('Ctrl Pts',(2.54508243567009,-0.0611331472974662,
6.93332368606776));
#67213=CARTESIAN_POINT('Ctrl Pts',(2.57813372899457,-1.21258668533932,6.92317098269856));
#67214=CARTESIAN_POINT('Ctrl Pts',(2.61118502231905,-2.361456453035,6.6199838629381));
#67215=CARTESIAN_POINT('Ctrl Pts',(2.64423631564353,-3.36797977445027,6.06064574417451));
#67216=CARTESIAN_POINT('Ctrl Pts',(2.67728760896801,-4.37450309586553,5.50130762541093));
#67217=CARTESIAN_POINT('Ctrl Pts',(2.71033890229248,-5.23867997100039,4.68581850764421));
#67218=CARTESIAN_POINT('Ctrl Pts',(2.74339019561696,-5.85538127560987,3.71338453633933));
#67219=CARTESIAN_POINT('Ctrl Pts',(2.77644148894144,-6.47208258021935,2.74095056503446));
#67220=CARTESIAN_POINT('Ctrl Pts',(2.80949278226592,-6.84130831430346,1.61157174019143));
#67221=CARTESIAN_POINT('Ctrl Pts',(2.8425440755904,-6.91814130964143,0.462639619271227));
#67222=CARTESIAN_POINT('Ctrl Pts',(2.84697216252484,-6.928435102972,0.308710050970712));
#67223=CARTESIAN_POINT('Ctrl Pts',(2.85140024945929,-6.93348055652585,0.154429508353912));
#67224=CARTESIAN_POINT('Ctrl Pts',(2.85582833639373,-6.93334073279147,0.000139834461613099));
#67225=CARTESIAN_POINT('Origin',(-3.775,0.,0.));
#67226=CARTESIAN_POINT('',(4.28517166360628,-6.93277727477507,-0.000169494543622584));
#67227=CARTESIAN_POINT('',(4.10582833639373,-6.93289696494239,-0.00017817873250203));
#67228=CARTESIAN_POINT('',(-3.775,-6.933,-8.4904762584886E-16));
#67229=CARTESIAN_POINT('Ctrl Pts',(4.28517166360628,-6.93277727477507,-0.000169494543622584));
#67230=CARTESIAN_POINT('Ctrl Pts',(4.26185782923023,-6.93203240702967,0.812354315076479));
#67231=CARTESIAN_POINT('Ctrl Pts',(4.23854399485419,-6.78921230528412,1.62513310006042));
#67232=CARTESIAN_POINT('Ctrl Pts',(4.21523016047815,-6.50950105747068,2.38769989929238));
#67233=CARTESIAN_POINT('Ctrl Pts',(4.18217886715367,-6.1129631757768,3.46876698394251));
#67234=CARTESIAN_POINT('Ctrl Pts',(4.14912757382919,-5.44130358377228,4.44891879543591));
#67235=CARTESIAN_POINT('Ctrl Pts',(4.11607628050472,-4.57623123673602,5.20891759062465));
#67236=CARTESIAN_POINT('Ctrl Pts',(4.08302498718024,-3.71115888969976,5.9689163858134));
#67237=CARTESIAN_POINT('Ctrl Pts',(4.04997369385575,-2.65267378763176,6.50876216469748));
#67238=CARTESIAN_POINT('Ctrl Pts',(4.01692240053127,-1.52954309898529,6.76278143350002));
#67239=CARTESIAN_POINT('Ctrl Pts',(3.9838711072068,-0.406412410338816,7.01680070230257));
#67240=CARTESIAN_POINT('Ctrl Pts',(3.95081981388232,0.781363864886133,6.98499346102357));
#67241=CARTESIAN_POINT('Ctrl Pts',(3.91776852055784,1.88928998221405,6.67122913484938));
#67242=CARTESIAN_POINT('Ctrl Pts',(3.88471722723336,2.99721609954198,6.35746480867518));
#67243=CARTESIAN_POINT('Ctrl Pts',(3.85166593390889,4.02529205897287,5.7617433976058));
#67244=CARTESIAN_POINT('Ctrl Pts',(3.81861464058441,4.8484500327254,4.95653579488448));
#67245=CARTESIAN_POINT('Ctrl Pts',(3.78556334725993,5.67160800647792,4.15132819216316));
#67246=CARTESIAN_POINT('Ctrl Pts',(3.75251205393545,6.28984799455207,3.13663439778989));
#67247=CARTESIAN_POINT('Ctrl Pts',(3.71946076061097,6.62795966589096,2.03589426897532));
#67248=CARTESIAN_POINT('Ctrl Pts',(3.68640946728649,6.96607133722985,0.93515414016076));
#67249=CARTESIAN_POINT('Ctrl Pts',(3.65335817396201,7.02405469183348,-0.251632323095101));
#67250=CARTESIAN_POINT('Ctrl Pts',(3.62030688063753,6.79485592013532,-1.38008979082198));
#67251=CARTESIAN_POINT('Ctrl Pts',(3.58725558731305,6.56565714843717,-2.50854725854886));
#67252=CARTESIAN_POINT('Ctrl Pts',(3.55420429398857,6.04927625043723,-3.57867573074675));
#67253=CARTESIAN_POINT('Ctrl Pts',(3.52115300066409,5.30853216176314,-4.4602915929574));
#67254=CARTESIAN_POINT('Ctrl Pts',(3.48810170733961,4.56778807308904,-5.34190745516806));
#67255=CARTESIAN_POINT('Ctrl Pts',(3.45505041401514,3.60268079374078,-6.03501070739147));
#67256=CARTESIAN_POINT('Ctrl Pts',(3.42199912069066,2.53061786614165,-6.45528372900915));
#67257=CARTESIAN_POINT('Ctrl Pts',(3.38894782736618,1.45855493854251,-6.87555675062682));
#67258=CARTESIAN_POINT('Ctrl Pts',(3.3558965340417,0.279536362692491,-7.02299954163876));
#67259=CARTESIAN_POINT('Ctrl Pts',(3.32284524071722,-0.863007512958787,
-6.87967534401792));
#67260=CARTESIAN_POINT('Ctrl Pts',(3.28979394739274,-2.00555138861006,-6.73635114639708));
#67261=CARTESIAN_POINT('Ctrl Pts',(3.25674265406826,-3.1116205640626,-6.30225996014347));
#67262=CARTESIAN_POINT('Ctrl Pts',(3.22369136074378,-4.04665915483455,-5.63020998641329));
#67263=CARTESIAN_POINT('Ctrl Pts',(3.19064006741931,-4.98169774560653,-4.95816001268309));
#67264=CARTESIAN_POINT('Ctrl Pts',(3.15758877409483,-5.74570575169792,-4.04815125147631));
#67265=CARTESIAN_POINT('Ctrl Pts',(3.12453748077035,-6.24573982447149,-3.01088838243881));
#67266=CARTESIAN_POINT('Ctrl Pts',(3.09474887504899,-6.6964125922468,-2.07601983336822));
#67267=CARTESIAN_POINT('Ctrl Pts',(3.06496026932763,-6.93265588658114,-1.03778111061277));
#67268=CARTESIAN_POINT('Ctrl Pts',(3.03517166360627,-6.93344508439855,0.000110442622268392));
#67269=CARTESIAN_POINT('Ctrl Pts',(2.85582833639373,-6.93334073279147,0.000139834461613099));
#67270=CARTESIAN_POINT('Ctrl Pts',(2.88445154278377,-6.93243691051637,-0.997190444968419));
#67271=CARTESIAN_POINT('Ctrl Pts',(2.9130747491738,-6.71487431850579,-1.99490226058369));
#67272=CARTESIAN_POINT('Ctrl Pts',(2.94169795556383,-6.29768542292325,-2.90066766648421));
#67273=CARTESIAN_POINT('Ctrl Pts',(2.97474924888831,-5.81595628427528,-3.94655741432206));
#67274=CARTESIAN_POINT('Ctrl Pts',(3.00780054221279,-5.06805775038753,-4.86985149300039));
#67275=CARTESIAN_POINT('Ctrl Pts',(3.04085183553727,-4.14497341519097,-5.55822903314057));
#67276=CARTESIAN_POINT('Ctrl Pts',(3.07390312886175,-3.2218890799944,-6.24660657328076));
#67277=CARTESIAN_POINT('Ctrl Pts',(3.10695442218623,-2.12361894348903,-6.7000675748828));
#67278=CARTESIAN_POINT('Ctrl Pts',(3.14000571551071,-0.983770118937337,
-6.86344745376349));
#67279=CARTESIAN_POINT('Ctrl Pts',(3.17305700883518,0.156078705614327,-7.02682733264417));
#67280=CARTESIAN_POINT('Ctrl Pts',(3.20610830215966,1.33750621821232,-6.90012608880352));
#67281=CARTESIAN_POINT('Ctrl Pts',(3.23915959548414,2.41678901762657,-6.49875722286713));
#67282=CARTESIAN_POINT('Ctrl Pts',(3.27221088880862,3.49607181704081,-6.09738835693074));
#67283=CARTESIAN_POINT('Ctrl Pts',(3.3052621821331,4.47320990327132,-5.4213518688986));
#67284=CARTESIAN_POINT('Ctrl Pts',(3.33831347545757,5.2293321583483,-4.55288916789631));
#67285=CARTESIAN_POINT('Ctrl Pts',(3.37136476878205,5.98545441342532,-3.68442646689396));
#67286=CARTESIAN_POINT('Ctrl Pts',(3.40441606210653,6.52056083734878,-2.62353755292144));
#67287=CARTESIAN_POINT('Ctrl Pts',(3.43746735543101,6.76955449065496,-1.49928202668714));
#67288=CARTESIAN_POINT('Ctrl Pts',(3.47051864875549,7.01854814396113,-0.375026500452875));
#67289=CARTESIAN_POINT('Ctrl Pts',(3.50356994207997,6.98142902665003,0.812595638043157));
#67290=CARTESIAN_POINT('Ctrl Pts',(3.53662123540445,6.66271276556983,1.91910739693977));
#67291=CARTESIAN_POINT('Ctrl Pts',(3.56967252872893,6.34399650448963,3.02561915583639));
#67292=CARTESIAN_POINT('Ctrl Pts',(3.60272382205341,5.74368309964034,4.05102053513359));
#67293=CARTESIAN_POINT('Ctrl Pts',(3.63577511537789,4.93480207117444,4.87056907515219));
#67294=CARTESIAN_POINT('Ctrl Pts',(3.66882640870237,4.12592104270852,5.69011761517081));
#67295=CARTESIAN_POINT('Ctrl Pts',(3.70187770202685,3.10847239062599,6.3038133159108));
#67296=CARTESIAN_POINT('Ctrl Pts',(3.73492899535132,2.0062311068846,6.63699866982526));
#67297=CARTESIAN_POINT('Ctrl Pts',(3.7679802886758,0.903989823143268,6.9701840237397));
#67298=CARTESIAN_POINT('Ctrl Pts',(3.80103158200028,-0.283044092256907,
7.02285903082863));
#67299=CARTESIAN_POINT('Ctrl Pts',(3.83408287532476,-1.41046520618992,6.7886156541341));
#67300=CARTESIAN_POINT('Ctrl Pts',(3.86713416864924,-2.53788632012296,6.55437227743956));
#67301=CARTESIAN_POINT('Ctrl Pts',(3.90018546197372,-3.60569463258884,6.03321051696155));
#67302=CARTESIAN_POINT('Ctrl Pts',(3.9332367552982,-4.48398878192539,5.28853091143765));
#67303=CARTESIAN_POINT('Ctrl Pts',(3.96628804862267,-5.36228293126194,4.54385130591376));
#67304=CARTESIAN_POINT('Ctrl Pts',(3.99933934194715,-6.05106291746916,3.57565385534399));
#67305=CARTESIAN_POINT('Ctrl Pts',(4.03239063527163,-6.4665370553702,2.50172202864973));
#67306=CARTESIAN_POINT('Ctrl Pts',(4.056869868979,-6.77425537734927,1.70632113727346));
#67307=CARTESIAN_POINT('Ctrl Pts',(4.08134910268637,-6.93205091289159,0.852919319868787));
#67308=CARTESIAN_POINT('Ctrl Pts',(4.10582833639373,-6.93289696494239,-0.00017817873250203));
#67309=CARTESIAN_POINT('Origin',(-3.775,0.,0.));
#67310=CARTESIAN_POINT('',(5.53517166360628,-6.93272540515737,0.000163154062267218));
#67311=CARTESIAN_POINT('',(5.35582833639373,-6.93262081645922,0.000142250729870931));
#67312=CARTESIAN_POINT('',(-3.775,-6.933,-8.4904762584886E-16));
#67313=CARTESIAN_POINT('Ctrl Pts',(5.53517166360628,-6.93272540515737,0.000163154062267218));
#67314=CARTESIAN_POINT('Ctrl Pts',(5.52485797578179,-6.93303262791813,0.359618454679378));
#67315=CARTESIAN_POINT('Ctrl Pts',(5.51454428795731,-6.9055597149569,0.719026621772691));
#67316=CARTESIAN_POINT('Ctrl Pts',(5.50423060013282,-6.8498977578155,1.07401516670493));
#67317=CARTESIAN_POINT('Ctrl Pts',(5.47117930680834,-6.67152318377348,2.21161315542136));
#67318=CARTESIAN_POINT('Ctrl Pts',(5.43812801348386,-6.20366145138839,3.30382387055088));
#67319=CARTESIAN_POINT('Ctrl Pts',(5.40507672015939,-5.50319805732819,4.21776921297274));
#67320=CARTESIAN_POINT('Ctrl Pts',(5.37202542683491,-4.802734663268,5.1317145553946));
#67321=CARTESIAN_POINT('Ctrl Pts',(5.33897413351042,-3.86966960753269,5.86739452510881));
#67322=CARTESIAN_POINT('Ctrl Pts',(5.30592284018595,-2.817528404932,6.33531613923483));
#67323=CARTESIAN_POINT('Ctrl Pts',(5.27287154686147,-1.7653872023313,6.80323775336085));
#67324=CARTESIAN_POINT('Ctrl Pts',(5.23982025353699,-0.59416985286522,7.00340101189867));
#67325=CARTESIAN_POINT('Ctrl Pts',(5.20676896021251,0.553650582751667,6.91145342449458));
#67326=CARTESIAN_POINT('Ctrl Pts',(5.17371766688803,1.70147101836855,6.81950583709048));
#67327=CARTESIAN_POINT('Ctrl Pts',(5.14066637356355,2.82589454013615,6.4354474037445));
#67328=CARTESIAN_POINT('Ctrl Pts',(5.10761508023908,3.79012815577094,5.80600084257848));
#67329=CARTESIAN_POINT('Ctrl Pts',(5.0745637869146,4.75436177140573,5.17655428141245));
#67330=CARTESIAN_POINT('Ctrl Pts',(5.04151249359012,5.55840548090767,4.30171959242633));
#67331=CARTESIAN_POINT('Ctrl Pts',(5.00846120026564,6.10444769783574,3.28792187076906));
#67332=CARTESIAN_POINT('Ctrl Pts',(4.97540990694116,6.65048991476382,2.27412414911179));
#67333=CARTESIAN_POINT('Ctrl Pts',(4.94235861361668,6.9385306391181,1.12136339478331));
#67334=CARTESIAN_POINT('Ctrl Pts',(4.9093073202922,6.93352791278986,-0.0301240709127577));
#67335=CARTESIAN_POINT('Ctrl Pts',(4.87625602696772,6.92852518646162,-1.18161153660883));
#67336=CARTESIAN_POINT('Ctrl Pts',(4.84320473364324,6.63047900945084,-2.3318257136725));
#67337=CARTESIAN_POINT('Ctrl Pts',(4.81015344031876,6.07564797737095,-3.34084052937886));
#67338=CARTESIAN_POINT('Ctrl Pts',(4.77710214699428,5.52081694529103,-4.34985534508526));
#67339=CARTESIAN_POINT('Ctrl Pts',(4.74405085366981,4.70920105814205,-5.21767079943428));
#67340=CARTESIAN_POINT('Ctrl Pts',(4.71099956034533,3.73953497146248,-5.83871504720933));
#67341=CARTESIAN_POINT('Ctrl Pts',(4.67794826702085,2.76986888478297,-6.45975929498434));
#67342=CARTESIAN_POINT('Ctrl Pts',(4.64489697369637,1.64215259857284,-6.83403233618537));
#67343=CARTESIAN_POINT('Ctrl Pts',(4.61184568037189,0.493575574722173,-6.91600302692225));
#67344=CARTESIAN_POINT('Ctrl Pts',(4.57879438704741,-0.655001449128527,
-6.99797371765914));
#67345=CARTESIAN_POINT('Ctrl Pts',(4.54574309372293,-1.82443921061986,-6.78764205793191));
#67346=CARTESIAN_POINT('Ctrl Pts',(4.51269180039845,-2.87247297018407,-6.31059536157588));
#67347=CARTESIAN_POINT('Ctrl Pts',(4.47964050707397,-3.92050672974827,-5.83354866521985));
#67348=CARTESIAN_POINT('Ctrl Pts',(4.4465892137495,-4.84713648738534,-5.08978693223501));
#67349=CARTESIAN_POINT('Ctrl Pts',(4.41353792042502,-5.53963553902198,-4.16979051602946));
#67350=CARTESIAN_POINT('Ctrl Pts',(4.38048662710054,-6.23213459065862,-3.2497940998239));
#67351=CARTESIAN_POINT('Ctrl Pts',(4.34743533377606,-6.69050293629485,-2.15356300039762));
#67352=CARTESIAN_POINT('Ctrl Pts',(4.31438404045158,-6.85897902342132,-1.01445627178106));
#67353=CARTESIAN_POINT('Ctrl Pts',(4.30464658150315,-6.90861487173992,-0.678856545050398));
#67354=CARTESIAN_POINT('Ctrl Pts',(4.29490912255471,-6.93308838271965,-0.339535259659124));
#67355=CARTESIAN_POINT('Ctrl Pts',(4.28517166360628,-6.93277727477507,-0.000169494543622584));
#67356=CARTESIAN_POINT('Ctrl Pts',(4.10582833639373,-6.93289696494239,-0.00017817873250203));
#67357=CARTESIAN_POINT('Ctrl Pts',(4.11440039601084,-6.9331932327384,-0.298913127082497));
#67358=CARTESIAN_POINT('Ctrl Pts',(4.12297245562795,-6.91424376032206,-0.597610758708019));
#67359=CARTESIAN_POINT('Ctrl Pts',(4.13154451524506,-6.87574682128536,-0.893767446093456));
#67360=CARTESIAN_POINT('Ctrl Pts',(4.16459580856954,-6.72731415970462,-2.03565889132375));
#67361=CARTESIAN_POINT('Ctrl Pts',(4.19764710189402,-6.28828054694824,-3.13977557896555));
#67362=CARTESIAN_POINT('Ctrl Pts',(4.2306983952185,-5.61205544221947,-4.07179914905405));
#67363=CARTESIAN_POINT('Ctrl Pts',(4.26374968854298,-4.93583033749073,-5.0038227191425));
#67364=CARTESIAN_POINT('Ctrl Pts',(4.29680098186746,-4.02241374078962,-5.76375317167767));
#67365=CARTESIAN_POINT('Ctrl Pts',(4.32985227519194,-2.98292490212011,-6.25914320221618));
#67366=CARTESIAN_POINT('Ctrl Pts',(4.36290356851642,-1.94343606345054,-6.75453323275473));
#67367=CARTESIAN_POINT('Ctrl Pts',(4.3959548618409,-0.777874982812544,-6.98538284129659));
#67368=CARTESIAN_POINT('Ctrl Pts',(4.42900615516538,0.371965125420105,-6.92360863606738));
#67369=CARTESIAN_POINT('Ctrl Pts',(4.46205744848986,1.52180523365269,-6.86183443083818));
#67370=CARTESIAN_POINT('Ctrl Pts',(4.49510874181433,2.65592436947993,-6.50743641183794));
#67371=CARTESIAN_POINT('Ctrl Pts',(4.52816003513881,3.6363543084025,-5.90352792257827));
#67372=CARTESIAN_POINT('Ctrl Pts',(4.56121132846329,4.6167842473251,-5.29961943331858));
#67373=CARTESIAN_POINT('Ctrl Pts',(4.59426262178776,5.44352498934302,-4.44620047379944));
#67374=CARTESIAN_POINT('Ctrl Pts',(4.62731391511224,6.01600159733496,-3.44709144037499));
#67375=CARTESIAN_POINT('Ctrl Pts',(4.66036520843672,6.5884782053269,-2.44798240695053));
#67376=CARTESIAN_POINT('Ctrl Pts',(4.69341650176121,6.90669067929286,-1.30318329962076));
#67377=CARTESIAN_POINT('Ctrl Pts',(4.72646779508568,6.93192774311814,-0.15196159380743));
#67378=CARTESIAN_POINT('Ctrl Pts',(4.75951908841016,6.95716480694343,0.999260112005898));
#67379=CARTESIAN_POINT('Ctrl Pts',(4.79257038173464,6.68942646062803,2.15690441630278));
#67380=CARTESIAN_POINT('Ctrl Pts',(4.82562167505912,6.16128367556587,3.18014120963901));
#67381=CARTESIAN_POINT('Ctrl Pts',(4.8586729683836,5.63314089050373,4.20337800297521));
#67382=CARTESIAN_POINT('Ctrl Pts',(4.89172426170808,4.84459366669486,5.09220728535076));
#67383=CARTESIAN_POINT('Ctrl Pts',(4.92477555503256,3.89157064504942,5.73850089200341));
#67384=CARTESIAN_POINT('Ctrl Pts',(4.95782684835704,2.93854762340393,6.38479449865609));
#67385=CARTESIAN_POINT('Ctrl Pts',(4.99087814168152,1.82104880392187,6.78855242958583));
#67386=CARTESIAN_POINT('Ctrl Pts',(5.023929435006,0.675020437465834,6.90065662929625));
#67387=CARTESIAN_POINT('Ctrl Pts',(5.05698072833047,-0.471007928990167,
7.01276082900667));
#67388=CARTESIAN_POINT('Ctrl Pts',(5.09003202165495,-1.64556584242014,6.83321129749778));
#67389=CARTESIAN_POINT('Ctrl Pts',(5.12308331497943,-2.70576545644266,6.3838505851852));
#67390=CARTESIAN_POINT('Ctrl Pts',(5.15613460830391,-3.7659650704652,5.93448987287263));
#67391=CARTESIAN_POINT('Ctrl Pts',(5.18918590162839,-4.71180638508021,5.21531797975642));
#67392=CARTESIAN_POINT('Ctrl Pts',(5.22223719495287,-5.42822589358189,4.31382396725108));
#67393=CARTESIAN_POINT('Ctrl Pts',(5.25528848827735,-6.14464540208356,3.41232995474574));
#67394=CARTESIAN_POINT('Ctrl Pts',(5.28833978160182,-6.63164310447184,2.32851382285121));
#67395=CARTESIAN_POINT('Ctrl Pts',(5.3213910749263,-6.82997404460943,1.19422406973633));
#67396=CARTESIAN_POINT('Ctrl Pts',(5.33287016208211,-6.89885661828612,0.800272438006842));
#67397=CARTESIAN_POINT('Ctrl Pts',(5.34434924923792,-6.93291872661601,0.400232419221871));
#67398=CARTESIAN_POINT('Ctrl Pts',(5.35582833639373,-6.93262081645922,0.000142250729870931));
#67399=CARTESIAN_POINT('Origin',(-15.9277445817596,0.,0.));
#67400=CARTESIAN_POINT('',(5.94725541824039,-6.21900367460334,0.000146357406630245));
#67401=CARTESIAN_POINT('',(6.,-6.21925,-5.19709976349859E-13));
#67402=CARTESIAN_POINT('',(-15.9277445817596,-6.21925,-5.19709976349859E-13));
#67403=CARTESIAN_POINT('',(6.,-6.00216240205941,-1.62981090527758));
#67404=CARTESIAN_POINT('Ctrl Pts',(5.94725541824039,-6.21900367460334,0.000146357406630437));
#67405=CARTESIAN_POINT('Ctrl Pts',(5.96483694549359,-6.21853387481332,-0.54952653898896));
#67406=CARTESIAN_POINT('Ctrl Pts',(5.9824184727468,-6.14564776188864,-1.09932230145161));
#67407=CARTESIAN_POINT('Ctrl Pts',(6.,-6.00216240205941,-1.62981090527758));
#67408=CARTESIAN_POINT('Origin',(6.,0.,0.));
#67409=CARTESIAN_POINT('Origin',(-15.9277445817596,0.,0.));
#67410=CARTESIAN_POINT('',(4.69725541824038,-6.21905020426149,-0.000152045137862922));
#67411=CARTESIAN_POINT('',(4.94374458175965,-6.21890985327621,0.000127606064774521));
#67412=CARTESIAN_POINT('',(-15.9277445817596,-6.21925,-5.19709976349859E-13));
#67413=CARTESIAN_POINT('Ctrl Pts',(4.69725541824038,-6.21905020426149,-0.00015204513786251));
#67414=CARTESIAN_POINT('Ctrl Pts',(4.70699287718881,-6.21932928374862,-0.304580219765699));
#67415=CARTESIAN_POINT('Ctrl Pts',(4.74978162946173,-6.1228582182286,-1.64213599516804));
#67416=CARTESIAN_POINT('Ctrl Pts',(4.82562167505912,-5.17935896716503,-3.89860337811007));
#67417=CARTESIAN_POINT('Ctrl Pts',(4.92477555503255,-2.68565835263266,-5.90017852214549));
#67418=CARTESIAN_POINT('Ctrl Pts',(5.02392943500599,0.461475268377732,-6.46621278210156));
#67419=CARTESIAN_POINT('Ctrl Pts',(5.12308331497942,3.49633009875934,-5.45898750668426));
#67420=CARTESIAN_POINT('Ctrl Pts',(5.22223719495286,5.68051101877298,-3.1235650642522));
#67421=CARTESIAN_POINT('Ctrl Pts',(5.3213910749263,6.48259829111145,-0.0281650120223385));
#67422=CARTESIAN_POINT('Ctrl Pts',(5.42054495489973,5.70743720286374,3.07408826420326));
#67423=CARTESIAN_POINT('Ctrl Pts',(5.51969883487318,3.54363415642518,5.42840052706632));
#67424=CARTESIAN_POINT('Ctrl Pts',(5.6188527148466,0.51764065242096,6.46195977050514));
#67425=CARTESIAN_POINT('Ctrl Pts',(5.71800659482005,-2.63428210857727,5.92329021374989));
#67426=CARTESIAN_POINT('Ctrl Pts',(5.81716047479348,-5.14530108213061,3.94346431515829));
#67427=CARTESIAN_POINT('Ctrl Pts',(5.89357674926693,-6.11565852522162,1.67819078777056));
#67428=CARTESIAN_POINT('Ctrl Pts',(5.9369417304159,-6.21927926888502,0.322595856665736));
#67429=CARTESIAN_POINT('Ctrl Pts',(5.94725541824039,-6.21900367460334,0.000146357406630437));
#67430=CARTESIAN_POINT('',(6.,-3.49587713861109,5.14372565308808));
#67431=CARTESIAN_POINT('Origin',(6.,0.,0.));
#67432=CARTESIAN_POINT('Ctrl Pts',(4.94374458175965,-6.21890985327621,0.000127606064774174));
#67433=CARTESIAN_POINT('Ctrl Pts',(4.96531678792832,-6.21840763867658,-0.674341253668515));
#67434=CARTESIAN_POINT('Ctrl Pts',(5.01994028742146,-5.94150400537597,-2.38258228935399));
#67435=CARTESIAN_POINT('Ctrl Pts',(5.10761508023907,-4.40502769148852,-4.75611250736834));
#67436=CARTESIAN_POINT('Ctrl Pts',(5.20676896021251,-1.59561249292064,-6.28322342394515));
#67437=CARTESIAN_POINT('Ctrl Pts',(5.30592284018595,1.60200834941566,-6.28159039988369));
#67438=CARTESIAN_POINT('Ctrl Pts',(5.40507672015938,4.40988078716951,-4.75162981867586));
#67439=CARTESIAN_POINT('Ctrl Pts',(5.50423060013282,6.14475515867778,-2.06555128428737));
#67440=CARTESIAN_POINT('Ctrl Pts',(5.60338448010625,6.38468584605272,1.12303831208186));
#67441=CARTESIAN_POINT('Ctrl Pts',(5.7025383600797,5.07099150144849,4.03847901383656));
#67442=CARTESIAN_POINT('Ctrl Pts',(5.80169224005312,2.52389427730921,5.97115958776782));
#67443=CARTESIAN_POINT('Ctrl Pts',(5.90084612002658,-0.638069512693321,
6.45139792173227));
#67444=CARTESIAN_POINT('Ctrl Pts',(5.96694870667552,-2.64132982999147,5.72450942764096));
#67445=CARTESIAN_POINT('Ctrl Pts',(6.,-3.49587713861109,5.14372565308808));
#67446=CARTESIAN_POINT('Origin',(-15.9277445817596,0.,0.));
#67447=CARTESIAN_POINT('',(3.44725541824037,-6.21964926311058,9.90725915984747E-5));
#67448=CARTESIAN_POINT('',(3.69374458175965,-6.21915757236664,-0.000159835292970756));
#67449=CARTESIAN_POINT('',(-15.9277445817596,-6.21925,-5.19709976349859E-13));
#67450=CARTESIAN_POINT('Ctrl Pts',(3.44725541824037,-6.21964926311058,9.90725915984633E-5));
#67451=CARTESIAN_POINT('Ctrl Pts',(3.47704402396173,-6.21894131294095,-0.930941897040162));
#67452=CARTESIAN_POINT('Ctrl Pts',(3.53988392300757,-5.77188564316155,-2.89565589622528));
#67453=CARTESIAN_POINT('Ctrl Pts',(3.63577511537788,-3.78348001045424,-5.26404278768421));
#67454=CARTESIAN_POINT('Ctrl Pts',(3.73492899535132,-0.806880824200139,
-6.43224772498744));
#67455=CARTESIAN_POINT('Ctrl Pts',(3.83408287532476,2.36603621511411,-6.03545690802462));
#67456=CARTESIAN_POINT('Ctrl Pts',(3.93323675529819,4.96328565132639,-4.17021138600364));
#67457=CARTESIAN_POINT('Ctrl Pts',(4.03239063527163,6.35294463007415,-1.29033405986049));
#67458=CARTESIAN_POINT('Ctrl Pts',(4.13154451524507,6.1969026663707,1.90348753754495));
#67459=CARTESIAN_POINT('Ctrl Pts',(4.2306983952185,4.53312549379163,4.63418177409014));
#67460=CARTESIAN_POINT('Ctrl Pts',(4.32985227519194,1.76641783014358,6.23735805526417));
#67461=CARTESIAN_POINT('Ctrl Pts',(4.42900615516537,-1.430067500749,6.32295614497614));
#67462=CARTESIAN_POINT('Ctrl Pts',(4.52816003513881,-4.27861075952717,4.87014962817609));
#67463=CARTESIAN_POINT('Ctrl Pts',(4.61757645616381,-5.90863799280524,2.4914533890396));
#67464=CARTESIAN_POINT('Ctrl Pts',(4.67394158386433,-6.218382020398,0.728722713693786));
#67465=CARTESIAN_POINT('Ctrl Pts',(4.69725541824038,-6.21905020426149,-0.00015204513786251));
#67466=CARTESIAN_POINT('Ctrl Pts',(3.69374458175965,-6.21915757236664,-0.000159835292970999));
#67467=CARTESIAN_POINT('Ctrl Pts',(3.70231664137676,-6.21942333949345,-0.268140121968968));
#67468=CARTESIAN_POINT('Ctrl Pts',(3.74393999431834,-6.13688308256028,-1.56920955113219));
#67469=CARTESIAN_POINT('Ctrl Pts',(3.8186146405844,-5.24706894496936,-3.80698499626393));
#67470=CARTESIAN_POINT('Ctrl Pts',(3.91776852055784,-2.78892694192586,-5.85207260635886));
#67471=CARTESIAN_POINT('Ctrl Pts',(4.01692240053128,0.347773945463821,-6.47332376513164));
#67472=CARTESIAN_POINT('Ctrl Pts',(4.11607628050471,3.3998598111037,-5.51958517592035));
#67473=CARTESIAN_POINT('Ctrl Pts',(4.21523016047815,5.62474399967788,-3.2229058751893));
#67474=CARTESIAN_POINT('Ctrl Pts',(4.31438404045158,6.48110182257391,-0.142078593380259));
#67475=CARTESIAN_POINT('Ctrl Pts',(4.41353792042502,5.76057749963056,2.97331705330878));
#67476=CARTESIAN_POINT('Ctrl Pts',(4.51269180039846,3.63847783642259,5.36529088040279));
#67477=CARTESIAN_POINT('Ctrl Pts',(4.6118456803719,0.631119752015993,6.45186444679596));
#67478=CARTESIAN_POINT('Ctrl Pts',(4.71099956034532,-2.5297929710906,5.96866954249621));
#67479=CARTESIAN_POINT('Ctrl Pts',(4.81015344031878,-5.07519478672013,4.03326937102785));
#67480=CARTESIAN_POINT('Ctrl Pts',(4.88773511412354,-6.10064460767951,1.75112501397285));
#67481=CARTESIAN_POINT('Ctrl Pts',(4.93226549460384,-6.21917709368338,0.359028627324734));
#67482=CARTESIAN_POINT('Ctrl Pts',(4.94374458175965,-6.21890985327621,0.000127606064774174));
#67483=CARTESIAN_POINT('Origin',(-15.9277445817596,0.,0.));
#67484=CARTESIAN_POINT('',(2.19725541824037,-6.21871987332621,7.63675412254265E-6));
#67485=CARTESIAN_POINT('',(2.44374458175965,-6.21955565446608,0.000125438550603943));
#67486=CARTESIAN_POINT('',(-15.9277445817596,-6.21925,-5.19709976349859E-13));
#67487=CARTESIAN_POINT('Ctrl Pts',(2.19725541824037,-6.21871987332621,7.6367541225128E-6));
#67488=CARTESIAN_POINT('Ctrl Pts',(2.21404387741017,-6.21869739988965,-0.524940189831289));
#67489=CARTESIAN_POINT('Ctrl Pts',(2.26388362990446,-6.02349410963766,-2.08336464204647));
#67490=CARTESIAN_POINT('Ctrl Pts',(2.34677467572321,-4.7363647693443,-4.42625306910482));
#67491=CARTESIAN_POINT('Ctrl Pts',(2.44592855569665,-2.04432714095016,-6.15187727452525));
#67492=CARTESIAN_POINT('Ctrl Pts',(2.54508243567009,1.14510477831697,-6.38072115882848));
#67493=CARTESIAN_POINT('Ctrl Pts',(2.64423631564352,4.05592738512275,-5.05710594180675));
#67494=CARTESIAN_POINT('Ctrl Pts',(2.74339019561696,5.97992401621031,-2.50307335497727));
#67495=CARTESIAN_POINT('Ctrl Pts',(2.84254407559039,6.44897735278439,0.659968607828769));
#67496=CARTESIAN_POINT('Ctrl Pts',(2.94169795556383,5.3489645389414,3.6624371422857));
#67497=CARTESIAN_POINT('Ctrl Pts',(3.04085183553727,2.94752380269873,5.77381770517306));
#67498=CARTESIAN_POINT('Ctrl Pts',(3.1400057155107,-0.171063168266469,6.48040159654536));
#67499=CARTESIAN_POINT('Ctrl Pts',(3.23915959548414,-3.2480296756728,5.61027367300375));
#67500=CARTESIAN_POINT('Ctrl Pts',(3.33831347545758,-5.53473547337747,3.37514010076197));
#67501=CARTESIAN_POINT('Ctrl Pts',(3.40767874970965,-6.1923883436481,1.23702373810622));
#67502=CARTESIAN_POINT('Ctrl Pts',(3.44399273063725,-6.21972680350518,0.10207416528405));
#67503=CARTESIAN_POINT('Ctrl Pts',(3.44725541824037,-6.21964926311058,9.90725915984633E-5));
#67504=CARTESIAN_POINT('Ctrl Pts',(2.44374458175965,-6.21955565446608,0.000125438550604151));
#67505=CARTESIAN_POINT('Ctrl Pts',(2.47236778814968,-6.21874488038776,-0.894530026665607));
#67506=CARTESIAN_POINT('Ctrl Pts',(2.53404228786418,-5.7982231990549,-2.82298402379256));
#67507=CARTESIAN_POINT('Ctrl Pts',(2.62876808090318,-3.87540028951621,-5.19674319871096));
#67508=CARTESIAN_POINT('Ctrl Pts',(2.7279219608766,-0.919789494855471,-6.41707523428578));
#67509=CARTESIAN_POINT('Ctrl Pts',(2.82707584085005,2.25961035703773,-6.07610305308455));
#67510=CARTESIAN_POINT('Ctrl Pts',(2.92622972082348,4.88923651142507,-4.25678677087163));
#67511=CARTESIAN_POINT('Ctrl Pts',(3.02538360079692,6.32928870830338,-1.40177449124226));
#67512=CARTESIAN_POINT('Ctrl Pts',(3.12453748077035,6.22939555800606,1.79429603443556));
#67513=CARTESIAN_POINT('Ctrl Pts',(3.22369136074379,4.61386152810167,4.55380599903706));
#67514=CARTESIAN_POINT('Ctrl Pts',(3.32284524071722,1.87575355343092,6.20535380813579));
#67515=CARTESIAN_POINT('Ctrl Pts',(3.42199912069066,-1.31873397506443,6.34711020702708));
#67516=CARTESIAN_POINT('Ctrl Pts',(3.5211530006641,-4.19236740098541,4.94458520535987));
#67517=CARTESIAN_POINT('Ctrl Pts',(3.61173482102043,-5.88572982976849,2.56427622532341));
#67518=CARTESIAN_POINT('Ctrl Pts',(3.66926534805228,-6.21839862108777,0.76511156499223));
#67519=CARTESIAN_POINT('Ctrl Pts',(3.69374458175965,-6.21915757236664,-0.000159835292970999));
#67520=CARTESIAN_POINT('Origin',(-15.9277445817596,0.,0.));
#67521=CARTESIAN_POINT('',(0.947255418240376,-6.2196090925826,-0.000111756317149322));
#67522=CARTESIAN_POINT('',(1.19374458175965,-6.21872571138575,-2.6124611402778E-5));
#67523=CARTESIAN_POINT('',(-15.9277445817596,-6.21925,-5.19709976349859E-13));
#67524=CARTESIAN_POINT('Ctrl Pts',(0.947255418240376,-6.2196090925826,-0.000111756317148926));
#67525=CARTESIAN_POINT('Ctrl Pts',(0.95104373085862,-6.21970780557128,-0.11851744084317));
#67526=CARTESIAN_POINT('Ctrl Pts',(0.987883336801342,-6.18750070111082,
-1.26990484747838));
#67527=CARTESIAN_POINT('Ctrl Pts',(1.05777423606854,-5.50780972843139,-3.4189032533025));
#67528=CARTESIAN_POINT('Ctrl Pts',(1.15692811604198,-3.20345974553442,-5.63584182875872));
#67529=CARTESIAN_POINT('Ctrl Pts',(1.25608199601542,-0.119693124002174,
-6.48155390443623));
#67530=CARTESIAN_POINT('Ctrl Pts',(1.35523587598885,2.99319539066687,-5.75027380333636));
#67531=CARTESIAN_POINT('Ctrl Pts',(1.45438975596229,5.3778255610804,-3.61992537141806));
#67532=CARTESIAN_POINT('Ctrl Pts',(1.55354363593573,6.45400578832633,-0.608832279282255));
#67533=CARTESIAN_POINT('Ctrl Pts',(1.65269751590916,5.95989642342674,2.55039253489949));
#67534=CARTESIAN_POINT('Ctrl Pts',(1.7518513958826,4.01571657038161,5.08909499679543));
#67535=CARTESIAN_POINT('Ctrl Pts',(1.85100527585604,1.09449421965509,6.38959700319101));
#67536=CARTESIAN_POINT('Ctrl Pts',(1.95015915582947,-2.09302365948521,6.13548037409304));
#67537=CARTESIAN_POINT('Ctrl Pts',(2.04931303580291,-4.77129915855997,4.38857286592929));
#67538=CARTESIAN_POINT('Ctrl Pts',(2.13167845660654,-6.03177409386706,2.05047689312513));
#67539=CARTESIAN_POINT('Ctrl Pts',(2.1809925840857,-6.21874164314844,0.508520023583037));
#67540=CARTESIAN_POINT('Ctrl Pts',(2.19725541824037,-6.21871987332621,7.6367541225128E-6));
#67541=CARTESIAN_POINT('Ctrl Pts',(1.19374458175965,-6.21872571138575,-2.61246114025351E-5));
#67542=CARTESIAN_POINT('Ctrl Pts',(1.20936764159813,-6.21879733536845,-0.488532492648138));
#67543=CARTESIAN_POINT('Ctrl Pts',(1.25804199476107,-6.04166009992344,-2.0104452049757));
#67544=CARTESIAN_POINT('Ctrl Pts',(1.3397676412485,-4.81341550856989,-4.34233789785988));
#67545=CARTESIAN_POINT('Ctrl Pts',(1.43892152122194,-2.15211780533888,-6.11500255349699));
#67546=CARTESIAN_POINT('Ctrl Pts',(1.53807540119537,1.03280015818185,-6.39985867895463));
#67547=CARTESIAN_POINT('Ctrl Pts',(1.63722928116881,3.96643304506188,-5.12759945553204));
#67548=CARTESIAN_POINT('Ctrl Pts',(1.73638316114225,5.93501434493084,-2.60777146291548));
#67549=CARTESIAN_POINT('Ctrl Pts',(1.83553704111568,6.45957908194884,0.546539441742633));
#67550=CARTESIAN_POINT('Ctrl Pts',(1.93469092108912,5.41249821859067,3.56787476112659));
#67551=CARTESIAN_POINT('Ctrl Pts',(2.03384480106256,3.0485313934114,5.72112957559227));
#67552=CARTESIAN_POINT('Ctrl Pts',(2.13299868103599,-0.0571572825696857,
6.48240698524711));
#67553=CARTESIAN_POINT('Ctrl Pts',(2.23215256100943,-3.14893932616178,5.66648465960009));
#67554=CARTESIAN_POINT('Ctrl Pts',(2.33130644098286,-5.47456980244149,3.471880291071));
#67555=CARTESIAN_POINT('Ctrl Pts',(2.40183711456627,-6.18137274724245,1.30992838602558));
#67556=CARTESIAN_POINT('Ctrl Pts',(2.4393164948252,-6.21968108339441,0.13853104281368));
#67557=CARTESIAN_POINT('Ctrl Pts',(2.44374458175965,-6.21955565446608,0.000125438550604151));
#67558=CARTESIAN_POINT('Origin',(-15.9277445817596,0.,0.));
#67559=CARTESIAN_POINT('',(-0.30274458175963,-6.21909759658405,0.000156462538848766));
#67560=CARTESIAN_POINT('',(-0.0562554182403474,-6.21969263819396,-8.20542562895987E-5));
#67561=CARTESIAN_POINT('',(-15.9277445817596,-6.21925,-5.19709976349859E-13));
#67562=CARTESIAN_POINT('Ctrl Pts',(-0.30274458175963,-6.21909759658405,
0.000156462538848587));
#67563=CARTESIAN_POINT('Ctrl Pts',(-0.278905122368461,-6.21838583129681,
-0.745134927932084));
#67564=CARTESIAN_POINT('Ctrl Pts',(-0.222014369652814,-5.89839721002363,
-2.52430138060163));
#67565=CARTESIAN_POINT('Ctrl Pts',(-0.132072323612687,-4.2398747970514,
-4.9039095796491));
#67566=CARTESIAN_POINT('Ctrl Pts',(-0.0329184436392546,-1.37990584390503,
-6.33409246238185));
#67567=CARTESIAN_POINT('Ctrl Pts',(0.0662354363341833,1.81580061179276,
-6.22316122226147));
#67568=CARTESIAN_POINT('Ctrl Pts',(0.165389316307621,4.56971434284393,-4.59810594537058));
#67569=CARTESIAN_POINT('Ctrl Pts',(0.264543196281055,6.21179534442574,-1.85431013021464));
#67570=CARTESIAN_POINT('Ctrl Pts',(0.363697076254493,6.34251768011774,1.34064795432643));
#67571=CARTESIAN_POINT('Ctrl Pts',(0.462850956227929,4.93007599833982,4.20942016323384));
#67572=CARTESIAN_POINT('Ctrl Pts',(0.562004836201364,2.31812392215191,6.05402089041596));
#67573=CARTESIAN_POINT('Ctrl Pts',(0.6611587161748,-0.857838473773044,6.42565020935318));
#67574=CARTESIAN_POINT('Ctrl Pts',(0.76031259614824,-3.82508478370621,5.23388898024262));
#67575=CARTESIAN_POINT('Ctrl Pts',(0.855678163503428,-5.78385960214847,
2.86288430550369));
#67576=CARTESIAN_POINT('Ctrl Pts',(0.917992437534142,-6.21884657993534,
0.914517951143361));
#67577=CARTESIAN_POINT('Ctrl Pts',(0.947255418240376,-6.2196090925826,-0.000111756317148926));
#67578=CARTESIAN_POINT('Ctrl Pts',(-0.0562554182403475,-6.21969263819397,
-8.20542562896334E-5));
#67579=CARTESIAN_POINT('Ctrl Pts',(-0.0536325049534321,-6.21974623332796,
-0.0820593826459758));
#67580=CARTESIAN_POINT('Ctrl Pts',(-0.0179582983420387,-6.19815906612472,
-1.197003612836));
#67581=CARTESIAN_POINT('Ctrl Pts',(0.0507672015938321,-5.56703928211486,
-3.32158710689955));
#67582=CARTESIAN_POINT('Ctrl Pts',(0.149921081567268,-3.30200317851016,
-5.5786774675043));
#67583=CARTESIAN_POINT('Ctrl Pts',(0.249074961540705,-0.233574361216745,
-6.47844968299619));
#67584=CARTESIAN_POINT('Ctrl Pts',(0.348228841514139,2.89168418329416,-5.8019849932086));
#67585=CARTESIAN_POINT('Ctrl Pts',(0.447382721487577,5.31338253190132,-3.71387039986819));
#67586=CARTESIAN_POINT('Ctrl Pts',(0.546536601461015,6.44231022572788,-0.722153884441094));
#67587=CARTESIAN_POINT('Ctrl Pts',(0.645690481434449,6.00379391212401,2.44526602603354));
#67588=CARTESIAN_POINT('Ctrl Pts',(0.744844361407886,4.10452664743683,5.01774135222336));
#67589=CARTESIAN_POINT('Ctrl Pts',(0.843998241381322,1.20660898072922,6.36937689613002));
#67590=CARTESIAN_POINT('Ctrl Pts',(0.943152121354761,-1.9848822566212,6.17131345052912));
#67591=CARTESIAN_POINT('Ctrl Pts',(1.04230600132819,-4.69344241962331,4.47174077189317));
#67592=CARTESIAN_POINT('Ctrl Pts',(1.12583682146316,-6.0132230713283,2.12339252898828));
#67593=CARTESIAN_POINT('Ctrl Pts',(1.17631634827365,-6.21864581157698,0.544924936804922));
#67594=CARTESIAN_POINT('Ctrl Pts',(1.19374458175965,-6.21872571138575,-2.61246114025351E-5));
#67595=CARTESIAN_POINT('Origin',(-15.9277445817596,0.,0.));
#67596=CARTESIAN_POINT('',(-1.55274458175964,-6.21895806039946,-0.000138248926431941));
#67597=CARTESIAN_POINT('',(-1.30625541824035,-6.2189953734855,0.000144753730515756));
#67598=CARTESIAN_POINT('',(-15.9277445817596,-6.21925,-5.19709976349859E-13));
#67599=CARTESIAN_POINT('Ctrl Pts',(-1.55274458175964,-6.21895806039946,
-0.000138248926431564));
#67600=CARTESIAN_POINT('Ctrl Pts',(-1.54190526892002,-6.21923430388303,
-0.339028765878233));
#67601=CARTESIAN_POINT('Ctrl Pts',(-1.49801466275593,-6.10897986203804,
-1.71108823079692));
#67602=CARTESIAN_POINT('Ctrl Pts',(-1.42107276326736,-5.11386949628186,
-3.98411925462125));
#67603=CARTESIAN_POINT('Ctrl Pts',(-1.32191888329392,-2.58725738181136,
-5.9439857587572));
#67604=CARTESIAN_POINT('Ctrl Pts',(-1.22276500332049,0.568846473464286,
-6.45765291337906));
#67605=CARTESIAN_POINT('Ctrl Pts',(-1.12361112334705,3.58654733901449,-5.40014311338634));
#67606=CARTESIAN_POINT('Ctrl Pts',(-1.02445724337361,5.73162457469774,-3.02875340606772));
#67607=CARTESIAN_POINT('Ctrl Pts',(-0.925303363400179,6.4821709235304,0.0795460758479203));
#67608=CARTESIAN_POINT('Ctrl Pts',(-0.826149483426742,5.65557497197356,
3.16849162795677));
#67609=CARTESIAN_POINT('Ctrl Pts',(-0.726995603453303,3.45295135521813,
5.4865284468909));
#67610=CARTESIAN_POINT('Ctrl Pts',(-0.627841723479869,0.410208632109992,
6.46966740553085));
#67611=CARTESIAN_POINT('Ctrl Pts',(-0.528687843506432,-2.73233975692668,
5.87870622779908));
#67612=CARTESIAN_POINT('Ctrl Pts',(-0.429533963532995,-5.21009718927287,
3.85742851370921));
#67613=CARTESIAN_POINT('Ctrl Pts',(-0.354219542950729,-6.1292667586287,
1.60924393406421));
#67614=CARTESIAN_POINT('Ctrl Pts',(-0.31195641569294,-6.21937263065751,
0.288145397534895));
#67615=CARTESIAN_POINT('Ctrl Pts',(-0.30274458175963,-6.21909759658405,
0.000156462538848587));
#67616=CARTESIAN_POINT('Ctrl Pts',(-1.30625541824035,-6.2189953734855,0.000144753730515756));
#67617=CARTESIAN_POINT('Ctrl Pts',(-1.28358135818052,-6.21838497526395,
-0.708746276277476));
#67618=CARTESIAN_POINT('Ctrl Pts',(-1.2278560047962,-5.92090099563265,-2.4514656171939));
#67619=CARTESIAN_POINT('Ctrl Pts',(-1.1390793580874,-4.32539601471359,-4.82864542011847));
#67620=CARTESIAN_POINT('Ctrl Pts',(-1.03992547811397,-1.49100115648436,
-6.30886541532577));
#67621=CARTESIAN_POINT('Ctrl Pts',(-0.940771598140529,1.70616120997042,
-6.25410914542779));
#67622=CARTESIAN_POINT('Ctrl Pts',(-0.841617718167091,4.48820662760173,
-4.67769906527593));
#67623=CARTESIAN_POINT('Ctrl Pts',(-0.742463838193658,6.17825052154845,
-1.96318307101446));
#67624=CARTESIAN_POINT('Ctrl Pts',(-0.643309958220219,6.36509736085303,
1.22898448492769));
#67625=CARTESIAN_POINT('Ctrl Pts',(-0.544156078246782,5.00328644146473,
4.12213440610403));
#67626=CARTESIAN_POINT('Ctrl Pts',(-0.445002198273347,2.42415268673505,
6.01234987577457));
#67627=CARTESIAN_POINT('Ctrl Pts',(-0.34584831829991,-0.744788678740318,
6.43973268865655));
#67628=CARTESIAN_POINT('Ctrl Pts',(-0.246694438326474,-3.73251949855906,
5.3002986208522));
#67629=CARTESIAN_POINT('Ctrl Pts',(-0.150163471639955,-5.7570996405633,
2.93553207094277));
#67630=CARTESIAN_POINT('Ctrl Pts',(-0.0866837982779112,-6.21907088180063,
0.950935775860047));
#67631=CARTESIAN_POINT('Ctrl Pts',(-0.0562554182403475,-6.21969263819397,
-8.20542562896334E-5));
#67632=CARTESIAN_POINT('Origin',(-15.9277445817596,0.,0.));
#67633=CARTESIAN_POINT('',(-2.80274458175963,-6.21971960642536,6.88125055054123E-5));
#67634=CARTESIAN_POINT('',(-2.55625541824035,-6.21905581821482,-0.000152655409548785));
#67635=CARTESIAN_POINT('',(-15.9277445817596,-6.21925,-5.19709976349859E-13));
#67636=CARTESIAN_POINT('Ctrl Pts',(-2.80274458175963,-6.21971960642536,
6.88125055054584E-5));
#67637=CARTESIAN_POINT('Ctrl Pts',(-2.7718541221471,-6.21917464400886,-0.965378845559518));
#67638=CARTESIAN_POINT('Ctrl Pts',(-2.70791236921008,-5.74627529022682,
-2.96432394809749));
#67639=CARTESIAN_POINT('Ctrl Pts',(-2.61091932294859,-3.69549673468289,
-5.3261779301854));
#67640=CARTESIAN_POINT('Ctrl Pts',(-2.51176544297515,-0.699898932068888,
-6.4447660116512));
#67641=CARTESIAN_POINT('Ctrl Pts',(-2.41261156300172,2.46598753228901,-5.99531258156246));
#67642=CARTESIAN_POINT('Ctrl Pts',(-2.31345768302828,5.03188777362273,-4.0871717475183));
#67643=CARTESIAN_POINT('Ctrl Pts',(-2.21430380305485,6.37350634262576,-1.18460303923088));
#67644=CARTESIAN_POINT('Ctrl Pts',(-2.11514992308141,6.16442120860435,2.00618509189823));
#67645=CARTESIAN_POINT('Ctrl Pts',(-2.01599604310798,4.45550375602798,4.708859069888));
#67646=CARTESIAN_POINT('Ctrl Pts',(-1.91684216313454,1.66254154035103,6.26584575988373));
#67647=CARTESIAN_POINT('Ctrl Pts',(-1.8176882831611,-1.53492475588388,6.29832306680283));
#67648=CARTESIAN_POINT('Ctrl Pts',(-1.71853440318767,-4.35893672810028,
4.79838911098967));
#67649=CARTESIAN_POINT('Ctrl Pts',(-1.63021983605385,-5.929620799522,2.42258033937297));
#67650=CARTESIAN_POINT('Ctrl Pts',(-1.5749565622445,-6.21839198070816,0.694318093502356));
#67651=CARTESIAN_POINT('Ctrl Pts',(-1.55274458175964,-6.21895806039946,
-0.000138248926431564));
#67652=CARTESIAN_POINT('Ctrl Pts',(-2.55625541824035,-6.21905581821482,
-0.000152655409548716));
#67653=CARTESIAN_POINT('Ctrl Pts',(-2.54658150473207,-6.21933458755579,
-0.302593383880689));
#67654=CARTESIAN_POINT('Ctrl Pts',(-2.50385629789931,-6.12364022690166,
-1.63815947675647));
#67655=CARTESIAN_POINT('Ctrl Pts',(-2.42807979774207,-5.18309236738467,
-3.8936385025436));
#67656=CARTESIAN_POINT('Ctrl Pts',(-2.32892591776863,-2.69131095073478,
-5.89760227921367));
#67657=CARTESIAN_POINT('Ctrl Pts',(-2.2297720377952,0.455278923448612,-6.46665202242975));
#67658=CARTESIAN_POINT('Ctrl Pts',(-2.13061815782176,3.49109732043444,-5.4623352859914));
#67659=CARTESIAN_POINT('Ctrl Pts',(-2.03146427784832,5.67751552051297,-3.12900699770163));
#67660=CARTESIAN_POINT('Ctrl Pts',(-1.93231039787489,6.48256781800243,-0.0343767702148776));
#67661=CARTESIAN_POINT('Ctrl Pts',(-1.83315651790145,5.71038124883349,3.06861748517184));
#67662=CARTESIAN_POINT('Ctrl Pts',(-1.73400263792802,3.54883239268839,5.42500285031601));
#67663=CARTESIAN_POINT('Ctrl Pts',(-1.63484875795458,0.523836128332554,
6.46145981864663));
#67664=CARTESIAN_POINT('Ctrl Pts',(-1.53569487798115,-2.62861189967033,
5.92581359462503));
#67665=CARTESIAN_POINT('Ctrl Pts',(-1.43654099800771,-5.14150644054926,
3.94838939304646));
#67666=CARTESIAN_POINT('Ctrl Pts',(-1.36006117809411,-6.11487336731535,
1.68217183221436));
#67667=CARTESIAN_POINT('Ctrl Pts',(-1.31663265150499,-6.21927473433717,
0.324582792537371));
#67668=CARTESIAN_POINT('Ctrl Pts',(-1.30625541824035,-6.2189953734855,0.000144753730515756));
#67669=CARTESIAN_POINT('Origin',(-15.9277445817596,0.,0.));
#67670=CARTESIAN_POINT('',(-4.05274458175964,-6.21873391926796,3.92816190650305E-5));
#67671=CARTESIAN_POINT('',(-3.80625541824035,-6.21964459475637,0.000100671161871041));
#67672=CARTESIAN_POINT('',(-15.9277445817596,-6.21925,-5.19709976349859E-13));
#67673=CARTESIAN_POINT('Ctrl Pts',(-4.05274458175964,-6.21873391926796,
3.92816190651624E-5));
#67674=CARTESIAN_POINT('Ctrl Pts',(-4.03485426869866,-6.21861039758982,
-0.559358110548367));
#67675=CARTESIAN_POINT('Ctrl Pts',(-3.9839126623132,-6.00567259807345,-2.15230124746295));
#67676=CARTESIAN_POINT('Ctrl Pts',(-3.89991976260326,-4.66216967103227,
-4.50433584655415));
#67677=CARTESIAN_POINT('Ctrl Pts',(-3.80076588262983,-1.94183273665795,
-6.18499418616455));
#67678=CARTESIAN_POINT('Ctrl Pts',(-3.70161200265638,1.25096112385931,-6.36081470620222));
#67679=CARTESIAN_POINT('Ctrl Pts',(-3.60245812268296,4.13939033126021,-4.98901945731978));
#67680=CARTESIAN_POINT('Ctrl Pts',(-3.50330424270952,6.02068664039774,-2.40337259661961));
#67681=CARTESIAN_POINT('Ctrl Pts',(-3.40415036273608,6.43712191918314,0.767025982361597));
#67682=CARTESIAN_POINT('Ctrl Pts',(-3.30499648276265,5.28737552962418,3.75080357640562));
#67683=CARTESIAN_POINT('Ctrl Pts',(-3.20584260278921,2.85118610976127,5.82199323492824));
#67684=CARTESIAN_POINT('Ctrl Pts',(-3.10668872281577,-0.278710136569954,
6.47666489173394));
#67685=CARTESIAN_POINT('Ctrl Pts',(-3.00753484284234,-3.34079491184971,
5.55553389126599));
#67686=CARTESIAN_POINT('Ctrl Pts',(-2.9083809628689,-5.59004876450166,3.28271568530374));
#67687=CARTESIAN_POINT('Ctrl Pts',(-2.840117542508,-6.20220553006854,1.16810013092565));
#67688=CARTESIAN_POINT('Ctrl Pts',(-2.80490541547158,-6.21975772735901,
0.0676033158062671));
#67689=CARTESIAN_POINT('Ctrl Pts',(-2.80274458175963,-6.21971960642536,
6.88125055054584E-5));
#67690=CARTESIAN_POINT('Ctrl Pts',(-3.80625541824035,-6.21964459475637,
0.000100671161871058));
#67691=CARTESIAN_POINT('Ctrl Pts',(-3.77653035795915,-6.21892929456546,
-0.928956203119842));
#67692=CARTESIAN_POINT('Ctrl Pts',(-3.71375400435347,-5.77334154366877,
-2.89169444538626));
#67693=CARTESIAN_POINT('Ctrl Pts',(-3.6179263574233,-3.78852249476445,-5.26041486804939));
#67694=CARTESIAN_POINT('Ctrl Pts',(-3.51877247744987,-0.813044105235338,
-6.43147157035411));
#67695=CARTESIAN_POINT('Ctrl Pts',(-3.41961859747643,2.36025169231589,-6.03772136043487));
#67696=CARTESIAN_POINT('Ctrl Pts',(-3.32046471750299,4.95928728793312,-4.17496549363898));
#67697=CARTESIAN_POINT('Ctrl Pts',(-3.22131083752956,6.35170524667332,-1.29642112629886));
#67698=CARTESIAN_POINT('Ctrl Pts',(-3.12215695755612,6.19872381031724,1.89754852394804));
#67699=CARTESIAN_POINT('Ctrl Pts',(-3.02300307758268,4.53756407304736,4.62983580273871));
#67700=CARTESIAN_POINT('Ctrl Pts',(-2.92384919760925,1.77239391631247,6.23566252155694));
#67701=CARTESIAN_POINT('Ctrl Pts',(-2.82469531763581,-1.42400791440103,
6.32432357940788));
#67702=CARTESIAN_POINT('Ctrl Pts',(-2.72554143766238,-4.27394200392325,
4.87424732901725));
#67703=CARTESIAN_POINT('Ctrl Pts',(-2.63606147119722,-5.90740787501663,
2.49542479295947));
#67704=CARTESIAN_POINT('Ctrl Pts',(-2.57963279805655,-6.21838216150297,
0.730706864401547));
#67705=CARTESIAN_POINT('Ctrl Pts',(-2.55625541824035,-6.21905581821482,
-0.000152655409548716));
#67706=CARTESIAN_POINT('Origin',(-15.9277445817596,0.,0.));
#67707=CARTESIAN_POINT('',(-5.30274458175963,-6.2195145656829,-0.000134032925609376));
#67708=CARTESIAN_POINT('',(-5.05625541824036,-6.21871962902234,5.79115600640723E-6));
#67709=CARTESIAN_POINT('',(-15.9277445817596,-6.21925,-5.19709976349859E-13));
#67710=CARTESIAN_POINT('Ctrl Pts',(-5.30274458175963,-6.2195145656829,-0.000134032925609619));
#67711=CARTESIAN_POINT('Ctrl Pts',(-5.29785441525021,-6.21965942650832,
-0.152985454681894));
#67712=CARTESIAN_POINT('Ctrl Pts',(-5.25991295541631,-6.17682437695265,
-1.3388366666538));
#67713=CARTESIAN_POINT('Ctrl Pts',(-5.18892020225794,-5.45024505989854,
-3.50994248487028));
#67714=CARTESIAN_POINT('Ctrl Pts',(-5.08976632228449,-3.10937916608465,
-5.68828872874475));
#67715=CARTESIAN_POINT('Ctrl Pts',(-4.99061244231106,-0.0119868756926444,
-6.48264789841751));
#67716=CARTESIAN_POINT('Ctrl Pts',(-4.89145856233762,3.08832187724368,-5.69974871749482));
#67717=CARTESIAN_POINT('Ctrl Pts',(-4.79230468236419,5.43722756980429,-3.53007419386704));
#67718=CARTESIAN_POINT('Ctrl Pts',(-4.69315080239075,6.46323053450655,-0.501516218948075));
#67719=CARTESIAN_POINT('Ctrl Pts',(-4.59399692241732,5.91669948346157,2.64906298197146));
#67720=CARTESIAN_POINT('Ctrl Pts',(-4.49484304244388,3.93060796044775,5.15511285243209));
#67721=CARTESIAN_POINT('Ctrl Pts',(-4.39568916247044,0.988181259944745,
6.40689981641197));
#67722=CARTESIAN_POINT('Ctrl Pts',(-4.29653528249701,-2.19467453196863,
6.09985829005677));
#67723=CARTESIAN_POINT('Ctrl Pts',(-4.19738140252357,-4.84355581429439,
4.30869290317386));
#67724=CARTESIAN_POINT('Ctrl Pts',(-4.11611783561112,-6.04866960539269,
1.98153115056918));
#67725=CARTESIAN_POINT('Ctrl Pts',(-4.06790556202314,-6.21883859657115,
0.474095425477252));
#67726=CARTESIAN_POINT('Ctrl Pts',(-4.05274458175964,-6.21873391926796,
3.92816190651624E-5));
#67727=CARTESIAN_POINT('Ctrl Pts',(-5.05625541824036,-6.21871962902234,
5.79115600630314E-6));
#67728=CARTESIAN_POINT('Ctrl Pts',(-5.03953050451071,-6.21870265207545,
-0.522955127194714));
#67729=CARTESIAN_POINT('Ctrl Pts',(-4.98975429745658,-6.02450268975374,
-2.07938874875887));
#67730=CARTESIAN_POINT('Ctrl Pts',(-4.90692679707797,-4.74060400838073,
-4.42171244124443));
#67731=CARTESIAN_POINT('Ctrl Pts',(-4.80777291710454,-2.05022118826812,
-6.14991547555801));
#67732=CARTESIAN_POINT('Ctrl Pts',(-4.7086190371311,1.13898997181236,-6.38181550355714));
#67733=CARTESIAN_POINT('Ctrl Pts',(-4.60946515715766,4.05107958026204,-5.06099017107475));
#67734=CARTESIAN_POINT('Ctrl Pts',(-4.51031127718423,5.9775227064379,-2.50880241775846));
#67735=CARTESIAN_POINT('Ctrl Pts',(-4.41115739721079,6.44960678792389,0.653788619124958));
#67736=CARTESIAN_POINT('Ctrl Pts',(-4.31200351723735,5.35247157449903,3.65730984762178));
#67737=CARTESIAN_POINT('Ctrl Pts',(-4.21284963726392,2.9530551606307,5.77099059916091));
#67738=CARTESIAN_POINT('Ctrl Pts',(-4.11369575729048,-0.164853293042968,
6.48056252721199));
#67739=CARTESIAN_POINT('Ctrl Pts',(-4.01454187731705,-3.24265217464831,
5.61338348517005));
#67740=CARTESIAN_POINT('Ctrl Pts',(-3.91538799734361,-5.53149871753584,
3.3804421626809));
#67741=CARTESIAN_POINT('Ctrl Pts',(-3.84595917765138,-6.19180447005486,
1.24099882977293));
#67742=CARTESIAN_POINT('Ctrl Pts',(-3.80958165128363,-6.2197246368188,0.104062097819437));
#67743=CARTESIAN_POINT('Ctrl Pts',(-3.80625541824035,-6.21964459475637,
0.000100671161871058));
#67744=CARTESIAN_POINT('Origin',(-15.9277445817596,0.,0.));
#67745=CARTESIAN_POINT('',(-6.55274458175964,-6.21920212302629,0.000160857331407452));
#67746=CARTESIAN_POINT('',(-6.30625541824035,-6.21961412857971,-0.000110289616846448));
#67747=CARTESIAN_POINT('',(-15.9277445817596,-6.21925,-5.19709976349859E-13));
#67748=CARTESIAN_POINT('Ctrl Pts',(-6.55274458175964,-6.21920212302629,
0.000160857331407242));
#67749=CARTESIAN_POINT('Ctrl Pts',(-6.52780326847729,-6.21841381317065,
-0.779540053029137));
#67750=CARTESIAN_POINT('Ctrl Pts',(-6.46981066187046,-5.87644188319325,
-2.59314334766061));
#67751=CARTESIAN_POINT('Ctrl Pts',(-6.37876676193917,-4.1578120641639,-4.97367734167979));
#67752=CARTESIAN_POINT('Ctrl Pts',(-6.27961288196573,-1.27447568419159,
-6.3561449944483));
#67753=CARTESIAN_POINT('Ctrl Pts',(-6.18045900199229,1.91894655066922,-6.19213304086084));
#67754=CARTESIAN_POINT('Ctrl Pts',(-6.08130512201886,4.64548017476219,-4.52154635118754));
#67755=CARTESIAN_POINT('Ctrl Pts',(-5.98215124204542,6.24174689048921,-1.75084642819241));
#67756=CARTESIAN_POINT('Ctrl Pts',(-5.88299736207198,6.31936759002112,1.44584256481697));
#67757=CARTESIAN_POINT('Ctrl Pts',(-5.78384348209855,4.85945679655365,4.29075134475004));
#67758=CARTESIAN_POINT('Ctrl Pts',(-5.68468960212512,2.21721758855159,6.09170038864876));
#67759=CARTESIAN_POINT('Ctrl Pts',(-5.58553572215167,-0.964480959434654,
6.41051042733211));
#67760=CARTESIAN_POINT('Ctrl Pts',(-5.48638184217824,-3.91151680923086,
5.16961349726944));
#67761=CARTESIAN_POINT('Ctrl Pts',(-5.39211812871423,-5.80845407019422,
2.7941582823786));
#67762=CARTESIAN_POINT('Ctrl Pts',(-5.33090570857469,-6.21868035194655,
0.880095354692622));
#67763=CARTESIAN_POINT('Ctrl Pts',(-5.30274458175963,-6.2195145656829,-0.000134032925609619));
#67764=CARTESIAN_POINT('Ctrl Pts',(-6.30625541824035,-6.21961412857971,
-0.000110289616846275));
#67765=CARTESIAN_POINT('Ctrl Pts',(-6.30253065106226,-6.21971023156661,
-0.116529554341081));
#67766=CARTESIAN_POINT('Ctrl Pts',(-6.26575459055969,-6.18809861508296,
-1.26592961559787));
#67767=CARTESIAN_POINT('Ctrl Pts',(-6.19592723673265,-5.51108332618975,
-3.41362385876426));
#67768=CARTESIAN_POINT('Ctrl Pts',(-6.0967733567592,-3.20885877105538,-5.63276953769212));
#67769=CARTESIAN_POINT('Ctrl Pts',(-5.99761947678577,-0.125903969293837,
-6.48143621953093));
#67770=CARTESIAN_POINT('Ctrl Pts',(-5.89846559681233,2.98768385311816,-5.75313935787656));
#67771=CARTESIAN_POINT('Ctrl Pts',(-5.7993117168389,5.37435431396556,-3.62507696267142));
#67772=CARTESIAN_POINT('Ctrl Pts',(-5.70015783686546,6.45341940219507,-0.615016501163695));
#67773=CARTESIAN_POINT('Ctrl Pts',(-5.60100395689203,5.96233756874898,2.5446803323042));
#67774=CARTESIAN_POINT('Ctrl Pts',(-5.50185007691858,4.02059130515946,5.08524461891535));
#67775=CARTESIAN_POINT('Ctrl Pts',(-5.40269619694516,1.10061649827017,6.38854526485231));
#67776=CARTESIAN_POINT('Ctrl Pts',(-5.30354231697171,-2.08714341586264,
6.1374831681197));
#67777=CARTESIAN_POINT('Ctrl Pts',(-5.20438843699829,-4.76709164052158,
4.39314290323005));
#67778=CARTESIAN_POINT('Ctrl Pts',(-5.12195947075449,-6.03078064977054,
2.0544529265738));
#67779=CARTESIAN_POINT('Ctrl Pts',(-5.07258179783519,-6.21873620142945,
0.510505193680209));
#67780=CARTESIAN_POINT('Ctrl Pts',(-5.05625541824036,-6.21871962902234,
5.79115600630314E-6));
#67781=CARTESIAN_POINT('Origin',(-15.9277445817596,0.,0.));
#67782=CARTESIAN_POINT('',(-7.80274458175964,-6.21887801778165,-0.000118905825011546));
#67783=CARTESIAN_POINT('',(-7.55625541824036,-6.21909175420816,0.000156006089798849));
#67784=CARTESIAN_POINT('',(-15.9277445817596,-6.21925,-5.19709976349859E-13));
#67785=CARTESIAN_POINT('Ctrl Pts',(-7.80274458175964,-6.21887801778165,
-0.000118905825011589));
#67786=CARTESIAN_POINT('Ctrl Pts',(-7.79080341502885,-6.21913509997953,
-0.373472596954706));
#67787=CARTESIAN_POINT('Ctrl Pts',(-7.74581095497358,-6.09449665494633,
-1.7800416268261));
#67788=CARTESIAN_POINT('Ctrl Pts',(-7.66776720159383,-5.0469682541968,-4.06853522796294));
#67789=CARTESIAN_POINT('Ctrl Pts',(-7.5686133216204,-2.48814211006943,-5.98615204452285));
#67790=CARTESIAN_POINT('Ctrl Pts',(-7.46945944164697,0.676060568781244,
-6.44731025834689));
#67791=CARTESIAN_POINT('Ctrl Pts',(-7.37030556167352,3.6757745704235,-5.3398079335753));
#67792=CARTESIAN_POINT('Ctrl Pts',(-7.2711516817001,5.78115554226751,-2.93310553102942));
#67793=CARTESIAN_POINT('Ctrl Pts',(-7.17199780172665,6.47995451274163,0.187235073758361));
#67794=CARTESIAN_POINT('Ctrl Pts',(-7.07284392175322,5.60215044586807,3.26202051524908));
#67795=CARTESIAN_POINT('Ctrl Pts',(-6.97369004177978,3.36131714919565,5.54314121077292));
#67796=CARTESIAN_POINT('Ctrl Pts',(-6.87453616180634,0.302659774207504,
6.47558989754003));
#67797=CARTESIAN_POINT('Ctrl Pts',(-6.77538228183291,-2.82963612993394,
5.83249747811505));
#67798=CARTESIAN_POINT('Ctrl Pts',(-6.67622840185946,-5.27346841781536,
3.77033132580544));
#67799=CARTESIAN_POINT('Ctrl Pts',(-6.60201583516839,-6.14225880651794,
1.54029520057943));
#67800=CARTESIAN_POINT('Ctrl Pts',(-6.56085456180177,-6.219458451838,0.253690362785901));
#67801=CARTESIAN_POINT('Ctrl Pts',(-6.55274458175964,-6.21920212302629,
0.000160857331407242));
#67802=CARTESIAN_POINT('Ctrl Pts',(-7.55625541824035,-6.21909175420816,
0.00015600608979878));
#67803=CARTESIAN_POINT('Ctrl Pts',(-7.53247950428934,-6.21838504441926,
-0.743150766835367));
#67804=CARTESIAN_POINT('Ctrl Pts',(-7.47565229701384,-5.89964322201078,
-2.52033047309439));
#67805=CARTESIAN_POINT('Ctrl Pts',(-7.38577379641388,-4.2445719758881,-4.89984448925031));
#67806=CARTESIAN_POINT('Ctrl Pts',(-7.28661991644044,-1.38597480405236,
-6.33276725609456));
#67807=CARTESIAN_POINT('Ctrl Pts',(-7.187466036467,1.80983647653362,-6.22489832893194));
#67808=CARTESIAN_POINT('Ctrl Pts',(-7.08831215649357,4.56530613428956,-4.6024827188757));
#67809=CARTESIAN_POINT('Ctrl Pts',(-6.98915827652013,6.21001560019695,-1.86026168122711));
#67810=CARTESIAN_POINT('Ctrl Pts',(-6.89000439654669,6.34379942025369,1.3345696658175));
#67811=CARTESIAN_POINT('Ctrl Pts',(-6.79085051657326,4.93410736951075,4.204694013061));
#67812=CARTESIAN_POINT('Ctrl Pts',(-6.69169663659982,2.3239240730231,6.05179677287292));
#67813=CARTESIAN_POINT('Ctrl Pts',(-6.59254275662638,-0.851680746854733,
6.42646926257087));
#67814=CARTESIAN_POINT('Ctrl Pts',(-6.49338887665295,-3.8200676843074,5.23755192476806));
#67815=CARTESIAN_POINT('Ctrl Pts',(-6.39795976385761,-5.78242031070725,
2.86684669246173));
#67816=CARTESIAN_POINT('Ctrl Pts',(-6.33558194438674,-6.21885747276121,
0.916503406659185));
#67817=CARTESIAN_POINT('Ctrl Pts',(-6.30625541824035,-6.21961412857971,
-0.000110289616846275));
#67818=CARTESIAN_POINT('Origin',(-15.9277445817596,0.,0.));
#67819=CARTESIAN_POINT('',(-9.05274458175964,-6.21976606909926,3.47298191171853E-5));
#67820=CARTESIAN_POINT('',(-8.80625541824036,-6.21896305789945,-0.000139202748639933));
#67821=CARTESIAN_POINT('',(-15.9277445817596,-6.21925,-5.19709976349859E-13));
#67822=CARTESIAN_POINT('Ctrl Pts',(-9.05274458175964,-6.21976606909926,
3.47298191171689E-5));
#67823=CARTESIAN_POINT('Ctrl Pts',(-9.02075226825592,-6.21945831059647,
-0.999828447687547));
#67824=CARTESIAN_POINT('Ctrl Pts',(-8.95570866142774,-5.71997014190296,
-3.03294779101907));
#67825=CARTESIAN_POINT('Ctrl Pts',(-8.85761376127506,-3.60649324070849,
-5.38684267124721));
#67826=CARTESIAN_POINT('Ctrl Pts',(-8.75845988130164,-0.592723818367459,
-6.45550508753466));
#67827=CARTESIAN_POINT('Ctrl Pts',(-8.65930600132819,2.56525806264267,-5.95351312521376));
#67828=CARTESIAN_POINT('Ctrl Pts',(-8.56015212135476,5.09910073940523,-4.00300376085795));
#67829=CARTESIAN_POINT('Ctrl Pts',(-8.46099824138133,6.39230851700605,-1.07854498443864));
#67830=CARTESIAN_POINT('Ctrl Pts',(-8.36184436140788,6.13023793520507,2.10832879736973));
#67831=CARTESIAN_POINT('Ctrl Pts',(-8.26269048143445,4.37665198407491,4.78223638796107));
#67832=CARTESIAN_POINT('Ctrl Pts',(-8.16353660146101,1.55820627228779,6.29260364817686));
#67833=CARTESIAN_POINT('Ctrl Pts',(-8.06438272148758,-1.63935826461956,
6.27195120678321));
#67834=CARTESIAN_POINT('Ctrl Pts',(-7.96522884151414,-4.43805931965865,
4.72530389871772));
#67835=CARTESIAN_POINT('Ctrl Pts',(-7.87801612827149,-5.94995159800372,
2.35368967431146));
#67836=CARTESIAN_POINT('Ctrl Pts',(-7.82385470835333,-6.21842353641775,
0.659912384387782));
#67837=CARTESIAN_POINT('Ctrl Pts',(-7.80274458175964,-6.21887801778165,
-0.000118905825011589));
#67838=CARTESIAN_POINT('Ctrl Pts',(-8.80625541824036,-6.21896305789945,
-0.000139202748640176));
#67839=CARTESIAN_POINT('Ctrl Pts',(-8.7954796508409,-6.21923989921398,-0.337042195846759));
#67840=CARTESIAN_POINT('Ctrl Pts',(-8.75165259011697,-6.10979663044418,
-1.707111614424));
#67841=CARTESIAN_POINT('Ctrl Pts',(-8.67477423606854,-5.11768488976202,
-3.97921708963369));
#67842=CARTESIAN_POINT('Ctrl Pts',(-8.57562035609511,-2.5929519681933,-5.94150379684923));
#67843=CARTESIAN_POINT('Ctrl Pts',(-8.47646647612167,0.56265821350308,-6.45819502741354));
#67844=CARTESIAN_POINT('Ctrl Pts',(-8.37731259614824,3.58137103787181,-5.40357740450012));
#67845=CARTESIAN_POINT('Ctrl Pts',(-8.2781587161748,5.72871965048953,-3.0342442952779));
#67846=CARTESIAN_POINT('Ctrl Pts',(-8.17900483620137,6.48224415781214,0.0733345473956177));
#67847=CARTESIAN_POINT('Ctrl Pts',(-8.07985095622792,5.65860854650426,3.16307075399211));
#67848=CARTESIAN_POINT('Ctrl Pts',(-7.98069707625449,3.45820718722118,5.48321715123368));
#67849=CARTESIAN_POINT('Ctrl Pts',(-7.88154319628105,0.416407953241648,
6.46927134179796));
#67850=CARTESIAN_POINT('Ctrl Pts',(-7.78238931630763,-2.72670527029838,
5.88132176013677));
#67851=CARTESIAN_POINT('Ctrl Pts',(-7.68323543633418,-5.20639843392111,
3.86241927094858));
#67852=CARTESIAN_POINT('Ctrl Pts',(-7.60785747031176,-6.12849923849585,
1.61322038691257));
#67853=CARTESIAN_POINT('Ctrl Pts',(-7.56553079761382,-6.21936745344784,
0.290132337765249));
#67854=CARTESIAN_POINT('Ctrl Pts',(-7.55625541824035,-6.21909175420816,
0.00015600608979878));
#67855=CARTESIAN_POINT('Origin',(-15.9277445817596,0.,0.));
#67856=CARTESIAN_POINT('',(-10.3027445817596,-6.21876660816596,6.94236083599781E-5));
#67857=CARTESIAN_POINT('',(-10.0562554182404,-6.21971612434898,7.06762300196201E-5));
#67858=CARTESIAN_POINT('',(-15.9277445817596,-6.21925,-5.19709976349859E-13));
#67859=CARTESIAN_POINT('Ctrl Pts',(-10.3027445817596,-6.21876660816596,
6.94236083600974E-5));
#67860=CARTESIAN_POINT('Ctrl Pts',(-10.2837524148075,-6.21853335738712,
-0.593771994205459));
#67861=CARTESIAN_POINT('Ctrl Pts',(-10.2317089545308,-5.98721839491704,
-2.22122932514984));
#67862=CARTESIAN_POINT('Ctrl Pts',(-10.1466142009297,-4.58668748447852,
-4.58117510904947));
#67863=CARTESIAN_POINT('Ctrl Pts',(-10.0474603209563,-1.83880224932734,
-6.21640360239859));
#67864=CARTESIAN_POINT('Ctrl Pts',(-9.94830644098286,1.35647211574301,-6.33915221928435));
#67865=CARTESIAN_POINT('Ctrl Pts',(-9.84915256100943,4.22171051319157,-4.91955565095604));
#67866=CARTESIAN_POINT('Ctrl Pts',(-9.749998681036,6.05978712967198,-2.30300833761142));
#67867=CARTESIAN_POINT('Ctrl Pts',(-9.65084480106255,6.42348938510785,0.873871603528));
#67868=CARTESIAN_POINT('Ctrl Pts',(-9.55169092108912,5.22432683107353,3.83813452371996));
#67869=CARTESIAN_POINT('Ctrl Pts',(-9.45253704111568,2.75406128800256,5.86856148318917));
#67870=CARTESIAN_POINT('Ctrl Pts',(-9.35338316114225,-0.386280161182942,
6.47114016979406));
#67871=CARTESIAN_POINT('Ctrl Pts',(-9.25422928116881,-3.43263785258272,
5.49926038963988));
#67872=CARTESIAN_POINT('Ctrl Pts',(-9.15507540119538,-5.6438188071929,3.18938500837096));
#67873=CARTESIAN_POINT('Ctrl Pts',(-9.08791383472565,-6.2114446770495,1.09918238554259));
#67874=CARTESIAN_POINT('Ctrl Pts',(-9.0538035615804,-6.21977625623512,0.0331312712238126));
#67875=CARTESIAN_POINT('Ctrl Pts',(-9.05274458175964,-6.21976606909926,
3.47298191171689E-5));
#67876=CARTESIAN_POINT('Ctrl Pts',(-10.0562554182404,-6.21971612434898,
7.06762300198109E-5));
#67877=CARTESIAN_POINT('Ctrl Pts',(-10.025428504068,-6.21915984463267,-0.963392497100496));
#67878=CARTESIAN_POINT('Ctrl Pts',(-9.96155029657112,-5.74777108715391,
-2.96036492166516));
#67879=CARTESIAN_POINT('Ctrl Pts',(-9.86462079574977,-3.70059880012039,
-5.32263429120195));
#67880=CARTESIAN_POINT('Ctrl Pts',(-9.76546691577635,-0.706074257995519,
-6.44409236584388));
#67881=CARTESIAN_POINT('Ctrl Pts',(-9.66631303580289,2.46024143136038,-5.99767283008577));
#67882=CARTESIAN_POINT('Ctrl Pts',(-9.56715915582948,5.02796895074312,-4.0919916309414));
#67883=CARTESIAN_POINT('Ctrl Pts',(-9.46800527585603,6.37236826560774,-1.1907098575248));
#67884=CARTESIAN_POINT('Ctrl Pts',(-9.36885139588261,6.16634077687366,2.00027715599528));
#67885=CARTESIAN_POINT('Ctrl Pts',(-9.26969751590915,4.4600139297068,4.70458744462813));
#67886=CARTESIAN_POINT('Ctrl Pts',(-9.17054363593573,1.66854497323006,6.2642497515377));
#67887=CARTESIAN_POINT('Ctrl Pts',(-9.07138975596228,-1.52888872691469,
6.29979099161586));
#67888=CARTESIAN_POINT('Ctrl Pts',(-8.97223587598886,-4.35433669693118,
4.80256381603513));
#67889=CARTESIAN_POINT('Ctrl Pts',(-8.88385776341487,-5.92842844484179,
2.42655284231093));
#67890=CARTESIAN_POINT('Ctrl Pts',(-8.82853094416538,-6.21839077514218,
0.696302273646909));
#67891=CARTESIAN_POINT('Ctrl Pts',(-8.80625541824036,-6.21896305789945,
-0.000139202748640176));
#67892=CARTESIAN_POINT('Origin',(-15.9277445817596,0.,0.));
#67893=CARTESIAN_POINT('',(-11.5527445817596,-6.21941055513622,-0.000149866139592504));
#67894=CARTESIAN_POINT('',(-11.3062554182404,-6.21873258297641,3.7485977482099E-5));
#67895=CARTESIAN_POINT('',(-15.9277445817596,-6.21925,-5.19709976349859E-13));
#67896=CARTESIAN_POINT('Ctrl Pts',(-11.5527445817596,-6.21941055513622,
-0.000149866139592288));
#67897=CARTESIAN_POINT('Ctrl Pts',(-11.546752561359,-6.21960006073928,-0.187450862764453));
#67898=CARTESIAN_POINT('Ctrl Pts',(-11.507709247634,-6.16556255002488,-1.40777360244643));
#67899=CARTESIAN_POINT('Ctrl Pts',(-11.4356146405844,-5.39117573865922,
-3.60001272395876));
#67900=CARTESIAN_POINT('Ctrl Pts',(-11.336460760611,-3.01444017827433,-5.73916525930964));
#67901=CARTESIAN_POINT('Ctrl Pts',(-11.2373068806375,0.0957226818348403,
-6.48195222344366));
#67902=CARTESIAN_POINT('Ctrl Pts',(-11.1381530006641,3.18259576877592,-5.64765009833173));
#67903=CARTESIAN_POINT('Ctrl Pts',(-11.0389991206906,5.49512851954185,-3.43924846639081));
#67904=CARTESIAN_POINT('Ctrl Pts',(-10.9398452407172,6.47067097239111,-0.394061704715005));
#67905=CARTESIAN_POINT('Ctrl Pts',(-10.8406913607438,5.87186911638537,2.7470021004937));
#67906=CARTESIAN_POINT('Ctrl Pts',(-10.7415374807704,3.84441422499412,5.219707532676));
#67907=CARTESIAN_POINT('Ctrl Pts',(-10.6423836007969,0.881595492385054,
6.42243387259649));
#67908=CARTESIAN_POINT('Ctrl Pts',(-10.5432297208235,-2.29571951921329,
6.062552214137));
#67909=CARTESIAN_POINT('Ctrl Pts',(-10.44407584085,-4.9144753063956,4.22762343674055));
#67910=CARTESIAN_POINT('Ctrl Pts',(-10.3639141278288,-6.06494378424448,
1.91258134226202));
#67911=CARTESIAN_POINT('Ctrl Pts',(-10.316803708132,-6.21893927420161,0.439665998301346));
#67912=CARTESIAN_POINT('Ctrl Pts',(-10.3027445817596,-6.21876660816596,
6.94236083600974E-5));
#67913=CARTESIAN_POINT('Ctrl Pts',(-11.3062554182404,-6.21873258297641,
3.74859774820643E-5));
#67914=CARTESIAN_POINT('Ctrl Pts',(-11.2884286506195,-6.21861515675503,
-0.557373294400618));
#67915=CARTESIAN_POINT('Ctrl Pts',(-11.2375505896742,-6.00671752297004,
-2.14832578591357));
#67916=CARTESIAN_POINT('Ctrl Pts',(-11.1536212354044,-4.66648376653058,
-4.49986627956914));
#67917=CARTESIAN_POINT('Ctrl Pts',(-11.054467355431,-1.94775856528816,-6.18313058641824));
#67918=CARTESIAN_POINT('Ctrl Pts',(-10.9553134754576,1.24486534373372,-6.36201049616318));
#67919=CARTESIAN_POINT('Ctrl Pts',(-10.8561595954841,4.13460773126303,-4.99298369573902));
#67920=CARTESIAN_POINT('Ctrl Pts',(-10.7570057155107,6.01838084932733,-2.40914076587077));
#67921=CARTESIAN_POINT('Ctrl Pts',(-10.6578518355373,6.43785394671903,0.760857304653864));
#67922=CARTESIAN_POINT('Ctrl Pts',(-10.5586979555638,5.2909672700661,3.74573525818645));
#67923=CARTESIAN_POINT('Ctrl Pts',(-10.4595440755904,2.85676367597327,5.81925842156633));
#67924=CARTESIAN_POINT('Ctrl Pts',(-10.360390195617,-0.272503792359383,
6.4769289760257));
#67925=CARTESIAN_POINT('Ctrl Pts',(-10.2612363156435,-3.33546982202023,
5.55873262027628));
#67926=CARTESIAN_POINT('Ctrl Pts',(-10.1620824356701,-5.58690054814797,
3.28807079340383));
#67927=CARTESIAN_POINT('Ctrl Pts',(-10.093755469869,-6.20165507982626,1.17207489074341));
#67928=CARTESIAN_POINT('Ctrl Pts',(-10.0584797973925,-6.21975626385165,
0.0695913355015432));
#67929=CARTESIAN_POINT('Ctrl Pts',(-10.0562554182404,-6.21971612434898,
7.06762300198109E-5));
#67930=CARTESIAN_POINT('Origin',(-15.9277445817596,0.,0.));
#67931=CARTESIAN_POINT('',(-12.8027445817596,-6.21931067987726,0.000159553896288647));
#67932=CARTESIAN_POINT('',(-12.5562554182404,-6.21952031151783,-0.000132913339471741));
#67933=CARTESIAN_POINT('',(-15.9277445817596,-6.21925,-5.19709976349859E-13));
#67934=CARTESIAN_POINT('Ctrl Pts',(-12.8027445817596,-6.21931067987726,
0.000159553896288585));
#67935=CARTESIAN_POINT('Ctrl Pts',(-12.7767014145861,-6.21847181659383,
-0.813946089195492));
#67936=CARTESIAN_POINT('Ctrl Pts',(-12.7176069540881,-5.8538214760635,-2.66196229397221));
#67937=CARTESIAN_POINT('Ctrl Pts',(-12.6254612002656,-4.07460155155841,
-5.04207103051742));
#67938=CARTESIAN_POINT('Ctrl Pts',(-12.5263073202922,-1.16869364290732,
-6.37644329080494));
#67939=CARTESIAN_POINT('Ctrl Pts',(-12.4271534403188,2.02156270600836,-6.15939513026191));
#67940=CARTESIAN_POINT('Ctrl Pts',(-12.3279995603453,4.71996353557397,-4.4437386264808));
#67941=CARTESIAN_POINT('Ctrl Pts',(-12.2288456803719,6.26997526840712,-1.6468992987736));
#67942=CARTESIAN_POINT('Ctrl Pts',(-12.1296918003985,6.29447291053824,1.55063798442858));
#67943=CARTESIAN_POINT('Ctrl Pts',(-12.030537920425,4.78749604001144,4.37089799439875));
#67944=CARTESIAN_POINT('Ctrl Pts',(-11.9313840404516,2.11569914692158,6.12769813751704));
#67945=CARTESIAN_POINT('Ctrl Pts',(-11.8322301604782,-1.07085718055863,
6.39360089646495));
#67946=CARTESIAN_POINT('Ctrl Pts',(-11.7330762805047,-3.99686897955958,
5.10391083313569));
#67947=CARTESIAN_POINT('Ctrl Pts',(-11.6399144209319,-5.83236767530601,
2.72539768871601));
#67948=CARTESIAN_POINT('Ctrl Pts',(-11.5798038546835,-6.21855476969312,
0.845679828645856));
#67949=CARTESIAN_POINT('Ctrl Pts',(-11.5527445817596,-6.21941055513622,
-0.000149866139592288));
#67950=CARTESIAN_POINT('Ctrl Pts',(-12.5562554182404,-6.21952031151782,
-0.000132913339471047));
#67951=CARTESIAN_POINT('Ctrl Pts',(-12.5514287971711,-6.21966250851912,
-0.150997695672446));
#67952=CARTESIAN_POINT('Ctrl Pts',(-12.5135508827773,-6.17745595899215,
-1.33486110651861));
#67953=CARTESIAN_POINT('Ctrl Pts',(-12.4426216750591,-5.45360592369372,
-3.50471822801767));
#67954=CARTESIAN_POINT('Ctrl Pts',(-12.3434677950857,-3.11482849091286,
-5.68530655580378));
#67955=CARTESIAN_POINT('Ctrl Pts',(-12.2443139151122,-0.0181988194650487,
-6.4826334267188));
#67956=CARTESIAN_POINT('Ctrl Pts',(-12.1451600351388,3.08285871135025,-5.70270544700054));
#67957=CARTESIAN_POINT('Ctrl Pts',(-12.0460061551654,5.43384239437673,-3.5352827494326));
#67958=CARTESIAN_POINT('Ctrl Pts',(-11.9468522751919,6.46274697899828,-0.507709329187834));
#67959=CARTESIAN_POINT('Ctrl Pts',(-11.8476983952185,5.91923519889273,2.64339212664902));
#67960=CARTESIAN_POINT('Ctrl Pts',(-11.7485445152451,3.93554599561895,5.15134399897086));
#67961=CARTESIAN_POINT('Ctrl Pts',(-11.6493906352716,0.994320167882758,
6.4059499435945));
#67962=CARTESIAN_POINT('Ctrl Pts',(-11.5502367552982,-2.18882837604633,
6.10195850675201));
#67963=CARTESIAN_POINT('Ctrl Pts',(-11.4510828753248,-4.83942480730361,
4.3133322166964));
#67964=CARTESIAN_POINT('Ctrl Pts',(-11.3697557629721,-6.04771213056323,
1.98550746867938));
#67965=CARTESIAN_POINT('Ctrl Pts',(-11.321479943944,-6.21883286804007,0.476080868258791));
#67966=CARTESIAN_POINT('Ctrl Pts',(-11.3062554182404,-6.21873258297641,
3.74859774820643E-5));
#67967=CARTESIAN_POINT('Origin',(-14.,0.,0.));
#67968=CARTESIAN_POINT('',(-14.25,5.55,-6.79678973526781E-16));
#67969=CARTESIAN_POINT('Origin',(-14.25,0.,0.));
#67970=CARTESIAN_POINT('',(-13.75,5.05,6.18446633569413E-16));
#67971=CARTESIAN_POINT('',(-14.,5.3,-6.49062803548097E-16));
#67972=CARTESIAN_POINT('',(-13.75,-5.05,-6.18446633569413E-16));
#67973=CARTESIAN_POINT('Origin',(-13.75,0.,0.));
#67974=CARTESIAN_POINT('Origin',(-13.75,0.,0.));
#67975=CARTESIAN_POINT('Origin',(1.375,0.,0.));
#67976=CARTESIAN_POINT('',(16.5,5.05,-6.18446633569413E-16));
#67977=CARTESIAN_POINT('',(16.5,-5.05,-6.18446633569413E-16));
#67978=CARTESIAN_POINT('Origin',(16.5,0.,0.));
#67979=CARTESIAN_POINT('Origin',(16.5,0.,0.));
#67980=CARTESIAN_POINT('',(1.375,-5.05,-6.18446633569413E-16));
#67981=CARTESIAN_POINT('',(9.12159512479098,5.,-0.708872343937891));
#67982=CARTESIAN_POINT('',(8.95,5.05,-1.8164630073276E-16));
#67983=CARTESIAN_POINT('Ctrl Pts',(9.12159512479098,5.,-0.708872343937891));
#67984=CARTESIAN_POINT('Ctrl Pts',(9.10247449902065,5.00527119275577,-0.671692216931588));
#67985=CARTESIAN_POINT('Ctrl Pts',(9.08480986974434,5.01024201937277,-0.633637055570846));
#67986=CARTESIAN_POINT('Ctrl Pts',(8.98942081262808,5.03746706515582,-0.404140998411014));
#67987=CARTESIAN_POINT('Ctrl Pts',(8.95,5.05,-0.195962800871854));
#67988=CARTESIAN_POINT('Ctrl Pts',(8.95,5.05,-1.73472347597681E-16));
#67989=CARTESIAN_POINT('',(9.12159512479098,5.,0.708872343937891));
#67990=CARTESIAN_POINT('Ctrl Pts',(8.95,5.05,-1.73472347597681E-16));
#67991=CARTESIAN_POINT('Ctrl Pts',(8.95,5.05,0.195962800871854));
#67992=CARTESIAN_POINT('Ctrl Pts',(8.98942081262808,5.03746706515582,0.404140998411014));
#67993=CARTESIAN_POINT('Ctrl Pts',(9.08480986974434,5.01024201937277,0.633637055570845));
#67994=CARTESIAN_POINT('Ctrl Pts',(9.10247449902065,5.00527119275577,0.671692216931588));
#67995=CARTESIAN_POINT('Ctrl Pts',(9.12159512479098,5.,0.708872343937891));
#67996=CARTESIAN_POINT('',(11.878404875209,5.,0.708872343937891));
#67997=CARTESIAN_POINT('',(1.375,5.,0.708872343937891));
#67998=CARTESIAN_POINT('',(11.878404875209,5.,-0.708872343937891));
#67999=CARTESIAN_POINT('Ctrl Pts',(11.878404875209,5.,0.708872343937891));
#68000=CARTESIAN_POINT('Ctrl Pts',(11.8975255009794,5.00527119275577,0.671692216931588));
#68001=CARTESIAN_POINT('Ctrl Pts',(11.9151901302557,5.01024201937277,0.633637055570845));
#68002=CARTESIAN_POINT('Ctrl Pts',(12.0105791873719,5.03746706515582,0.404140998411014));
#68003=CARTESIAN_POINT('Ctrl Pts',(12.05,5.05,0.195962800871854));
#68004=CARTESIAN_POINT('Ctrl Pts',(12.05,5.05,-0.195962800871853));
#68005=CARTESIAN_POINT('Ctrl Pts',(12.0105791873719,5.03746706515582,-0.404140998411013));
#68006=CARTESIAN_POINT('Ctrl Pts',(11.9151901302557,5.01024201937277,-0.633637055570844));
#68007=CARTESIAN_POINT('Ctrl Pts',(11.8975255009794,5.00527119275577,-0.671692216931587));
#68008=CARTESIAN_POINT('Ctrl Pts',(11.878404875209,5.,-0.708872343937891));
#68009=CARTESIAN_POINT('',(1.375,5.,-0.708872343937891));
#68010=CARTESIAN_POINT('Origin',(-14.25,6.3,0.));
#68011=CARTESIAN_POINT('',(-14.25,-6.3,-7.71527483462833E-16));
#68012=CARTESIAN_POINT('Origin',(-14.25,0.,0.));
#68013=CARTESIAN_POINT('Origin',(16.75,0.,0.));
#68014=CARTESIAN_POINT('',(17.,5.55,6.79678973526781E-16));
#68015=CARTESIAN_POINT('',(16.75,5.3,-6.49062803548097E-16));
#68016=CARTESIAN_POINT('Origin',(17.,0.,0.));
#68017=CARTESIAN_POINT('Origin',(17.,5.05,0.));
#68018=CARTESIAN_POINT('',(17.,-7.6,-9.30731567351989E-16));
#68019=CARTESIAN_POINT('Origin',(17.,0.,0.));
#68020=CARTESIAN_POINT('Ctrl Pts',(10.5,11.8245760568039,-2.04435835333739));
#68021=CARTESIAN_POINT('Ctrl Pts',(10.7582304278698,11.8245760568039,-2.04435835333739));
#68022=CARTESIAN_POINT('Ctrl Pts',(11.3081516759042,11.8433355261774,-1.94148312624803));
#68023=CARTESIAN_POINT('Ctrl Pts',(11.7686177715371,11.8905905388006,-1.62853836082025));
#68024=CARTESIAN_POINT('Ctrl Pts',(12.1310271901565,11.9342839542065,-1.26813573971222));
#68025=CARTESIAN_POINT('Ctrl Pts',(12.4471177841003,11.981691241836,-0.802237030533718));
#68026=CARTESIAN_POINT('Ctrl Pts',(12.573833144828,12.0043367284087,-0.12872161701368));
#68027=CARTESIAN_POINT('Ctrl Pts',(12.501821965583,11.9916659712442,0.655782750176622));
#68028=CARTESIAN_POINT('Ctrl Pts',(12.2256409941389,11.9460677454848,1.17959764711775));
#68029=CARTESIAN_POINT('Ctrl Pts',(11.769637233635,11.8905834208578,1.62938507413833));
#68030=CARTESIAN_POINT('Ctrl Pts',(11.5402696174063,11.8672568247713,1.78727577115204));
#68031=CARTESIAN_POINT('Ctrl Pts',(11.0342336769945,11.8338577790529,1.99483160104378));
#68032=CARTESIAN_POINT('Ctrl Pts',(10.7590524777073,11.8246005449034,2.04641526111906));
#68033=CARTESIAN_POINT('Ctrl Pts',(10.2419038685047,11.8246359138644,2.04555244927938));
#68034=CARTESIAN_POINT('Ctrl Pts',(9.76152674270748,11.8410305581576,1.95718242696326));
#68035=CARTESIAN_POINT('Ctrl Pts',(9.2872402918347,11.8849211742903,1.66633669567092));
#68036=CARTESIAN_POINT('Ctrl Pts',(8.80831114863381,11.9403112406462,1.23618144218895));
#68037=CARTESIAN_POINT('Ctrl Pts',(8.53046789037361,11.9865603322116,0.729866720037598));
#68038=CARTESIAN_POINT('Ctrl Pts',(8.46006855397992,11.9984238321423,0.229180604878363));
#68039=CARTESIAN_POINT('Ctrl Pts',(8.45066730819559,12.0000222095556,0.0975454104158677));
#68040=CARTESIAN_POINT('Ctrl Pts',(8.44002425265866,12.0019480576085,-0.288216463181939));
#68041=CARTESIAN_POINT('Ctrl Pts',(8.58689532600872,11.9752818489509,-0.880228435298227));
#68042=CARTESIAN_POINT('Ctrl Pts',(8.99410238797636,11.9173755533414,-1.41710240312987));
#68043=CARTESIAN_POINT('Ctrl Pts',(9.34406991814095,11.8790166897006,-1.70485788162001));
#68044=CARTESIAN_POINT('Ctrl Pts',(9.83136405381611,11.8382527878677,-1.96874089736921));
#68045=CARTESIAN_POINT('Ctrl Pts',(10.2417708031704,11.8245760568039,-2.04435835333739));
#68046=CARTESIAN_POINT('Ctrl Pts',(10.5,11.8245760568039,-2.04435835333739));
#68047=CARTESIAN_POINT('Ctrl Pts',(10.5,11.6828756306444,-1.87957223555826));
#68048=CARTESIAN_POINT('Ctrl Pts',(10.7398027760933,11.6829069804735,-1.87967019655954));
#68049=CARTESIAN_POINT('Ctrl Pts',(11.2505600171714,11.699146809745,-1.78220242363967));
#68050=CARTESIAN_POINT('Ctrl Pts',(11.6737064964281,11.7398399156241,-1.4904193266981));
#68051=CARTESIAN_POINT('Ctrl Pts',(12.0049140807901,11.7773485944662,-1.15671595176948));
#68052=CARTESIAN_POINT('Ctrl Pts',(12.2910542687146,11.8177655371996,-0.728963555699616));
#68053=CARTESIAN_POINT('Ctrl Pts',(12.4045816142874,11.8370021724303,-0.116752087098428));
#68054=CARTESIAN_POINT('Ctrl Pts',(12.3400974998438,11.8262599163346,0.595201711882176));
#68055=CARTESIAN_POINT('Ctrl Pts',(12.0912278889217,11.787426402354,1.07451743336628));
#68056=CARTESIAN_POINT('Ctrl Pts',(11.6749144056302,11.7399000722776,1.49146106495459));
#68057=CARTESIAN_POINT('Ctrl Pts',(11.4639499848756,11.7197556690285,1.63828893506523));
#68058=CARTESIAN_POINT('Ctrl Pts',(10.9962576770092,11.6909565881495,1.8331120645509));
#68059=CARTESIAN_POINT('Ctrl Pts',(10.7406079241326,11.6828973823575,1.88145785991136));
#68060=CARTESIAN_POINT('Ctrl Pts',(10.2603645125265,11.6829578323396,1.88097023487898));
#68061=CARTESIAN_POINT('Ctrl Pts',(9.81417055101731,11.6971628557272,1.79707772775124));
#68062=CARTESIAN_POINT('Ctrl Pts',(9.37753152881029,11.7349932027385,1.52567415133084));
#68063=CARTESIAN_POINT('Ctrl Pts',(8.93924111117345,11.7825597062905,1.12661882189384));
#68064=CARTESIAN_POINT('Ctrl Pts',(8.68891806495232,11.8219474983071,0.662730723367097));
#68065=CARTESIAN_POINT('Ctrl Pts',(8.62561972670899,11.8320403251539,0.208365587035192));
#68066=CARTESIAN_POINT('Ctrl Pts',(8.6171018952244,11.8334177518436,0.0886180256498179));
#68067=CARTESIAN_POINT('Ctrl Pts',(8.60807558809857,11.8348997741416,-0.261658779614536));
#68068=CARTESIAN_POINT('Ctrl Pts',(8.73914827441268,11.8123885442958,-0.799850727292736));
#68069=CARTESIAN_POINT('Ctrl Pts',(9.10913830169419,11.7628090930054,-1.29430484284161));
#68070=CARTESIAN_POINT('Ctrl Pts',(9.42978691918065,11.7298811826287,-1.56142921347393));
#68071=CARTESIAN_POINT('Ctrl Pts',(9.87903805739242,11.6947195019836,-1.80813827520343));
#68072=CARTESIAN_POINT('Ctrl Pts',(10.2602598473556,11.6828949702791,-1.87963186326188));
#68073=CARTESIAN_POINT('Ctrl Pts',(10.5,11.6828756306444,-1.87957223555826));
#68074=CARTESIAN_POINT('Ctrl Pts',(10.5,11.5411752044848,-1.71478611777913));
#68075=CARTESIAN_POINT('Ctrl Pts',(10.7214715587286,11.5411438546557,-1.71468815677786));
#68076=CARTESIAN_POINT('Ctrl Pts',(11.1928739297933,11.5549205780978,-1.62336308521331));
#68077=CARTESIAN_POINT('Ctrl Pts',(11.5790873321378,11.5891311971719,-1.35148921845341));
#68078=CARTESIAN_POINT('Ctrl Pts',(11.8789049510917,11.6203680543884,-1.0453393213789));
#68079=CARTESIAN_POINT('Ctrl Pts',(12.1354850996937,11.6539745700422,-0.654632815392126));
#68080=CARTESIAN_POINT('Ctrl Pts',(12.235459123101,11.6696685204615,-0.104671223272519));
#68081=CARTESIAN_POINT('Ctrl Pts',(12.1785311912426,11.6608817102649,0.535319205819066));
#68082=CARTESIAN_POINT('Ctrl Pts',(11.9570548103486,11.6288249810861,0.969991925022837));
#68083=CARTESIAN_POINT('Ctrl Pts',(11.5795643809747,11.5890385606483,1.35211162816705));
#68084=CARTESIAN_POINT('Ctrl Pts',(11.3875459523367,11.5722428144048,1.48911191242604));
#68085=CARTESIAN_POINT('Ctrl Pts',(10.9579127537214,11.5479295617558,1.67029625018663));
#68086=CARTESIAN_POINT('Ctrl Pts',(10.7221443818625,11.5411913571738,1.71640740577542));
#68087=CARTESIAN_POINT('Ctrl Pts',(10.278600155584,11.5411826549977,1.71544744258993));
#68088=CARTESIAN_POINT('Ctrl Pts',(9.86678553559699,11.5532267637952,1.63688927133756));
#68089=CARTESIAN_POINT('Ctrl Pts',(9.46792380300963,11.5849776467071,1.38455066231656));
#68090=CARTESIAN_POINT('Ctrl Pts',(9.07028237660262,11.6247208601492,1.01726046285402));
#68091=CARTESIAN_POINT('Ctrl Pts',(8.84748056075628,11.6572783761553,0.596330563124787));
#68092=CARTESIAN_POINT('Ctrl Pts',(8.79154265363212,11.6655159168803,0.187037243054655));
#68093=CARTESIAN_POINT('Ctrl Pts',(8.78410590418262,11.6666169288766,0.0796337437952312));
#68094=CARTESIAN_POINT('Ctrl Pts',(8.77522139956891,11.6681056405353,-0.235179054312069));
#68095=CARTESIAN_POINT('Ctrl Pts',(8.89145925390984,11.6494496025653,-0.719393697895783));
#68096=CARTESIAN_POINT('Ctrl Pts',(9.2236096687965,11.6083855638654,-1.17137711112015));
#68097=CARTESIAN_POINT('Ctrl Pts',(9.51543333718696,11.5807480684238,-1.41804950400415));
#68098=CARTESIAN_POINT('Ctrl Pts',(9.92659698779092,11.5512199541647,-1.64755889631587));
#68099=CARTESIAN_POINT('Ctrl Pts',(10.2784680168167,11.5411558648501,-1.71472649007551));
#68100=CARTESIAN_POINT('Ctrl Pts',(10.5,11.5411752044848,-1.71478611777913));
#68101=CARTESIAN_POINT('Ctrl Pts',(10.5,11.3994747783253,-1.55));
#68102=CARTESIAN_POINT('Ctrl Pts',(10.7030439069521,11.3994747783253,-1.55));
#68103=CARTESIAN_POINT('Ctrl Pts',(11.1352822710605,11.4107318616654,-1.46408238260495));
#68104=CARTESIAN_POINT('Ctrl Pts',(11.4841760570289,11.4383805739953,-1.21337018433126));
#68105=CARTESIAN_POINT('Ctrl Pts',(11.7527918417253,11.4634326946481,-0.933919533436165));
#68106=CARTESIAN_POINT('Ctrl Pts',(11.9794215843079,11.4900488654058,-0.581359340558024));
#68107=CARTESIAN_POINT('Ctrl Pts',(12.0662075925604,11.5023339644831,-0.0927016933572669));
#68108=CARTESIAN_POINT('Ctrl Pts',(12.0168067255034,11.4954756553553,0.47473816752462));
#68109=CARTESIAN_POINT('Ctrl Pts',(11.8226417051315,11.4701836379553,0.864911711271363));
#68110=CARTESIAN_POINT('Ctrl Pts',(11.4848415529699,11.4383552120681,1.21418761898331));
#68111=CARTESIAN_POINT('Ctrl Pts',(11.311226319806,11.4247416586619,1.34012507633923));
#68112=CARTESIAN_POINT('Ctrl Pts',(10.9199367537361,11.4050283708524,1.50857671369375));
#68113=CARTESIAN_POINT('Ctrl Pts',(10.7036998282878,11.399488194628,1.55145000456772));
#68114=CARTESIAN_POINT('Ctrl Pts',(10.2970607996058,11.3995045734729,1.55086522818953));
#68115=CARTESIAN_POINT('Ctrl Pts',(9.91942934390681,11.4093590613647,1.47678457212554));
#68116=CARTESIAN_POINT('Ctrl Pts',(9.55821503998522,11.4350496751553,1.24388811797647));
#68117=CARTESIAN_POINT('Ctrl Pts',(9.20121233914227,11.4669693257936,0.907697842558912));
#68118=CARTESIAN_POINT('Ctrl Pts',(9.00593073533499,11.4926655422508,0.529194566454286));
#68119=CARTESIAN_POINT('Ctrl Pts',(8.95709382636119,11.4991324098919,0.166222225211484));
#68120=CARTESIAN_POINT('Ctrl Pts',(8.95054049121143,11.5000124711646,0.0707063590291814));
#68121=CARTESIAN_POINT('Ctrl Pts',(8.94327273500882,11.5010573570684,-0.208621370744666));
#68122=CARTESIAN_POINT('Ctrl Pts',(9.04371220231381,11.4865562979102,-0.639015989890292));
#68123=CARTESIAN_POINT('Ctrl Pts',(9.33864558251432,11.4538191035294,-1.04857955083189));
#68124=CARTESIAN_POINT('Ctrl Pts',(9.60115033822666,11.4316125613519,-1.27462083585808));
#68125=CARTESIAN_POINT('Ctrl Pts',(9.97427099136723,11.4076866682806,-1.4869562741501));
#68126=CARTESIAN_POINT('Ctrl Pts',(10.296957061002,11.3994747783253,-1.55));
#68127=CARTESIAN_POINT('Ctrl Pts',(10.5,11.3994747783253,-1.55));
#68128=CARTESIAN_POINT('',(10.5,11.8245760568039,-2.04435835333739));
#68129=CARTESIAN_POINT('',(10.5,11.3994747783253,-1.55));
#68130=CARTESIAN_POINT('',(10.5,11.8245760568039,-2.04435835333739));
#68131=CARTESIAN_POINT('',(8.94931572037071,11.5001882310673,0.00068897024722115));
#68132=CARTESIAN_POINT('Ctrl Pts',(10.5,11.3994747783253,-1.55));
#68133=CARTESIAN_POINT('Ctrl Pts',(10.7030439069521,11.3994747783253,-1.55));
#68134=CARTESIAN_POINT('Ctrl Pts',(11.1352822710605,11.4107318616654,-1.46408238260495));
#68135=CARTESIAN_POINT('Ctrl Pts',(11.4841760570289,11.4383805739953,-1.21337018433126));
#68136=CARTESIAN_POINT('Ctrl Pts',(11.7527918417253,11.4634326946481,-0.933919533436165));
#68137=CARTESIAN_POINT('Ctrl Pts',(11.9794215843079,11.4900488654058,-0.581359340558024));
#68138=CARTESIAN_POINT('Ctrl Pts',(12.0662075925604,11.5023339644831,-0.0927016933572669));
#68139=CARTESIAN_POINT('Ctrl Pts',(12.0168067255034,11.4954756553553,0.47473816752462));
#68140=CARTESIAN_POINT('Ctrl Pts',(11.8226417051315,11.4701836379553,0.864911711271363));
#68141=CARTESIAN_POINT('Ctrl Pts',(11.4848415529699,11.4383552120681,1.21418761898331));
#68142=CARTESIAN_POINT('Ctrl Pts',(11.311226319806,11.4247416586619,1.34012507633923));
#68143=CARTESIAN_POINT('Ctrl Pts',(10.9199367537361,11.4050283708524,1.50857671369375));
#68144=CARTESIAN_POINT('Ctrl Pts',(10.7036998282878,11.399488194628,1.55145000456772));
#68145=CARTESIAN_POINT('Ctrl Pts',(10.2970607996058,11.3995045734729,1.55086522818953));
#68146=CARTESIAN_POINT('Ctrl Pts',(9.91942934390681,11.4093590613647,1.47678457212554));
#68147=CARTESIAN_POINT('Ctrl Pts',(9.55821503998522,11.4350496751553,1.24388811797647));
#68148=CARTESIAN_POINT('Ctrl Pts',(9.20121233914227,11.4669693257936,0.907697842558912));
#68149=CARTESIAN_POINT('Ctrl Pts',(9.00593073533499,11.4926655422508,0.529194566454286));
#68150=CARTESIAN_POINT('Ctrl Pts',(8.95709382636119,11.4991324098919,0.166222225211484));
#68151=CARTESIAN_POINT('Ctrl Pts',(8.95054049121143,11.5000124711646,0.0707063590291814));
#68152=CARTESIAN_POINT('Ctrl Pts',(8.94932919851099,11.5001866188152,0.0241517374002067));
#68153=CARTESIAN_POINT('Ctrl Pts',(8.94931572037071,11.5001882310673,0.00068897024722007));
#68154=CARTESIAN_POINT('Ctrl Pts',(8.94931572037071,11.5001882310673,0.00068897024722007));
#68155=CARTESIAN_POINT('Ctrl Pts',(8.94918093896793,11.5002043535885,-0.233938701282644));
#68156=CARTESIAN_POINT('Ctrl Pts',(9.04371220231381,11.4865562979102,-0.639015989890292));
#68157=CARTESIAN_POINT('Ctrl Pts',(9.33864558251432,11.4538191035294,-1.04857955083189));
#68158=CARTESIAN_POINT('Ctrl Pts',(9.60115033822666,11.4316125613519,-1.27462083585808));
#68159=CARTESIAN_POINT('Ctrl Pts',(9.97427099136723,11.4076866682806,-1.4869562741501));
#68160=CARTESIAN_POINT('Ctrl Pts',(10.296957061002,11.3994747783253,-1.55));
#68161=CARTESIAN_POINT('Ctrl Pts',(10.5,11.3994747783253,-1.55));
#68162=CARTESIAN_POINT('Ctrl Pts',(10.5,11.8245760568039,-2.04435835333739));
#68163=CARTESIAN_POINT('Ctrl Pts',(10.2417708031704,11.8245760568039,-2.04435835333739));
#68164=CARTESIAN_POINT('Ctrl Pts',(9.83136405381611,11.8382527878677,-1.96874089736921));
#68165=CARTESIAN_POINT('Ctrl Pts',(9.34406991814095,11.8790166897006,-1.70485788162001));
#68166=CARTESIAN_POINT('Ctrl Pts',(8.99410238797636,11.9173755533414,-1.41710240312987));
#68167=CARTESIAN_POINT('Ctrl Pts',(8.58689532600872,11.9752818489509,-0.880228435298227));
#68168=CARTESIAN_POINT('Ctrl Pts',(8.44002425265866,12.0019480576085,-0.288216463181939));
#68169=CARTESIAN_POINT('Ctrl Pts',(8.45066730819559,12.0000222095556,0.0975454104158677));
#68170=CARTESIAN_POINT('Ctrl Pts',(8.46006855397992,11.9984238321423,0.229180604878363));
#68171=CARTESIAN_POINT('Ctrl Pts',(8.53046789037361,11.9865603322116,0.729866720037598));
#68172=CARTESIAN_POINT('Ctrl Pts',(8.80831114863381,11.9403112406462,1.23618144218895));
#68173=CARTESIAN_POINT('Ctrl Pts',(9.2872402918347,11.8849211742903,1.66633669567092));
#68174=CARTESIAN_POINT('Ctrl Pts',(9.76152674270748,11.8410305581576,1.95718242696326));
#68175=CARTESIAN_POINT('Ctrl Pts',(10.2419038685047,11.8246359138644,2.04555244927938));
#68176=CARTESIAN_POINT('Ctrl Pts',(10.7590524777073,11.8246005449034,2.04641526111906));
#68177=CARTESIAN_POINT('Ctrl Pts',(11.0342336769945,11.8338577790529,1.99483160104378));
#68178=CARTESIAN_POINT('Ctrl Pts',(11.5402696174063,11.8672568247713,1.78727577115204));
#68179=CARTESIAN_POINT('Ctrl Pts',(11.769637233635,11.8905834208578,1.62938507413833));
#68180=CARTESIAN_POINT('Ctrl Pts',(12.2256409941389,11.9460677454848,1.17959764711775));
#68181=CARTESIAN_POINT('Ctrl Pts',(12.501821965583,11.9916659712442,0.655782750176622));
#68182=CARTESIAN_POINT('Ctrl Pts',(12.573833144828,12.0043367284087,-0.12872161701368));
#68183=CARTESIAN_POINT('Ctrl Pts',(12.4471177841003,11.981691241836,-0.802237030533718));
#68184=CARTESIAN_POINT('Ctrl Pts',(12.1310271901565,11.9342839542065,-1.26813573971222));
#68185=CARTESIAN_POINT('Ctrl Pts',(11.7686177715371,11.8905905388006,-1.62853836082025));
#68186=CARTESIAN_POINT('Ctrl Pts',(11.3081516759042,11.8433355261774,-1.94148312624803));
#68187=CARTESIAN_POINT('Ctrl Pts',(10.7582304278698,11.8245760568039,-2.04435835333739));
#68188=CARTESIAN_POINT('Ctrl Pts',(10.5,11.8245760568039,-2.04435835333739));
#68189=CARTESIAN_POINT('Origin',(10.5,12.5,0.));
#68190=CARTESIAN_POINT('',(8.95,12.5,-1.8982025386784E-16));
#68191=CARTESIAN_POINT('Origin',(10.5,5.,0.));
#68192=CARTESIAN_POINT('Origin',(10.5,5.,0.));
#68193=CARTESIAN_POINT('Origin',(10.5,0.,0.));
#68194=CARTESIAN_POINT('',(14.5,-12.,-1.46957615897682E-15));
#68195=CARTESIAN_POINT('Origin',(14.5,0.,0.));
#68196=CARTESIAN_POINT('',(6.5,-12.,-1.46957615897682E-15));
#68197=CARTESIAN_POINT('',(10.5,-12.,-1.46957615897682E-15));
#68198=CARTESIAN_POINT('Origin',(6.5,0.,0.));
#68199=CARTESIAN_POINT('Ctrl Pts',(-14.0290837546341,-2.70929682014932,
5.59810515289136));
#68200=CARTESIAN_POINT('Ctrl Pts',(-13.9960324613096,-3.63933197645688,
5.14799905041672));
#68201=CARTESIAN_POINT('Ctrl Pts',(-13.9299298746607,-5.26981959467749,
3.77580048295898));
#68202=CARTESIAN_POINT('Ctrl Pts',(-13.8307759946872,-6.43349921927399,
0.79679165484266));
#68203=CARTESIAN_POINT('Ctrl Pts',(-13.7316221147138,-6.03180256523361,
-2.37521059424263));
#68204=CARTESIAN_POINT('Ctrl Pts',(-13.6324682347403,-4.1625811938585,-4.96974307260698));
#68205=CARTESIAN_POINT('Ctrl Pts',(-13.5333143547669,-1.28056321092969,
-6.35489385677935));
#68206=CARTESIAN_POINT('Ctrl Pts',(-13.4341604747935,1.91301075045669,-6.193982915654));
#68207=CARTESIAN_POINT('Ctrl Pts',(-13.33500659482,4.64114599103167,-4.52598857637084));
#68208=CARTESIAN_POINT('Ctrl Pts',(-13.2358527148466,6.24006591576224,-1.75683043852266));
#68209=CARTESIAN_POINT('Ctrl Pts',(-13.1366988348732,6.3207503286919,1.43978832745216));
#68210=CARTESIAN_POINT('Ctrl Pts',(-13.0375449548997,4.86356603929123,4.28609183779942));
#68211=CARTESIAN_POINT('Ctrl Pts',(-12.9383910749263,2.2230539416448,6.08957345749443));
#68212=CARTESIAN_POINT('Ctrl Pts',(-12.8392371949529,-0.958337716508845,
6.41143141299502));
#68213=CARTESIAN_POINT('Ctrl Pts',(-12.7400833149794,-3.90656124824087,
5.17335943056773));
#68214=CARTESIAN_POINT('Ctrl Pts',(-12.640929435006,-5.90430033493565,2.67658449074433));
#68215=CARTESIAN_POINT('Ctrl Pts',(-12.5417755550326,-6.46549569135999,
-0.471415594223555));
#68216=CARTESIAN_POINT('Ctrl Pts',(-12.4426216750591,-5.45360592369372,
-3.50471822801767));
#68217=CARTESIAN_POINT('Ctrl Pts',(-12.3434677950857,-3.11482849091286,
-5.68530655580378));
#68218=CARTESIAN_POINT('Ctrl Pts',(-12.2443139151122,-0.0181988194650487,
-6.4826334267188));
#68219=CARTESIAN_POINT('Ctrl Pts',(-12.1451600351388,3.08285871135025,-5.70270544700054));
#68220=CARTESIAN_POINT('Ctrl Pts',(-12.0460061551654,5.43384239437673,-3.5352827494326));
#68221=CARTESIAN_POINT('Ctrl Pts',(-11.9468522751919,6.46274697899828,-0.507709329187834));
#68222=CARTESIAN_POINT('Ctrl Pts',(-11.8476983952185,5.91923519889273,2.64339212664902));
#68223=CARTESIAN_POINT('Ctrl Pts',(-11.7485445152451,3.93554599561895,5.15134399897086));
#68224=CARTESIAN_POINT('Ctrl Pts',(-11.6493906352716,0.994320167882758,
6.4059499435945));
#68225=CARTESIAN_POINT('Ctrl Pts',(-11.5502367552982,-2.18882837604633,
6.10195850675201));
#68226=CARTESIAN_POINT('Ctrl Pts',(-11.4510828753248,-4.83942480730361,
4.3133322166964));
#68227=CARTESIAN_POINT('Ctrl Pts',(-11.3519289953513,-6.31256670006456,
1.47525215966285));
#68228=CARTESIAN_POINT('Ctrl Pts',(-11.2527751153779,-6.2498317879533,-1.72176360155833));
#68229=CARTESIAN_POINT('Ctrl Pts',(-11.1536212354044,-4.66648376653058,
-4.49986627956914));
#68230=CARTESIAN_POINT('Ctrl Pts',(-11.054467355431,-1.94775856528816,-6.18313058641824));
#68231=CARTESIAN_POINT('Ctrl Pts',(-10.9553134754576,1.24486534373372,-6.36201049616318));
#68232=CARTESIAN_POINT('Ctrl Pts',(-10.8561595954841,4.13460773126303,-4.99298369573902));
#68233=CARTESIAN_POINT('Ctrl Pts',(-10.7570057155107,6.01838084932733,-2.40914076587077));
#68234=CARTESIAN_POINT('Ctrl Pts',(-10.6578518355373,6.43785394671903,0.760857304653864));
#68235=CARTESIAN_POINT('Ctrl Pts',(-10.5586979555638,5.2909672700661,3.74573525818645));
#68236=CARTESIAN_POINT('Ctrl Pts',(-10.4595440755904,2.85676367597327,5.81925842156633));
#68237=CARTESIAN_POINT('Ctrl Pts',(-10.360390195617,-0.272503792359383,
6.4769289760257));
#68238=CARTESIAN_POINT('Ctrl Pts',(-10.2612363156435,-3.33546982202023,
5.55873262027628));
#68239=CARTESIAN_POINT('Ctrl Pts',(-10.1620824356701,-5.58690054814797,
3.28807079340383));
#68240=CARTESIAN_POINT('Ctrl Pts',(-10.0629285556967,-6.47901241543966,
0.217406066865759));
#68241=CARTESIAN_POINT('Ctrl Pts',(-9.96377467572322,-5.79475046203404,
-2.90615456575997));
#68242=CARTESIAN_POINT('Ctrl Pts',(-9.86462079574977,-3.70059880012039,
-5.32263429120195));
#68243=CARTESIAN_POINT('Ctrl Pts',(-9.76546691577635,-0.706074257995519,
-6.44409236584388));
#68244=CARTESIAN_POINT('Ctrl Pts',(-9.66631303580289,2.46024143136038,-5.99767283008577));
#68245=CARTESIAN_POINT('Ctrl Pts',(-9.56715915582948,5.02796895074312,-4.0919916309414));
#68246=CARTESIAN_POINT('Ctrl Pts',(-9.46800527585603,6.37236826560774,-1.1907098575248));
#68247=CARTESIAN_POINT('Ctrl Pts',(-9.36885139588261,6.16634077687366,2.00027715599528));
#68248=CARTESIAN_POINT('Ctrl Pts',(-9.26969751590915,4.4600139297068,4.70458744462813));
#68249=CARTESIAN_POINT('Ctrl Pts',(-9.17054363593573,1.66854497323006,6.2642497515377));
#68250=CARTESIAN_POINT('Ctrl Pts',(-9.07138975596228,-1.52888872691469,
6.29979099161586));
#68251=CARTESIAN_POINT('Ctrl Pts',(-8.97223587598886,-4.35433669693118,
4.80256381603513));
#68252=CARTESIAN_POINT('Ctrl Pts',(-8.87308199601541,-6.1203543193245,2.13685055239179));
#68253=CARTESIAN_POINT('Ctrl Pts',(-8.77392811604199,-6.39726130204945,
-1.04876837797101));
#68254=CARTESIAN_POINT('Ctrl Pts',(-8.67477423606854,-5.11768488976202,
-3.97921708963369));
#68255=CARTESIAN_POINT('Ctrl Pts',(-8.57562035609511,-2.5929519681933,-5.94150379684923));
#68256=CARTESIAN_POINT('Ctrl Pts',(-8.47646647612167,0.56265821350308,-6.45819502741354));
#68257=CARTESIAN_POINT('Ctrl Pts',(-8.37731259614824,3.58137103787181,-5.40357740450012));
#68258=CARTESIAN_POINT('Ctrl Pts',(-8.2781587161748,5.72871965048953,-3.0342442952779));
#68259=CARTESIAN_POINT('Ctrl Pts',(-8.17900483620137,6.48224415781214,0.0733345473956177));
#68260=CARTESIAN_POINT('Ctrl Pts',(-8.07985095622792,5.65860854650426,3.16307075399211));
#68261=CARTESIAN_POINT('Ctrl Pts',(-7.98069707625449,3.45820718722118,5.48321715123368));
#68262=CARTESIAN_POINT('Ctrl Pts',(-7.88154319628105,0.416407953241648,
6.46927134179796));
#68263=CARTESIAN_POINT('Ctrl Pts',(-7.78238931630763,-2.72670527029838,
5.88132176013677));
#68264=CARTESIAN_POINT('Ctrl Pts',(-7.68323543633418,-5.20639843392111,
3.86241927094858));
#68265=CARTESIAN_POINT('Ctrl Pts',(-7.58408155636075,-6.41935067082568,
0.903772229215514));
#68266=CARTESIAN_POINT('Ctrl Pts',(-7.48492767638731,-6.07044506667244,
-2.27476679460632));
#68267=CARTESIAN_POINT('Ctrl Pts',(-7.38577379641388,-4.2445719758881,-4.89984448925031));
#68268=CARTESIAN_POINT('Ctrl Pts',(-7.28661991644044,-1.38597480405236,
-6.33276725609456));
#68269=CARTESIAN_POINT('Ctrl Pts',(-7.187466036467,1.80983647653362,-6.22489832893194));
#68270=CARTESIAN_POINT('Ctrl Pts',(-7.08831215649357,4.56530613428956,-4.6024827188757));
#68271=CARTESIAN_POINT('Ctrl Pts',(-6.98915827652013,6.21001560019695,-1.86026168122711));
#68272=CARTESIAN_POINT('Ctrl Pts',(-6.89000439654669,6.34379942025369,1.3345696658175));
#68273=CARTESIAN_POINT('Ctrl Pts',(-6.79085051657326,4.93410736951075,4.204694013061));
#68274=CARTESIAN_POINT('Ctrl Pts',(-6.69169663659982,2.3239240730231,6.05179677287292));
#68275=CARTESIAN_POINT('Ctrl Pts',(-6.59254275662638,-0.851680746854733,
6.42646926257087));
#68276=CARTESIAN_POINT('Ctrl Pts',(-6.49338887665295,-3.8200676843074,5.23755192476806));
#68277=CARTESIAN_POINT('Ctrl Pts',(-6.39423499667952,-5.85901440700082,
2.77431387119195));
#68278=CARTESIAN_POINT('Ctrl Pts',(-6.29508111670607,-6.47243570482011,
-0.363927636077572));
#68279=CARTESIAN_POINT('Ctrl Pts',(-6.19592723673265,-5.51108332618975,
-3.41362385876426));
#68280=CARTESIAN_POINT('Ctrl Pts',(-6.0967733567592,-3.20885877105538,-5.63276953769212));
#68281=CARTESIAN_POINT('Ctrl Pts',(-5.99761947678577,-0.125903969293837,
-6.48143621953093));
#68282=CARTESIAN_POINT('Ctrl Pts',(-5.89846559681233,2.98768385311816,-5.75313935787656));
#68283=CARTESIAN_POINT('Ctrl Pts',(-5.7993117168389,5.37435431396556,-3.62507696267142));
#68284=CARTESIAN_POINT('Ctrl Pts',(-5.70015783686546,6.45341940219507,-0.615016501163695));
#68285=CARTESIAN_POINT('Ctrl Pts',(-5.60100395689203,5.96233756874898,2.5446803323042));
#68286=CARTESIAN_POINT('Ctrl Pts',(-5.50185007691858,4.02059130515946,5.08524461891535));
#68287=CARTESIAN_POINT('Ctrl Pts',(-5.40269619694516,1.10061649827017,6.38854526485231));
#68288=CARTESIAN_POINT('Ctrl Pts',(-5.30354231697171,-2.08714341586264,
6.1374831681197));
#68289=CARTESIAN_POINT('Ctrl Pts',(-5.20438843699829,-4.76709164052158,
4.39314290323005));
#68290=CARTESIAN_POINT('Ctrl Pts',(-5.10523455702484,-6.28718432221605,
1.57993056043994));
#68291=CARTESIAN_POINT('Ctrl Pts',(-5.00608067705141,-6.27757584948428,
-1.61768622770392));
#68292=CARTESIAN_POINT('Ctrl Pts',(-4.90692679707797,-4.74060400838073,
-4.42171244124443));
#68293=CARTESIAN_POINT('Ctrl Pts',(-4.80777291710454,-2.05022118826812,
-6.14991547555801));
#68294=CARTESIAN_POINT('Ctrl Pts',(-4.7086190371311,1.13898997181236,-6.38181550355714));
#68295=CARTESIAN_POINT('Ctrl Pts',(-4.60946515715766,4.05107958026204,-5.06099017107475));
#68296=CARTESIAN_POINT('Ctrl Pts',(-4.51031127718423,5.9775227064379,-2.50880241775846));
#68297=CARTESIAN_POINT('Ctrl Pts',(-4.41115739721079,6.44960678792389,0.653788619124958));
#68298=CARTESIAN_POINT('Ctrl Pts',(-4.31200351723735,5.35247157449903,3.65730984762178));
#68299=CARTESIAN_POINT('Ctrl Pts',(-4.21284963726392,2.9530551606307,5.77099059916091));
#68300=CARTESIAN_POINT('Ctrl Pts',(-4.11369575729048,-0.164853293042968,
6.48056252721199));
#68301=CARTESIAN_POINT('Ctrl Pts',(-4.01454187731705,-3.24265217464831,
5.61338348517005));
#68302=CARTESIAN_POINT('Ctrl Pts',(-3.91538799734361,-5.53149871753584,
3.3804421626809));
#68303=CARTESIAN_POINT('Ctrl Pts',(-3.81623411737017,-6.47450592435959,
0.325023557244591));
#68304=CARTESIAN_POINT('Ctrl Pts',(-3.71708023739674,-5.84223576070193,
-2.80947478965496));
#68305=CARTESIAN_POINT('Ctrl Pts',(-3.6179263574233,-3.78852249476445,-5.26041486804939));
#68306=CARTESIAN_POINT('Ctrl Pts',(-3.51877247744987,-0.813044105235338,
-6.43147157035411));
#68307=CARTESIAN_POINT('Ctrl Pts',(-3.41961859747643,2.36025169231589,-6.03772136043487));
#68308=CARTESIAN_POINT('Ctrl Pts',(-3.32046471750299,4.95928728793312,-4.17496549363898));
#68309=CARTESIAN_POINT('Ctrl Pts',(-3.22131083752956,6.35170524667332,-1.29642112629886));
#68310=CARTESIAN_POINT('Ctrl Pts',(-3.12215695755612,6.19872381031724,1.89754852394804));
#68311=CARTESIAN_POINT('Ctrl Pts',(-3.02300307758268,4.53756407304736,4.62983580273871));
#68312=CARTESIAN_POINT('Ctrl Pts',(-2.92384919760925,1.77239391631247,6.23566252155694));
#68313=CARTESIAN_POINT('Ctrl Pts',(-2.82469531763581,-1.42400791440103,
6.32432357940788));
#68314=CARTESIAN_POINT('Ctrl Pts',(-2.72554143766238,-4.27394200392325,
4.87424732901725));
#68315=CARTESIAN_POINT('Ctrl Pts',(-2.62638755768894,-6.08400614812665,
2.23824405883015));
#68316=CARTESIAN_POINT('Ctrl Pts',(-2.5272336777155,-6.41380333157943,-0.942334389244107));
#68317=CARTESIAN_POINT('Ctrl Pts',(-2.42807979774207,-5.18309236738467,
-3.8936385025436));
#68318=CARTESIAN_POINT('Ctrl Pts',(-2.32892591776863,-2.69131095073478,
-5.89760227921367));
#68319=CARTESIAN_POINT('Ctrl Pts',(-2.2297720377952,0.455278923448612,-6.46665202242975));
#68320=CARTESIAN_POINT('Ctrl Pts',(-2.13061815782176,3.49109732043444,-5.4623352859914));
#68321=CARTESIAN_POINT('Ctrl Pts',(-2.03146427784832,5.67751552051297,-3.12900699770163));
#68322=CARTESIAN_POINT('Ctrl Pts',(-1.93231039787489,6.48256781800243,-0.0343767702148776));
#68323=CARTESIAN_POINT('Ctrl Pts',(-1.83315651790145,5.71038124883349,3.06861748517184));
#68324=CARTESIAN_POINT('Ctrl Pts',(-1.73400263792802,3.54883239268839,5.42500285031601));
#68325=CARTESIAN_POINT('Ctrl Pts',(-1.63484875795458,0.523836128332554,
6.46145981864663));
#68326=CARTESIAN_POINT('Ctrl Pts',(-1.53569487798115,-2.62861189967033,
5.92581359462503));
#68327=CARTESIAN_POINT('Ctrl Pts',(-1.43654099800771,-5.14150644054926,
3.94838939304646));
#68328=CARTESIAN_POINT('Ctrl Pts',(-1.33738711803427,-6.40344857817083,
1.01030370881892));
#68329=CARTESIAN_POINT('Ctrl Pts',(-1.23823323806084,-6.10740192775504,
-2.17359356140592));
#68330=CARTESIAN_POINT('Ctrl Pts',(-1.1390793580874,-4.32539601471359,-4.82864542011847));
#68331=CARTESIAN_POINT('Ctrl Pts',(-1.03992547811397,-1.49100115648436,
-6.30886541532577));
#68332=CARTESIAN_POINT('Ctrl Pts',(-0.940771598140529,1.70616120997042,
-6.25410914542779));
#68333=CARTESIAN_POINT('Ctrl Pts',(-0.841617718167091,4.48820662760173,
-4.67769906527593));
#68334=CARTESIAN_POINT('Ctrl Pts',(-0.742463838193658,6.17825052154845,
-1.96318307101446));
#68335=CARTESIAN_POINT('Ctrl Pts',(-0.643309958220219,6.36509736085303,
1.22898448492769));
#68336=CARTESIAN_POINT('Ctrl Pts',(-0.544156078246782,5.00328644146473,
4.12213440610403));
#68337=CARTESIAN_POINT('Ctrl Pts',(-0.445002198273347,2.42415268673505,
6.01234987577457));
#68338=CARTESIAN_POINT('Ctrl Pts',(-0.34584831829991,-0.744788678740318,
6.43973268865655));
#68339=CARTESIAN_POINT('Ctrl Pts',(-0.246694438326474,-3.73251949855906,
5.3002986208522));
#68340=CARTESIAN_POINT('Ctrl Pts',(-0.14754055835304,-5.81211098394011,
2.87127727461039));
#68341=CARTESIAN_POINT('Ctrl Pts',(-0.0483866783796017,-6.47758886518034,
-0.256339171846516));
#68342=CARTESIAN_POINT('Ctrl Pts',(0.0507672015938321,-5.56703928211486,
-3.32158710689955));
#68343=CARTESIAN_POINT('Ctrl Pts',(0.149921081567268,-3.30200317851016,
-5.5786774675043));
#68344=CARTESIAN_POINT('Ctrl Pts',(0.249074961540705,-0.233574361216745,
-6.47844968299619));
#68345=CARTESIAN_POINT('Ctrl Pts',(0.348228841514139,2.89168418329416,-5.8019849932086));
#68346=CARTESIAN_POINT('Ctrl Pts',(0.447382721487577,5.31338253190132,-3.71387039986819));
#68347=CARTESIAN_POINT('Ctrl Pts',(0.546536601461015,6.44231022572788,-0.722153884441094));
#68348=CARTESIAN_POINT('Ctrl Pts',(0.645690481434449,6.00379391212401,2.44526602603354));
#68349=CARTESIAN_POINT('Ctrl Pts',(0.744844361407886,4.10452664743683,5.01774135222336));
#68350=CARTESIAN_POINT('Ctrl Pts',(0.843998241381322,1.20660898072922,6.36937689613002));
#68351=CARTESIAN_POINT('Ctrl Pts',(0.943152121354761,-1.9848822566212,6.17131345052912));
#68352=CARTESIAN_POINT('Ctrl Pts',(1.04230600132819,-4.69344241962331,4.47174077189317));
#68353=CARTESIAN_POINT('Ctrl Pts',(1.14145988130163,-6.26006623726308,1.68417278876314));
#68354=CARTESIAN_POINT('Ctrl Pts',(1.24061376127507,-6.30358685653012,-1.51316225815738));
#68355=CARTESIAN_POINT('Ctrl Pts',(1.3397676412485,-4.81341550856989,-4.34233789785988));
#68356=CARTESIAN_POINT('Ctrl Pts',(1.43892152122194,-2.15211780533888,-6.11500255349699));
#68357=CARTESIAN_POINT('Ctrl Pts',(1.53807540119537,1.03280015818185,-6.39985867895463));
#68358=CARTESIAN_POINT('Ctrl Pts',(1.63722928116881,3.96643304506188,-5.12759945553204));
#68359=CARTESIAN_POINT('Ctrl Pts',(1.73638316114225,5.93501434493084,-2.60777146291548));
#68360=CARTESIAN_POINT('Ctrl Pts',(1.83553704111568,6.45957908194884,0.546539441742633));
#68361=CARTESIAN_POINT('Ctrl Pts',(1.93469092108912,5.41249821859067,3.56787476112659));
#68362=CARTESIAN_POINT('Ctrl Pts',(2.03384480106256,3.0485313934114,5.72112957559227));
#68363=CARTESIAN_POINT('Ctrl Pts',(2.13299868103599,-0.0571572825696857,
6.48240698524711));
#68364=CARTESIAN_POINT('Ctrl Pts',(2.23215256100943,-3.14893932616178,5.66648465960009));
#68365=CARTESIAN_POINT('Ctrl Pts',(2.33130644098286,-5.47456980244149,3.471880291071));
#68366=CARTESIAN_POINT('Ctrl Pts',(2.4304603209563,-6.46821201217862,0.432551318156661));
#68367=CARTESIAN_POINT('Ctrl Pts',(2.52961420092973,-5.8881081895082,-2.71201940000037));
#68368=CARTESIAN_POINT('Ctrl Pts',(2.62876808090318,-3.87540028951621,-5.19674319871096));
#68369=CARTESIAN_POINT('Ctrl Pts',(2.7279219608766,-0.919789494855471,-6.41707523428578));
#68370=CARTESIAN_POINT('Ctrl Pts',(2.82707584085005,2.25961035703773,-6.07610305308455));
#68371=CARTESIAN_POINT('Ctrl Pts',(2.92622972082348,4.88923651142507,-4.25678677087163));
#68372=CARTESIAN_POINT('Ctrl Pts',(3.02538360079692,6.32928870830338,-1.40177449124226));
#68373=CARTESIAN_POINT('Ctrl Pts',(3.12453748077035,6.22939555800606,1.79429603443556));
#68374=CARTESIAN_POINT('Ctrl Pts',(3.22369136074379,4.61386152810167,4.55380599903706));
#68375=CARTESIAN_POINT('Ctrl Pts',(3.32284524071722,1.87575355343092,6.20535380813579));
#68376=CARTESIAN_POINT('Ctrl Pts',(3.42199912069066,-1.31873397506443,6.34711020702708));
#68377=CARTESIAN_POINT('Ctrl Pts',(3.5211530006641,-4.19236740098541,4.94458520535987));
#68378=CARTESIAN_POINT('Ctrl Pts',(3.62030688063753,-6.04597836127066,2.33901965172245));
#68379=CARTESIAN_POINT('Ctrl Pts',(3.71946076061097,-6.42857469838133,-0.835640249567287));
#68380=CARTESIAN_POINT('Ctrl Pts',(3.8186146405844,-5.24706894496936,-3.80698499626393));
#68381=CARTESIAN_POINT('Ctrl Pts',(3.91776852055784,-2.78892694192586,-5.85207260635886));
#68382=CARTESIAN_POINT('Ctrl Pts',(4.01692240053128,0.347773945463821,-6.47332376513164));
#68383=CARTESIAN_POINT('Ctrl Pts',(4.11607628050471,3.3998598111037,-5.51958517592035));
#68384=CARTESIAN_POINT('Ctrl Pts',(4.21523016047815,5.62474399967788,-3.2229058751893));
#68385=CARTESIAN_POINT('Ctrl Pts',(4.31438404045158,6.48110182257391,-0.142078593380259));
#68386=CARTESIAN_POINT('Ctrl Pts',(4.41353792042502,5.76057749963056,2.97331705330878));
#68387=CARTESIAN_POINT('Ctrl Pts',(4.51269180039846,3.63847783642259,5.36529088040279));
#68388=CARTESIAN_POINT('Ctrl Pts',(4.6118456803719,0.631119752015993,6.45186444679596));
#68389=CARTESIAN_POINT('Ctrl Pts',(4.71099956034532,-2.5297929710906,5.96866954249621));
#68390=CARTESIAN_POINT('Ctrl Pts',(4.81015344031878,-5.07519478672013,4.03326937102785));
#68391=CARTESIAN_POINT('Ctrl Pts',(4.9093073202922,-6.3857791487184,1.1165564855737));
#68392=CARTESIAN_POINT('Ctrl Pts',(5.00846120026564,-6.14267180917851,-2.07182067402597));
#68393=CARTESIAN_POINT('Ctrl Pts',(5.10761508023907,-4.40502769148852,-4.75611250736834));
#68394=CARTESIAN_POINT('Ctrl Pts',(5.20676896021251,-1.59561249292064,-6.28322342394515));
#68395=CARTESIAN_POINT('Ctrl Pts',(5.30592284018595,1.60200834941566,-6.28159039988369));
#68396=CARTESIAN_POINT('Ctrl Pts',(5.40507672015938,4.40988078716951,-4.75162981867586));
#68397=CARTESIAN_POINT('Ctrl Pts',(5.50423060013282,6.14475515867778,-2.06555128428737));
#68398=CARTESIAN_POINT('Ctrl Pts',(5.60338448010625,6.38468584605272,1.12303831208186));
#68399=CARTESIAN_POINT('Ctrl Pts',(5.7025383600797,5.07099150144849,4.03847901383656));
#68400=CARTESIAN_POINT('Ctrl Pts',(5.80169224005312,2.52389427730921,5.97115958776782));
#68401=CARTESIAN_POINT('Ctrl Pts',(5.90084612002658,-0.638069512693321,
6.45139792173227));
#68402=CARTESIAN_POINT('Ctrl Pts',(5.96694870667552,-2.64132982999147,5.72450942764096));
#68403=CARTESIAN_POINT('Ctrl Pts',(6.,-3.49587713861109,5.14372565308808));
#68404=CARTESIAN_POINT('Ctrl Pts',(-13.8917225030894,-2.81294064672976,
5.81225999754714));
#68405=CARTESIAN_POINT('Ctrl Pts',(-13.8586712097649,-3.77855418696971,
5.34493513982917));
#68406=CARTESIAN_POINT('Ctrl Pts',(-13.792568623116,-5.47141591447493,3.92024327990461));
#68407=CARTESIAN_POINT('Ctrl Pts',(-13.6934147431425,-6.67961196425968,
0.827272824525194));
#68408=CARTESIAN_POINT('Ctrl Pts',(-13.5942608631691,-6.26254845264959,
-2.46607399211431));
#68409=CARTESIAN_POINT('Ctrl Pts',(-13.4951069831957,-4.32182024074876,
-5.15986000085787));
#68410=CARTESIAN_POINT('Ctrl Pts',(-13.3959531032222,-1.32955100376653,
-6.59799956300203));
#68411=CARTESIAN_POINT('Ctrl Pts',(-13.2967992232488,1.9861927484542,-6.43093299302389));
#68412=CARTESIAN_POINT('Ctrl Pts',(-13.1976453432754,4.81869247713522,-4.6991297293172));
#68413=CARTESIAN_POINT('Ctrl Pts',(-13.0984914633019,6.47877889280262,-1.82403777732267));
#68414=CARTESIAN_POINT('Ctrl Pts',(-12.9993375833285,6.56254987832162,1.49486725812272));
#68415=CARTESIAN_POINT('Ctrl Pts',(-12.900183703355,5.04962117780174,4.45005576963626));
#68416=CARTESIAN_POINT('Ctrl Pts',(-12.8010298233816,2.30809660492678,6.3225293635006));
#68417=CARTESIAN_POINT('Ctrl Pts',(-12.7018759434082,-0.994998811504643,
6.65669995668465));
#68418=CARTESIAN_POINT('Ctrl Pts',(-12.6027220634347,-4.05600628265989,
5.37126567829685));
#68419=CARTESIAN_POINT('Ctrl Pts',(-12.5035681834613,-6.1301686397452,2.77897691106667));
#68420=CARTESIAN_POINT('Ctrl Pts',(-12.4044143034879,-6.7128324575675,-0.489449541531061));
#68421=CARTESIAN_POINT('Ctrl Pts',(-12.3052604235144,-5.66223296757825,
-3.63879080564613));
#68422=CARTESIAN_POINT('Ctrl Pts',(-12.206106543541,-3.23398588317021,-5.90279727972304));
#68423=CARTESIAN_POINT('Ctrl Pts',(-12.1069526635675,-0.0188950131322108,
-6.73062579494758));
#68424=CARTESIAN_POINT('Ctrl Pts',(-12.0077987835941,3.20079310350503,-5.92086176342652));
#68425=CARTESIAN_POINT('Ctrl Pts',(-11.9086449036207,5.64171338680542,-3.67052456918084));
#68426=CARTESIAN_POINT('Ctrl Pts',(-11.8094910236472,6.70997859354236,-0.527131688995861));
#68427=CARTESIAN_POINT('Ctrl Pts',(-11.7103371436738,6.14567483514093,2.74451477704338));
#68428=CARTESIAN_POINT('Ctrl Pts',(-11.6111832637004,4.08609983809049,5.34840804899111));
#68429=CARTESIAN_POINT('Ctrl Pts',(-11.5120293837269,1.03235776726246,6.65100879432626));
#68430=CARTESIAN_POINT('Ctrl Pts',(-11.4128755037535,-2.27256174440011,
6.33538820133974));
#68431=CARTESIAN_POINT('Ctrl Pts',(-11.3137216237801,-5.02455642586494,
4.47833822597765));
#68432=CARTESIAN_POINT('Ctrl Pts',(-11.2145677438066,-6.55405318595761,
1.53168775500311));
#68433=CARTESIAN_POINT('Ctrl Pts',(-11.1154138638332,-6.4889183572691,-1.78762946269443));
#68434=CARTESIAN_POINT('Ctrl Pts',(-11.0162599838597,-4.84499954621256,
-4.67200812716823));
#68435=CARTESIAN_POINT('Ctrl Pts',(-10.9171061038863,-2.02226983679597,
-6.41966550922812));
#68436=CARTESIAN_POINT('Ctrl Pts',(-10.8179522239129,1.29248751892042,-6.60538844857633));
#68437=CARTESIAN_POINT('Ctrl Pts',(-10.7187983439394,4.29277665667947,-5.18398969125477));
#68438=CARTESIAN_POINT('Ctrl Pts',(-10.619644463966,6.2486132906028,-2.50130215840957));
#68439=CARTESIAN_POINT('Ctrl Pts',(-10.5204905839926,6.68413328128352,0.789963810057592));
#68440=CARTESIAN_POINT('Ctrl Pts',(-10.4213367040191,5.49337259166222,3.88902791354576));
#68441=CARTESIAN_POINT('Ctrl Pts',(-10.3221828240457,2.96604882952749,6.04187345812717));
#68442=CARTESIAN_POINT('Ctrl Pts',(-10.2230289440723,-0.282928392420811,
6.72470312117386));
#68443=CARTESIAN_POINT('Ctrl Pts',(-10.1238750640988,-3.46306782207204,
5.77138127339482));
#68444=CARTESIAN_POINT('Ctrl Pts',(-10.0247211841254,-5.8006267619862,3.41385554927162));
#68445=CARTESIAN_POINT('Ctrl Pts',(-9.92556730415195,-6.72686626231402,
0.225722910012753));
#68446=CARTESIAN_POINT('Ctrl Pts',(-9.82641342417851,-6.01642794952727,
-3.01732916190961));
#68447=CARTESIAN_POINT('Ctrl Pts',(-9.72725954420508,-3.84216476566213,
-5.52625103091307));
#68448=CARTESIAN_POINT('Ctrl Pts',(-9.62810566423164,-0.733085044486097,
-6.69061035038762));
#68449=CARTESIAN_POINT('Ctrl Pts',(-9.5289517842582,2.55435767376008,-6.22711308855605));
#68450=CARTESIAN_POINT('Ctrl Pts',(-9.42979790428477,5.22031330301457,-4.24853028252504));
#68451=CARTESIAN_POINT('Ctrl Pts',(-9.33064402431133,6.6161424532551,-1.23626032104847));
#68452=CARTESIAN_POINT('Ctrl Pts',(-9.2314901443379,6.40223340752278,2.076797519924));
#68453=CARTESIAN_POINT('Ctrl Pts',(-9.13233626436446,4.63063123041715,4.88456087596916));
#68454=CARTESIAN_POINT('Ctrl Pts',(-9.03318238439104,1.73237496208956,6.50388787833003));
#68455=CARTESIAN_POINT('Ctrl Pts',(-8.93402850441757,-1.5873761827352,6.54078874430662));
#68456=CARTESIAN_POINT('Ctrl Pts',(-8.83487462444418,-4.52091132771111,
4.98628532177378));
#68457=CARTESIAN_POINT('Ctrl Pts',(-8.7357207444707,-6.3544877435272,2.21859551530372));
#68458=CARTESIAN_POINT('Ctrl Pts',(-8.6365668644973,-6.64198776983563,-1.08888888713082));
#68459=CARTESIAN_POINT('Ctrl Pts',(-8.53741298452384,-5.31346131457574,
-4.13144156459587));
#68460=CARTESIAN_POINT('Ctrl Pts',(-8.43825910455042,-2.6921450363445,-6.16879531565515));
#68461=CARTESIAN_POINT('Ctrl Pts',(-8.33910522457696,0.584182636324011,
-6.70525250759289));
#68462=CARTESIAN_POINT('Ctrl Pts',(-8.23995134460355,3.71837595959501,-5.61029061335232));
#68463=CARTESIAN_POINT('Ctrl Pts',(-8.14079746463009,5.94787113716593,-3.15031894874656));
#68464=CARTESIAN_POINT('Ctrl Pts',(-8.04164358465668,6.73022163460534,0.0761399517559067));
#68465=CARTESIAN_POINT('Ctrl Pts',(-7.94248970468322,5.87507794126342,3.28407364826723));
#68466=CARTESIAN_POINT('Ctrl Pts',(-7.8433358247098,3.59050049053371,5.6929769690945));
#68467=CARTESIAN_POINT('Ctrl Pts',(-7.74418194473635,0.43233758980697,6.71675254506246));
#68468=CARTESIAN_POINT('Ctrl Pts',(-7.64502806476292,-2.83101505506209,
6.10631102230922));
#68469=CARTESIAN_POINT('Ctrl Pts',(-7.54587418478948,-5.40556858478126,
4.01017565929336));
#68470=CARTESIAN_POINT('Ctrl Pts',(-7.44672030481605,-6.66492216477869,
0.93834592800572));
#68471=CARTESIAN_POINT('Ctrl Pts',(-7.34756642484261,-6.30266921837014,
-2.3617877269079));
#68472=CARTESIAN_POINT('Ctrl Pts',(-7.24841254486918,-4.40694757036174,
-5.08728745553522));
#68473=CARTESIAN_POINT('Ctrl Pts',(-7.14925866489574,-1.43899510480635,
-6.57502651184819));
#68474=CARTESIAN_POINT('Ctrl Pts',(-7.05010478492231,1.879071554993,-6.46303107174794));
#68475=CARTESIAN_POINT('Ctrl Pts',(-6.95095090494887,4.73995137572269,-4.77855014611627));
#68476=CARTESIAN_POINT('Ctrl Pts',(-6.85179702497543,6.44757900600099,-1.93142576987532));
#68477=CARTESIAN_POINT('Ctrl Pts',(-6.752643145002,6.58648071013089,1.38562346914196));
#68478=CARTESIAN_POINT('Ctrl Pts',(-6.65348926502856,5.12286105819178,4.36554408082491));
#68479=CARTESIAN_POINT('Ctrl Pts',(-6.55433538505512,2.4128255111451,6.28330753631641));
#68480=CARTESIAN_POINT('Ctrl Pts',(-6.45518150508169,-0.884261692202764,
6.67231307740171));
#68481=CARTESIAN_POINT('Ctrl Pts',(-6.35602762510826,-3.9662039177586,5.43791384870334));
#68482=CARTESIAN_POINT('Ctrl Pts',(-6.25687374513481,-6.08315030404075,
2.88044491730221));
#68483=CARTESIAN_POINT('Ctrl Pts',(-6.15771986516138,-6.72003796041445,
-0.377849644371708));
#68484=CARTESIAN_POINT('Ctrl Pts',(-6.05856598518794,-5.72190916124855,
-3.54421163216635));
#68485=CARTESIAN_POINT('Ctrl Pts',(-5.95941210521451,-3.33161328045984,
-5.84825046425226));
#68486=CARTESIAN_POINT('Ctrl Pts',(-5.86025822524107,-0.130720410616282,
-6.7293827887416));
#68487=CARTESIAN_POINT('Ctrl Pts',(-5.76110434526764,3.10197734242757,-5.97322501754531));
#68488=CARTESIAN_POINT('Ctrl Pts',(-5.66195046529419,5.57994959697626,-3.76375384933284));
#68489=CARTESIAN_POINT('Ctrl Pts',(-5.56279658532076,6.70029419140152,-0.638543884031722));
#68490=CARTESIAN_POINT('Ctrl Pts',(-5.46364270534732,6.19042608101304,2.64202677478423));
#68491=CARTESIAN_POINT('Ctrl Pts',(-5.36448882537389,4.17439854579983,5.27978004503857));
#68492=CARTESIAN_POINT('Ctrl Pts',(-5.26533494540045,1.14272045108553,6.63293830167551));
#68493=CARTESIAN_POINT('Ctrl Pts',(-5.16618106542702,-2.16698683819769,
6.37227185438924));
#68494=CARTESIAN_POINT('Ctrl Pts',(-5.06702718545358,-4.94945616241849,
4.56120206080161));
#68495=CARTESIAN_POINT('Ctrl Pts',(-4.96787330548015,-6.52769980827313,
1.64037061551165));
#68496=CARTESIAN_POINT('Ctrl Pts',(-4.86871942550671,-6.51772376456351,
-1.67957062132176));
#68497=CARTESIAN_POINT('Ctrl Pts',(-4.76956554553327,-4.92195524907063,
-4.59086452308377));
#68498=CARTESIAN_POINT('Ctrl Pts',(-4.67041166555984,-2.12865215519214,
-6.38517975826516));
#68499=CARTESIAN_POINT('Ctrl Pts',(-4.5712577855864,1.18256189727929,-6.625951094165));
#68500=CARTESIAN_POINT('Ctrl Pts',(-4.47210390561296,4.20605314622856,-5.25459774618991));
#68501=CARTESIAN_POINT('Ctrl Pts',(-4.37295002563953,6.20619212433233,-2.60477635489854));
#68502=CARTESIAN_POINT('Ctrl Pts',(-4.27379614566609,6.69633572602634,0.67879922473925));
#68503=CARTESIAN_POINT('Ctrl Pts',(-4.17464226569266,5.5572297359225,3.7972197994509));
#68504=CARTESIAN_POINT('Ctrl Pts',(-4.07548838571922,3.06602393344096,5.99175915593496));
#68505=CARTESIAN_POINT('Ctrl Pts',(-3.97633450574579,-0.17115973609795,
6.72847567342724));
#68506=CARTESIAN_POINT('Ctrl Pts',(-3.87718062577234,-3.36669944667494,
5.82812280060413));
#68507=CARTESIAN_POINT('Ctrl Pts',(-3.77802674579892,-5.74310554095458,
3.5097605742586));
#68508=CARTESIAN_POINT('Ctrl Pts',(-3.67887286582547,-6.7221873759554,0.337457294645066));
#68509=CARTESIAN_POINT('Ctrl Pts',(-3.57971898585204,-6.06572979262974,
-2.91695091250557));
#68510=CARTESIAN_POINT('Ctrl Pts',(-3.4805651058786,-3.9334519707537,-5.46165141115185));
#68511=CARTESIAN_POINT('Ctrl Pts',(-3.38141122590517,-0.844147010468397,
-6.67750674787232));
#68512=CARTESIAN_POINT('Ctrl Pts',(-3.28225734593173,2.45054283917926,-6.26869367065504));
#68513=CARTESIAN_POINT('Ctrl Pts',(-3.1831034659583,5.1490042313889,-4.33467830043965));
#68514=CARTESIAN_POINT('Ctrl Pts',(-3.08394958598486,6.59468897299686,-1.34601556179596));
#68515=CARTESIAN_POINT('Ctrl Pts',(-2.98479570601143,6.43585525004679,1.97013901631542));
#68516=CARTESIAN_POINT('Ctrl Pts',(-2.88564182603798,4.71114804523789,4.80694961893865));
#68517=CARTESIAN_POINT('Ctrl Pts',(-2.78648794606455,1.84019663409828,6.47420704727741));
#68518=CARTESIAN_POINT('Ctrl Pts',(-2.68733406609112,-1.47848316725324,
6.56625982331739));
#68519=CARTESIAN_POINT('Ctrl Pts',(-2.58818018611768,-4.4374411453149,5.06071107899172));
#68520=CARTESIAN_POINT('Ctrl Pts',(-2.48902630614425,-6.31674907737723,
2.32386781823257));
#68521=CARTESIAN_POINT('Ctrl Pts',(-2.3898724261708,-6.65916261273149,-0.978383278864916));
#68522=CARTESIAN_POINT('Ctrl Pts',(-2.29071854619737,-5.38137094745038,
-4.04258917886792));
#68523=CARTESIAN_POINT('Ctrl Pts',(-2.19156466622393,-2.79426673002688,
-6.12321435070079));
#68524=CARTESIAN_POINT('Ctrl Pts',(-2.0924107862505,0.472695564341056,-6.71403302394436));
#68525=CARTESIAN_POINT('Ctrl Pts',(-1.99325690627706,3.62464883186855,-5.67129627058904));
#68526=CARTESIAN_POINT('Ctrl Pts',(-1.89410302630363,5.89470819930681,-3.24870678704439));
#68527=CARTESIAN_POINT('Ctrl Pts',(-1.79494914633019,6.73055767637759,-0.0356918494576151));
#68528=CARTESIAN_POINT('Ctrl Pts',(-1.69579526635676,5.92883120214271,3.18600708091843));
#68529=CARTESIAN_POINT('Ctrl Pts',(-1.59664138638331,3.68459255242263,5.63253568704139));
#68530=CARTESIAN_POINT('Ctrl Pts',(-1.49748750640989,0.543875416917607,
6.70864219302505));
#68531=CARTESIAN_POINT('Ctrl Pts',(-1.39833362643644,-2.7291691342452,6.15250488661704));
#68532=CARTESIAN_POINT('Ctrl Pts',(-1.29917974646301,-5.33819415594591,
4.09943455815411));
#68533=CARTESIAN_POINT('Ctrl Pts',(-1.20002586648957,-6.64841173946677,
1.04895275664998));
#68534=CARTESIAN_POINT('Ctrl Pts',(-1.10087198651614,-6.34103985976374,
-2.25674412374346));
#68535=CARTESIAN_POINT('Ctrl Pts',(-1.0017181065427,-4.49086352314854,-5.01336467450923));
#68536=CARTESIAN_POINT('Ctrl Pts',(-0.902564226569266,-1.54803922781885,
-6.55021030901278));
#68537=CARTESIAN_POINT('Ctrl Pts',(-0.80341034659583,1.771430203478,-6.49335934454339));
#68538=CARTESIAN_POINT('Ctrl Pts',(-0.704256466622392,4.65990243660605,
-4.8566438848732));
#68539=CARTESIAN_POINT('Ctrl Pts',(-0.605102586648959,6.41459875805902,
-2.03828440514837));
#68540=CARTESIAN_POINT('Ctrl Pts',(-0.50594870667552,6.60859340090657,1.27599913975567));
#68541=CARTESIAN_POINT('Ctrl Pts',(-0.406794826702084,5.19468656728889,
4.27982616595484));
#68542=CARTESIAN_POINT('Ctrl Pts',(-0.307640946728648,2.51688835851528,
6.24235160287639));
#68543=CARTESIAN_POINT('Ctrl Pts',(-0.208487066755212,-0.773280480777033,
6.68608389426968));
#68544=CARTESIAN_POINT('Ctrl Pts',(-0.109333186781774,-3.87530658661073,
5.50306091215922));
#68545=CARTESIAN_POINT('Ctrl Pts',(-0.0101793068083413,-6.03445259612738,
2.9811176441487));
#68546=CARTESIAN_POINT('Ctrl Pts',(0.0889745731650972,-6.72538825430939,
-0.26614539627899));
#68547=CARTESIAN_POINT('Ctrl Pts',(0.188128453138531,-5.78000570559087,
-3.44865402534091));
#68548=CARTESIAN_POINT('Ctrl Pts',(0.287282333111967,-3.42832091610777,
-5.79208910837369));
#68549=CARTESIAN_POINT('Ctrl Pts',(0.386436213085404,-0.242509720534929,
-6.72628200260807));
#68550=CARTESIAN_POINT('Ctrl Pts',(0.485590093058838,3.00230521668917,-6.02393923682869));
#68551=CARTESIAN_POINT('Ctrl Pts',(0.584743973032275,5.51664534666433,-3.85594406887471));
#68552=CARTESIAN_POINT('Ctrl Pts',(0.683897853005714,6.68876003471413,-0.749779795122723));
#68553=CARTESIAN_POINT('Ctrl Pts',(0.783051732979147,6.2334683318573,2.53880938608934));
#68554=CARTESIAN_POINT('Ctrl Pts',(0.882205612952585,4.26154482458082,5.20969444893381));
#68555=CARTESIAN_POINT('Ctrl Pts',(0.981359492926021,1.25276766331399,6.61303664929493));
#68556=CARTESIAN_POINT('Ctrl Pts',(1.08051337289946,-2.0608136905113,6.4073963102156));
#68557=CARTESIAN_POINT('Ctrl Pts',(1.17966725287289,-4.87298949936261,4.6428066815521));
#68558=CARTESIAN_POINT('Ctrl Pts',(1.27882113284633,-6.49954432421604,1.74860061784114));
#68559=CARTESIAN_POINT('Ctrl Pts',(1.37797501281977,-6.54472981958023,-1.57104809979206));
#68560=CARTESIAN_POINT('Ctrl Pts',(1.4771288927932,-4.99755214451164,-4.50845351601304));
#68561=CARTESIAN_POINT('Ctrl Pts',(1.57628277276664,-2.2344468151906,-6.34893124653652));
#68562=CARTESIAN_POINT('Ctrl Pts',(1.67543665274007,1.07230980499896,-6.64468450908441));
#68563=CARTESIAN_POINT('Ctrl Pts',(1.77459053271351,4.11816846792437,-5.32375516087627));
#68564=CARTESIAN_POINT('Ctrl Pts',(1.87374441268695,6.16205761052794,-2.70753144906902));
#68565=CARTESIAN_POINT('Ctrl Pts',(1.97289829266038,6.70668950896931,0.567447242873178));
#68566=CARTESIAN_POINT('Ctrl Pts',(2.07205217263382,5.61955269212147,3.70436338439326));
#68567=CARTESIAN_POINT('Ctrl Pts',(2.17120605260726,3.16515259811441,5.93999070485913));
#68568=CARTESIAN_POINT('Ctrl Pts',(2.27035993258069,-0.0593438275943384,
6.7303906909844));
#68569=CARTESIAN_POINT('Ctrl Pts',(2.36951381255413,-3.26940162435141,5.88325535412594));
#68570=CARTESIAN_POINT('Ctrl Pts',(2.46866769252756,-5.68399881700607,3.60469665733983));
#68571=CARTESIAN_POINT('Ctrl Pts',(2.567821572501,-6.71565269091494,0.449098517220573));
#68572=CARTESIAN_POINT('Ctrl Pts',(2.66697545247443,-6.11335706572648,-2.81576737854816));
#68573=CARTESIAN_POINT('Ctrl Pts',(2.76612933244788,-4.0236532651774,-5.39554398970022));
#68574=CARTESIAN_POINT('Ctrl Pts',(2.8652832124213,-0.954975932231545,-6.66255968168546));
#68575=CARTESIAN_POINT('Ctrl Pts',(2.96443709239475,2.3460514816286,-6.30854365037732));
#68576=CARTESIAN_POINT('Ctrl Pts',(3.06359097236817,5.07627367078402,-4.41962964086989));
#68577=CARTESIAN_POINT('Ctrl Pts',(3.16274485234162,6.57141489262633,-1.45539920714448));
#68578=CARTESIAN_POINT('Ctrl Pts',(3.26189873231505,6.46770034178368,1.86293661513677));
#68579=CARTESIAN_POINT('Ctrl Pts',(3.36105261228849,4.79036425033147,4.72801130416831));
#68580=CARTESIAN_POINT('Ctrl Pts',(3.46020649226192,1.94751028180179,6.44273887764077));
#68581=CARTESIAN_POINT('Ctrl Pts',(3.55936037223536,-1.36918198592865,6.58991815065725));
#68582=CARTESIAN_POINT('Ctrl Pts',(3.6585142522088,-4.35274591567518,5.13373972240108));
#68583=CARTESIAN_POINT('Ctrl Pts',(3.75766813218223,-6.27726654207255,2.42849856940638));
#68584=CARTESIAN_POINT('Ctrl Pts',(3.85682201215567,-6.67449905640789,-0.867607567605545));
#68585=CARTESIAN_POINT('Ctrl Pts',(3.9559758921291,-5.44779494137685,-3.95262075304505));
#68586=CARTESIAN_POINT('Ctrl Pts',(4.05512977210254,-2.89561700931341,-6.07594294564353));
#68587=CARTESIAN_POINT('Ctrl Pts',(4.15428365207598,0.361077996250999,-6.72095999336724));
#68588=CARTESIAN_POINT('Ctrl Pts',(4.25343753204941,3.52992104250486,-5.73073624822614));
#68589=CARTESIAN_POINT('Ctrl Pts',(4.35259141202285,5.83991791023889,-3.3461977548863));
#68590=CARTESIAN_POINT('Ctrl Pts',(4.45174529199628,6.72903559946889,-0.147513793017169));
#68591=CARTESIAN_POINT('Ctrl Pts',(4.55089917196972,5.98094770452458,3.08706094240574));
#68592=CARTESIAN_POINT('Ctrl Pts',(4.65005305194315,3.77766737191036,5.57053944284399));
#68593=CARTESIAN_POINT('Ctrl Pts',(4.7492069319166,0.655263162823926,6.69867975136916));
#68594=CARTESIAN_POINT('Ctrl Pts',(4.84836081189002,-2.62656989934376,6.19700028366044));
#68595=CARTESIAN_POINT('Ctrl Pts',(4.94751469186348,-5.26934575771189,4.18756160956527));
#68596=CARTESIAN_POINT('Ctrl Pts',(5.0466685718369,-6.63006636809895,1.15927022070139));
#68597=CARTESIAN_POINT('Ctrl Pts',(5.14582245181034,-6.37765898629265,-2.15107792670036));
#68598=CARTESIAN_POINT('Ctrl Pts',(5.24497633178377,-4.5735415002168,-4.93805702383651));
#68599=CARTESIAN_POINT('Ctrl Pts',(5.34413021175721,-1.65665245844824,-6.52358738631149));
#68600=CARTESIAN_POINT('Ctrl Pts',(5.44328409173065,1.66329298767028,-6.52189189110945));
#68601=CARTESIAN_POINT('Ctrl Pts',(5.54243797170408,4.57858025049396,-4.93340285042299));
#68602=CARTESIAN_POINT('Ctrl Pts',(5.64159185167752,6.37982203407842,-2.14456870220543));
#68603=CARTESIAN_POINT('Ctrl Pts',(5.74074573165094,6.62893124127026,1.16600000870917));
#68604=CARTESIAN_POINT('Ctrl Pts',(5.8398996116244,5.26498167626374,4.19297054663797));
#68605=CARTESIAN_POINT('Ctrl Pts',(5.93905349159781,2.62044555173564,6.19958558531679));
#68606=CARTESIAN_POINT('Ctrl Pts',(6.03820737157128,-0.662478785766676,
6.69819537944482));
#68607=CARTESIAN_POINT('Ctrl Pts',(6.10430995822022,-2.74237358747327,5.94349985274467));
#68608=CARTESIAN_POINT('Ctrl Pts',(6.1373612515447,-3.62961150141922,5.34049826419562));
#68609=CARTESIAN_POINT('Ctrl Pts',(-13.7543612515447,-2.91658447331021,
6.02641484220292));
#68610=CARTESIAN_POINT('Ctrl Pts',(-13.7213099582202,-3.91777639748254,
5.54187122924162));
#68611=CARTESIAN_POINT('Ctrl Pts',(-13.6552073715713,-5.67301223427239,
4.06468607685024));
#68612=CARTESIAN_POINT('Ctrl Pts',(-13.5560534915978,-6.92572470924536,
0.85775399420773));
#68613=CARTESIAN_POINT('Ctrl Pts',(-13.4568996116244,-6.49329434006559,
-2.55693738998599));
#68614=CARTESIAN_POINT('Ctrl Pts',(-13.357745731651,-4.48105928763902,-5.34997692910876));
#68615=CARTESIAN_POINT('Ctrl Pts',(-13.2585918516775,-1.37853879660337,
-6.84110526922471));
#68616=CARTESIAN_POINT('Ctrl Pts',(-13.1594379717041,2.05937474645172,-6.66788307039378));
#68617=CARTESIAN_POINT('Ctrl Pts',(-13.0602840917306,4.99623896323877,-4.87227088226356));
#68618=CARTESIAN_POINT('Ctrl Pts',(-12.9611302117572,6.71749186984302,-1.89124511612268));
#68619=CARTESIAN_POINT('Ctrl Pts',(-12.8619763317837,6.80434942795133,1.54994618879328));
#68620=CARTESIAN_POINT('Ctrl Pts',(-12.7628224518104,5.23567631631225,4.61401970147312));
#68621=CARTESIAN_POINT('Ctrl Pts',(-12.6636685718369,2.39313926820875,6.55548526950676));
#68622=CARTESIAN_POINT('Ctrl Pts',(-12.5645146918635,-1.03165990650043,
6.90196850037429));
#68623=CARTESIAN_POINT('Ctrl Pts',(-12.46536081189,-4.20545131707893,5.56917192602596));
#68624=CARTESIAN_POINT('Ctrl Pts',(-12.3662069319166,-6.35603694455473,
2.88136933138902));
#68625=CARTESIAN_POINT('Ctrl Pts',(-12.2670530519432,-6.96016922377503,
-0.507483488838575));
#68626=CARTESIAN_POINT('Ctrl Pts',(-12.1678991719697,-5.87086001146276,
-3.77286338327458));
#68627=CARTESIAN_POINT('Ctrl Pts',(-12.0687452919963,-3.35314327542756,
-6.12028800364231));
#68628=CARTESIAN_POINT('Ctrl Pts',(-11.9695914120228,-0.0195912067993729,
-6.97861816317637));
#68629=CARTESIAN_POINT('Ctrl Pts',(-11.8704375320494,3.31872749565981,-6.1390180798525));
#68630=CARTESIAN_POINT('Ctrl Pts',(-11.771283652076,5.84958437923409,-3.80576638892909));
#68631=CARTESIAN_POINT('Ctrl Pts',(-11.6721297721025,6.95721020808646,-0.546554048803889));
#68632=CARTESIAN_POINT('Ctrl Pts',(-11.5729758921291,6.37211447138913,2.84563742743775));
#68633=CARTESIAN_POINT('Ctrl Pts',(-11.4738220121557,4.23665368056203,5.54547209901134));
#68634=CARTESIAN_POINT('Ctrl Pts',(-11.3746681321822,1.07039536664217,6.89606764505803));
#68635=CARTESIAN_POINT('Ctrl Pts',(-11.2755142522088,-2.35629511275388,
6.56881789592747));
#68636=CARTESIAN_POINT('Ctrl Pts',(-11.1763603722354,-5.20968804442629,
4.64334423525892));
#68637=CARTESIAN_POINT('Ctrl Pts',(-11.0772064922619,-6.79553967185065,
1.58812335034336));
#68638=CARTESIAN_POINT('Ctrl Pts',(-10.9780526122885,-6.7280049265849,-1.85349532383051));
#68639=CARTESIAN_POINT('Ctrl Pts',(-10.8788987323151,-5.02351532589454,
-4.84414997476734));
#68640=CARTESIAN_POINT('Ctrl Pts',(-10.7797448523416,-2.09678110830378,
-6.656200432038));
#68641=CARTESIAN_POINT('Ctrl Pts',(-10.6805909723682,1.34010969410712,-6.84876640098948));
#68642=CARTESIAN_POINT('Ctrl Pts',(-10.5814370923947,4.45094558209592,-5.37499568677053));
#68643=CARTESIAN_POINT('Ctrl Pts',(-10.4822832124213,6.47884573187826,-2.59346355094835));
#68644=CARTESIAN_POINT('Ctrl Pts',(-10.3831293324479,6.93041261584803,0.819070315461309));
#68645=CARTESIAN_POINT('Ctrl Pts',(-10.2839754524744,5.69577791325833,4.03232056890508));
#68646=CARTESIAN_POINT('Ctrl Pts',(-10.184821572501,3.07533398308171,6.26448849468798));
#68647=CARTESIAN_POINT('Ctrl Pts',(-10.0856676925276,-0.293352992482243,
6.97247726632205));
#68648=CARTESIAN_POINT('Ctrl Pts',(-9.98651381255412,-3.59066582212385,
5.98402992651335));
#68649=CARTESIAN_POINT('Ctrl Pts',(-9.8873599325807,-6.01435297582444,3.53964030513942));
#68650=CARTESIAN_POINT('Ctrl Pts',(-9.78820605260725,-6.97472010918838,
0.234039753159747));
#68651=CARTESIAN_POINT('Ctrl Pts',(-9.68905217263381,-6.23810543702052,
-3.12850375805924));
#68652=CARTESIAN_POINT('Ctrl Pts',(-9.58989829266039,-3.98373073120386,
-5.72986777062419));
#68653=CARTESIAN_POINT('Ctrl Pts',(-9.49074441268694,-0.760095830976685,
-6.93712833493136));
#68654=CARTESIAN_POINT('Ctrl Pts',(-9.39159053271351,2.64847391615979,-6.45655334702634));
#68655=CARTESIAN_POINT('Ctrl Pts',(-9.29243665274007,5.41265765528602,-4.40506893410868));
#68656=CARTESIAN_POINT('Ctrl Pts',(-9.19328277276664,6.85991664090245,-1.28181078457213));
#68657=CARTESIAN_POINT('Ctrl Pts',(-9.0941288927932,6.6381260381719,2.15331788385273));
#68658=CARTESIAN_POINT('Ctrl Pts',(-8.99497501281976,4.8012485311275,5.06453430731019));
#68659=CARTESIAN_POINT('Ctrl Pts',(-8.89582113284634,1.79620495094906,6.74352600512238));
#68660=CARTESIAN_POINT('Ctrl Pts',(-8.79666725287289,-1.64586363855569,
6.78178649699738));
#68661=CARTESIAN_POINT('Ctrl Pts',(-8.69751337289946,-4.68748595849105,
5.17000682751243));
#68662=CARTESIAN_POINT('Ctrl Pts',(-8.59835949292602,-6.58862116772988,
2.30034047821565));
#68663=CARTESIAN_POINT('Ctrl Pts',(-8.49920561295258,-6.88671423762183,
-1.12900939629063));
#68664=CARTESIAN_POINT('Ctrl Pts',(-8.40005173297915,-5.50923773938943,
-4.28366603955806));
#68665=CARTESIAN_POINT('Ctrl Pts',(-8.30089785300571,-2.79133810449572,
-6.39608683446105));
#68666=CARTESIAN_POINT('Ctrl Pts',(-8.20174397303227,0.605707059144963,
-6.95230998777225));
#68667=CARTESIAN_POINT('Ctrl Pts',(-8.10259009305884,3.85538088131818,-5.81700382220452));
#68668=CARTESIAN_POINT('Ctrl Pts',(-8.0034362130854,6.16702262384234,-3.26639360221523));
#68669=CARTESIAN_POINT('Ctrl Pts',(-7.90428233311197,6.97819911139855,0.0789453561161987));
#68670=CARTESIAN_POINT('Ctrl Pts',(-7.80512845313852,6.09154733602257,3.40507654254235));
#68671=CARTESIAN_POINT('Ctrl Pts',(-7.7059745731651,3.72279379384625,5.90273678695532));
#68672=CARTESIAN_POINT('Ctrl Pts',(-7.60682069319165,0.448267226372286,
6.96423374832697));
#68673=CARTESIAN_POINT('Ctrl Pts',(-7.50766681321823,-2.9353248398258,6.33130028448165));
#68674=CARTESIAN_POINT('Ctrl Pts',(-7.40851293324478,-5.60473873564142,
4.15793204763815));
#68675=CARTESIAN_POINT('Ctrl Pts',(-7.30935905327135,-6.91049365873169,
0.972919626795923));
#68676=CARTESIAN_POINT('Ctrl Pts',(-7.21020517329792,-6.53489337006783,
-2.44880865920948));
#68677=CARTESIAN_POINT('Ctrl Pts',(-7.11105129332448,-4.56932316483537,
-5.27473042182012));
#68678=CARTESIAN_POINT('Ctrl Pts',(-7.01189741335104,-1.49201540556034,
-6.81728576760183));
#68679=CARTESIAN_POINT('Ctrl Pts',(-6.9127435333776,1.94830663345238,-6.70116381456395));
#68680=CARTESIAN_POINT('Ctrl Pts',(-6.81358965340418,4.91459661715582,-4.95461757335684));
#68681=CARTESIAN_POINT('Ctrl Pts',(-6.71443577343073,6.68514241180503,-2.00258985852354));
#68682=CARTESIAN_POINT('Ctrl Pts',(-6.6152818934573,6.82916200000809,1.43667727246641));
#68683=CARTESIAN_POINT('Ctrl Pts',(-6.51612801348386,5.31161474687281,4.52639414858881));
#68684=CARTESIAN_POINT('Ctrl Pts',(-6.41697413351043,2.50172694926709,6.51481829975991));
#68685=CARTESIAN_POINT('Ctrl Pts',(-6.31782025353699,-0.916842637550795,
6.91815689223255));
#68686=CARTESIAN_POINT('Ctrl Pts',(-6.21866637356355,-4.11234015120979,
5.63827577263862));
#68687=CARTESIAN_POINT('Ctrl Pts',(-6.11951249359012,-6.30728620108067,
2.98657596341246));
#68688=CARTESIAN_POINT('Ctrl Pts',(-6.02035861361668,-6.9676402160088,-0.391771652665847));
#68689=CARTESIAN_POINT('Ctrl Pts',(-5.92120473364325,-5.93273499630734,
-3.67479940556843));
#68690=CARTESIAN_POINT('Ctrl Pts',(-5.82205085366981,-3.4543677898643,-6.06373139081241));
#68691=CARTESIAN_POINT('Ctrl Pts',(-5.72289697369637,-0.135536851938726,
-6.97732935795225));
#68692=CARTESIAN_POINT('Ctrl Pts',(-5.62374309372294,3.21627083173698,-6.19331067721406));
#68693=CARTESIAN_POINT('Ctrl Pts',(-5.5245892137495,5.78554487998695,-3.90243073599426));
#68694=CARTESIAN_POINT('Ctrl Pts',(-5.42543533377606,6.94716898060797,-0.662071266899751));
#68695=CARTESIAN_POINT('Ctrl Pts',(-5.32628145380263,6.4185145932771,2.73937321726426));
#68696=CARTESIAN_POINT('Ctrl Pts',(-5.22712757382919,4.3282057864402,5.4743154711618));
#68697=CARTESIAN_POINT('Ctrl Pts',(-5.12797369385576,1.18482440390089,6.87733133849872));
#68698=CARTESIAN_POINT('Ctrl Pts',(-5.02881981388231,-2.24683026053273,
6.60706054065878));
#68699=CARTESIAN_POINT('Ctrl Pts',(-4.92966593390888,-5.13182068431539,
4.72926121837316));
#68700=CARTESIAN_POINT('Ctrl Pts',(-4.83051205393545,-6.76821529433023,
1.70081067058338));
#68701=CARTESIAN_POINT('Ctrl Pts',(-4.73135817396201,-6.75787167964274,
-1.7414550149396));
#68702=CARTESIAN_POINT('Ctrl Pts',(-4.63220429398857,-5.10330648976053,
-4.76001660492311));
#68703=CARTESIAN_POINT('Ctrl Pts',(-4.53305041401514,-2.20708312211616,
-6.62044404097231));
#68704=CARTESIAN_POINT('Ctrl Pts',(-4.43389653404171,1.22613382274623,-6.87008668477287));
#68705=CARTESIAN_POINT('Ctrl Pts',(-4.33474265406826,4.36102671219507,-5.44820532130507));
#68706=CARTESIAN_POINT('Ctrl Pts',(-4.23558877409484,6.43486154222677,-2.70075029203863));
#68707=CARTESIAN_POINT('Ctrl Pts',(-4.13643489412139,6.94306466412877,0.703809830353542));
#68708=CARTESIAN_POINT('Ctrl Pts',(-4.03728101414796,5.76198789734599,3.93712975128002));
#68709=CARTESIAN_POINT('Ctrl Pts',(-3.93812713417452,3.1789927062512,6.21252771270901));
#68710=CARTESIAN_POINT('Ctrl Pts',(-3.83897325420109,-0.177466179152926,
6.97638881964248));
#68711=CARTESIAN_POINT('Ctrl Pts',(-3.73981937422764,-3.49074671870157,
6.04286211603823));
#68712=CARTESIAN_POINT('Ctrl Pts',(-3.64066549425422,-5.95471236437332,
3.63907898583629));
#68713=CARTESIAN_POINT('Ctrl Pts',(-3.54151161428077,-6.9698688275512,0.349891032045548));
#68714=CARTESIAN_POINT('Ctrl Pts',(-3.44235773430735,-6.28922382455756,
-3.02442703535618));
#68715=CARTESIAN_POINT('Ctrl Pts',(-3.3432038543339,-4.07838144674295,-5.66288795425431));
#68716=CARTESIAN_POINT('Ctrl Pts',(-3.24404997436047,-0.875249915701455,
-6.92354192539052));
#68717=CARTESIAN_POINT('Ctrl Pts',(-3.14489609438703,2.54083398604264,-6.49966598087521));
#68718=CARTESIAN_POINT('Ctrl Pts',(-3.0457422144136,5.33872117484468,-4.49439110724032));
#68719=CARTESIAN_POINT('Ctrl Pts',(-2.94658833444016,6.83767269932039,-1.39560999729307));
#68720=CARTESIAN_POINT('Ctrl Pts',(-2.84743445446673,6.67298668977635,2.04272950868281));
#68721=CARTESIAN_POINT('Ctrl Pts',(-2.74828057449329,4.88473201742842,4.9840634351386));
#68722=CARTESIAN_POINT('Ctrl Pts',(-2.64912669451986,1.90799935188411,6.71275157299788));
#68723=CARTESIAN_POINT('Ctrl Pts',(-2.54997281454641,-1.53295842010545,
6.80819606722689));
#68724=CARTESIAN_POINT('Ctrl Pts',(-2.45081893457298,-4.60094028670655,
5.2471748289662));
#68725=CARTESIAN_POINT('Ctrl Pts',(-2.35166505459954,-6.54949200662783,
2.40949157763498));
#68726=CARTESIAN_POINT('Ctrl Pts',(-2.25251117462611,-6.90452189388355,
-1.01443216848572));
#68727=CARTESIAN_POINT('Ctrl Pts',(-2.15335729465267,-5.57964952751609,
-4.19153985519224));
#68728=CARTESIAN_POINT('Ctrl Pts',(-2.05420341467924,-2.89722250931899,
-6.3488264221879));
#68729=CARTESIAN_POINT('Ctrl Pts',(-1.9550495347058,0.490112205233504,-6.96141402545897));
#68730=CARTESIAN_POINT('Ctrl Pts',(-1.85589565473236,3.75820034330266,-5.88025725518668));
#68731=CARTESIAN_POINT('Ctrl Pts',(-1.75674177475893,6.11190087810066,-3.36840657638715));
#68732=CARTESIAN_POINT('Ctrl Pts',(-1.65758789478549,6.97854753475277,-0.0370069287003618));
#68733=CARTESIAN_POINT('Ctrl Pts',(-1.55843401481206,6.14728115545192,3.30339667666503));
#68734=CARTESIAN_POINT('Ctrl Pts',(-1.45928013483862,3.82035271215688,5.84006852376676));
#68735=CARTESIAN_POINT('Ctrl Pts',(-1.36012625486519,0.563914705502657,
6.95582456740348));
#68736=CARTESIAN_POINT('Ctrl Pts',(-1.26097237489175,-2.82972636882007,
6.37919617860903));
#68737=CARTESIAN_POINT('Ctrl Pts',(-1.16181849491831,-5.53488187134256,
4.25047972326176));
#68738=CARTESIAN_POINT('Ctrl Pts',(-1.06266461494487,-6.8933749007627,1.08760180448103));
#68739=CARTESIAN_POINT('Ctrl Pts',(-0.96351073497144,-6.57467779177244,
-2.33989468608098));
#68740=CARTESIAN_POINT('Ctrl Pts',(-0.864356854998002,-4.65633103158349,
-5.1980839289));
#68741=CARTESIAN_POINT('Ctrl Pts',(-0.765202975024568,-1.60507729915334,
-6.79155520269978));
#68742=CARTESIAN_POINT('Ctrl Pts',(-0.666049095051131,1.83669919698557,
-6.73260954365901));
#68743=CARTESIAN_POINT('Ctrl Pts',(-0.566895215077694,4.83159824561038,
-5.03558870447046));
#68744=CARTESIAN_POINT('Ctrl Pts',(-0.46774133510426,6.65094699456959,-2.11338573928228));
#68745=CARTESIAN_POINT('Ctrl Pts',(-0.368587455130822,6.85208944096011,
1.32301379458366));
#68746=CARTESIAN_POINT('Ctrl Pts',(-0.269433575157385,5.38608669311305,
4.43751792580564));
#68747=CARTESIAN_POINT('Ctrl Pts',(-0.17027969518395,2.6096240302955,6.47235332997821));
#68748=CARTESIAN_POINT('Ctrl Pts',(-0.0711258152105136,-0.801772282813753,
6.93243509988283));
#68749=CARTESIAN_POINT('Ctrl Pts',(0.0280280647629242,-4.01809367466241,
5.70582320346624));
#68750=CARTESIAN_POINT('Ctrl Pts',(0.127181944736357,-6.25679420831466,
3.09095801368702));
#68751=CARTESIAN_POINT('Ctrl Pts',(0.226335824709796,-6.97318764343842,
-0.275951620711471));
#68752=CARTESIAN_POINT('Ctrl Pts',(0.325489704683229,-5.9929721290669,-3.57572094378226));
#68753=CARTESIAN_POINT('Ctrl Pts',(0.424643584656666,-3.55463865370539,
-6.00550074924309));
#68754=CARTESIAN_POINT('Ctrl Pts',(0.523797464630102,-0.251445079853116,
-6.97411432221995));
#68755=CARTESIAN_POINT('Ctrl Pts',(0.622951344603537,3.11292625008419,-6.24589348044878));
#68756=CARTESIAN_POINT('Ctrl Pts',(0.722105224576973,5.71990816142732,-3.99801773788122));
#68757=CARTESIAN_POINT('Ctrl Pts',(0.821259104550414,6.93520984370039,-0.777405705804355));
#68758=CARTESIAN_POINT('Ctrl Pts',(0.920412984523845,6.46314275159058,2.63235274614514));
#68759=CARTESIAN_POINT('Ctrl Pts',(1.01956686449728,4.41856300172481,5.40164754564424));
#68760=CARTESIAN_POINT('Ctrl Pts',(1.11872074447072,1.29892634589875,6.85669640245985));
#68761=CARTESIAN_POINT('Ctrl Pts',(1.21787462444416,-2.1367451244014,6.64347916990207));
#68762=CARTESIAN_POINT('Ctrl Pts',(1.31702850441759,-5.05253657910191,4.81387259121105));
#68763=CARTESIAN_POINT('Ctrl Pts',(1.41618238439103,-6.73902241116898,1.81302844691914));
#68764=CARTESIAN_POINT('Ctrl Pts',(1.51533626436446,-6.78587278263037,-1.62893394142675));
#68765=CARTESIAN_POINT('Ctrl Pts',(1.6144901443379,-5.18168878045337,-4.6745691341662));
#68766=CARTESIAN_POINT('Ctrl Pts',(1.71364402431134,-2.31677582504233,-6.58285993957605));
#68767=CARTESIAN_POINT('Ctrl Pts',(1.81279790428477,1.11181945181607,-6.88951033921419));
#68768=CARTESIAN_POINT('Ctrl Pts',(1.91195178425821,4.26990389078685,-5.5199108662205));
#68769=CARTESIAN_POINT('Ctrl Pts',(2.01110566423164,6.38910087612505,-2.80729143522257));
#68770=CARTESIAN_POINT('Ctrl Pts',(2.11025954420508,6.95379993598976,0.588355044003722));
#68771=CARTESIAN_POINT('Ctrl Pts',(2.20941342417852,5.82660716565228,3.84085200765993));
#68772=CARTESIAN_POINT('Ctrl Pts',(2.30856730415196,3.28177380281742,6.158851834126));
#68773=CARTESIAN_POINT('Ctrl Pts',(2.40772118412539,-0.0615303726189893,
6.97837439672171));
#68774=CARTESIAN_POINT('Ctrl Pts',(2.50687506409883,-3.38986392254105,6.10002604865179));
#68775=CARTESIAN_POINT('Ctrl Pts',(2.60602894407226,-5.89342783157066,3.73751302360866));
#68776=CARTESIAN_POINT('Ctrl Pts',(2.7051828240457,-6.96309336965125,0.465645716284481));
#68777=CARTESIAN_POINT('Ctrl Pts',(2.80433670401913,-6.33860594194476,-2.91951535709594));
#68778=CARTESIAN_POINT('Ctrl Pts',(2.90349058399257,-4.17190624083858,-5.59434478068947));
#68779=CARTESIAN_POINT('Ctrl Pts',(3.002644463966,-0.990162369607622,-6.90804412908513));
#68780=CARTESIAN_POINT('Ctrl Pts',(3.10179834393944,2.43249260621947,-6.54098424767011));
#68781=CARTESIAN_POINT('Ctrl Pts',(3.20095222391288,5.26331083014297,-4.58247251086813));
#68782=CARTESIAN_POINT('Ctrl Pts',(3.30010610388631,6.81354107694928,-1.5090239230467));
#68783=CARTESIAN_POINT('Ctrl Pts',(3.39925998385975,6.70600512556131,1.93157719583798));
#68784=CARTESIAN_POINT('Ctrl Pts',(3.49841386383318,4.96686697256125,4.90221660929955));
#68785=CARTESIAN_POINT('Ctrl Pts',(3.59756774380662,2.01926701017267,6.68012394714576));
#68786=CARTESIAN_POINT('Ctrl Pts',(3.69672162378006,-1.41962999679287,6.83272609428742));
#68787=CARTESIAN_POINT('Ctrl Pts',(3.7958755037535,-4.51312443036494,5.3228942394423));
#68788=CARTESIAN_POINT('Ctrl Pts',(3.89502938372693,-6.50855472287447,2.5179774870903));
#68789=CARTESIAN_POINT('Ctrl Pts',(3.99418326370037,-6.92042341443442,-0.899574885643797));
#68790=CARTESIAN_POINT('Ctrl Pts',(4.0933371436738,-5.64852093778436,-4.09825650982619));
#68791=CARTESIAN_POINT('Ctrl Pts',(4.19249102364723,-3.00230707670095,-6.29981328492818));
#68792=CARTESIAN_POINT('Ctrl Pts',(4.29164490362068,0.374382047038171,-6.96859622160285));
#68793=CARTESIAN_POINT('Ctrl Pts',(4.39079878359411,3.65998227390602,-5.94188732053192));
#68794=CARTESIAN_POINT('Ctrl Pts',(4.48995266356754,6.05509182079991,-3.4694896345833));
#68795=CARTESIAN_POINT('Ctrl Pts',(4.58910654354098,6.97696937636385,-0.152948992654073));
#68796=CARTESIAN_POINT('Ctrl Pts',(4.68826042351442,6.2013179094186,3.2008048315027));
#68797=CARTESIAN_POINT('Ctrl Pts',(4.78741430348786,3.91685690739814,5.77578800528519));
#68798=CARTESIAN_POINT('Ctrl Pts',(4.8865681834613,0.67940657363186,6.94549505594236));
#68799=CARTESIAN_POINT('Ctrl Pts',(4.98572206343472,-2.72334682759693,6.42533102482466));
#68800=CARTESIAN_POINT('Ctrl Pts',(5.08487594340817,-5.46349672870364,4.34185384810268));
#68801=CARTESIAN_POINT('Ctrl Pts',(5.1840298233816,-6.87435358747951,1.20198395582908));
#68802=CARTESIAN_POINT('Ctrl Pts',(5.28318370335504,-6.61264616340679,-2.23033517937476));
#68803=CARTESIAN_POINT('Ctrl Pts',(5.38233758332847,-4.74205530894508,-5.12000154030467));
#68804=CARTESIAN_POINT('Ctrl Pts',(5.48149146330192,-1.71769242397583,-6.76395134867786));
#68805=CARTESIAN_POINT('Ctrl Pts',(5.58064534327534,1.7245776259249,-6.76219338233518));
#68806=CARTESIAN_POINT('Ctrl Pts',(5.67979922324879,4.74727971381842,-5.11517588217014));
#68807=CARTESIAN_POINT('Ctrl Pts',(5.77895310322222,6.61488890947906,-2.22358612012347));
#68808=CARTESIAN_POINT('Ctrl Pts',(5.87810698319565,6.8731766364878,1.20896170533647));
#68809=CARTESIAN_POINT('Ctrl Pts',(5.9772608631691,5.45897185107899,4.34746207943939));
#68810=CARTESIAN_POINT('Ctrl Pts',(6.07641474314252,2.71699682616207,6.42801158286575));
#68811=CARTESIAN_POINT('Ctrl Pts',(6.17556862311597,-0.686888058840034,
6.94499283715739));
#68812=CARTESIAN_POINT('Ctrl Pts',(6.24167120976492,-2.84341734495507,6.16249027784839));
#68813=CARTESIAN_POINT('Ctrl Pts',(6.2747225030894,-3.76334586422734,5.53727087530317));
#68814=CARTESIAN_POINT('Ctrl Pts',(-13.617,-3.02022829989065,6.2405696868587));
#68815=CARTESIAN_POINT('Ctrl Pts',(-13.5839487066755,-4.05699860799537,
5.73880731865407));
#68816=CARTESIAN_POINT('Ctrl Pts',(-13.5178461200266,-5.87460855406983,
4.20912887379586));
#68817=CARTESIAN_POINT('Ctrl Pts',(-13.4186922400531,-7.17183745423105,
0.88823516389027));
#68818=CARTESIAN_POINT('Ctrl Pts',(-13.3195383600797,-6.72404022748158,
-2.64780078785767));
#68819=CARTESIAN_POINT('Ctrl Pts',(-13.2203844801063,-4.64029833452928,
-5.54009385735964));
#68820=CARTESIAN_POINT('Ctrl Pts',(-13.1212306001328,-1.4275265894402,-7.08421097544739));
#68821=CARTESIAN_POINT('Ctrl Pts',(-13.0220767201594,2.13255674444923,-6.90483314776367));
#68822=CARTESIAN_POINT('Ctrl Pts',(-12.922922840186,5.17378544934233,-5.04541203520993));
#68823=CARTESIAN_POINT('Ctrl Pts',(-12.8237689602125,6.95620484688339,-1.95845245492269));
#68824=CARTESIAN_POINT('Ctrl Pts',(-12.7246150802391,7.04614897758106,1.60502511946383));
#68825=CARTESIAN_POINT('Ctrl Pts',(-12.6254612002656,5.42173145482275,4.77798363330997));
#68826=CARTESIAN_POINT('Ctrl Pts',(-12.5263073202922,2.47818193149074,6.78844117551293));
#68827=CARTESIAN_POINT('Ctrl Pts',(-12.4271534403188,-1.06832100149623,
7.14723704406392));
#68828=CARTESIAN_POINT('Ctrl Pts',(-12.3279995603453,-4.35489635149795,
5.76707817375509));
#68829=CARTESIAN_POINT('Ctrl Pts',(-12.2288456803719,-6.58190524936427,
2.98376175171135));
#68830=CARTESIAN_POINT('Ctrl Pts',(-12.1296918003985,-7.20750598998253,
-0.52551743614608));
#68831=CARTESIAN_POINT('Ctrl Pts',(-12.030537920425,-6.07948705534731,-3.90693596090304));
#68832=CARTESIAN_POINT('Ctrl Pts',(-11.9313840404516,-3.47230066768488,
-6.33777872756158));
#68833=CARTESIAN_POINT('Ctrl Pts',(-11.8322301604781,-0.0202874004665461,
-7.22661053140516));
#68834=CARTESIAN_POINT('Ctrl Pts',(-11.7330762805047,3.4366618878146,-6.35717439627847));
#68835=CARTESIAN_POINT('Ctrl Pts',(-11.6339224005313,6.05745537166277,-3.94100820867734));
#68836=CARTESIAN_POINT('Ctrl Pts',(-11.5347685205578,7.20444182263055,-0.565976408611909));
#68837=CARTESIAN_POINT('Ctrl Pts',(-11.4356146405844,6.59855410763732,2.9467600778321));
#68838=CARTESIAN_POINT('Ctrl Pts',(-11.3364607606109,4.38720752303357,5.7425361490316));
#68839=CARTESIAN_POINT('Ctrl Pts',(-11.2373068806376,1.10843296602187,7.14112649578979));
#68840=CARTESIAN_POINT('Ctrl Pts',(-11.1381530006641,-2.44002848110766,
6.80224759051522));
#68841=CARTESIAN_POINT('Ctrl Pts',(-11.0389991206907,-5.39481966298761,
4.80835024454017));
#68842=CARTESIAN_POINT('Ctrl Pts',(-10.9398452407172,-7.03702615774369,
1.64455894568363));
#68843=CARTESIAN_POINT('Ctrl Pts',(-10.8406913607438,-6.9670914959007,-1.91936118496661));
#68844=CARTESIAN_POINT('Ctrl Pts',(-10.7415374807704,-5.20203110557652,
-5.01629182236644));
#68845=CARTESIAN_POINT('Ctrl Pts',(-10.6423836007969,-2.17129237981159,
-6.89273535484788));
#68846=CARTESIAN_POINT('Ctrl Pts',(-10.5432297208235,1.38773186929381,-7.09214435340263));
#68847=CARTESIAN_POINT('Ctrl Pts',(-10.4440758408501,4.60911450751237,-5.56600168228627));
#68848=CARTESIAN_POINT('Ctrl Pts',(-10.3449219608766,6.70907817315371,-2.68562494348715));
#68849=CARTESIAN_POINT('Ctrl Pts',(-10.2457680809032,7.17669195041253,0.848176820865036));
#68850=CARTESIAN_POINT('Ctrl Pts',(-10.1466142009297,5.89818323485443,4.17561322426439));
#68851=CARTESIAN_POINT('Ctrl Pts',(-10.0474603209563,3.18461913663593,6.48710353124882));
#68852=CARTESIAN_POINT('Ctrl Pts',(-9.94830644098287,-0.303777592543674,
7.22025141147022));
#68853=CARTESIAN_POINT('Ctrl Pts',(-9.84915256100942,-3.71826382217565,
6.19667857963189));
#68854=CARTESIAN_POINT('Ctrl Pts',(-9.749998681036,-6.22807918966268,3.66542506100721));
#68855=CARTESIAN_POINT('Ctrl Pts',(-9.65084480106256,-7.22257395606273,
0.242356596306747));
#68856=CARTESIAN_POINT('Ctrl Pts',(-9.55169092108911,-6.45978292451376,
-3.23967835420889));
#68857=CARTESIAN_POINT('Ctrl Pts',(-9.45253704111569,-4.12529669674559,
-5.9334845103353));
#68858=CARTESIAN_POINT('Ctrl Pts',(-9.35338316114224,-0.787106617467268,
-7.18364631947511));
#68859=CARTESIAN_POINT('Ctrl Pts',(-9.25422928116881,2.7425901585595,-6.68599360549662));
#68860=CARTESIAN_POINT('Ctrl Pts',(-9.15507540119538,5.60500200755747,-4.56160758569233));
#68861=CARTESIAN_POINT('Ctrl Pts',(-9.05592152122194,7.1036908285498,-1.3273612480958));
#68862=CARTESIAN_POINT('Ctrl Pts',(-8.9567676412485,6.87401866882103,2.22983824778147));
#68863=CARTESIAN_POINT('Ctrl Pts',(-8.85761376127506,4.97186583183785,5.24450773865122));
#68864=CARTESIAN_POINT('Ctrl Pts',(-8.75845988130163,1.86003493980857,6.98316413191473));
#68865=CARTESIAN_POINT('Ctrl Pts',(-8.65930600132819,-1.7043510943762,7.02278424968813));
#68866=CARTESIAN_POINT('Ctrl Pts',(-8.56015212135476,-4.85406058927098,
5.35372833325108));
#68867=CARTESIAN_POINT('Ctrl Pts',(-8.46099824138132,-6.82275459193258,
2.38208544112758));
#68868=CARTESIAN_POINT('Ctrl Pts',(-8.36184436140789,-7.13144070540802,
-1.16912990545044));
#68869=CARTESIAN_POINT('Ctrl Pts',(-8.26269048143445,-5.70501416420314,
-4.43589051452024));
#68870=CARTESIAN_POINT('Ctrl Pts',(-8.16353660146102,-2.89053117264693,
-6.62337835326697));
#68871=CARTESIAN_POINT('Ctrl Pts',(-8.06438272148757,0.627231481965904,
-7.19936746795161));
#68872=CARTESIAN_POINT('Ctrl Pts',(-7.96522884151415,3.99238580304136,-6.02371703105673));
#68873=CARTESIAN_POINT('Ctrl Pts',(-7.8660749615407,6.38617411051875,-3.38246825568388));
#68874=CARTESIAN_POINT('Ctrl Pts',(-7.76692108156728,7.22617658819175,0.0817507604764866));
#68875=CARTESIAN_POINT('Ctrl Pts',(-7.66776720159382,6.30801673078173,3.52607943681746));
#68876=CARTESIAN_POINT('Ctrl Pts',(-7.56861332162041,3.85508709715878,6.11249660481615));
#68877=CARTESIAN_POINT('Ctrl Pts',(-7.46945944164694,0.46419686293761,7.21171495159147));
#68878=CARTESIAN_POINT('Ctrl Pts',(-7.37030556167353,-3.03963462458951,
6.55628954665409));
#68879=CARTESIAN_POINT('Ctrl Pts',(-7.27115168170008,-5.80390888650157,
4.30568843598292));
#68880=CARTESIAN_POINT('Ctrl Pts',(-7.17199780172666,-7.15606515268471,
1.00749332558613));
#68881=CARTESIAN_POINT('Ctrl Pts',(-7.07284392175321,-6.76711752176552,
-2.53582959151107));
#68882=CARTESIAN_POINT('Ctrl Pts',(-6.97369004177979,-4.731698759309,-5.46217338810503));
#68883=CARTESIAN_POINT('Ctrl Pts',(-6.87453616180633,-1.54503570631433,
-7.05954502335547));
#68884=CARTESIAN_POINT('Ctrl Pts',(-6.77538228183291,2.01754171191176,-6.93929655737995));
#68885=CARTESIAN_POINT('Ctrl Pts',(-6.67622840185947,5.08924185858894,-5.13068500059742));
#68886=CARTESIAN_POINT('Ctrl Pts',(-6.57707452188604,6.92270581760909,-2.07375394717175));
#68887=CARTESIAN_POINT('Ctrl Pts',(-6.47792064191259,7.07184328988527,1.48773107579087));
#68888=CARTESIAN_POINT('Ctrl Pts',(-6.37876676193917,5.50036843555384,4.68724421635273));
#68889=CARTESIAN_POINT('Ctrl Pts',(-6.27961288196572,2.59062838738908,6.74632906320341));
#68890=CARTESIAN_POINT('Ctrl Pts',(-6.18045900199229,-0.949423582898823,
7.16400070706338));
#68891=CARTESIAN_POINT('Ctrl Pts',(-6.08130512201885,-4.25847638466099,
5.83863769657389));
#68892=CARTESIAN_POINT('Ctrl Pts',(-5.98215124204542,-6.53142209812059,
3.09270700952272));
#68893=CARTESIAN_POINT('Ctrl Pts',(-5.88299736207198,-7.21524247160315,
-0.405693660959992));
#68894=CARTESIAN_POINT('Ctrl Pts',(-5.78384348209854,-6.14356083136612,
-3.80538717897051));
#68895=CARTESIAN_POINT('Ctrl Pts',(-5.68468960212512,-3.57712229926877,
-6.27921231737256));
#68896=CARTESIAN_POINT('Ctrl Pts',(-5.58553572215167,-0.140353293261173,
-7.22527592716291));
#68897=CARTESIAN_POINT('Ctrl Pts',(-5.48638184217824,3.3305643210464,-6.4133963368828));
#68898=CARTESIAN_POINT('Ctrl Pts',(-5.3872279622048,5.99114016299764,-4.04110762265567));
#68899=CARTESIAN_POINT('Ctrl Pts',(-5.28807408223137,7.19404376981442,-0.685598649767781));
#68900=CARTESIAN_POINT('Ctrl Pts',(-5.18892020225793,6.64660310554116,2.83671965974429));
#68901=CARTESIAN_POINT('Ctrl Pts',(-5.08976632228449,4.48201302708057,5.66885089728502));
#68902=CARTESIAN_POINT('Ctrl Pts',(-4.99061244231105,1.22692835671624,7.12172437532194));
#68903=CARTESIAN_POINT('Ctrl Pts',(-4.89145856233762,-2.32667368286776,
6.84184922692832));
#68904=CARTESIAN_POINT('Ctrl Pts',(-4.79230468236418,-5.31418520621231,
4.89732037594473));
#68905=CARTESIAN_POINT('Ctrl Pts',(-4.69315080239075,-7.0087307803873,1.7612507256551));
#68906=CARTESIAN_POINT('Ctrl Pts',(-4.5939969224173,-6.99801959472198,-1.80333940855744));
#68907=CARTESIAN_POINT('Ctrl Pts',(-4.49484304244388,-5.28465773045043,
-4.92916868676245));
#68908=CARTESIAN_POINT('Ctrl Pts',(-4.39568916247043,-2.28551408904019,
-6.85570832367946));
#68909=CARTESIAN_POINT('Ctrl Pts',(-4.29653528249701,1.26970574821316,-7.11422227538074));
#68910=CARTESIAN_POINT('Ctrl Pts',(-4.19738140252356,4.51600027816159,-5.64181289642023));
#68911=CARTESIAN_POINT('Ctrl Pts',(-4.09822752255013,6.6635309601212,-2.79672422917872));
#68912=CARTESIAN_POINT('Ctrl Pts',(-3.9990736425767,7.1897936022312,0.728820435967838));
#68913=CARTESIAN_POINT('Ctrl Pts',(-3.89991976260326,5.96674605876947,4.07703970310913));
#68914=CARTESIAN_POINT('Ctrl Pts',(-3.80076588262982,3.29196147906146,6.43329626948305));
#68915=CARTESIAN_POINT('Ctrl Pts',(-3.70161200265639,-0.183772622207902,
7.22430196585773));
#68916=CARTESIAN_POINT('Ctrl Pts',(-3.60245812268295,-3.61479399072821,
6.25760143147231));
#68917=CARTESIAN_POINT('Ctrl Pts',(-3.50330424270951,-6.16631918779205,
3.768397397414));
#68918=CARTESIAN_POINT('Ctrl Pts',(-3.40415036273608,-7.21755027914701,
0.362324769446019));
#68919=CARTESIAN_POINT('Ctrl Pts',(-3.30499648276264,-6.51271785648537,
-3.13190315820678));
#68920=CARTESIAN_POINT('Ctrl Pts',(-3.20584260278921,-4.22331092273221,
-5.86412449735678));
#68921=CARTESIAN_POINT('Ctrl Pts',(-3.10668872281577,-0.906352820934512,
-7.16957710290872));
#68922=CARTESIAN_POINT('Ctrl Pts',(-3.00753484284234,2.63112513290601,-6.73063829109539));
#68923=CARTESIAN_POINT('Ctrl Pts',(-2.9083809628689,5.52843811830046,-4.65410391404099));
#68924=CARTESIAN_POINT('Ctrl Pts',(-2.80922708289546,7.08065642564394,-1.44520443279018));
#68925=CARTESIAN_POINT('Ctrl Pts',(-2.71007320292203,6.9101181295059,2.11532000105019));
#68926=CARTESIAN_POINT('Ctrl Pts',(-2.61091932294859,5.05831598961895,5.16117725133854));
#68927=CARTESIAN_POINT('Ctrl Pts',(-2.51176544297515,1.97580206966993,6.95129609871836));
#68928=CARTESIAN_POINT('Ctrl Pts',(-2.41261156300172,-1.58743367295767,
7.05013231113639));
#68929=CARTESIAN_POINT('Ctrl Pts',(-2.31345768302828,-4.76443942809818,
5.43363857894068));
#68930=CARTESIAN_POINT('Ctrl Pts',(-2.21430380305484,-6.78223493587843,
2.4951153370374));
#68931=CARTESIAN_POINT('Ctrl Pts',(-2.11514992308141,-7.1498811750356,-1.05048105810653));
#68932=CARTESIAN_POINT('Ctrl Pts',(-2.01599604310797,-5.77792810758181,
-4.34049053151657));
#68933=CARTESIAN_POINT('Ctrl Pts',(-1.91684216313454,-3.00017828861109,
-6.57443849367501));
#68934=CARTESIAN_POINT('Ctrl Pts',(-1.8176882831611,0.50752884612595,-7.20879502697359));
#68935=CARTESIAN_POINT('Ctrl Pts',(-1.71853440318767,3.89175185473677,-6.08921823978432));
#68936=CARTESIAN_POINT('Ctrl Pts',(-1.61938052321423,6.32909355689451,-3.48810636572991));
#68937=CARTESIAN_POINT('Ctrl Pts',(-1.52022664324079,7.22653739312793,-0.0383220079431006));
#68938=CARTESIAN_POINT('Ctrl Pts',(-1.42107276326736,6.36573110876114,3.42078627241163));
#68939=CARTESIAN_POINT('Ctrl Pts',(-1.32191888329392,3.95611287189113,6.04760136049213));
#68940=CARTESIAN_POINT('Ctrl Pts',(-1.22276500332049,0.58395399408771,7.2030069417819));
#68941=CARTESIAN_POINT('Ctrl Pts',(-1.12361112334705,-2.93028360339495,
6.60588747060103));
#68942=CARTESIAN_POINT('Ctrl Pts',(-1.02445724337361,-5.7315695867392,4.40152488836941));
#68943=CARTESIAN_POINT('Ctrl Pts',(-0.925303363400176,-7.13833806205865,
1.12625085231209));
#68944=CARTESIAN_POINT('Ctrl Pts',(-0.826149483426741,-6.80831572378113,
-2.42304524841852));
#68945=CARTESIAN_POINT('Ctrl Pts',(-0.726995603453303,-4.82179854001844,
-5.38280318329076));
#68946=CARTESIAN_POINT('Ctrl Pts',(-0.627841723479869,-1.66211537048783,
-7.03290009638678));
#68947=CARTESIAN_POINT('Ctrl Pts',(-0.528687843506433,1.90196819049315,
-6.97185974277461));
#68948=CARTESIAN_POINT('Ctrl Pts',(-0.429533963532995,5.0032940546147,-5.21453352406773));
#68949=CARTESIAN_POINT('Ctrl Pts',(-0.330380083559562,6.88729523108016,
-2.18848707341619));
#68950=CARTESIAN_POINT('Ctrl Pts',(-0.231226203586123,7.09558548101365,
1.37002844941164));
#68951=CARTESIAN_POINT('Ctrl Pts',(-0.132072323612686,5.57748681893721,
4.59520968565645));
#68952=CARTESIAN_POINT('Ctrl Pts',(-0.0329184436392514,2.70235970207573,
6.70235505708003));
#68953=CARTESIAN_POINT('Ctrl Pts',(0.0662354363341854,-0.830264084850464,
7.17878630549598));
#68954=CARTESIAN_POINT('Ctrl Pts',(0.165389316307623,-4.16088076271409,
5.90858549477325));
#68955=CARTESIAN_POINT('Ctrl Pts',(0.264543196281057,-6.47913582050193,
3.20079838322534));
#68956=CARTESIAN_POINT('Ctrl Pts',(0.363697076254494,-7.22098703256748,
-0.285757845143952));
#68957=CARTESIAN_POINT('Ctrl Pts',(0.462850956227929,-6.20593855254291,
-3.70278786222361));
#68958=CARTESIAN_POINT('Ctrl Pts',(0.562004836201364,-3.68095639130301,
-6.21891239011249));
#68959=CARTESIAN_POINT('Ctrl Pts',(0.661158716174802,-0.260380439171297,
-7.22194664183183));
#68960=CARTESIAN_POINT('Ctrl Pts',(0.760312596148235,3.22354728347921,-6.46784772406888));
#68961=CARTESIAN_POINT('Ctrl Pts',(0.859466476121674,5.92317097619031,-4.14009140688773));
#68962=CARTESIAN_POINT('Ctrl Pts',(0.95862035609511,7.18165965268664,-0.805031616485985));
#68963=CARTESIAN_POINT('Ctrl Pts',(1.05777423606855,6.69281717132386,2.72589610620094));
#68964=CARTESIAN_POINT('Ctrl Pts',(1.15692811604198,4.5755811788688,5.59360064235469));
#68965=CARTESIAN_POINT('Ctrl Pts',(1.25608199601542,1.34508502848351,7.10035615562477));
#68966=CARTESIAN_POINT('Ctrl Pts',(1.35523587598886,-2.2126765582915,6.87956202958854));
#68967=CARTESIAN_POINT('Ctrl Pts',(1.45438975596229,-5.2320836588412,4.98493850086998));
#68968=CARTESIAN_POINT('Ctrl Pts',(1.55354363593573,-6.97850049812194,1.87745627599714));
#68969=CARTESIAN_POINT('Ctrl Pts',(1.65269751590916,-7.02701574568049,-1.68681978306143));
#68970=CARTESIAN_POINT('Ctrl Pts',(1.7518513958826,-5.36582541639512,-4.84068475231937));
#68971=CARTESIAN_POINT('Ctrl Pts',(1.85100527585604,-2.39910483489405,-6.81678863261558));
#68972=CARTESIAN_POINT('Ctrl Pts',(1.95015915582947,1.15132909863318,-7.13433616934397));
#68973=CARTESIAN_POINT('Ctrl Pts',(2.04931303580291,4.42163931364934,-5.71606657156472));
#68974=CARTESIAN_POINT('Ctrl Pts',(2.14846691577634,6.61614414172214,-2.90705142137611));
#68975=CARTESIAN_POINT('Ctrl Pts',(2.24762079574978,7.20091036301022,0.609262845134264));
#68976=CARTESIAN_POINT('Ctrl Pts',(2.34677467572321,6.03366163918308,3.97734063092661));
#68977=CARTESIAN_POINT('Ctrl Pts',(2.44592855569666,3.39839500752044,6.37771296339286));
#68978=CARTESIAN_POINT('Ctrl Pts',(2.54508243567008,-0.0637169176436377,
7.22635810245902));
#68979=CARTESIAN_POINT('Ctrl Pts',(2.64423631564353,-3.51032622073068,6.31679674317765));
#68980=CARTESIAN_POINT('Ctrl Pts',(2.74339019561696,-6.10285684613524,3.87032938987749));
#68981=CARTESIAN_POINT('Ctrl Pts',(2.8425440755904,-7.21053404838757,0.482192915348399));
#68982=CARTESIAN_POINT('Ctrl Pts',(2.94169795556383,-6.56385481816304,-3.02326333564373));
#68983=CARTESIAN_POINT('Ctrl Pts',(3.04085183553727,-4.32015921649977,-5.79314557167872));
#68984=CARTESIAN_POINT('Ctrl Pts',(3.14000571551071,-1.02534880698369,-7.15352857648482));
#68985=CARTESIAN_POINT('Ctrl Pts',(3.23915959548414,2.51893373081034,-6.77342484496287));
#68986=CARTESIAN_POINT('Ctrl Pts',(3.33831347545758,5.45034798950191,-4.7453153808664));
#68987=CARTESIAN_POINT('Ctrl Pts',(3.43746735543101,7.05566726127222,-1.56264863894891));
#68988=CARTESIAN_POINT('Ctrl Pts',(3.53662123540445,6.94430990933893,2.00021777653919));
#68989=CARTESIAN_POINT('Ctrl Pts',(3.63577511537789,5.14336969479104,5.07642191443079));
#68990=CARTESIAN_POINT('Ctrl Pts',(3.73492899535132,2.09102373854355,6.91750901665076));
#68991=CARTESIAN_POINT('Ctrl Pts',(3.83408287532475,-1.47007800765708,7.07553403791758));
#68992=CARTESIAN_POINT('Ctrl Pts',(3.9332367552982,-4.67350294505472,5.51204875648353));
#68993=CARTESIAN_POINT('Ctrl Pts',(4.03239063527163,-6.73984290367638,2.60745640477422));
#68994=CARTESIAN_POINT('Ctrl Pts',(4.13154451524507,-7.16634777246096,-0.93154220368205));
#68995=CARTESIAN_POINT('Ctrl Pts',(4.2306983952185,-5.84924693419187,-4.24389226660731));
#68996=CARTESIAN_POINT('Ctrl Pts',(4.32985227519194,-3.10899714408849,-6.52368362421285));
#68997=CARTESIAN_POINT('Ctrl Pts',(4.42900615516538,0.387686097825344,-7.21623244983844));
#68998=CARTESIAN_POINT('Ctrl Pts',(4.52816003513881,3.79004350530718,-6.15303839283771));
#68999=CARTESIAN_POINT('Ctrl Pts',(4.62731391511224,6.27026573136093,-3.59278151428031));
#69000=CARTESIAN_POINT('Ctrl Pts',(4.72646779508569,7.22490315325883,-0.158384192290982));
#69001=CARTESIAN_POINT('Ctrl Pts',(4.82562167505912,6.42168811431263,3.31454872059966));
#69002=CARTESIAN_POINT('Ctrl Pts',(4.92477555503256,4.0560464428859,5.98103656772639));
#69003=CARTESIAN_POINT('Ctrl Pts',(5.023929435006,0.703549984439801,7.19231036051555));
#69004=CARTESIAN_POINT('Ctrl Pts',(5.12308331497942,-2.8201237558501,6.65366176598889));
#69005=CARTESIAN_POINT('Ctrl Pts',(5.22223719495288,-5.65764769969538,4.49614608664009));
#69006=CARTESIAN_POINT('Ctrl Pts',(5.3213910749263,-7.11864080686008,1.24469769095677));
#69007=CARTESIAN_POINT('Ctrl Pts',(5.42054495489974,-6.84763334052093,-2.30959243204915));
#69008=CARTESIAN_POINT('Ctrl Pts',(5.51969883487318,-4.91056911767337,-5.30194605677284));
#69009=CARTESIAN_POINT('Ctrl Pts',(5.61885271484661,-1.77873238950342,-7.0043153110442));
#69010=CARTESIAN_POINT('Ctrl Pts',(5.71800659482005,1.78586226417951,-7.00249487356092));
#69011=CARTESIAN_POINT('Ctrl Pts',(5.81716047479348,4.91597917714289,-5.29694891391728));
#69012=CARTESIAN_POINT('Ctrl Pts',(5.91631435476692,6.84995578487968,-2.30260353804152));
#69013=CARTESIAN_POINT('Ctrl Pts',(6.01546823474035,7.11742203170536,1.25192340196377));
#69014=CARTESIAN_POINT('Ctrl Pts',(6.11462211471379,5.65296202589422,4.5019536122408));
#69015=CARTESIAN_POINT('Ctrl Pts',(6.21377599468722,2.81354810058851,6.65643758041471));
#69016=CARTESIAN_POINT('Ctrl Pts',(6.31292987466067,-0.711297331913398,
7.19179029486994));
#69017=CARTESIAN_POINT('Ctrl Pts',(6.37903246130962,-2.94446110243687,6.38148070295211));
#69018=CARTESIAN_POINT('Ctrl Pts',(6.4120837546341,-3.89708022703547,5.73404348641072));
#69019=CARTESIAN_POINT('',(6.,6.90110124345015,0.667252526942056));
#69020=CARTESIAN_POINT('Ctrl Pts',(6.,6.90110124345015,0.667252526942055));
#69021=CARTESIAN_POINT('Ctrl Pts',(6.,6.87512084914595,0.845079749951139));
#69022=CARTESIAN_POINT('Ctrl Pts',(6.,6.8422227909989,1.02164116641632));
#69023=CARTESIAN_POINT('Ctrl Pts',(6.,6.80237868150643,1.19653215063161));
#69024=CARTESIAN_POINT('Ctrl Pts',(6.,6.76059281023488,1.37994626744993));
#69025=CARTESIAN_POINT('Ctrl Pts',(6.,6.71116752238872,1.56152391244805));
#69026=CARTESIAN_POINT('Ctrl Pts',(6.,6.65432880950473,1.74083702432569));
#69027=CARTESIAN_POINT('Ctrl Pts',(6.,6.61860356983375,1.85354196736429));
#69028=CARTESIAN_POINT('Ctrl Pts',(6.,6.57994859237711,1.96535194631467));
#69029=CARTESIAN_POINT('Ctrl Pts',(6.,6.53841065439784,2.07615582015086));
#69030=CARTESIAN_POINT('Ctrl Pts',(6.,6.51423804398105,2.14063708728189));
#69031=CARTESIAN_POINT('Ctrl Pts',(6.,6.48908897520853,2.20477755420385));
#69032=CARTESIAN_POINT('Ctrl Pts',(6.,6.46297163102309,2.26855457840167));
#69033=CARTESIAN_POINT('Ctrl Pts',(6.,6.45029733594765,2.29950446434633));
#69034=CARTESIAN_POINT('Ctrl Pts',(6.00000000000001,6.43739500160117,2.33036875102595));
#69035=CARTESIAN_POINT('Ctrl Pts',(6.00000000000001,6.42426550165052,2.36114479888992));
#69036=CARTESIAN_POINT('Ctrl Pts',(6.00000000000001,6.41370848887882,2.38589083884451));
#69037=CARTESIAN_POINT('Ctrl Pts',(6.,6.40300509881027,2.41057855434172));
#69038=CARTESIAN_POINT('Ctrl Pts',(6.,6.3921608998279,2.43519538126747));
#69039=CARTESIAN_POINT('Ctrl Pts',(6.,6.31690021844114,2.60604056504019));
#69040=CARTESIAN_POINT('Ctrl Pts',(6.,6.23479842551277,2.77362133337677));
#69041=CARTESIAN_POINT('Ctrl Pts',(6.,6.14608035170904,2.93752067517517));
#69042=CARTESIAN_POINT('Ctrl Pts',(6.,6.05778543340776,3.10063827199919));
#69043=CARTESIAN_POINT('Ctrl Pts',(6.00000000000001,5.96293679676374,3.26011007278674));
#69044=CARTESIAN_POINT('Ctrl Pts',(6.00000000000001,5.86171344922557,3.4154964720103));
#69045=CARTESIAN_POINT('Ctrl Pts',(6.00000000000001,5.77251333828363,3.55242618621861));
#69046=CARTESIAN_POINT('Ctrl Pts',(6.,5.67836217835066,3.6861832393832));
#69047=CARTESIAN_POINT('Ctrl Pts',(6.,5.57935844247498,3.81644275297445));
#69048=CARTESIAN_POINT('Ctrl Pts',(6.,5.56179714751913,3.83954820166029));
#69049=CARTESIAN_POINT('Ctrl Pts',(6.,5.54408311980832,3.86254353976059));
#69050=CARTESIAN_POINT('Ctrl Pts',(6.,5.52621684224323,3.88542686726127));
#69051=CARTESIAN_POINT('Ctrl Pts',(6.,5.5120906212318,3.90351988862925));
#69052=CARTESIAN_POINT('Ctrl Pts',(6.,5.49787159919033,3.9215397938568));
#69053=CARTESIAN_POINT('Ctrl Pts',(6.,5.48356530754569,3.9394793139752));
#69054=CARTESIAN_POINT('Ctrl Pts',(6.,5.41395857010921,4.02676339133329));
#69055=CARTESIAN_POINT('Ctrl Pts',(6.00000000000001,5.34225042088021,4.112191032286));
#69056=CARTESIAN_POINT('Ctrl Pts',(6.00000000000001,5.26848862833751,4.19567458971719));
#69057=CARTESIAN_POINT('Ctrl Pts',(6.00000000000001,5.14726642343806,4.33287381652286));
#69058=CARTESIAN_POINT('Ctrl Pts',(6.00000000000001,5.02049957218978,4.46482444068325));
#69059=CARTESIAN_POINT('Ctrl Pts',(6.,4.88860267407126,4.59129948324502));
#69060=CARTESIAN_POINT('Ctrl Pts',(6.,4.75596452769754,4.71848530373989));
#69061=CARTESIAN_POINT('Ctrl Pts',(6.00000000000001,4.61813790255797,4.84013424195775));
#69062=CARTESIAN_POINT('Ctrl Pts',(6.00000000000001,4.47551055286989,4.95597518165141));
#69063=CARTESIAN_POINT('Ctrl Pts',(6.,4.33223183470951,5.07234515828002));
#69064=CARTESIAN_POINT('Ctrl Pts',(6.,4.18410782009949,5.18285439570423));
#69065=CARTESIAN_POINT('Ctrl Pts',(6.,4.03150680793832,5.28718112877869));
#69066=CARTESIAN_POINT('Ctrl Pts',(6.,3.91705604881744,5.36542617858453));
#69067=CARTESIAN_POINT('Ctrl Pts',(6.,3.80008641070901,5.44019264427881));
#69068=CARTESIAN_POINT('Ctrl Pts',(6.,3.68074738017099,5.51132537150878));
#69069=CARTESIAN_POINT('Ctrl Pts',(6.,3.64726712747172,5.53128147197407));
#69070=CARTESIAN_POINT('Ctrl Pts',(6.,3.6136003658972,5.55095146610427));
#69071=CARTESIAN_POINT('Ctrl Pts',(6.,3.57975035326996,5.57033167451751));
#69072=CARTESIAN_POINT('Ctrl Pts',(6.,3.56056135851451,5.58131798408544));
#69073=CARTESIAN_POINT('Ctrl Pts',(5.99999999999999,3.54131353286354,5.59221107875469));
#69074=CARTESIAN_POINT('Ctrl Pts',(5.99999999999999,3.52202007761294,5.60300338569058));
#69075=CARTESIAN_POINT('Ctrl Pts',(5.99999999999999,3.36376168596919,5.69152942292001));
#69076=CARTESIAN_POINT('Ctrl Pts',(5.99999999999999,3.20222425639891,5.7733994532117));
#69077=CARTESIAN_POINT('Ctrl Pts',(5.99999999999999,3.03778929826304,5.84837571003259));
#69078=CARTESIAN_POINT('Ctrl Pts',(5.99999999999999,2.87948768288287,5.9205553894904));
#69079=CARTESIAN_POINT('Ctrl Pts',(6.,2.7184999884668,5.98634601537609));
#69080=CARTESIAN_POINT('Ctrl Pts',(6.,2.55514743307005,6.0454940255894));
#69081=CARTESIAN_POINT('Ctrl Pts',(6.,2.38509059043805,6.10706957817509));
#69082=CARTESIAN_POINT('Ctrl Pts',(6.,2.21247016466867,6.16144647749524));
#69083=CARTESIAN_POINT('Ctrl Pts',(6.00000000000001,2.03775930492053,6.20856933932807));
#69084=CARTESIAN_POINT('Ctrl Pts',(6.00000000000001,1.86371390683491,6.25551271341741));
#69085=CARTESIAN_POINT('Ctrl Pts',(6.,1.68759322518328,6.29525721624741));
#69086=CARTESIAN_POINT('Ctrl Pts',(6.,1.50986401183211,6.32769663740758));
#69087=CARTESIAN_POINT('Ctrl Pts',(6.,1.42166905351582,6.34379412269477));
#69088=CARTESIAN_POINT('Ctrl Pts',(6.,1.33307805394327,6.35809195955199));
#69089=CARTESIAN_POINT('Ctrl Pts',(6.,1.24414881613908,6.37057241832403));
#69090=CARTESIAN_POINT('Ctrl Pts',(6.,1.21992034554203,6.37397267717997));
#69091=CARTESIAN_POINT('Ctrl Pts',(6.00000000000001,1.1956667730464,6.37723801904711));
#69092=CARTESIAN_POINT('Ctrl Pts',(6.00000000000001,1.17138927881511,6.38036804447858));
#69093=CARTESIAN_POINT('Ctrl Pts',(6.00000000000001,1.15206171036832,6.38285989063826));
#69094=CARTESIAN_POINT('Ctrl Pts',(6.,1.13272121299246,6.38526565950859));
#69095=CARTESIAN_POINT('Ctrl Pts',(6.,1.1133772217241,6.38758422312348));
#69096=CARTESIAN_POINT('Ctrl Pts',(6.,0.935876273983282,6.40885942084931));
#69097=CARTESIAN_POINT('Ctrl Pts',(6.,0.757869165584463,6.42282400107153));
#69098=CARTESIAN_POINT('Ctrl Pts',(6.,0.579814660575315,6.42946647010954));
#69099=CARTESIAN_POINT('Ctrl Pts',(6.,0.401928577292704,6.43610265603719));
#69100=CARTESIAN_POINT('Ctrl Pts',(6.,0.223994448325209,6.43543058097201));
#69101=CARTESIAN_POINT('Ctrl Pts',(6.,0.0464678143495036,6.42738694530138));
#69102=CARTESIAN_POINT('Ctrl Pts',(6.,-0.128897738801852,6.41944122703288));
#69103=CARTESIAN_POINT('Ctrl Pts',(6.00000000000001,-0.303866334909319,
6.40430224928206));
#69104=CARTESIAN_POINT('Ctrl Pts',(6.00000000000001,-0.477990242294203,
6.38185908387302));
#69105=CARTESIAN_POINT('Ctrl Pts',(6.00000000000001,-0.528330376469423,
6.37537064713291));
#69106=CARTESIAN_POINT('Ctrl Pts',(6.00000000000001,-0.578599818986257,
6.36827139495402));
#69107=CARTESIAN_POINT('Ctrl Pts',(6.00000000000001,-0.628787491712748,
6.36055786920434));
#69108=CARTESIAN_POINT('Ctrl Pts',(6.00000000000001,-0.758270673288377,
6.34065712862454));
#69109=CARTESIAN_POINT('Ctrl Pts',(6.00000000000001,-0.887210108491146,
6.31666852198741));
#69110=CARTESIAN_POINT('Ctrl Pts',(6.00000000000001,-1.0154256226731,6.28864626423226));
#69111=CARTESIAN_POINT('Ctrl Pts',(6.00000000000001,-1.0715199101277,6.27638652646438));
#69112=CARTESIAN_POINT('Ctrl Pts',(6.00000000000001,-1.12747553722447,6.26335455099811));
#69113=CARTESIAN_POINT('Ctrl Pts',(6.00000000000001,-1.18327691273108,6.24955409931957));
#69114=CARTESIAN_POINT('Ctrl Pts',(6.00000000000001,-1.21645335177475,6.2413491072431));
#69115=CARTESIAN_POINT('Ctrl Pts',(6.00000000000001,-1.24957525908693,6.23287246231486));
#69116=CARTESIAN_POINT('Ctrl Pts',(6.00000000000001,-1.28263929909211,6.22412487911342));
#69117=CARTESIAN_POINT('Ctrl Pts',(6.00000000000001,-1.30830712007077,6.21733407558259));
#69118=CARTESIAN_POINT('Ctrl Pts',(6.00000000000001,-1.33394273334406,6.21037917995715));
#69119=CARTESIAN_POINT('Ctrl Pts',(6.00000000000001,-1.35952145145008,6.20326713279195));
#69120=CARTESIAN_POINT('Ctrl Pts',(6.00000000000001,-1.52810164644578,6.15639417016115));
#69121=CARTESIAN_POINT('Ctrl Pts',(6.00000000000001,-1.69441995109146,6.10264583742032));
#69122=CARTESIAN_POINT('Ctrl Pts',(6.00000000000001,-1.85808244723373,6.04224631836195));
#69123=CARTESIAN_POINT('Ctrl Pts',(6.00000000000001,-2.02266743867339,5.98150635311946));
#69124=CARTESIAN_POINT('Ctrl Pts',(6.,-2.18456727282551,5.9140397073175));
#69125=CARTESIAN_POINT('Ctrl Pts',(6.,-2.34336323590439,5.84002531164617));
#69126=CARTESIAN_POINT('Ctrl Pts',(6.,-2.50120497939138,5.76645567530665));
#69127=CARTESIAN_POINT('Ctrl Pts',(6.00000000000001,-2.65598065856633,5.68641637359828));
#69128=CARTESIAN_POINT('Ctrl Pts',(6.00000000000001,-2.80725163501019,5.60003997452776));
#69129=CARTESIAN_POINT('Ctrl Pts',(6.,-2.95558268225547,5.51534228808054));
#69130=CARTESIAN_POINT('Ctrl Pts',(6.,-3.10054441261676,5.42455102216784));
#69131=CARTESIAN_POINT('Ctrl Pts',(6.,-3.24168883972874,5.32775543156938));
#69132=CARTESIAN_POINT('Ctrl Pts',(6.,-3.32787899344155,5.26864699205739));
#69133=CARTESIAN_POINT('Ctrl Pts',(6.,-3.41264498807892,5.20729889266937));
#69134=CARTESIAN_POINT('Ctrl Pts',(6.,-3.49587713861109,5.14372565308808));
#69135=CARTESIAN_POINT('Ctrl Pts',(5.35582833639373,-6.93262081645922,0.000142250729870931));
#69136=CARTESIAN_POINT('Ctrl Pts',(5.3774005425624,-6.93206096538092,-0.75173178625728));
#69137=CARTESIAN_POINT('Ctrl Pts',(5.39897274873107,-6.81015446000589,-1.50378293313638));
#69138=CARTESIAN_POINT('Ctrl Pts',(5.42054495489974,-6.56995721443619,-2.21593634900211));
#69139=CARTESIAN_POINT('Ctrl Pts',(5.45359624822422,-6.20194526623841,-3.30704364029038));
#69140=CARTESIAN_POINT('Ctrl Pts',(5.4866475415487,-5.5562571919559,-4.3044948485316));
#69141=CARTESIAN_POINT('Ctrl Pts',(5.51969883487318,-4.71144036678631,-5.08694866169745));
#69142=CARTESIAN_POINT('Ctrl Pts',(5.55275012819765,-3.86662354161672,-5.8694024748633));
#69143=CARTESIAN_POINT('Ctrl Pts',(5.58580142152213,-2.82267796556008,-6.43685889295375));
#69144=CARTESIAN_POINT('Ctrl Pts',(5.61885271484661,-1.70660606858459,-6.72028369575176));
#69145=CARTESIAN_POINT('Ctrl Pts',(5.65190400817109,-0.590534171609124,
-7.00370849854977));
#69146=CARTESIAN_POINT('Ctrl Pts',(5.68495530149557,0.597664046285246,-7.00310168605534));
#69147=CARTESIAN_POINT('Ctrl Pts',(5.71800659482005,1.71344930739295,-6.71854061986752));
#69148=CARTESIAN_POINT('Ctrl Pts',(5.75105788814453,2.82923456850066,-6.4339795536797));
#69149=CARTESIAN_POINT('Ctrl Pts',(5.784109181469,3.87260687282175,-5.8654642337985));
#69150=CARTESIAN_POINT('Ctrl Pts',(5.81716047479348,4.7166224596051,-5.08214901121195));
#69151=CARTESIAN_POINT('Ctrl Pts',(5.85021176811796,5.56063804638848,-4.29883378862537));
#69152=CARTESIAN_POINT('Ctrl Pts',(5.88326306144244,6.20529691563407,-3.30071866333345));
#69153=CARTESIAN_POINT('Ctrl Pts',(5.91631435476692,6.57220405806116,-2.20923994401993));
#69154=CARTESIAN_POINT('Ctrl Pts',(5.94420956984461,6.88187283716353,-1.28803443084786));
#69155=CARTESIAN_POINT('Ctrl Pts',(5.9721047849223,6.99369014720255,-0.300323033281158));
#69156=CARTESIAN_POINT('Ctrl Pts',(6.,6.90110124345015,0.667252526942056));
#69157=CARTESIAN_POINT('',(-13.617,-3.61129923637168,-5.06367012420432));
#69158=CARTESIAN_POINT('Ctrl Pts',(-13.617,-3.61129923637173,-5.06367012420428));
#69159=CARTESIAN_POINT('Ctrl Pts',(-13.617,-3.74821940074788,-4.9772215892196));
#69160=CARTESIAN_POINT('Ctrl Pts',(-13.617,-3.88155875406187,-4.8855130775753));
#69161=CARTESIAN_POINT('Ctrl Pts',(-13.617,-4.01098648203258,-4.78872019092777));
#69162=CARTESIAN_POINT('Ctrl Pts',(-13.617,-4.14999389329108,-4.68476311146675));
#69163=CARTESIAN_POINT('Ctrl Pts',(-13.617,-4.28449018187927,-4.57494160616014));
#69164=CARTESIAN_POINT('Ctrl Pts',(-13.617,-4.41423794256447,-4.4596577141252));
#69165=CARTESIAN_POINT('Ctrl Pts',(-13.617,-4.49638395135372,-4.38666908173302));
#69166=CARTESIAN_POINT('Ctrl Pts',(-13.617,-4.57662608008218,-4.31148992041847));
#69167=CARTESIAN_POINT('Ctrl Pts',(-13.617,-4.65489813141777,-4.23421332941955));
#69168=CARTESIAN_POINT('Ctrl Pts',(-13.617,-4.70991755617827,-4.17989363916403));
#69169=CARTESIAN_POINT('Ctrl Pts',(-13.617,-4.76396345962384,-4.12453745736493));
#69170=CARTESIAN_POINT('Ctrl Pts',(-13.617,-4.81701125140619,-4.06817532341179));
#69171=CARTESIAN_POINT('Ctrl Pts',(-13.617,-4.84235650451882,-4.04124653895131));
#69172=CARTESIAN_POINT('Ctrl Pts',(-13.617,-4.86747747607571,-4.01408402234033));
#69173=CARTESIAN_POINT('Ctrl Pts',(-13.617,-4.89235012235299,-3.9867147784119));
#69174=CARTESIAN_POINT('Ctrl Pts',(-13.617,-5.01128793420523,-3.8558385560507));
#69175=CARTESIAN_POINT('Ctrl Pts',(-13.617,-5.12463251721525,-3.72015406049308));
#69176=CARTESIAN_POINT('Ctrl Pts',(-13.617,-5.23214095883406,-3.58007840859063));
#69177=CARTESIAN_POINT('Ctrl Pts',(-13.617,-5.34000106729645,-3.43954456046075));
#69178=CARTESIAN_POINT('Ctrl Pts',(-13.617,-5.4419873053284,-3.29459024569057));
#69179=CARTESIAN_POINT('Ctrl Pts',(-13.617,-5.53782072571578,-3.14559625945889));
#69180=CARTESIAN_POINT('Ctrl Pts',(-13.617,-5.61942688539801,-3.01872165785366));
#69181=CARTESIAN_POINT('Ctrl Pts',(-13.617,-5.69657110816774,-2.88891693505272));
#69182=CARTESIAN_POINT('Ctrl Pts',(-13.617,-5.76905775679567,-2.75639865042115));
#69183=CARTESIAN_POINT('Ctrl Pts',(-13.617,-5.78080653204021,-2.73491983230224));
#69184=CARTESIAN_POINT('Ctrl Pts',(-13.617,-5.79243289965685,-2.71336969612923));
#69185=CARTESIAN_POINT('Ctrl Pts',(-13.617,-5.80393596649487,-2.69174912918771));
#69186=CARTESIAN_POINT('Ctrl Pts',(-13.617,-5.81531874733626,-2.67035464555759));
#69187=CARTESIAN_POINT('Ctrl Pts',(-13.617,-5.82657684846509,-2.64889857665108));
#69188=CARTESIAN_POINT('Ctrl Pts',(-13.617,-5.83770783831778,-2.62738549567325));
#69189=CARTESIAN_POINT('Ctrl Pts',(-13.617,-5.88472903406521,-2.53650671443489));
#69190=CARTESIAN_POINT('Ctrl Pts',(-13.617,-5.92949293450927,-2.44459071409149));
#69191=CARTESIAN_POINT('Ctrl Pts',(-13.617,-5.97195499129405,-2.3517149301572));
#69192=CARTESIAN_POINT('Ctrl Pts',(-13.617,-6.04516132784387,-2.19159324951219));
#69193=CARTESIAN_POINT('Ctrl Pts',(-13.617,-6.11152842057772,-2.02862056578686));
#69194=CARTESIAN_POINT('Ctrl Pts',(-13.617,-6.17107314357316,-1.86327271702071));
#69195=CARTESIAN_POINT('Ctrl Pts',(-13.617,-6.23139190661368,-1.69577546105483));
#69196=CARTESIAN_POINT('Ctrl Pts',(-13.617,-6.2847100279,-1.52584027291554));
#69197=CARTESIAN_POINT('Ctrl Pts',(-13.617,-6.33100000828456,-1.35393263393096));
#69198=CARTESIAN_POINT('Ctrl Pts',(-13.617,-6.37823410871505,-1.17851880534197));
#69199=CARTESIAN_POINT('Ctrl Pts',(-13.617,-6.41815081170317,-1.00105057130705));
#69200=CARTESIAN_POINT('Ctrl Pts',(-13.617,-6.45066957280197,-0.822002128173549));
#69201=CARTESIAN_POINT('Ctrl Pts',(-13.617,-6.47505864362608,-0.687715795823425));
#69202=CARTESIAN_POINT('Ctrl Pts',(-13.617,-6.4952853305009,-0.552540099903254));
#69203=CARTESIAN_POINT('Ctrl Pts',(-13.617,-6.5112955086982,-0.416671418134875));
#69204=CARTESIAN_POINT('Ctrl Pts',(-13.617,-6.51564948719698,-0.379721840698151));
#69205=CARTESIAN_POINT('Ctrl Pts',(-13.617,-6.51969152334182,-0.342721004431168));
#69206=CARTESIAN_POINT('Ctrl Pts',(-13.617,-6.52342029919769,-0.305672850016471));
#69207=CARTESIAN_POINT('Ctrl Pts',(-13.617,-6.52548275285274,-0.285180842870193));
#69208=CARTESIAN_POINT('Ctrl Pts',(-13.617,-6.52744895761689,-0.264678160216595));
#69209=CARTESIAN_POINT('Ctrl Pts',(-13.617,-6.52931811777843,-0.244173644297405));
#69210=CARTESIAN_POINT('Ctrl Pts',(-13.617,-6.54586442705464,-0.062662145744726));
#69211=CARTESIAN_POINT('Ctrl Pts',(-13.617,-6.55482935469237,0.119181209939556));
#69212=CARTESIAN_POINT('Ctrl Pts',(-13.617,-6.55620696958347,0.300870273217915));
#69213=CARTESIAN_POINT('Ctrl Pts',(-13.617,-6.55749612429352,0.470892616328059));
#69214=CARTESIAN_POINT('Ctrl Pts',(-13.617,-6.55214075841214,0.640780576326433));
#69215=CARTESIAN_POINT('Ctrl Pts',(-13.617,-6.54009687944681,0.810149061967126));
#69216=CARTESIAN_POINT('Ctrl Pts',(-13.617,-6.52728479397343,0.990320543328873));
#69217=CARTESIAN_POINT('Ctrl Pts',(-13.617,-6.5069044992998,1.16990477407658));
#69218=CARTESIAN_POINT('Ctrl Pts',(-13.617,-6.47915416231961,1.34847769329285));
#69219=CARTESIAN_POINT('Ctrl Pts',(-13.617,-6.45125503441877,1.52800807940656));
#69220=CARTESIAN_POINT('Ctrl Pts',(-13.617,-6.41590648915762,1.7065169794788));
#69221=CARTESIAN_POINT('Ctrl Pts',(-13.617,-6.37325744722561,1.88356902905038));
#69222=CARTESIAN_POINT('Ctrl Pts',(-13.617,-6.3513454550729,1.97453386542391));
#69223=CARTESIAN_POINT('Ctrl Pts',(-13.617,-6.32750555767679,2.06511400851921));
#69224=CARTESIAN_POINT('Ctrl Pts',(-13.617,-6.30175278232589,2.15524902944258));
#69225=CARTESIAN_POINT('Ctrl Pts',(-13.617,-6.29423752239852,2.1815525288351));
#69226=CARTESIAN_POINT('Ctrl Pts',(-13.617,-6.28655933789324,2.20781811305338));
#69227=CARTESIAN_POINT('Ctrl Pts',(-13.617,-6.27871854750472,2.23404425858231));
#69228=CARTESIAN_POINT('Ctrl Pts',(-13.617,-6.27182667314066,2.25709643713613));
#69229=CARTESIAN_POINT('Ctrl Pts',(-13.617,-6.26481116263825,2.2801113732589));
#69230=CARTESIAN_POINT('Ctrl Pts',(-13.617,-6.25767498527291,2.30308018036077));
#69231=CARTESIAN_POINT('Ctrl Pts',(-13.617,-6.20307361309252,2.47882250302214));
#69232=CARTESIAN_POINT('Ctrl Pts',(-13.617,-6.1413695380144,2.6520078842564));
#69233=CARTESIAN_POINT('Ctrl Pts',(-13.617,-6.07280403431614,2.82220755207323));
#69234=CARTESIAN_POINT('Ctrl Pts',(-13.617,-6.00377201206077,2.99356525562474));
#69235=CARTESIAN_POINT('Ctrl Pts',(-13.617,-5.92778472312197,3.16189718654644));
#69236=CARTESIAN_POINT('Ctrl Pts',(-13.617,-5.84503562544626,3.32676190057267));
#69237=CARTESIAN_POINT('Ctrl Pts',(-13.617,-5.76244833580976,3.49130423723336));
#69238=CARTESIAN_POINT('Ctrl Pts',(-13.617,-5.67312543976135,3.65239361081794));
#69239=CARTESIAN_POINT('Ctrl Pts',(-13.617,-5.57720973772646,3.80957671010982));
#69240=CARTESIAN_POINT('Ctrl Pts',(-13.617,-5.55089861053992,3.85269441064586));
#69241=CARTESIAN_POINT('Ctrl Pts',(-13.617,-5.52409110541491,3.89551805044802));
#69242=CARTESIAN_POINT('Ctrl Pts',(-13.617,-5.49678954957014,3.93803797214658));
#69243=CARTESIAN_POINT('Ctrl Pts',(-13.617,-5.41998906945479,4.05764838627403));
#69244=CARTESIAN_POINT('Ctrl Pts',(-13.617,-5.33928015461665,4.17485620063647));
#69245=CARTESIAN_POINT('Ctrl Pts',(-13.617,-5.25481751197263,4.2895246234203));
#69246=CARTESIAN_POINT('Ctrl Pts',(-13.617,-5.21786510581587,4.33969205838822));
#69247=CARTESIAN_POINT('Ctrl Pts',(-13.617,-5.1801940180667,4.38937329875199));
#69248=CARTESIAN_POINT('Ctrl Pts',(-13.617,-5.14181633873687,4.43855619232835));
#69249=CARTESIAN_POINT('Ctrl Pts',(-13.617,-5.12064999833221,4.46568190408848));
#69250=CARTESIAN_POINT('Ctrl Pts',(-13.617,-5.09926871628423,4.49265601958829));
#69251=CARTESIAN_POINT('Ctrl Pts',(-13.617,-5.07767445742497,4.51947643921585));
#69252=CARTESIAN_POINT('Ctrl Pts',(-13.617,-5.0623536077347,4.53850518293992));
#69253=CARTESIAN_POINT('Ctrl Pts',(-13.617,-5.04692457910768,4.55745765964485));
#69254=CARTESIAN_POINT('Ctrl Pts',(-13.617,-5.03139997187395,4.57631887404553));
#69255=CARTESIAN_POINT('Ctrl Pts',(-13.617,-4.91417163799297,4.71874236379161));
#69256=CARTESIAN_POINT('Ctrl Pts',(-13.617,-4.79135007651547,4.85614873648681));
#69257=CARTESIAN_POINT('Ctrl Pts',(-13.617,-4.66335466830376,4.98829842572615));
#69258=CARTESIAN_POINT('Ctrl Pts',(-13.617,-4.5330631770047,5.12281872083878));
#69259=CARTESIAN_POINT('Ctrl Pts',(-13.617,-4.39741019028498,5.25189260637322));
#69260=CARTESIAN_POINT('Ctrl Pts',(-13.617,-4.25678987213029,5.37524320479101));
#69261=CARTESIAN_POINT('Ctrl Pts',(-13.617,-4.11589880764864,5.49883129891275));
#69262=CARTESIAN_POINT('Ctrl Pts',(-13.617,-3.97002076950435,5.61667457298439));
#69263=CARTESIAN_POINT('Ctrl Pts',(-13.617,-3.81951090759404,5.72846233525811));
#69264=CARTESIAN_POINT('Ctrl Pts',(-13.617,-3.67054101929963,5.83910631730177));
#69265=CARTESIAN_POINT('Ctrl Pts',(-13.617,-3.51703305935551,5.94381851790106));
#69266=CARTESIAN_POINT('Ctrl Pts',(-13.617,-3.359298849805,6.04225900678258));
#69267=CARTESIAN_POINT('Ctrl Pts',(-13.617,-3.2483339549443,6.1115111907565));
#69268=CARTESIAN_POINT('Ctrl Pts',(-13.617,-3.13527679518198,6.17765870225568));
#69269=CARTESIAN_POINT('Ctrl Pts',(-13.617,-3.02022829989065,6.2405696868587));
#69270=CARTESIAN_POINT('Ctrl Pts',(-13.617,-3.61129923637168,-5.06367012420432));
#69271=CARTESIAN_POINT('Ctrl Pts',(-13.5891047849223,-2.90091050768866,
-5.56924680684122));
#69272=CARTESIAN_POINT('Ctrl Pts',(-13.5281582765201,-1.11449490138686,
-6.34652636371273));
#69273=CARTESIAN_POINT('Ctrl Pts',(-13.4341604747935,1.91301075045669,-6.193982915654));
#69274=CARTESIAN_POINT('Ctrl Pts',(-13.33500659482,4.64114599103167,-4.52598857637084));
#69275=CARTESIAN_POINT('Ctrl Pts',(-13.2358527148466,6.24006591576224,-1.75683043852266));
#69276=CARTESIAN_POINT('Ctrl Pts',(-13.1366988348732,6.3207503286919,1.43978832745216));
#69277=CARTESIAN_POINT('Ctrl Pts',(-13.0375449548997,4.86356603929123,4.28609183779942));
#69278=CARTESIAN_POINT('Ctrl Pts',(-12.9383910749263,2.2230539416448,6.08957345749443));
#69279=CARTESIAN_POINT('Ctrl Pts',(-12.8392371949529,-0.958337716508845,
6.41143141299502));
#69280=CARTESIAN_POINT('Ctrl Pts',(-12.7400833149794,-3.90656124824087,
5.17335943056773));
#69281=CARTESIAN_POINT('Ctrl Pts',(-12.6457560560753,-5.80705422041825,
2.79812271529996));
#69282=CARTESIAN_POINT('Ctrl Pts',(-12.5844800904956,-6.21868878492818,
0.882080331722138));
#69283=CARTESIAN_POINT('Ctrl Pts',(-12.5562554182404,-6.21952031151782,
-0.000132913339471047));
#69284=CARTESIAN_POINT('Origin',(-13.617,-1.12618006296016E-15,0.));
#69285=CARTESIAN_POINT('',(-13.617,-6.933,-8.4904762584886E-16));
#69286=CARTESIAN_POINT('Origin',(-13.617,0.,0.));
#69287=CARTESIAN_POINT('Origin',(-13.617,0.,0.));
#69288=CARTESIAN_POINT('',(-13.617,3.61104546693872,-5.06353840690493));
#69289=CARTESIAN_POINT('Ctrl Pts',(-13.617,3.02048254223756,6.24076191290031));
#69290=CARTESIAN_POINT('Ctrl Pts',(-13.617,3.17824519336757,6.15468957050444));
#69291=CARTESIAN_POINT('Ctrl Pts',(-13.617,3.33242025106992,6.06256863353936));
#69292=CARTESIAN_POINT('Ctrl Pts',(-13.617,3.48261838037657,5.96451288457896));
#69293=CARTESIAN_POINT('Ctrl Pts',(-13.617,3.64013626193522,5.86167848895641));
#69294=CARTESIAN_POINT('Ctrl Pts',(-13.617,3.79328089376711,5.75231661468439));
#69295=CARTESIAN_POINT('Ctrl Pts',(-13.617,3.94172923226954,5.63678774775573));
#69296=CARTESIAN_POINT('Ctrl Pts',(-13.617,4.03503451979194,5.56417356928354));
#69297=CARTESIAN_POINT('Ctrl Pts',(-13.617,4.12648382947108,5.48912224730297));
#69298=CARTESIAN_POINT('Ctrl Pts',(-13.617,4.2159891579907,5.41171621830808));
#69299=CARTESIAN_POINT('Ctrl Pts',(-13.617,4.26807594012178,5.3666705094707));
#69300=CARTESIAN_POINT('Ctrl Pts',(-13.617,4.31950426551617,5.32082727289711));
#69301=CARTESIAN_POINT('Ctrl Pts',(-13.617,4.37025573807922,5.27420203999897));
#69302=CARTESIAN_POINT('Ctrl Pts',(-13.617,4.39488454444256,5.25157562593252));
#69303=CARTESIAN_POINT('Ctrl Pts',(-13.617,4.41935394043864,5.22876504499028));
#69304=CARTESIAN_POINT('Ctrl Pts',(-13.617,4.44366175369453,5.20577203247252));
#69305=CARTESIAN_POINT('Ctrl Pts',(-13.617,4.46320689558227,5.18728408016865));
#69306=CARTESIAN_POINT('Ctrl Pts',(-13.617,4.48264654393124,5.16867908441253));
#69307=CARTESIAN_POINT('Ctrl Pts',(-13.617,4.50197084753761,5.14996662735338));
#69308=CARTESIAN_POINT('Ctrl Pts',(-13.617,4.6360849691378,5.02009883016965));
#69309=CARTESIAN_POINT('Ctrl Pts',(-13.617,4.76476363751091,4.8849477516844));
#69310=CARTESIAN_POINT('Ctrl Pts',(-13.617,4.88769376982304,4.74486895472631));
#69311=CARTESIAN_POINT('Ctrl Pts',(-13.617,5.01003756789948,4.60545828520619));
#69312=CARTESIAN_POINT('Ctrl Pts',(-13.617,5.12668795564162,4.46116620848808));
#69313=CARTESIAN_POINT('Ctrl Pts',(-13.617,5.23729475898094,4.31231315172846));
#69314=CARTESIAN_POINT('Ctrl Pts',(-13.617,5.3347637657555,4.18114075401248));
#69315=CARTESIAN_POINT('Ctrl Pts',(-13.617,5.42753922720179,4.04642585709307));
#69316=CARTESIAN_POINT('Ctrl Pts',(-13.617,5.51535062192892,3.90837354772389));
#69317=CARTESIAN_POINT('Ctrl Pts',(-13.617,5.53092661714939,3.88388581332916));
#69318=CARTESIAN_POINT('Ctrl Pts',(-13.617,5.5463463451654,3.85929304469139));
#69319=CARTESIAN_POINT('Ctrl Pts',(-13.617,5.56160819159072,3.83459635400809));
#69320=CARTESIAN_POINT('Ctrl Pts',(-13.617,5.57367518302917,3.81506957155148));
#69321=CARTESIAN_POINT('Ctrl Pts',(-13.617,5.58564139940011,3.79548112560944));
#69322=CARTESIAN_POINT('Ctrl Pts',(-13.617,5.59750194280488,3.77583872625322));
#69323=CARTESIAN_POINT('Ctrl Pts',(-13.617,5.65520898570643,3.68026934602712));
#69324=CARTESIAN_POINT('Ctrl Pts',(-13.617,5.71044575082297,3.58337330982993));
#69325=CARTESIAN_POINT('Ctrl Pts',(-13.617,5.76314661286957,3.48522583142202));
#69326=CARTESIAN_POINT('Ctrl Pts',(-13.617,5.8497566907193,3.32392750696295));
#69327=CARTESIAN_POINT('Ctrl Pts',(-13.617,5.92952029322569,3.15925032066695));
#69328=CARTESIAN_POINT('Ctrl Pts',(-13.617,6.0023684100752,2.99166187481058));
#69329=CARTESIAN_POINT('Ctrl Pts',(-13.617,6.07562592405362,2.82313160325521));
#69330=CARTESIAN_POINT('Ctrl Pts',(-13.617,6.14189018518748,2.65165654249902));
#69331=CARTESIAN_POINT('Ctrl Pts',(-13.617,6.20104147301423,2.47769443325878));
#69332=CARTESIAN_POINT('Ctrl Pts',(-13.617,6.2604629017156,2.30293784805581));
#69333=CARTESIAN_POINT('Ctrl Pts',(-13.617,6.31270642666534,2.12567071291085));
#69334=CARTESIAN_POINT('Ctrl Pts',(-13.617,6.35759807452877,1.94635009739155));
#69335=CARTESIAN_POINT('Ctrl Pts',(-13.617,6.39126681042635,1.81185963575207));
#69336=CARTESIAN_POINT('Ctrl Pts',(-13.617,6.42079905049903,1.67621387994155));
#69337=CARTESIAN_POINT('Ctrl Pts',(-13.617,6.44610115240018,1.53960686779479));
#69338=CARTESIAN_POINT('Ctrl Pts',(-13.617,6.45319959001507,1.50128213266926));
#69339=CARTESIAN_POINT('Ctrl Pts',(-13.617,6.45996497978633,1.46288175683764));
#69340=CARTESIAN_POINT('Ctrl Pts',(-13.617,6.466395001408,1.42441007246538));
#69341=CARTESIAN_POINT('Ctrl Pts',(-13.617,6.47004007180214,1.40260112593786));
#69342=CARTESIAN_POINT('Ctrl Pts',(-13.617,6.47357730478795,1.38076934970857));
#69343=CARTESIAN_POINT('Ctrl Pts',(-13.617,6.47700417893135,1.35892975260253));
#69344=CARTESIAN_POINT('Ctrl Pts',(-13.617,6.50511378819952,1.1797861612311));
#69345=CARTESIAN_POINT('Ctrl Pts',(-13.617,6.52584313224597,0.999876921866305));
#69346=CARTESIAN_POINT('Ctrl Pts',(-13.617,6.53910160122101,0.81964234584923));
#69347=CARTESIAN_POINT('Ctrl Pts',(-13.617,6.55186553820663,0.646130398486221));
#69348=CARTESIAN_POINT('Ctrl Pts',(-13.617,6.5577053299578,0.472316286598931));
#69349=CARTESIAN_POINT('Ctrl Pts',(-13.617,6.55649463142021,0.298589257555608));
#69350=CARTESIAN_POINT('Ctrl Pts',(-13.617,6.55523424373395,0.117732172676484));
#69351=CARTESIAN_POINT('Ctrl Pts',(-13.617,6.54633292198605,-0.0630312575838317));
#69352=CARTESIAN_POINT('Ctrl Pts',(-13.617,6.52990290843545,-0.243238067897483));
#69353=CARTESIAN_POINT('Ctrl Pts',(-13.617,6.51353547205042,-0.422758522635574));
#69354=CARTESIAN_POINT('Ctrl Pts',(-13.617,6.48969633624267,-0.601727290924061));
#69355=CARTESIAN_POINT('Ctrl Pts',(-13.617,6.45844785533837,-0.779669770145348));
#69356=CARTESIAN_POINT('Ctrl Pts',(-13.617,6.44294135723537,-0.867970533466823));
#69357=CARTESIAN_POINT('Ctrl Pts',(-13.617,6.42560960552124,-0.956018249370113));
#69358=CARTESIAN_POINT('Ctrl Pts',(-13.617,6.40645603012195,-1.0437525546006));
#69359=CARTESIAN_POINT('Ctrl Pts',(-13.617,6.40123761064567,-1.06765589366958));
#69360=CARTESIAN_POINT('Ctrl Pts',(-13.617,6.39588394211369,-1.09153595774107));
#69361=CARTESIAN_POINT('Ctrl Pts',(-13.617,6.3903950594231,-1.11539150131513));
#69362=CARTESIAN_POINT('Ctrl Pts',(-13.617,6.38602531807229,-1.13438308140121));
#69363=CARTESIAN_POINT('Ctrl Pts',(-13.617,6.38157035926579,-1.15335691703556));
#69364=CARTESIAN_POINT('Ctrl Pts',(-13.617,6.37703239899045,-1.17230376852458));
#69365=CARTESIAN_POINT('Ctrl Pts',(-13.617,6.33539254634327,-1.34615811194329));
#69366=CARTESIAN_POINT('Ctrl Pts',(-13.617,6.2867206860848,-1.51795037154905));
#69367=CARTESIAN_POINT('Ctrl Pts',(-13.617,6.23116523195699,-1.68724630323634));
#69368=CARTESIAN_POINT('Ctrl Pts',(-13.617,6.17566231906677,-1.85638212431142));
#69369=CARTESIAN_POINT('Ctrl Pts',(-13.617,6.1132885745343,-2.02302703146196));
#69370=CARTESIAN_POINT('Ctrl Pts',(-13.617,6.0441427066901,-2.18673182669575));
#69371=CARTESIAN_POINT('Ctrl Pts',(-13.617,5.97583855230202,-2.3484438415469));
#69372=CARTESIAN_POINT('Ctrl Pts',(-13.617,5.90092583665929,-2.50728749672662));
#69373=CARTESIAN_POINT('Ctrl Pts',(-13.617,5.81945588920982,-2.66280439039303));
#69374=CARTESIAN_POINT('Ctrl Pts',(-13.617,5.79590290227599,-2.70776437231505));
#69375=CARTESIAN_POINT('Ctrl Pts',(-13.617,5.77180160189991,-2.75244611117256));
#69376=CARTESIAN_POINT('Ctrl Pts',(-13.617,5.74715258895802,-2.79683801784677));
#69377=CARTESIAN_POINT('Ctrl Pts',(-13.617,5.6835575761326,-2.91137014458735));
#69378=CARTESIAN_POINT('Ctrl Pts',(-13.617,5.61631738202126,-3.02397382199317));
#69379=CARTESIAN_POINT('Ctrl Pts',(-13.617,5.54554537288572,-3.13449888198446));
#69380=CARTESIAN_POINT('Ctrl Pts',(-13.617,5.51458261888893,-3.18285359573065));
#69381=CARTESIAN_POINT('Ctrl Pts',(-13.617,5.48294372620547,-3.23081029824356));
#69382=CARTESIAN_POINT('Ctrl Pts',(-13.617,5.45063763270645,-3.27835567218871));
#69383=CARTESIAN_POINT('Ctrl Pts',(-13.617,5.4314302006912,-3.30662354486477));
#69384=CARTESIAN_POINT('Ctrl Pts',(-13.617,5.41198691778349,-3.33474601054841));
#69385=CARTESIAN_POINT('Ctrl Pts',(-13.617,5.39230961159509,-3.36272018885805));
#69386=CARTESIAN_POINT('Ctrl Pts',(-13.617,5.37703399546923,-3.38443671881408));
#69387=CARTESIAN_POINT('Ctrl Pts',(-13.617,5.36161565934957,-3.40606610228615));
#69388=CARTESIAN_POINT('Ctrl Pts',(-13.617,5.34606967910636,-3.42758759414123));
#69389=CARTESIAN_POINT('Ctrl Pts',(-13.617,5.24361164791509,-3.56942809884234));
#69390=CARTESIAN_POINT('Ctrl Pts',(-13.617,5.13549032829701,-3.70676149773043));
#69391=CARTESIAN_POINT('Ctrl Pts',(-13.617,5.0220526626288,-3.83929613750716));
#69392=CARTESIAN_POINT('Ctrl Pts',(-13.617,4.90797564391624,-3.9725777639653));
#69393=CARTESIAN_POINT('Ctrl Pts',(-13.617,4.78852166418632,-4.10100691347751));
#69394=CARTESIAN_POINT('Ctrl Pts',(-13.617,4.66400382821274,-4.22425297526121));
#69395=CARTESIAN_POINT('Ctrl Pts',(-13.617,4.54023426066734,-4.34675841112407));
#69396=CARTESIAN_POINT('Ctrl Pts',(-13.617,4.41146095294851,-4.46414331471841));
#69397=CARTESIAN_POINT('Ctrl Pts',(-13.617,4.27796044161972,-4.57604230105919));
#69398=CARTESIAN_POINT('Ctrl Pts',(-13.617,4.14705452965938,-4.6857665164092));
#69399=CARTESIAN_POINT('Ctrl Pts',(-13.617,4.01160282440768,-4.79021629205608));
#69400=CARTESIAN_POINT('Ctrl Pts',(-13.617,3.87184448414395,-4.88900244664526));
#69401=CARTESIAN_POINT('Ctrl Pts',(-13.617,3.78650057188512,-4.94932655248207));
#69402=CARTESIAN_POINT('Ctrl Pts',(-13.617,3.69955034012038,-5.00753781673398));
#69403=CARTESIAN_POINT('Ctrl Pts',(-13.617,3.61104546693877,-5.0635384069049));
#69404=CARTESIAN_POINT('Origin',(-13.617,0.,0.));
#69405=CARTESIAN_POINT('Origin',(-15.9277445817596,0.,0.));
#69406=CARTESIAN_POINT('Ctrl Pts',(-13.617,3.61104546693871,-5.06353840690493));
#69407=CARTESIAN_POINT('Ctrl Pts',(-13.5839487066755,4.45227095397745,-4.46362126645189));
#69408=CARTESIAN_POINT('Ctrl Pts',(-13.5178461200266,5.82912718297219,-2.83706456600194));
#69409=CARTESIAN_POINT('Ctrl Pts',(-13.4186922400531,6.47593427309586,0.295071888562534));
#69410=CARTESIAN_POINT('Ctrl Pts',(-13.3195383600797,5.54718661553207,3.35454744289073));
#69411=CARTESIAN_POINT('Ctrl Pts',(-13.2203844801062,3.26875126278153,5.59827586641925));
#69412=CARTESIAN_POINT('Ctrl Pts',(-13.1212306001328,0.195029276623322,
6.47969774398204));
#69413=CARTESIAN_POINT('Ctrl Pts',(-13.0220767201594,-2.92615231197546,
5.78469244453168));
#69414=CARTESIAN_POINT('Ctrl Pts',(-12.9229228401859,-5.33538328621662,
3.6821860861499));
#69415=CARTESIAN_POINT('Ctrl Pts',(-12.849812127386,-6.15465544744627,1.47135071718486));
#69416=CARTESIAN_POINT('Ctrl Pts',(-12.8097527079106,-6.21953641508352,
0.219232564831544));
#69417=CARTESIAN_POINT('Ctrl Pts',(-12.8027445817596,-6.21931067987726,
0.000159553896288585));
#69418=CARTESIAN_POINT('Ctrl Pts',(-14.0290837546341,4.02546580733783,-5.64465357962329));
#69419=CARTESIAN_POINT('Ctrl Pts',(-13.9960324613096,4.96323423627052,-4.9758871632932));
#69420=CARTESIAN_POINT('Ctrl Pts',(-13.9299298746607,6.49810487752479,-3.16265926536026));
#69421=CARTESIAN_POINT('Ctrl Pts',(-13.8307759946872,7.2191425518147,0.328935708229076));
#69422=CARTESIAN_POINT('Ctrl Pts',(-13.7316221147138,6.18380750178624,3.7395308793763));
#69423=CARTESIAN_POINT('Ctrl Pts',(-13.6324682347404,3.64388833136868,6.24075999226346));
#69424=CARTESIAN_POINT('Ctrl Pts',(-13.5333143547669,0.217411741742154,
7.22333793608995));
#69425=CARTESIAN_POINT('Ctrl Pts',(-13.4341604747935,-3.26197113461037,
6.44857060223313));
#69426=CARTESIAN_POINT('Ctrl Pts',(-13.33500659482,-5.94769663919919,4.1047708542473));
#69427=CARTESIAN_POINT('Ctrl Pts',(-13.2358527148466,-7.1863223146633,0.76229495696539));
#69428=CARTESIAN_POINT('Ctrl Pts',(-13.1366988348732,-6.67648114875678,
-2.76566822514195));
#69429=CARTESIAN_POINT('Ctrl Pts',(-13.0375449548997,-4.54222174007392,
-5.62072250746908));
#69430=CARTESIAN_POINT('Ctrl Pts',(-12.9383910749263,-1.3028183504887,-7.10823352255506));
#69431=CARTESIAN_POINT('Ctrl Pts',(-12.8392371949529,2.2535666263224,-6.86627590756217));
#69432=CARTESIAN_POINT('Ctrl Pts',(-12.7400833149794,5.26164846117041,-4.95372269926303));
#69433=CARTESIAN_POINT('Ctrl Pts',(-12.640929435006,6.98954673567817,-1.83590510727142));
#69434=CARTESIAN_POINT('Ctrl Pts',(-12.5417755550326,7.0168558409393,1.72859639764328));
#69435=CARTESIAN_POINT('Ctrl Pts',(-12.4426216750591,5.33693130930571,4.87252253811412));
#69436=CARTESIAN_POINT('Ctrl Pts',(-12.3434677950857,2.35850660217995,6.83094122079118));
#69437=CARTESIAN_POINT('Ctrl Pts',(-12.2443139151123,-1.19375372156009,
7.1273602146869));
#69438=CARTESIAN_POINT('Ctrl Pts',(-12.1451600351388,-4.45556821727479,
5.68965933289867));
#69439=CARTESIAN_POINT('Ctrl Pts',(-12.0460061551654,-6.63332226702549,
2.86763791460573));
#69440=CARTESIAN_POINT('Ctrl Pts',(-11.9468522751919,-7.19715819185692,
-0.652093136928579));
#69441=CARTESIAN_POINT('Ctrl Pts',(-11.8476983952185,-6.00989209247491,
-4.01316689555907));
#69442=CARTESIAN_POINT('Ctrl Pts',(-11.7485445152451,-3.36039132628151,
-6.39781850589597));
#69443=CARTESIAN_POINT('Ctrl Pts',(-11.6493906352716,0.106708261150547,
-7.22585115007998));
#69444=CARTESIAN_POINT('Ctrl Pts',(-11.5502367552982,3.54784523293374,-6.29580064022737));
#69445=CARTESIAN_POINT('Ctrl Pts',(-11.4510828753247,6.1257749770444,-3.8339525855188));
#69446=CARTESIAN_POINT('Ctrl Pts',(-11.3519289953513,7.21327521028865,-0.439286055197895));
#69447=CARTESIAN_POINT('Ctrl Pts',(-11.2527751153779,6.54575207362621,3.06226081323672));
#69448=CARTESIAN_POINT('Ctrl Pts',(-11.1536212354045,4.28561704737463,5.81874539921091));
#69449=CARTESIAN_POINT('Ctrl Pts',(-11.054467355431,0.982771483491727,7.15950219700309));
#69450=CARTESIAN_POINT('Ctrl Pts',(-10.9553134754576,-2.5591869480573,6.75831884883418));
#69451=CARTESIAN_POINT('Ctrl Pts',(-10.8561595954841,-5.47848330574273,
4.7128051271331));
#69452=CARTESIAN_POINT('Ctrl Pts',(-10.7570057155107,-7.06483922335105,
1.52064402337556));
#69453=CARTESIAN_POINT('Ctrl Pts',(-10.6578518355373,-6.93228693627894,
-2.04149683583503));
#69454=CARTESIAN_POINT('Ctrl Pts',(-10.5586979555638,-5.11307703177873,
-5.1069320305567));
#69455=CARTESIAN_POINT('Ctrl Pts',(-10.4595440755904,-2.04983173125164,
-6.92982693659675));
#69456=CARTESIAN_POINT('Ctrl Pts',(-10.360390195617,1.51214715254185,-7.06666275456019));
#69457=CARTESIAN_POINT('Ctrl Pts',(-10.2612363156435,4.70621360902953,-5.48414669422815));
#69458=CARTESIAN_POINT('Ctrl Pts',(-10.1620824356701,6.75523643044027,-2.5673122650899));
#69459=CARTESIAN_POINT('Ctrl Pts',(-10.0629285556967,7.16067884503,0.974161165294735));
#69460=CARTESIAN_POINT('Ctrl Pts',(-9.96377467572322,5.82389482973557,4.27861665843151));
#69461=CARTESIAN_POINT('Ctrl Pts',(-9.86462079574978,3.07013014587324,6.54206484109023));
#69462=CARTESIAN_POINT('Ctrl Pts',(-9.76546691577634,-0.430611465607748,
7.21379825496357));
#69463=CARTESIAN_POINT('Ctrl Pts',(-9.6663130358029,-3.82658330698325,6.13038103973526));
#69464=CARTESIAN_POINT('Ctrl Pts',(-9.56715915582948,-6.2915296523324,3.55541363718072));
#69465=CARTESIAN_POINT('Ctrl Pts',(-9.46800527585602,-7.22571760425057,
0.115397579055486));
#69466=CARTESIAN_POINT('Ctrl Pts',(-9.36885139588261,-6.40185489401093,
-3.3526952461649));
#69467=CARTESIAN_POINT('Ctrl Pts',(-9.26969751590916,-4.02039114649391,
-6.00506174213237));
#69468=CARTESIAN_POINT('Ctrl Pts',(-9.17054363593573,-0.660747555210352,
-7.19636881808541));
#69469=CARTESIAN_POINT('Ctrl Pts',(-9.07138975596229,2.85965898593902,-6.63676592790242));
#69470=CARTESIAN_POINT('Ctrl Pts',(-8.97223587598885,5.68429721048297,-4.46240705455296));
#69471=CARTESIAN_POINT('Ctrl Pts',(-8.87308199601543,7.12591951576202,-1.20232381350058));
#69472=CARTESIAN_POINT('Ctrl Pts',(-8.77392811604198,6.83377249745176,2.35029039709997));
#69473=CARTESIAN_POINT('Ctrl Pts',(-8.67477423606854,4.87893688235586,5.33106803517046));
#69474=CARTESIAN_POINT('Ctrl Pts',(-8.57562035609512,1.73703325734962,7.01477205335211));
#69475=CARTESIAN_POINT('Ctrl Pts',(-8.47646647612167,-1.82749862903197,
6.99174944191472));
#69476=CARTESIAN_POINT('Ctrl Pts',(-8.37731259614824,-4.94739160882633,
5.26760170917879));
#69477=CARTESIAN_POINT('Ctrl Pts',(-8.27815871617481,-6.86356122573495,
2.26182200851794));
#69478=CARTESIAN_POINT('Ctrl Pts',(-8.17900483620136,-7.10979450987494,
-1.29426949472691));
#69479=CARTESIAN_POINT('Ctrl Pts',(-8.07985095622793,-5.62618175927108,
-4.53545921702244));
#69480=CARTESIAN_POINT('Ctrl Pts',(-7.98069707625449,-2.77369284867334,
-6.67315064110252));
#69481=CARTESIAN_POINT('Ctrl Pts',(-7.88154319628106,0.753648417953927,
-7.18723351225935));
#69482=CARTESIAN_POINT('Ctrl Pts',(-7.78238931630763,4.09762352321354,-5.95262907962823));
#69483=CARTESIAN_POINT('Ctrl Pts',(-7.68323543633418,6.44462778864662,-3.26972233736018));
#69484=CARTESIAN_POINT('Ctrl Pts',(-7.58408155636075,7.22362417282433,0.20872303997529));
#69485=CARTESIAN_POINT('Ctrl Pts',(-7.48492767638731,6.24507923643584,3.63638513200491));
#69486=CARTESIAN_POINT('Ctrl Pts',(-7.38577379641388,3.74707750860212,6.17929782759794));
#69487=CARTESIAN_POINT('Ctrl Pts',(-7.28661991644044,0.337394414854048,
7.21875865412148));
#69488=CARTESIAN_POINT('Ctrl Pts',(-7.18746603646701,-3.1543783074859,6.50186196338333));
#69489=CARTESIAN_POINT('Ctrl Pts',(-7.08831215649357,-5.87867613308897,
4.20303205077935));
#69490=CARTESIAN_POINT('Ctrl Pts',(-6.98915827652014,-7.17266474451676,
0.88158491388799));
#69491=CARTESIAN_POINT('Ctrl Pts',(-6.89000439654669,-6.72151070103148,
-2.65435592819569));
#69492=CARTESIAN_POINT('Ctrl Pts',(-6.79085051657327,-4.63498187737245,
-5.54447964141429));
#69493=CARTESIAN_POINT('Ctrl Pts',(-6.69169663659982,-1.42074042987509,
-7.08560569948305));
#69494=CARTESIAN_POINT('Ctrl Pts',(-6.59254275662639,2.13917376464837,-6.90277097275208));
#69495=CARTESIAN_POINT('Ctrl Pts',(-6.49338887665296,5.17861704411722,-5.0404599996436));
#69496=CARTESIAN_POINT('Ctrl Pts',(-6.39423499667951,6.95807873807318,-1.95178169178893));
#69497=CARTESIAN_POINT('Ctrl Pts',(-6.29508111670609,7.04460754940169,1.61177416921263));
#69498=CARTESIAN_POINT('Ctrl Pts',(-6.19592723673263,5.41715061631334,4.78317788690788));
#69499=CARTESIAN_POINT('Ctrl Pts',(-6.09677335675922,2.47167577142396,6.79081220315981));
#69500=CARTESIAN_POINT('Ctrl Pts',(-5.99761947678577,-1.07516927149738,
7.14621036181109));
#69501=CARTESIAN_POINT('Ctrl Pts',(-5.89846559681234,-4.36042063567106,
5.76290233976271));
#69502=CARTESIAN_POINT('Ctrl Pts',(-5.7993117168389,-6.58476140166159,2.97745340531404));
#69503=CARTESIAN_POINT('Ctrl Pts',(-5.70015783686546,-7.20699912732122,
-0.532423775220128));
#69504=CARTESIAN_POINT('Ctrl Pts',(-5.60100395689203,-6.07574048322174,
-3.91275977772325));
#69505=CARTESIAN_POINT('Ctrl Pts',(-5.50185007691859,-3.46622595304341,
-6.34110314851262));
#69506=CARTESIAN_POINT('Ctrl Pts',(-5.40269619694516,-0.0133625451907377,
-7.22662666394319));
#69507=CARTESIAN_POINT('Ctrl Pts',(-5.30354231697172,3.44275203198619,-6.35387833876942));
#69508=CARTESIAN_POINT('Ctrl Pts',(-5.20438843699829,6.0612290455365,-3.93520189509677));
#69509=CARTESIAN_POINT('Ctrl Pts',(-5.10523455702485,7.20498087321364,-0.559072548292375));
#69510=CARTESIAN_POINT('Ctrl Pts',(-5.00608067705141,6.59572738173239,2.95308174683567));
#69511=CARTESIAN_POINT('Ctrl Pts',(-4.90692679707797,4.38170277602357,5.74673753361121));
#69512=CARTESIAN_POINT('Ctrl Pts',(-4.80777291710454,1.10158952851184,7.14218538042113));
#69513=CARTESIAN_POINT('Ctrl Pts',(-4.7086190371311,-2.44654556902168,6.79990634320274));
#69514=CARTESIAN_POINT('Ctrl Pts',(-4.60946515715767,-5.39942476351695,
4.80317850186191));
#69515=CARTESIAN_POINT('Ctrl Pts',(-4.51031127718423,-7.03859882854682,
1.63781501654116));
#69516=CARTESIAN_POINT('Ctrl Pts',(-4.4111573972108,-6.96524909885898,-1.92603647122083));
#69517=CARTESIAN_POINT('Ctrl Pts',(-4.31200351723736,-5.19722190445262,
-5.02127433760656));
#69518=CARTESIAN_POINT('Ctrl Pts',(-4.21284963726393,-2.16468647557985,
-6.89481282995197));
#69519=CARTESIAN_POINT('Ctrl Pts',(-4.11369575729048,1.39452722944346,-7.09081132903485));
#69520=CARTESIAN_POINT('Ctrl Pts',(-4.01454187731705,4.61444598088623,-5.5615824894639));
#69521=CARTESIAN_POINT('Ctrl Pts',(-3.91538799734361,6.71164858751094,-2.67919479235665));
#69522=CARTESIAN_POINT('Ctrl Pts',(-3.81623411737018,7.17587591199851,0.855053444661745));
#69523=CARTESIAN_POINT('Ctrl Pts',(-3.71708023739674,5.89417928960641,4.18126320620973));
#69524=CARTESIAN_POINT('Ctrl Pts',(-3.61792635742331,3.17840146303416,6.49015220448725));
#69525=CARTESIAN_POINT('Ctrl Pts',(-3.51877247744987,-0.310696205625941,
7.21995701963925));
#69526=CARTESIAN_POINT('Ctrl Pts',(-3.41961859747644,-3.72420004403323,
6.19311274963175));
#69527=CARTESIAN_POINT('Ctrl Pts',(-3.32046471750299,-6.23158870993929,
3.65945537584293));
#69528=CARTESIAN_POINT('Ctrl Pts',(-3.22131083752956,-7.22280289217062,
0.235435508112602));
#69529=CARTESIAN_POINT('Ctrl Pts',(-3.12215695755613,-6.45667557523428,
-3.24586691252144));
#69530=CARTESIAN_POINT('Ctrl Pts',(-3.02300307758269,-4.11960909459448,
-5.93743483377822));
#69531=CARTESIAN_POINT('Ctrl Pts',(-2.92384919760925,-0.780222582471201,
-7.18439727600238));
#69532=CARTESIAN_POINT('Ctrl Pts',(-2.82469531763581,2.74899570870432,-6.68336248389639));
#69533=CARTESIAN_POINT('Ctrl Pts',(-2.72554143766238,5.60937057274208,-4.55623455007352));
#69534=CARTESIAN_POINT('Ctrl Pts',(-2.62638755768894,7.10495951656942,-1.32055358298638));
#69535=CARTESIAN_POINT('Ctrl Pts',(-2.52723367771551,6.87187880198643,2.23642420583352));
#69536=CARTESIAN_POINT('Ctrl Pts',(-2.42807979774207,4.96683804969124,5.24926959545495));
#69537=CARTESIAN_POINT('Ctrl Pts',(-2.32892591776863,1.85334252510417,6.9849433055873));
#69538=CARTESIAN_POINT('Ctrl Pts',(-2.2297720377952,-1.71107984604937,7.02114785900938));
#69539=CARTESIAN_POINT('Ctrl Pts',(-2.13061815782176,-4.85918854137058,
5.34907451967547));
#69540=CARTESIAN_POINT('Ctrl Pts',(-2.03146427784833,-6.82503408988951,
2.37554649911859));
#69541=CARTESIAN_POINT('Ctrl Pts',(-1.93231039787489,-7.13031713677931,
-1.17596302092359));
#69542=CARTESIAN_POINT('Ctrl Pts',(-1.83315651790145,-5.70076089845598,
-4.44135527471782));
#69543=CARTESIAN_POINT('Ctrl Pts',(-1.73400263792802,-2.88418304909733,
-6.62614515664486));
#69544=CARTESIAN_POINT('Ctrl Pts',(-1.63484875795458,0.634129935366402,
-7.19876313839403));
#69545=CARTESIAN_POINT('Ctrl Pts',(-1.53569487798115,3.99815616053177,-6.01988860475261));
#69546=CARTESIAN_POINT('Ctrl Pts',(-1.43654099800771,6.38941241731386,-3.37634720653903));
#69547=CARTESIAN_POINT('Ctrl Pts',(-1.33738711803427,7.22609494920389,0.0886751527681432));
#69548=CARTESIAN_POINT('Ctrl Pts',(-1.23823323806084,6.30463500915592,3.5321224354422));
#69549=CARTESIAN_POINT('Ctrl Pts',(-1.1390793580874,3.84922808147728,6.11618792013417));
#69550=CARTESIAN_POINT('Ctrl Pts',(-1.03992547811397,0.457286078935402,
7.21215646943689));
#69551=CARTESIAN_POINT('Ctrl Pts',(-0.940771598140529,-3.04591575105879,
6.55337384368391));
#69552=CARTESIAN_POINT('Ctrl Pts',(-0.841617718167091,-5.80803212818724,
4.30012491627548));
#69553=CARTESIAN_POINT('Ctrl Pts',(-0.742463838193658,-7.157027305729,1.00063561933304));
#69554=CARTESIAN_POINT('Ctrl Pts',(-0.64330995822022,-6.76468448986276,
-2.54231297251901));
#69555=CARTESIAN_POINT('Ctrl Pts',(-0.544156078246784,-4.72646251042451,
-5.46670500714828));
#69556=CARTESIAN_POINT('Ctrl Pts',(-0.445002198273351,-1.53827024412814,
-7.06102231646795));
#69557=CARTESIAN_POINT('Ctrl Pts',(-0.345848318299913,2.02419031901898,
-6.93736009228426));
#69558=CARTESIAN_POINT('Ctrl Pts',(-0.246694438326475,5.09415597362008,
-5.1258059282477));
#69559=CARTESIAN_POINT('Ctrl Pts',(-0.147540558353041,6.92468981354721,
-2.06711936853776));
#69560=CARTESIAN_POINT('Ctrl Pts',(-0.0483866783796038,7.07041445130143,
1.49450693690473));
#69561=CARTESIAN_POINT('Ctrl Pts',(0.0507672015938331,5.49587440551356,
4.69251276145835));
#69562=CARTESIAN_POINT('Ctrl Pts',(0.149921081567267,2.58416258427939,6.74880843080014));
#69563=CARTESIAN_POINT('Ctrl Pts',(0.249074961540705,-0.95628799914268,
7.16308765549634));
#69564=CARTESIAN_POINT('Ctrl Pts',(0.348228841514144,-4.26406926967639,
5.83455437553118));
#69565=CARTESIAN_POINT('Ctrl Pts',(0.447382721487575,-6.53438267699997,
3.08644690998419));
#69566=CARTESIAN_POINT('Ctrl Pts',(0.546536601461014,-7.21485042175099,
-0.412607427693591));
#69567=CARTESIAN_POINT('Ctrl Pts',(0.645690481434445,-6.13991154033284,
-3.8112724613331));
#69568=CARTESIAN_POINT('Ctrl Pts',(0.744844361407885,-3.57110365651654,
-6.28263719882365));
#69569=CARTESIAN_POINT('Ctrl Pts',(0.843998241381321,-0.133429662532856,
-7.22540711813424));
#69570=CARTESIAN_POINT('Ctrl Pts',(0.943152121354755,3.33670838822898,-6.41020191800155));
#69571=CARTESIAN_POINT('Ctrl Pts',(1.04230600132819,5.99500978654503,-4.0353648108762));
#69572=CARTESIAN_POINT('Ctrl Pts',(1.14145988130163,7.19469745234014,-0.678704697875825));
#69573=CARTESIAN_POINT('Ctrl Pts',(1.24061376127506,6.64388180304984,2.84308742122567));
#69574=CARTESIAN_POINT('Ctrl Pts',(1.3397676412485,4.47657884511091,5.67314316240424));
#69575=CARTESIAN_POINT('Ctrl Pts',(1.43892152122194,1.22010345698743,7.12289681603459));
#69576=CARTESIAN_POINT('Ctrl Pts',(1.53807540119537,-2.33322877054477,6.83961658296214));
#69577=CARTESIAN_POINT('Ctrl Pts',(1.63722928116881,-5.31887559855225,4.89222585994902));
#69578=CARTESIAN_POINT('Ctrl Pts',(1.73638316114225,-7.01041528314337,1.75453385703958));
#69579=CARTESIAN_POINT('Ctrl Pts',(1.83553704111569,-6.9962883605478,-1.81004438445359));
#69580=CARTESIAN_POINT('Ctrl Pts',(1.93469092108911,-5.27993197666347,-4.93423041815386));
#69581=CARTESIAN_POINT('Ctrl Pts',(2.03384480106256,-2.27894361349163,-6.85789526780295));
#69582=CARTESIAN_POINT('Ctrl Pts',(2.13299868103599,1.27652231829741,-7.11300233857104));
#69583=CARTESIAN_POINT('Ctrl Pts',(2.23215256100943,4.5214044396118,-5.63748289497069));
#69584=CARTESIAN_POINT('Ctrl Pts',(2.33130644098286,6.66620785535008,-2.79033767255823));
#69585=CARTESIAN_POINT('Ctrl Pts',(2.4304603209563,7.18909193019322,0.73570966886304));
#69586=CARTESIAN_POINT('Ctrl Pts',(2.52961420092973,5.96283653953145,4.08275542990979));
#69587=CARTESIAN_POINT('Ctrl Pts',(2.62876808090317,3.28579531681644,6.43644782730468));
#69588=CARTESIAN_POINT('Ctrl Pts',(2.72792196087661,-0.190695171538537,
7.22412256604076));
#69589=CARTESIAN_POINT('Ctrl Pts',(2.82707584085004,-3.62078863873284,6.25413472282594));
#69590=CARTESIAN_POINT('Ctrl Pts',(2.92622972082349,-6.16992740875923,3.76248684625687));
#69591=CARTESIAN_POINT('Ctrl Pts',(3.02538360079691,-7.21789417615659,0.35540844033487));
#69592=CARTESIAN_POINT('Ctrl Pts',(3.12453748077035,-6.50971375778922,-3.13814249026964));
#69593=CARTESIAN_POINT('Ctrl Pts',(3.22369136074378,-4.21768973951514,-5.86816877388985));
#69594=CARTESIAN_POINT('Ctrl Pts',(3.32284524071722,-0.899482213157528,
-7.17044233265069));
#69595=CARTESIAN_POINT('Ctrl Pts',(3.42199912069066,2.63757351439253,-6.72811395961489));
#69596=CARTESIAN_POINT('Ctrl Pts',(3.52115300066409,5.5328953524373,-4.64880420294464));
#69597=CARTESIAN_POINT('Ctrl Pts',(3.62030688063753,7.0820380464371,-1.43841878635096));
#69598=CARTESIAN_POINT('Ctrl Pts',(3.71946076061097,6.90808798262623,2.12194060341662));
#69599=CARTESIAN_POINT('Ctrl Pts',(3.81861464058441,5.05336801840377,5.16602198653642));
#69600=CARTESIAN_POINT('Ctrl Pts',(3.91776852055784,1.96914014011108,6.95318621974456));
#69601=CARTESIAN_POINT('Ctrl Pts',(4.01692240053127,-1.59418868556376,7.04860794358157));
#69602=CARTESIAN_POINT('Ctrl Pts',(4.11607628050472,-4.76964399176775,5.42907060692931));
#69603=CARTESIAN_POINT('Ctrl Pts',(4.21523016047815,-6.78462276778132,2.48861517244911));
#69604=CARTESIAN_POINT('Ctrl Pts',(4.31438404045158,-7.14887128193105,-1.05733190097141));
#69605=CARTESIAN_POINT('Ctrl Pts',(4.41353792042502,-5.77376624502238,-4.3460251992502));
#69606=CARTESIAN_POINT('Ctrl Pts',(4.51269180039845,-2.9938769721112,-6.57731039820468));
#69607=CARTESIAN_POINT('Ctrl Pts',(4.6118456803719,0.514436312362811,-7.20830537738637));
#69608=CARTESIAN_POINT('Ctrl Pts',(4.71099956034533,3.897585170993,-6.08548625378336));
#69609=CARTESIAN_POINT('Ctrl Pts',(4.81015344031876,6.33243283244007,-3.48203989073616));
#69610=CARTESIAN_POINT('Ctrl Pts',(4.9093073202922,7.22657136347239,-0.031397359545163));
#69611=CARTESIAN_POINT('Ctrl Pts',(5.00846120026564,6.36244919040953,3.42688490344027));
#69612=CARTESIAN_POINT('Ctrl Pts',(5.10761508023907,3.95031806190394,6.05138897039844));
#69613=CARTESIAN_POINT('Ctrl Pts',(5.20676896021251,0.577047496600863,7.2035642704365));
#69614=CARTESIAN_POINT('Ctrl Pts',(5.30592284018594,-2.93660455179739,6.60307449482303));
#69615=CARTESIAN_POINT('Ctrl Pts',(5.40507672015939,-5.7357997190033,4.39603458568039));
#69616=CARTESIAN_POINT('Ctrl Pts',(5.50423060013282,-7.13938491615856,1.11940244029185));
#69617=CARTESIAN_POINT('Ctrl Pts',(5.60338448010626,-6.80604716325542,-2.4295533466182));
#69618=CARTESIAN_POINT('Ctrl Pts',(5.70253836007969,-4.81652869657057,-5.38745002130588));
#69619=CARTESIAN_POINT('Ctrl Pts',(5.80169224005313,-1.65559090405508,-7.03443221887737));
#69620=CARTESIAN_POINT('Ctrl Pts',(5.90084612002656,1.90909700073592,-6.97015991709384));
#69621=CARTESIAN_POINT('Ctrl Pts',(5.96694870667552,3.97444177895362,-5.79628844103034));
#69622=CARTESIAN_POINT('Ctrl Pts',(6.,4.80478746383271,-4.99805026259201));
#69623=CARTESIAN_POINT('Ctrl Pts',(-13.8917225030894,3.88732569387146,-5.4509485220505));
#69624=CARTESIAN_POINT('Ctrl Pts',(-13.8586712097649,4.79291314217283,-4.8051318643461));
#69625=CARTESIAN_POINT('Ctrl Pts',(-13.792568623116,6.27511231267392,-3.05412769890749));
#69626=CARTESIAN_POINT('Ctrl Pts',(-13.6934147431425,6.97140645890842,0.317647768340228));
#69627=CARTESIAN_POINT('Ctrl Pts',(-13.5942608631691,5.97160053970152,3.61120306721445));
#69628=CARTESIAN_POINT('Ctrl Pts',(-13.4951069831956,3.51884264183963,6.02659861698205));
#69629=CARTESIAN_POINT('Ctrl Pts',(-13.3959531032222,0.209950920035877,
6.97545787205399));
#69630=CARTESIAN_POINT('Ctrl Pts',(-13.2967992232488,-3.1500315270654,6.22727788299931));
#69631=CARTESIAN_POINT('Ctrl Pts',(-13.1976453432753,-5.743592188205,3.9639092648815));
#69632=CARTESIAN_POINT('Ctrl Pts',(-13.0984914633019,-6.93971249918703,
0.73613562115432));
#69633=CARTESIAN_POINT('Ctrl Pts',(-12.9993375833285,-6.44736732501885,
-2.67076002303153));
#69634=CARTESIAN_POINT('Ctrl Pts',(-12.900183703355,-4.38634834390208,-5.42783868181853));
#69635=CARTESIAN_POINT('Ctrl Pts',(-12.8010298233816,-1.25811011462824,
-6.86430344530502));
#69636=CARTESIAN_POINT('Ctrl Pts',(-12.7018759434082,2.17623198621772,-6.63064898179542));
#69637=CARTESIAN_POINT('Ctrl Pts',(-12.6027220634347,5.08108681930493,-4.78372800833562));
#69638=CARTESIAN_POINT('Ctrl Pts',(-12.5035681834613,6.74968957992116,-1.77290317110548));
#69639=CARTESIAN_POINT('Ctrl Pts',(-12.4044143034878,6.77606153080561,1.66927692657171));
#69640=CARTESIAN_POINT('Ctrl Pts',(-12.3052604235144,5.15378621954096,4.70531435687567));
#69641=CARTESIAN_POINT('Ctrl Pts',(-12.206106543541,2.27757078376049,6.5965268596998));
#69642=CARTESIAN_POINT('Ctrl Pts',(-12.1069526635675,-1.15278820789294,
6.88277377527959));
#69643=CARTESIAN_POINT('Ctrl Pts',(-12.0077987835941,-4.30266847136972,
5.49440983297767));
#69644=CARTESIAN_POINT('Ctrl Pts',(-11.9086449036207,-6.40568950736929,
2.76923046417301));
#69645=CARTESIAN_POINT('Ctrl Pts',(-11.8094910236473,-6.95017652641927,
-0.629715547790527));
#69646=CARTESIAN_POINT('Ctrl Pts',(-11.7103371436738,-5.80365330786967,
-3.87544883835896));
#69647=CARTESIAN_POINT('Ctrl Pts',(-11.6111832637004,-3.24507427694579,
-6.17826742370054));
#69648=CARTESIAN_POINT('Ctrl Pts',(-11.5120293837269,0.103046401378646,
-6.9778848412012));
#69649=CARTESIAN_POINT('Ctrl Pts',(-11.4128755037535,3.4260954115478,-6.0797504595955));
#69650=CARTESIAN_POINT('Ctrl Pts',(-11.3137216237801,5.91555949121022,-3.70238454580946));
#69651=CARTESIAN_POINT('Ctrl Pts',(-11.2145677438066,6.96574046432281,-0.424211271703603));
#69652=CARTESIAN_POINT('Ctrl Pts',(-11.1154138638332,6.32112442121259,2.95717457565572));
#69653=CARTESIAN_POINT('Ctrl Pts',(-11.0162599838598,4.13854943991446,5.61906611036594));
#69654=CARTESIAN_POINT('Ctrl Pts',(-10.9171061038863,0.949046153122836,
6.91381275553423));
#69655=CARTESIAN_POINT('Ctrl Pts',(-10.8179522239129,-2.47136447177597,
6.52639663726845));
#69656=CARTESIAN_POINT('Ctrl Pts',(-10.7187983439394,-5.29048063929369,
4.55107789700226));
#69657=CARTESIAN_POINT('Ctrl Pts',(-10.619644463966,-6.82239828889908,1.46846076111849));
#69658=CARTESIAN_POINT('Ctrl Pts',(-10.5204905839926,-6.69439473950172,
-1.97143970007961));
#69659=CARTESIAN_POINT('Ctrl Pts',(-10.4213367040191,-4.93761384934533,
-4.93167972338762));
#69660=CARTESIAN_POINT('Ctrl Pts',(-10.3221828240457,-1.97948857061021,
-6.6920191585307));
#69661=CARTESIAN_POINT('Ctrl Pts',(-10.2230289440723,1.46025547360891,-6.82415924280158));
#69662=CARTESIAN_POINT('Ctrl Pts',(-10.1238750640988,4.54471257708354,-5.29594967980412));
#69663=CARTESIAN_POINT('Ctrl Pts',(-10.0247211841254,6.52341999685084,-2.47921095593041));
#69664=CARTESIAN_POINT('Ctrl Pts',(-9.92556730415195,6.91494902505595,0.940731311372487));
#69665=CARTESIAN_POINT('Ctrl Pts',(-9.82641342417852,5.62403883018155,4.13178928019433));
#69666=CARTESIAN_POINT('Ctrl Pts',(-9.72725954420508,2.96477385991635,6.31756372178987));
#69667=CARTESIAN_POINT('Ctrl Pts',(-9.62810566423165,-0.415834364132817,
6.96624555990707));
#69668=CARTESIAN_POINT('Ctrl Pts',(-9.5289517842582,-3.6952681555164,5.92000748970347));
#69669=CARTESIAN_POINT('Ctrl Pts',(-9.42979790428479,-6.0756260372859,3.43340409424414));
#69670=CARTESIAN_POINT('Ctrl Pts',(-9.33064402431132,-6.97775587820442,
0.111437531839213));
#69671=CARTESIAN_POINT('Ctrl Pts',(-9.23149014433791,-6.18216529688604,
-3.23764229977566));
#69672=CARTESIAN_POINT('Ctrl Pts',(-9.13233626436446,-3.88242517789877,
-5.79898871850399));
#69673=CARTESIAN_POINT('Ctrl Pts',(-9.03318238439104,-0.638072976262717,
-6.94941424123515));
#69674=CARTESIAN_POINT('Ctrl Pts',(-8.93402850441759,2.76152534484023,-6.40901499367288));
#69675=CARTESIAN_POINT('Ctrl Pts',(-8.83487462444415,5.48923172012373,-4.30927262332129));
#69676=CARTESIAN_POINT('Ctrl Pts',(-8.73572074447072,6.88138251617669,-1.16106420381327));
#69677=CARTESIAN_POINT('Ctrl Pts',(-8.63656686449728,6.59926097670287,2.26963653052322));
#69678=CARTESIAN_POINT('Ctrl Pts',(-8.53741298452385,4.71150858292888,5.14812415276733));
#69679=CARTESIAN_POINT('Ctrl Pts',(-8.43825910455041,1.677424262329,6.77404925162703));
#69680=CARTESIAN_POINT('Ctrl Pts',(-8.33910522457698,-1.76478517422783,
6.75181669687089));
#69681=CARTESIAN_POINT('Ctrl Pts',(-8.23995134460354,-4.77761417910377,
5.08683577235843));
#69682=CARTESIAN_POINT('Ctrl Pts',(-8.14079746463011,-6.62802745849286,
2.18420407214696));
#69683=CARTESIAN_POINT('Ctrl Pts',(-8.04164358465666,-6.86581086491974,
-1.24985462613414));
#69684=CARTESIAN_POINT('Ctrl Pts',(-7.94248970468324,-5.43311059091299,
-4.37981788733594));
#69685=CARTESIAN_POINT('Ctrl Pts',(-7.8433358247098,-2.6785092691387,-6.44415110890929));
#69686=CARTESIAN_POINT('Ctrl Pts',(-7.74418194473636,0.727785801563031,
-6.94059242762187));
#69687=CARTESIAN_POINT('Ctrl Pts',(-7.64502806476293,3.95700720561687,-5.74835536427725));
#69688=CARTESIAN_POINT('Ctrl Pts',(-7.54587418478947,6.22347037318691,-3.15751673524993));
#69689=CARTESIAN_POINT('Ctrl Pts',(-7.44672030481606,6.97573428613011,0.201560384569647));
#69690=CARTESIAN_POINT('Ctrl Pts',(-7.34756642484261,6.03076963957991,3.51159692641963));
#69691=CARTESIAN_POINT('Ctrl Pts',(-7.24841254486919,3.6184907221333,5.9672456219896));
#69692=CARTESIAN_POINT('Ctrl Pts',(-7.14925866489573,0.325816201305197,
6.97103573526099));
#69693=CARTESIAN_POINT('Ctrl Pts',(-7.05010478492232,-3.04613091496857,
6.2787404682939));
#69694=CARTESIAN_POINT('Ctrl Pts',(-6.95095090494887,-5.67694022799777,
4.05879847578804));
#69695=CARTESIAN_POINT('Ctrl Pts',(-6.85179702497544,-6.92652360977957,
0.851331957866649));
#69696=CARTESIAN_POINT('Ctrl Pts',(-6.75264314500199,-6.49085161824571,
-2.56326758049872));
#69697=CARTESIAN_POINT('Ctrl Pts',(-6.65348926502857,-4.4759252729696,-5.35421220816945));
#69698=CARTESIAN_POINT('Ctrl Pts',(-6.55433538505512,-1.37198551464726,
-6.84245213113814));
#69699=CARTESIAN_POINT('Ctrl Pts',(-6.4551815050817,2.06576469332199,-6.66589166212166));
#69700=CARTESIAN_POINT('Ctrl Pts',(-6.35602762510825,5.00090475433221,-4.86748878349157));
#69701=CARTESIAN_POINT('Ctrl Pts',(-6.25687374513482,6.71930145554519,-1.88480327059009));
#69702=CARTESIAN_POINT('Ctrl Pts',(-6.15771986516138,6.80286089627483,1.55646363441408));
#69703=CARTESIAN_POINT('Ctrl Pts',(-6.05856598518795,5.23125267639344,4.61903570618861));
#69704=CARTESIAN_POINT('Ctrl Pts',(-5.95941210521452,2.38685637713317,6.55777493165612));
#69705=CARTESIAN_POINT('Ctrl Pts',(-5.86025822524107,-1.03827316747647,
6.9009770503181));
#69706=CARTESIAN_POINT('Ctrl Pts',(-5.76110434526764,-4.21078602685766,
5.56513939226495));
#69707=CARTESIAN_POINT('Ctrl Pts',(-5.6619504652942,-6.35879508354843,2.87527746569948));
#69708=CARTESIAN_POINT('Ctrl Pts',(-5.56279658532077,-6.95967975489342,
-0.514152826157048));
#69709=CARTESIAN_POINT('Ctrl Pts',(-5.46364270534732,-5.86724200878069,
-3.77848734677226));
#69710=CARTESIAN_POINT('Ctrl Pts',(-5.3644888253739,-3.34727702405715,-6.12349834192333));
#69711=CARTESIAN_POINT('Ctrl Pts',(-5.26533494540046,-0.0129039886913769,
-6.9786337421013));
#69712=CARTESIAN_POINT('Ctrl Pts',(-5.16618106542702,3.32460864707202,-6.13583513167788));
#69713=CARTESIAN_POINT('Ctrl Pts',(-5.06702718545359,5.85322855362576,-3.8001593280202));
#69714=CARTESIAN_POINT('Ctrl Pts',(-4.96787330548015,6.95773076031128,-0.539887105177606));
#69715=CARTESIAN_POINT('Ctrl Pts',(-4.86871942550671,6.36938474897545,2.8517421585476));
#69716=CARTESIAN_POINT('Ctrl Pts',(-4.76956554553328,4.2313378374983,5.5495293065515));
#69717=CARTESIAN_POINT('Ctrl Pts',(-4.67041166555984,1.06378677232281,6.89709019241808));
#69718=CARTESIAN_POINT('Ctrl Pts',(-4.57125778558641,-2.36258855667067,
6.56655699215408));
#69719=CARTESIAN_POINT('Ctrl Pts',(-4.47210390561297,-5.21413511377609,
4.63834996896589));
#69720=CARTESIAN_POINT('Ctrl Pts',(-4.37295002563954,-6.79705837401175,
1.58161084960733));
#69721=CARTESIAN_POINT('Ctrl Pts',(-4.27379614566609,-6.72622575426015,
-1.85994153726566));
#69722=CARTESIAN_POINT('Ctrl Pts',(-4.17464226569266,-5.01887115997917,
-4.84896150725576));
#69723=CARTESIAN_POINT('Ctrl Pts',(-4.07548838571922,-2.09040189593921,
-6.65820661535616));
#69724=CARTESIAN_POINT('Ctrl Pts',(-3.97633450574579,1.34667186091541,-6.84747912142397));
#69725=CARTESIAN_POINT('Ctrl Pts',(-3.87718062577235,4.45609409767756,-5.37072814541586));
#69726=CARTESIAN_POINT('Ctrl Pts',(-3.77802674579892,6.4813279384732,-2.5872540604443));
#69727=CARTESIAN_POINT('Ctrl Pts',(-3.67887286582548,6.92962458106006,0.825710957228362));
#69728=CARTESIAN_POINT('Ctrl Pts',(-3.57971898585204,5.69191136961234,4.03777666294169));
#69729=CARTESIAN_POINT('Ctrl Pts',(-3.48056510587861,3.06932967860987,6.26743254796759));
#69730=CARTESIAN_POINT('Ctrl Pts',(-3.38141122590517,-0.300034182607279,
6.97219297700414));
#69731=CARTESIAN_POINT('Ctrl Pts',(-3.28225734593174,-3.59639833330539,
5.98058646350983));
#69732=CARTESIAN_POINT('Ctrl Pts',(-3.1831034659583,-6.01774206146008,3.53387547899653));
#69733=CARTESIAN_POINT('Ctrl Pts',(-3.08394958598486,-6.97494118899802,
0.227356172860154));
#69734=CARTESIAN_POINT('Ctrl Pts',(-2.98479570601143,-6.2351047212594,-3.13447994637828));
#69735=CARTESIAN_POINT('Ctrl Pts',(-2.88564182603799,-3.97823830795728,
-5.73368253258061));
#69736=CARTESIAN_POINT('Ctrl Pts',(-2.78648794606455,-0.753448032337097,
-6.93785352121866));
#69737=CARTESIAN_POINT('Ctrl Pts',(-2.68733406609112,2.65465964989922,-6.45401251645174));
#69738=CARTESIAN_POINT('Ctrl Pts',(-2.58818018611768,5.41687630636897,-4.39988028255512));
#69739=CARTESIAN_POINT('Ctrl Pts',(-2.48902630614424,6.86114179192153,-1.27523673506788));
#69740=CARTESIAN_POINT('Ctrl Pts',(-2.38987242617081,6.6360596041924,2.15967783452175));
#69741=CARTESIAN_POINT('Ctrl Pts',(-2.29071854619738,4.79639328513682,5.06913275359931));
#69742=CARTESIAN_POINT('Ctrl Pts',(-2.19156466622393,1.78974219685312,6.7452441236861));
#69743=CARTESIAN_POINT('Ctrl Pts',(-2.0924107862505,-1.65236148266087,6.7802062616072));
#69744=CARTESIAN_POINT('Ctrl Pts',(-1.99325690627706,-4.69243793694715,
5.1655127167802));
#69745=CARTESIAN_POINT('Ctrl Pts',(-1.89410302630363,-6.59082244117281,
2.29402593016113));
#69746=CARTESIAN_POINT('Ctrl Pts',(-1.7949491463302,-6.88562922599628,-1.13560802278984));
#69747=CARTESIAN_POINT('Ctrl Pts',(-1.69579526635675,-5.5051304310646,-4.28894326801897));
#69748=CARTESIAN_POINT('Ctrl Pts',(-1.59664138638332,-2.78520782666867,
-6.3987586906823));
#69749=CARTESIAN_POINT('Ctrl Pts',(-1.49748750640988,0.612368781399033,
-6.95172639672238));
#69750=CARTESIAN_POINT('Ctrl Pts',(-1.39833362643645,3.86095322002601,-5.81330677429719));
#69751=CARTESIAN_POINT('Ctrl Pts',(-1.29917974646301,6.17014980310849,-3.26048260638193));
#69752=CARTESIAN_POINT('Ctrl Pts',(-1.20002586648958,6.9781202739794,0.085632127128072));
#69753=CARTESIAN_POINT('Ctrl Pts',(-1.10087198651614,6.08828166342847,3.41091216628038));
#69754=CARTESIAN_POINT('Ctrl Pts',(-1.0017181065427,3.7171358393909,5.90630142905309));
#69755=CARTESIAN_POINT('Ctrl Pts',(-0.902564226569267,0.441593596660263,
6.96466011480154));
#69756=CARTESIAN_POINT('Ctrl Pts',(-0.80341034659583,-2.94139041968142,
6.32848463838897));
#69757=CARTESIAN_POINT('Ctrl Pts',(-0.704256466622392,-5.60872048188245,
4.15255944875339));
#69758=CARTESIAN_POINT('Ctrl Pts',(-0.605102586648959,-6.91142279399939,
0.966297253387595));
#69759=CARTESIAN_POINT('Ctrl Pts',(-0.505948706675522,-6.53254383143497,
-2.45506955292504));
#69760=CARTESIAN_POINT('Ctrl Pts',(-0.406794826702085,-4.5642666059668,
-5.27910653131522));
#69761=CARTESIAN_POINT('Ctrl Pts',(-0.307640946728652,-1.48548211072044,
-6.81871236510591));
#69762=CARTESIAN_POINT('Ctrl Pts',(-0.208487066755214,1.95472708327691,
-6.69929380227666));
#69763=CARTESIAN_POINT('Ctrl Pts',(-0.109333186781776,4.9193420966947,-4.94990593395533));
#69764=CARTESIAN_POINT('Ctrl Pts',(-0.0101793068083421,6.68705832384006,
-1.99618295576339));
#69765=CARTESIAN_POINT('Ctrl Pts',(0.0889745731650949,6.8277821942402,1.44322060937863));
#69766=CARTESIAN_POINT('Ctrl Pts',(0.188128453138532,5.30727493645564,4.53148189538351));
#69767=CARTESIAN_POINT('Ctrl Pts',(0.287282333111966,2.4954830302369,6.51721258400542));
#69768=CARTESIAN_POINT('Ctrl Pts',(0.386436213085403,-0.92347149068614,
6.91727517344862));
#69769=CARTESIAN_POINT('Ctrl Pts',(0.485590093058842,-4.11774110768632,
5.63433257710166));
#69770=CARTESIAN_POINT('Ctrl Pts',(0.584743973032274,-6.31014518309602,
2.98053068891579));
#69771=CARTESIAN_POINT('Ctrl Pts',(0.683897853005712,-6.96726161995643,
-0.398448162752206));
#69772=CARTESIAN_POINT('Ctrl Pts',(0.783051732979144,-5.9292109363657,-3.6804827253229));
#69773=CARTESIAN_POINT('Ctrl Pts',(0.882205612952583,-3.44855568618915,
-6.06703874213535));
#69774=CARTESIAN_POINT('Ctrl Pts',(0.981359492926021,-0.12885081635597,
-6.97745604690156));
#69775=CARTESIAN_POINT('Ctrl Pts',(1.08051337289945,3.22220405570829,-6.19022587977982));
#69776=CARTESIAN_POINT('Ctrl Pts',(1.17966725287289,5.78928171139015,-3.89688499772348));
#69777=CARTESIAN_POINT('Ctrl Pts',(1.27882113284633,6.9478002310022,-0.65541389167797));
#69778=CARTESIAN_POINT('Ctrl Pts',(1.37797501281976,6.41588667650881,2.74552245911695));
#69779=CARTESIAN_POINT('Ctrl Pts',(1.4771288927932,4.32295808686781,5.47846044053464));
#69780=CARTESIAN_POINT('Ctrl Pts',(1.57628277276664,1.17823371120998,6.87846354508673));
#69781=CARTESIAN_POINT('Ctrl Pts',(1.67543665274007,-2.25316040019159,6.6049045133391));
#69782=CARTESIAN_POINT('Ctrl Pts',(1.77459053271351,-5.13635011855482,4.72434152860911));
#69783=CARTESIAN_POINT('Ctrl Pts',(1.87374441268695,-6.76984199075704,1.69432430175027));
#69784=CARTESIAN_POINT('Ctrl Pts',(1.97289829266038,-6.75619985545904,-1.74792989917048));
#69785=CARTESIAN_POINT('Ctrl Pts',(2.07205217263382,-5.09874290755708,-4.76490463513752));
#69786=CARTESIAN_POINT('Ctrl Pts',(2.17120605260725,-2.20073812264447,-6.62255593671038));
#69787=CARTESIAN_POINT('Ctrl Pts',(2.27035993258069,1.23271647163726,-6.86890861199019));
#69788=CARTESIAN_POINT('Ctrl Pts',(2.36951381255412,4.36624542144878,-5.4440239105827));
#69789=CARTESIAN_POINT('Ctrl Pts',(2.46866769252756,6.43744657563682,-2.69458290003125));
#69790=CARTESIAN_POINT('Ctrl Pts',(2.56782157250099,6.94238707105695,0.710462648518286));
#69791=CARTESIAN_POINT('Ctrl Pts',(2.66697545247444,5.75821253933475,3.94264933403509));
#69792=CARTESIAN_POINT('Ctrl Pts',(2.76612933244787,3.17303814544387,6.21557111992748));
#69793=CARTESIAN_POINT('Ctrl Pts',(2.86528321242131,-0.184151170447852,
6.97621557620895));
#69794=CARTESIAN_POINT('Ctrl Pts',(2.96443709239474,-3.49653565104616,6.03951437288521));
#69795=CARTESIAN_POINT('Ctrl Pts',(3.06359097236818,-5.95819676363198,3.63337126442523));
#69796=CARTESIAN_POINT('Ctrl Pts',(3.16274485234161,-6.97020092320059,0.34321204751361));
#69797=CARTESIAN_POINT('Ctrl Pts',(3.26189873231505,-6.28632281617557,-3.03045225504537));
#69798=CARTESIAN_POINT('Ctrl Pts',(3.36105261228848,-4.07295316316151,-5.66679344515464));
#69799=CARTESIAN_POINT('Ctrl Pts',(3.46020649226192,-0.868615083505064,
-6.92437746342961));
#69800=CARTESIAN_POINT('Ctrl Pts',(3.55936037223536,2.54706108129972,-6.49722827575147));
#69801=CARTESIAN_POINT('Ctrl Pts',(3.6585142522088,5.34302545206699,-4.4892732639643));
#69802=CARTESIAN_POINT('Ctrl Pts',(3.75766813218223,6.83900690764945,-1.38905721085414));
#69803=CARTESIAN_POINT('Ctrl Pts',(3.85682201215567,6.67102621054105,2.04912291479273));
#69804=CARTESIAN_POINT('Ctrl Pts',(3.95597589212911,4.87995384353306,4.98874191572099));
#69805=CARTESIAN_POINT('Ctrl Pts',(4.05512977210254,1.90156603678858,6.71457683158443));
#69806=CARTESIAN_POINT('Ctrl Pts',(4.15428365207597,-1.53948162395885,6.80672401071309));
#69807=CARTESIAN_POINT('Ctrl Pts',(4.25343753204942,-4.60596624768756,5.24276361401157));
#69808=CARTESIAN_POINT('Ctrl Pts',(4.35259141202285,-6.55179789636906,2.40321447629372));
#69809=CARTESIAN_POINT('Ctrl Pts',(4.45174529199628,-6.90354665682992,-1.02104791403367));
#69810=CARTESIAN_POINT('Ctrl Pts',(4.55089917196972,-5.5756304857366,-4.19688459220349));
#69811=CARTESIAN_POINT('Ctrl Pts',(4.65005305194315,-2.89113743228502,-6.35159977285162));
#69812=CARTESIAN_POINT('Ctrl Pts',(4.74920693191659,0.496782631034447,-6.9609411789581));
#69813=CARTESIAN_POINT('Ctrl Pts',(4.84836081189003,3.76383348024845,-5.87665333808366));
#69814=CARTESIAN_POINT('Ctrl Pts',(4.94751469186346,6.1151255612177,-3.36254828190817));
#69815=CARTESIAN_POINT('Ctrl Pts',(5.0466685718369,6.97858033935209,-0.0303199103708891));
#69816=CARTESIAN_POINT('Ctrl Pts',(5.14582245181034,6.1441118612276,3.3092860236946));
#69817=CARTESIAN_POINT('Ctrl Pts',(5.24497633178377,3.81475676007768,5.8437261559544));
#69818=CARTESIAN_POINT('Ctrl Pts',(5.34413021175722,0.557245215207563,6.95636277045938));
#69819=CARTESIAN_POINT('Ctrl Pts',(5.44328409173064,-2.83583040405735,6.37647973446532));
#69820=CARTESIAN_POINT('Ctrl Pts',(5.54243797170409,-5.53896684004573,4.24517782883969));
#69821=CARTESIAN_POINT('Ctrl Pts',(5.64159185167752,-6.89438583043771,1.08098840635952));
#69822=CARTESIAN_POINT('Ctrl Pts',(5.74074573165095,-6.57248708042578,-2.34617944877944));
#69823=CARTESIAN_POINT('Ctrl Pts',(5.83989961162439,-4.65124203100119,-5.20257130344893));
#69824=CARTESIAN_POINT('Ctrl Pts',(5.93905349159782,-1.59877672992316,-6.79303474802668));
#69825=CARTESIAN_POINT('Ctrl Pts',(6.03820737157127,1.84358337102897,-6.73096805013745));
#69826=CARTESIAN_POINT('Ctrl Pts',(6.10430995822022,3.83805263429629,-5.59737979759625));
#69827=CARTESIAN_POINT('Ctrl Pts',(6.1373612515447,4.63990371690688,-4.82653440245809));
#69828=CARTESIAN_POINT('Ctrl Pts',(-13.7543612515447,3.74918558040509,-5.25724346447772));
#69829=CARTESIAN_POINT('Ctrl Pts',(-13.7213099582202,4.62259204807514,-4.634376565399));
#69830=CARTESIAN_POINT('Ctrl Pts',(-13.6552073715713,6.05211974782306,-2.94559613245471));
#69831=CARTESIAN_POINT('Ctrl Pts',(-13.5560534915978,6.72367036600214,0.306359828451381));
#69832=CARTESIAN_POINT('Ctrl Pts',(-13.4568996116244,5.7593935776168,3.48287525505259));
#69833=CARTESIAN_POINT('Ctrl Pts',(-13.357745731651,3.39379695231058,5.81243724170065));
#69834=CARTESIAN_POINT('Ctrl Pts',(-13.2585918516775,0.202490098329601,
6.72757780801801));
#69835=CARTESIAN_POINT('Ctrl Pts',(-13.1594379717041,-3.03809191952043,
6.0059851637655));
#69836=CARTESIAN_POINT('Ctrl Pts',(-13.0602840917306,-5.53948773721081,
3.8230476755157));
#69837=CARTESIAN_POINT('Ctrl Pts',(-12.9611302117572,-6.69310268371076,
0.70997628534325));
#69838=CARTESIAN_POINT('Ctrl Pts',(-12.8619763317838,-6.2182535012809,-2.57585182092111));
#69839=CARTESIAN_POINT('Ctrl Pts',(-12.7628224518103,-4.23047494773025,
-5.23495485616797));
#69840=CARTESIAN_POINT('Ctrl Pts',(-12.6636685718369,-1.21340187876777,
-6.62037336805498));
#69841=CARTESIAN_POINT('Ctrl Pts',(-12.5645146918634,2.09889734611304,-6.39502205602867));
#69842=CARTESIAN_POINT('Ctrl Pts',(-12.4653608118901,4.90052517743945,-4.61373331740821));
#69843=CARTESIAN_POINT('Ctrl Pts',(-12.3662069319166,6.50983242416413,-1.70990123493954));
#69844=CARTESIAN_POINT('Ctrl Pts',(-12.2670530519432,6.53526722067193,1.60995745550014));
#69845=CARTESIAN_POINT('Ctrl Pts',(-12.1678991719697,4.97064112977619,4.53810617563721));
#69846=CARTESIAN_POINT('Ctrl Pts',(-12.0687452919963,2.19663496534104,6.36211249860841));
#69847=CARTESIAN_POINT('Ctrl Pts',(-11.9695914120228,-1.11182269422578,
6.63818733587228));
#69848=CARTESIAN_POINT('Ctrl Pts',(-11.8704375320494,-4.14976872546465,
5.29916033305668));
#69849=CARTESIAN_POINT('Ctrl Pts',(-11.771283652076,-6.1780567477131,2.67082301374029));
#69850=CARTESIAN_POINT('Ctrl Pts',(-11.6721297721026,-6.7031948609816,-0.607337958652469));
#69851=CARTESIAN_POINT('Ctrl Pts',(-11.5729758921291,-5.59741452326445,
-3.73773078115887));
#69852=CARTESIAN_POINT('Ctrl Pts',(-11.4738220121557,-3.12975722761006,
-5.95871634150508));
#69853=CARTESIAN_POINT('Ctrl Pts',(-11.3746681321822,0.0993845416067408,
-6.72991853232244));
#69854=CARTESIAN_POINT('Ctrl Pts',(-11.2755142522088,3.30434559016186,-5.8637002789636));
#69855=CARTESIAN_POINT('Ctrl Pts',(-11.1763603722353,5.70534400537603,-3.57081650610014));
#69856=CARTESIAN_POINT('Ctrl Pts',(-11.0772064922619,6.71820571835696,-0.409136488209301));
#69857=CARTESIAN_POINT('Ctrl Pts',(-10.9780526122885,6.09649676879898,2.85208833807471));
#69858=CARTESIAN_POINT('Ctrl Pts',(-10.8788987323151,3.9914818324543,5.41938682152096));
#69859=CARTESIAN_POINT('Ctrl Pts',(-10.7797448523416,0.915320822753942,
6.66812331406536));
#69860=CARTESIAN_POINT('Ctrl Pts',(-10.6805909723682,-2.38354199549463,
6.29447442570273));
#69861=CARTESIAN_POINT('Ctrl Pts',(-10.5814370923947,-5.10247797284465,
4.3893506668714));
#69862=CARTESIAN_POINT('Ctrl Pts',(-10.4822832124213,-6.57995735444709,
1.41627749886143));
#69863=CARTESIAN_POINT('Ctrl Pts',(-10.3831293324479,-6.45650254272451,
-1.9013825643242));
#69864=CARTESIAN_POINT('Ctrl Pts',(-10.2839754524745,-4.76215066691193,
-4.75642741621855));
#69865=CARTESIAN_POINT('Ctrl Pts',(-10.184821572501,-1.90914540996877,-6.45421138046464));
#69866=CARTESIAN_POINT('Ctrl Pts',(-10.0856676925276,1.40836379467596,-6.58165573104297));
#69867=CARTESIAN_POINT('Ctrl Pts',(-9.98651381255412,4.38321154513755,-5.10775266538008));
#69868=CARTESIAN_POINT('Ctrl Pts',(-9.8873599325807,6.29160356326141,-2.39110964677092));
#69869=CARTESIAN_POINT('Ctrl Pts',(-9.78820605260725,6.6692192050819,0.907301457450251));
#69870=CARTESIAN_POINT('Ctrl Pts',(-9.68905217263382,5.42418283062754,3.98496190195714));
#69871=CARTESIAN_POINT('Ctrl Pts',(-9.58989829266038,2.85941757395946,6.09306260248953));
#69872=CARTESIAN_POINT('Ctrl Pts',(-9.49074441268695,-0.40105726265788,
6.71869286485055));
#69873=CARTESIAN_POINT('Ctrl Pts',(-9.39159053271352,-3.56395300404956,
5.70963393967168));
#69874=CARTESIAN_POINT('Ctrl Pts',(-9.29243665274007,-5.8597224222394,3.31139455130754));
#69875=CARTESIAN_POINT('Ctrl Pts',(-9.19328277276663,-6.72979415215828,
0.107477484622944));
#69876=CARTESIAN_POINT('Ctrl Pts',(-9.09412889279321,-5.96247569976116,
-3.12258935338642));
#69877=CARTESIAN_POINT('Ctrl Pts',(-8.99497501281976,-3.74445920930363,
-5.5929156948756));
#69878=CARTESIAN_POINT('Ctrl Pts',(-8.89582113284633,-0.61539839731509,
-6.7024596643849));
#69879=CARTESIAN_POINT('Ctrl Pts',(-8.79666725287289,2.66339170374145,-6.18126405944332));
#69880=CARTESIAN_POINT('Ctrl Pts',(-8.69751337289946,5.29416622976448,-4.15613819208962));
#69881=CARTESIAN_POINT('Ctrl Pts',(-8.59835949292603,6.63684551659137,-1.11980459412596));
#69882=CARTESIAN_POINT('Ctrl Pts',(-8.49920561295258,6.36474945595398,2.18898266394648));
#69883=CARTESIAN_POINT('Ctrl Pts',(-8.40005173297916,4.54408028350189,4.9651802703642));
#69884=CARTESIAN_POINT('Ctrl Pts',(-8.30089785300571,1.6178152673084,6.53332644990195));
#69885=CARTESIAN_POINT('Ctrl Pts',(-8.20174397303229,-1.7020717194237,6.51188395182705));
#69886=CARTESIAN_POINT('Ctrl Pts',(-8.10259009305884,-4.60783674938121,
4.90606983553807));
#69887=CARTESIAN_POINT('Ctrl Pts',(-8.00343621308541,-6.39249369125078,
2.10658613577598));
#69888=CARTESIAN_POINT('Ctrl Pts',(-7.90428233311196,-6.62182721996452,
-1.20543975754137));
#69889=CARTESIAN_POINT('Ctrl Pts',(-7.80512845313853,-5.2400394225549,-4.22417655764945));
#69890=CARTESIAN_POINT('Ctrl Pts',(-7.7059745731651,-2.58332568960406,-6.21515157671607));
#69891=CARTESIAN_POINT('Ctrl Pts',(-7.60682069319166,0.701923185172142,
-6.69395134298438));
#69892=CARTESIAN_POINT('Ctrl Pts',(-7.50766681321823,3.81639088802017,-5.54408164892628));
#69893=CARTESIAN_POINT('Ctrl Pts',(-7.40851293324478,6.00231295772723,-3.04531113313967));
#69894=CARTESIAN_POINT('Ctrl Pts',(-7.30935905327136,6.72784439943585,0.194397729164));
#69895=CARTESIAN_POINT('Ctrl Pts',(-7.21020517329791,5.816460042724,3.38680872083436));
#69896=CARTESIAN_POINT('Ctrl Pts',(-7.11105129332449,3.48990393566447,5.75519341638126));
#69897=CARTESIAN_POINT('Ctrl Pts',(-7.01189741335103,0.314237987756349,
6.72331281640052));
#69898=CARTESIAN_POINT('Ctrl Pts',(-6.91274353337763,-2.93788352245125,
6.05561897320447));
#69899=CARTESIAN_POINT('Ctrl Pts',(-6.81358965340416,-5.47520432290657,
3.91456490079675));
#69900=CARTESIAN_POINT('Ctrl Pts',(-6.71443577343075,-6.68038247504238,
0.8210790018453));
#69901=CARTESIAN_POINT('Ctrl Pts',(-6.61528189345729,-6.26019253545994,
-2.47217923280175));
#69902=CARTESIAN_POINT('Ctrl Pts',(-6.51612801348387,-4.31686866856674,
-5.16394477492463));
#69903=CARTESIAN_POINT('Ctrl Pts',(-6.41697413351042,-1.32323059941942,
-6.59929856279322));
#69904=CARTESIAN_POINT('Ctrl Pts',(-6.31782025353699,1.99235562199561,-6.42901235149125));
#69905=CARTESIAN_POINT('Ctrl Pts',(-6.21866637356356,4.8231924645472,-4.69451756733956));
#69906=CARTESIAN_POINT('Ctrl Pts',(-6.11951249359011,6.4805241730172,-1.81782484939125));
#69907=CARTESIAN_POINT('Ctrl Pts',(-6.02035861361669,6.56111424314798,1.50115309961553));
#69908=CARTESIAN_POINT('Ctrl Pts',(-5.92120473364324,5.04535473647355,4.45489352546932));
#69909=CARTESIAN_POINT('Ctrl Pts',(-5.82205085366982,2.30203698284238,6.32473766015244));
#69910=CARTESIAN_POINT('Ctrl Pts',(-5.72289697369637,-1.00137706345556,
6.65574373882511));
#69911=CARTESIAN_POINT('Ctrl Pts',(-5.62374309372295,-4.06115141804426,
5.36737644476719));
#69912=CARTESIAN_POINT('Ctrl Pts',(-5.5245892137495,-6.13282876543525,2.77310152608492));
#69913=CARTESIAN_POINT('Ctrl Pts',(-5.42543533377607,-6.71236038246565,
-0.495881877093973));
#69914=CARTESIAN_POINT('Ctrl Pts',(-5.32628145380263,-5.65874353433961,
-3.64421491582127));
#69915=CARTESIAN_POINT('Ctrl Pts',(-5.22712757382919,-3.2283280950709,-5.90589353533404));
#69916=CARTESIAN_POINT('Ctrl Pts',(-5.12797369385576,-0.0124454321920131,
-6.7306408202594));
#69917=CARTESIAN_POINT('Ctrl Pts',(-5.02881981388232,3.20646526215786,-5.91779192458636));
#69918=CARTESIAN_POINT('Ctrl Pts',(-4.92966593390888,5.64522806171502,-3.66511676094361));
#69919=CARTESIAN_POINT('Ctrl Pts',(-4.83051205393545,6.71048064740892,-0.520701662062845));
#69920=CARTESIAN_POINT('Ctrl Pts',(-4.73135817396201,6.1430421162185,2.75040257025954));
#69921=CARTESIAN_POINT('Ctrl Pts',(-4.63220429398858,4.08097289897303,5.3523210794918));
#69922=CARTESIAN_POINT('Ctrl Pts',(-4.53305041401514,1.02598401613378,6.65199500441502));
#69923=CARTESIAN_POINT('Ctrl Pts',(-4.43389653404171,-2.27863154431964,
6.33320764110542));
#69924=CARTESIAN_POINT('Ctrl Pts',(-4.33474265406827,-5.02884546403524,
4.47352143606987));
#69925=CARTESIAN_POINT('Ctrl Pts',(-4.23558877409483,-6.55551791947666,
1.52540668267351));
#69926=CARTESIAN_POINT('Ctrl Pts',(-4.1364348941214,-6.48720240966135,-1.7938466033105));
#69927=CARTESIAN_POINT('Ctrl Pts',(-4.03728101414796,-4.84052041550572,
-4.67664867690495));
#69928=CARTESIAN_POINT('Ctrl Pts',(-3.93812713417453,-2.01611731629858,
-6.42160040076036));
#69929=CARTESIAN_POINT('Ctrl Pts',(-3.83897325420109,1.29881649238736,-6.60414691381309));
#69930=CARTESIAN_POINT('Ctrl Pts',(-3.73981937422765,4.29774221446888,-5.17987380136782));
#69931=CARTESIAN_POINT('Ctrl Pts',(-3.64066549425422,6.25100728943547,-2.49531332853195));
#69932=CARTESIAN_POINT('Ctrl Pts',(-3.54151161428078,6.68337325012159,0.796368469794977));
#69933=CARTESIAN_POINT('Ctrl Pts',(-3.44235773430735,5.48964344961827,3.89429011967366));
#69934=CARTESIAN_POINT('Ctrl Pts',(-3.34320385433391,2.96025789418556,6.04471289144791));
#69935=CARTESIAN_POINT('Ctrl Pts',(-3.24404997436047,-0.289372159588611,
6.72442893436904));
#69936=CARTESIAN_POINT('Ctrl Pts',(-3.14489609438704,-3.46859662257756,
5.7680601773879));
#69937=CARTESIAN_POINT('Ctrl Pts',(-3.0457422144136,-5.80389541298086,3.40829558215014));
#69938=CARTESIAN_POINT('Ctrl Pts',(-2.94658833444016,-6.72707948582544,
0.219276837607698));
#69939=CARTESIAN_POINT('Ctrl Pts',(-2.84743445446673,-6.01353386728451,
-3.02309298023511));
#69940=CARTESIAN_POINT('Ctrl Pts',(-2.74828057449329,-3.83686752132008,
-5.529930231383));
#69941=CARTESIAN_POINT('Ctrl Pts',(-2.64912669451986,-0.726673482202994,
-6.69130976643494));
#69942=CARTESIAN_POINT('Ctrl Pts',(-2.54997281454642,2.56032359109411,-6.22466254900709));
#69943=CARTESIAN_POINT('Ctrl Pts',(-2.45081893457298,5.22438203999585,-4.24352601503672));
#69944=CARTESIAN_POINT('Ctrl Pts',(-2.35166505459955,6.61732406727365,-1.22991988714937));
#69945=CARTESIAN_POINT('Ctrl Pts',(-2.25251117462611,6.40024040639838,2.08293146320999));
#69946=CARTESIAN_POINT('Ctrl Pts',(-2.15335729465268,4.6259485205824,4.88899591174365));
#69947=CARTESIAN_POINT('Ctrl Pts',(-2.05420341467923,1.72614186860208,6.50554494178492));
#69948=CARTESIAN_POINT('Ctrl Pts',(-1.9550495347058,-1.59364311927237,6.53926466420501));
#69949=CARTESIAN_POINT('Ctrl Pts',(-1.85589565473237,-4.52568733252372,
4.98195091388494));
#69950=CARTESIAN_POINT('Ctrl Pts',(-1.75674177475893,-6.35661079245612,
2.21250536120366));
#69951=CARTESIAN_POINT('Ctrl Pts',(-1.65758789478549,-6.64094131521324,
-1.09525302465609));
#69952=CARTESIAN_POINT('Ctrl Pts',(-1.55843401481206,-5.30949996367323,
-4.13653126132011));
#69953=CARTESIAN_POINT('Ctrl Pts',(-1.45928013483862,-2.68623260424001,
-6.17137222471975));
#69954=CARTESIAN_POINT('Ctrl Pts',(-1.36012625486518,0.590607627431654,
-6.70468965505072));
#69955=CARTESIAN_POINT('Ctrl Pts',(-1.26097237489175,3.72375027952026,-5.60672494384176));
#69956=CARTESIAN_POINT('Ctrl Pts',(-1.16181849491831,5.95088718890311,-3.14461800622483));
#69957=CARTESIAN_POINT('Ctrl Pts',(-1.06266461494488,6.7301455987549,0.0825891014880007));
#69958=CARTESIAN_POINT('Ctrl Pts',(-0.963510734971439,5.87192831770101,
3.28970189711857));
#69959=CARTESIAN_POINT('Ctrl Pts',(-0.864356854998003,3.58504359730451,
5.696414937972));
#69960=CARTESIAN_POINT('Ctrl Pts',(-0.765202975024567,0.425901114385129,
6.71716376016619));
#69961=CARTESIAN_POINT('Ctrl Pts',(-0.666049095051132,-2.83686508830405,
6.10359543309403));
#69962=CARTESIAN_POINT('Ctrl Pts',(-0.566895215077694,-5.40940883557766,
4.0049939812313));
#69963=CARTESIAN_POINT('Ctrl Pts',(-0.46774133510426,-6.66581828226979,
0.93195888744215));
#69964=CARTESIAN_POINT('Ctrl Pts',(-0.368587455130823,-6.30040317300718,
-2.36782613333107));
#69965=CARTESIAN_POINT('Ctrl Pts',(-0.269433575157386,-4.4020707015091,
-5.09150805548215));
#69966=CARTESIAN_POINT('Ctrl Pts',(-0.170279695183953,-1.43269397731273,
-6.57640241374388));
#69967=CARTESIAN_POINT('Ctrl Pts',(-0.0711258152105153,1.88526384753484,
-6.46122751226907));
#69968=CARTESIAN_POINT('Ctrl Pts',(0.0280280647629222,4.74452821976931,
-4.77400593966295));
#69969=CARTESIAN_POINT('Ctrl Pts',(0.127181944736356,6.44942683413289,-1.92524654298902));
#69970=CARTESIAN_POINT('Ctrl Pts',(0.226335824709794,6.58514993717897,1.39193428185253));
#69971=CARTESIAN_POINT('Ctrl Pts',(0.32548970468323,5.11867546739773,4.37045102930867));
#69972=CARTESIAN_POINT('Ctrl Pts',(0.424643584656665,2.4068034761944,6.28561673721068));
#69973=CARTESIAN_POINT('Ctrl Pts',(0.523797464630102,-0.890654982229587,
6.6714626914009));
#69974=CARTESIAN_POINT('Ctrl Pts',(0.622951344603541,-3.97141294569627,
5.43411077867214));
#69975=CARTESIAN_POINT('Ctrl Pts',(0.722105224576973,-6.08590768919204,
2.8746144678474));
#69976=CARTESIAN_POINT('Ctrl Pts',(0.82125910455041,-6.7196728181619,-0.384288897810818));
#69977=CARTESIAN_POINT('Ctrl Pts',(0.920412984523844,-5.71851033239854,
-3.5496929893127));
#69978=CARTESIAN_POINT('Ctrl Pts',(1.01956686449728,-3.32600771586179,-5.85144028544703));
#69979=CARTESIAN_POINT('Ctrl Pts',(1.11872074447072,-0.124271970179066,
-6.7295049756689));
#69980=CARTESIAN_POINT('Ctrl Pts',(1.21787462444415,3.10769972318758,-5.97024984155809));
#69981=CARTESIAN_POINT('Ctrl Pts',(1.31702850441759,5.58355363623528,-3.75840518457078));
#69982=CARTESIAN_POINT('Ctrl Pts',(1.41618238439102,6.70090300966427,-0.632123085480108));
#69983=CARTESIAN_POINT('Ctrl Pts',(1.51533626436446,6.18789154996778,2.64795749700821));
#69984=CARTESIAN_POINT('Ctrl Pts',(1.6144901443379,4.16933732862471,5.28377771866504));
#69985=CARTESIAN_POINT('Ctrl Pts',(1.71364402431134,1.13636396543253,6.63403027413886));
#69986=CARTESIAN_POINT('Ctrl Pts',(1.81279790428477,-2.1730920298384,6.37019244371608));
#69987=CARTESIAN_POINT('Ctrl Pts',(1.91195178425821,-4.9538246385574,4.55645719726919));
#69988=CARTESIAN_POINT('Ctrl Pts',(2.01110566423164,-6.52926869837069,1.63411474646096));
#69989=CARTESIAN_POINT('Ctrl Pts',(2.11025954420508,-6.51611135037028,-1.68581541388737));
#69990=CARTESIAN_POINT('Ctrl Pts',(2.20941342417852,-4.91755383845069,-4.59557885212116));
#69991=CARTESIAN_POINT('Ctrl Pts',(2.30856730415195,-2.12253263179732,-6.38721660561782));
#69992=CARTESIAN_POINT('Ctrl Pts',(2.40772118412539,1.18891062497711,-6.62481488540933));
#69993=CARTESIAN_POINT('Ctrl Pts',(2.50687506409882,4.21108640328576,-5.25056492619473));
#69994=CARTESIAN_POINT('Ctrl Pts',(2.60602894407226,6.20868529592357,-2.59882812750426));
#69995=CARTESIAN_POINT('Ctrl Pts',(2.70518282404569,6.69568221192067,0.685215628173524));
#69996=CARTESIAN_POINT('Ctrl Pts',(2.80433670401913,5.55358853913808,3.8025432381604));
#69997=CARTESIAN_POINT('Ctrl Pts',(2.90349058399257,3.0602809740713,5.99469441255026));
#69998=CARTESIAN_POINT('Ctrl Pts',(3.002644463966,-0.177607169357161,6.72830858637717));
#69999=CARTESIAN_POINT('Ctrl Pts',(3.10179834393944,-3.37228266335948,5.82489402294447));
#70000=CARTESIAN_POINT('Ctrl Pts',(3.20095222391288,-5.74646611850472,3.5042556825936));
#70001=CARTESIAN_POINT('Ctrl Pts',(3.30010610388631,-6.7225076702446,0.331015654692348));
#70002=CARTESIAN_POINT('Ctrl Pts',(3.39925998385975,-6.06293187456192,-2.9227620198211));
#70003=CARTESIAN_POINT('Ctrl Pts',(3.49841386383318,-3.92821658680787,-5.46541811641943));
#70004=CARTESIAN_POINT('Ctrl Pts',(3.59756774380662,-0.837747953852602,
-6.67831259420852));
#70005=CARTESIAN_POINT('Ctrl Pts',(3.69672162378006,2.45654864820692,-6.26634259188805));
#70006=CARTESIAN_POINT('Ctrl Pts',(3.79587550375349,5.15315555169669,-4.32974232498397));
#70007=CARTESIAN_POINT('Ctrl Pts',(3.89502938372693,6.5959757688618,-1.33969563535732));
#70008=CARTESIAN_POINT('Ctrl Pts',(3.99418326370036,6.43396443845587,1.97630522616884));
#70009=CARTESIAN_POINT('Ctrl Pts',(4.09333714367381,4.70653966866234,4.81146184490557));
#70010=CARTESIAN_POINT('Ctrl Pts',(4.19249102364724,1.83399193346608,6.47596744342429));
#70011=CARTESIAN_POINT('Ctrl Pts',(4.29164490362067,-1.48477456235392,6.56484007784463));
#70012=CARTESIAN_POINT('Ctrl Pts',(4.39079878359412,-4.44228850360737,5.05645662109383));
#70013=CARTESIAN_POINT('Ctrl Pts',(4.48995266356754,-6.31897302495677,2.31781378013833));
#70014=CARTESIAN_POINT('Ctrl Pts',(4.58910654354099,-6.6582220317288,-0.984763927095942));
#70015=CARTESIAN_POINT('Ctrl Pts',(4.68826042351442,-5.37749472645081,-4.04774398515678));
#70016=CARTESIAN_POINT('Ctrl Pts',(4.78741430348785,-2.78839789245884,-6.12588914749855));
#70017=CARTESIAN_POINT('Ctrl Pts',(4.88656818346129,0.47912894970609,-6.71357698052983));
#70018=CARTESIAN_POINT('Ctrl Pts',(4.98572206343473,3.63008178950389,-5.66782042238396));
#70019=CARTESIAN_POINT('Ctrl Pts',(5.08487594340816,5.89781828999535,-3.24305667308019));
#70020=CARTESIAN_POINT('Ctrl Pts',(5.18402982338161,6.73058931523177,-0.0292424611966137));
#70021=CARTESIAN_POINT('Ctrl Pts',(5.28318370335503,5.92577453204566,3.19168714394893));
#70022=CARTESIAN_POINT('Ctrl Pts',(5.38233758332848,3.67919545825143,5.63606334151036));
#70023=CARTESIAN_POINT('Ctrl Pts',(5.4814914633019,0.537442933814262,6.70916127048226));
#70024=CARTESIAN_POINT('Ctrl Pts',(5.58064534327535,-2.73505625631732,6.1498849741076));
#70025=CARTESIAN_POINT('Ctrl Pts',(5.67979922324878,-5.34213396108817,4.09432107199899));
#70026=CARTESIAN_POINT('Ctrl Pts',(5.77895310322222,-6.64938674471686,1.04257437242718));
#70027=CARTESIAN_POINT('Ctrl Pts',(5.87810698319565,-6.33892699759613,-2.26280555094068));
#70028=CARTESIAN_POINT('Ctrl Pts',(5.97726086316909,-4.48595536543181,-5.01769258559197));
#70029=CARTESIAN_POINT('Ctrl Pts',(6.07641474314252,-1.54196255579125,-6.55163727717598));
#70030=CARTESIAN_POINT('Ctrl Pts',(6.17556862311597,1.77806974132202,-6.49177618318107));
#70031=CARTESIAN_POINT('Ctrl Pts',(6.24167120976492,3.70166348963895,-5.39847115416216));
#70032=CARTESIAN_POINT('Ctrl Pts',(6.2747225030894,4.47501996998105,-4.65501854232418));
#70033=CARTESIAN_POINT('Ctrl Pts',(-13.617,3.61104546693871,-5.06353840690493));
#70034=CARTESIAN_POINT('Ctrl Pts',(-13.5839487066755,4.45227095397745,-4.46362126645189));
#70035=CARTESIAN_POINT('Ctrl Pts',(-13.5178461200266,5.82912718297219,-2.83706456600194));
#70036=CARTESIAN_POINT('Ctrl Pts',(-13.4186922400531,6.47593427309586,0.295071888562534));
#70037=CARTESIAN_POINT('Ctrl Pts',(-13.3195383600797,5.54718661553207,3.35454744289073));
#70038=CARTESIAN_POINT('Ctrl Pts',(-13.2203844801062,3.26875126278153,5.59827586641925));
#70039=CARTESIAN_POINT('Ctrl Pts',(-13.1212306001328,0.195029276623322,
6.47969774398204));
#70040=CARTESIAN_POINT('Ctrl Pts',(-13.0220767201594,-2.92615231197546,
5.78469244453168));
#70041=CARTESIAN_POINT('Ctrl Pts',(-12.9229228401859,-5.33538328621662,
3.6821860861499));
#70042=CARTESIAN_POINT('Ctrl Pts',(-12.8237689602125,-6.44649286823449,
0.683816949532182));
#70043=CARTESIAN_POINT('Ctrl Pts',(-12.7246150802391,-5.98913967754298,
-2.48094361881069));
#70044=CARTESIAN_POINT('Ctrl Pts',(-12.6254612002656,-4.07460155155841,
-5.04207103051742));
#70045=CARTESIAN_POINT('Ctrl Pts',(-12.5263073202922,-1.16869364290732,
-6.37644329080494));
#70046=CARTESIAN_POINT('Ctrl Pts',(-12.4271534403188,2.02156270600836,-6.15939513026191));
#70047=CARTESIAN_POINT('Ctrl Pts',(-12.3279995603453,4.71996353557397,-4.4437386264808));
#70048=CARTESIAN_POINT('Ctrl Pts',(-12.2288456803719,6.26997526840712,-1.6468992987736));
#70049=CARTESIAN_POINT('Ctrl Pts',(-12.1296918003985,6.29447291053824,1.55063798442858));
#70050=CARTESIAN_POINT('Ctrl Pts',(-12.030537920425,4.78749604001144,4.37089799439875));
#70051=CARTESIAN_POINT('Ctrl Pts',(-11.9313840404516,2.11569914692158,6.12769813751704));
#70052=CARTESIAN_POINT('Ctrl Pts',(-11.8322301604782,-1.07085718055863,
6.39360089646495));
#70053=CARTESIAN_POINT('Ctrl Pts',(-11.7330762805047,-3.99686897955958,
5.10391083313569));
#70054=CARTESIAN_POINT('Ctrl Pts',(-11.6339224005313,-5.9504239880569,2.57241556330756));
#70055=CARTESIAN_POINT('Ctrl Pts',(-11.5347685205579,-6.45621319554393,
-0.584960369514416));
#70056=CARTESIAN_POINT('Ctrl Pts',(-11.4356146405844,-5.39117573865922,
-3.60001272395876));
#70057=CARTESIAN_POINT('Ctrl Pts',(-11.336460760611,-3.01444017827433,-5.73916525930964));
#70058=CARTESIAN_POINT('Ctrl Pts',(-11.2373068806375,0.0957226818348403,
-6.48195222344366));
#70059=CARTESIAN_POINT('Ctrl Pts',(-11.1381530006641,3.18259576877592,-5.64765009833173));
#70060=CARTESIAN_POINT('Ctrl Pts',(-11.0389991206906,5.49512851954185,-3.43924846639081));
#70061=CARTESIAN_POINT('Ctrl Pts',(-10.9398452407172,6.47067097239111,-0.394061704715005));
#70062=CARTESIAN_POINT('Ctrl Pts',(-10.8406913607438,5.87186911638537,2.7470021004937));
#70063=CARTESIAN_POINT('Ctrl Pts',(-10.7415374807704,3.84441422499412,5.219707532676));
#70064=CARTESIAN_POINT('Ctrl Pts',(-10.6423836007969,0.881595492385054,
6.42243387259649));
#70065=CARTESIAN_POINT('Ctrl Pts',(-10.5432297208235,-2.29571951921329,
6.062552214137));
#70066=CARTESIAN_POINT('Ctrl Pts',(-10.44407584085,-4.9144753063956,4.22762343674055));
#70067=CARTESIAN_POINT('Ctrl Pts',(-10.3449219608766,-6.33751641999512,
1.36409423660437));
#70068=CARTESIAN_POINT('Ctrl Pts',(-10.2457680809032,-6.21861034594731,
-1.83132542856878));
#70069=CARTESIAN_POINT('Ctrl Pts',(-10.1466142009297,-4.58668748447852,
-4.58117510904947));
#70070=CARTESIAN_POINT('Ctrl Pts',(-10.0474603209563,-1.83880224932734,
-6.21640360239859));
#70071=CARTESIAN_POINT('Ctrl Pts',(-9.94830644098286,1.35647211574301,-6.33915221928435));
#70072=CARTESIAN_POINT('Ctrl Pts',(-9.84915256100943,4.22171051319157,-4.91955565095604));
#70073=CARTESIAN_POINT('Ctrl Pts',(-9.749998681036,6.05978712967198,-2.30300833761142));
#70074=CARTESIAN_POINT('Ctrl Pts',(-9.65084480106255,6.42348938510785,0.873871603528));
#70075=CARTESIAN_POINT('Ctrl Pts',(-9.55169092108912,5.22432683107353,3.83813452371996));
#70076=CARTESIAN_POINT('Ctrl Pts',(-9.45253704111568,2.75406128800256,5.86856148318917));
#70077=CARTESIAN_POINT('Ctrl Pts',(-9.35338316114225,-0.386280161182942,
6.47114016979406));
#70078=CARTESIAN_POINT('Ctrl Pts',(-9.25422928116881,-3.43263785258272,
5.49926038963988));
#70079=CARTESIAN_POINT('Ctrl Pts',(-9.15507540119538,-5.6438188071929,3.18938500837096));
#70080=CARTESIAN_POINT('Ctrl Pts',(-9.05592152122194,-6.48183242611213,
0.103517437406672));
#70081=CARTESIAN_POINT('Ctrl Pts',(-8.95676764124851,-5.74278610263628,
-3.00753640699718));
#70082=CARTESIAN_POINT('Ctrl Pts',(-8.85761376127506,-3.60649324070849,
-5.38684267124721));
#70083=CARTESIAN_POINT('Ctrl Pts',(-8.75845988130164,-0.592723818367459,
-6.45550508753466));
#70084=CARTESIAN_POINT('Ctrl Pts',(-8.65930600132819,2.56525806264267,-5.95351312521376));
#70085=CARTESIAN_POINT('Ctrl Pts',(-8.56015212135476,5.09910073940523,-4.00300376085795));
#70086=CARTESIAN_POINT('Ctrl Pts',(-8.46099824138133,6.39230851700605,-1.07854498443864));
#70087=CARTESIAN_POINT('Ctrl Pts',(-8.36184436140788,6.13023793520507,2.10832879736973));
#70088=CARTESIAN_POINT('Ctrl Pts',(-8.26269048143445,4.37665198407491,4.78223638796107));
#70089=CARTESIAN_POINT('Ctrl Pts',(-8.16353660146101,1.55820627228779,6.29260364817686));
#70090=CARTESIAN_POINT('Ctrl Pts',(-8.06438272148758,-1.63935826461956,
6.27195120678321));
#70091=CARTESIAN_POINT('Ctrl Pts',(-7.96522884151414,-4.43805931965865,
4.72530389871772));
#70092=CARTESIAN_POINT('Ctrl Pts',(-7.86607496154071,-6.15695992400869,
2.028968199405));
#70093=CARTESIAN_POINT('Ctrl Pts',(-7.76692108156727,-6.37784357500933,
-1.16102488894861));
#70094=CARTESIAN_POINT('Ctrl Pts',(-7.66776720159383,-5.0469682541968,-4.06853522796294));
#70095=CARTESIAN_POINT('Ctrl Pts',(-7.5686133216204,-2.48814211006943,-5.98615204452285));
#70096=CARTESIAN_POINT('Ctrl Pts',(-7.46945944164697,0.676060568781244,
-6.44731025834689));
#70097=CARTESIAN_POINT('Ctrl Pts',(-7.37030556167352,3.6757745704235,-5.3398079335753));
#70098=CARTESIAN_POINT('Ctrl Pts',(-7.2711516817001,5.78115554226751,-2.93310553102942));
#70099=CARTESIAN_POINT('Ctrl Pts',(-7.17199780172665,6.47995451274163,0.187235073758361));
#70100=CARTESIAN_POINT('Ctrl Pts',(-7.07284392175322,5.60215044586807,3.26202051524908));
#70101=CARTESIAN_POINT('Ctrl Pts',(-6.97369004177978,3.36131714919565,5.54314121077292));
#70102=CARTESIAN_POINT('Ctrl Pts',(-6.87453616180634,0.302659774207504,
6.47558989754003));
#70103=CARTESIAN_POINT('Ctrl Pts',(-6.77538228183291,-2.82963612993394,
5.83249747811505));
#70104=CARTESIAN_POINT('Ctrl Pts',(-6.67622840185946,-5.27346841781536,
3.77033132580544));
#70105=CARTESIAN_POINT('Ctrl Pts',(-6.57707452188605,-6.4342413403052,0.79082604582396));
#70106=CARTESIAN_POINT('Ctrl Pts',(-6.47792064191259,-6.02953345267415,
-2.38109088510478));
#70107=CARTESIAN_POINT('Ctrl Pts',(-6.37876676193917,-4.1578120641639,-4.97367734167979));
#70108=CARTESIAN_POINT('Ctrl Pts',(-6.27961288196573,-1.27447568419159,
-6.3561449944483));
#70109=CARTESIAN_POINT('Ctrl Pts',(-6.18045900199229,1.91894655066922,-6.19213304086084));
#70110=CARTESIAN_POINT('Ctrl Pts',(-6.08130512201886,4.64548017476219,-4.52154635118754));
#70111=CARTESIAN_POINT('Ctrl Pts',(-5.98215124204542,6.24174689048921,-1.75084642819241));
#70112=CARTESIAN_POINT('Ctrl Pts',(-5.88299736207198,6.31936759002112,1.44584256481697));
#70113=CARTESIAN_POINT('Ctrl Pts',(-5.78384348209855,4.85945679655365,4.29075134475004));
#70114=CARTESIAN_POINT('Ctrl Pts',(-5.68468960212512,2.21721758855159,6.09170038864876));
#70115=CARTESIAN_POINT('Ctrl Pts',(-5.58553572215167,-0.964480959434654,
6.41051042733211));
#70116=CARTESIAN_POINT('Ctrl Pts',(-5.48638184217824,-3.91151680923086,
5.16961349726944));
#70117=CARTESIAN_POINT('Ctrl Pts',(-5.38722796220481,-5.90686244732208,
2.67092558647035));
#70118=CARTESIAN_POINT('Ctrl Pts',(-5.28807408223136,-6.46504101003786,
-0.477610928030889));
#70119=CARTESIAN_POINT('Ctrl Pts',(-5.18892020225794,-5.45024505989854,
-3.50994248487028));
#70120=CARTESIAN_POINT('Ctrl Pts',(-5.08976632228449,-3.10937916608465,
-5.68828872874475));
#70121=CARTESIAN_POINT('Ctrl Pts',(-4.99061244231106,-0.0119868756926444,
-6.48264789841751));
#70122=CARTESIAN_POINT('Ctrl Pts',(-4.89145856233762,3.08832187724368,-5.69974871749482));
#70123=CARTESIAN_POINT('Ctrl Pts',(-4.79230468236419,5.43722756980429,-3.53007419386704));
#70124=CARTESIAN_POINT('Ctrl Pts',(-4.69315080239075,6.46323053450655,-0.501516218948075));
#70125=CARTESIAN_POINT('Ctrl Pts',(-4.59399692241732,5.91669948346157,2.64906298197146));
#70126=CARTESIAN_POINT('Ctrl Pts',(-4.49484304244388,3.93060796044775,5.15511285243209));
#70127=CARTESIAN_POINT('Ctrl Pts',(-4.39568916247044,0.988181259944745,
6.40689981641197));
#70128=CARTESIAN_POINT('Ctrl Pts',(-4.29653528249701,-2.19467453196863,
6.09985829005677));
#70129=CARTESIAN_POINT('Ctrl Pts',(-4.19738140252357,-4.84355581429439,
4.30869290317386));
#70130=CARTESIAN_POINT('Ctrl Pts',(-4.09822752255014,-6.31397746494157,
1.46920251573968));
#70131=CARTESIAN_POINT('Ctrl Pts',(-3.9990736425767,-6.24817906506253,-1.72775166935533));
#70132=CARTESIAN_POINT('Ctrl Pts',(-3.89991976260326,-4.66216967103227,
-4.50433584655415));
#70133=CARTESIAN_POINT('Ctrl Pts',(-3.80076588262983,-1.94183273665795,
-6.18499418616455));
#70134=CARTESIAN_POINT('Ctrl Pts',(-3.70161200265638,1.25096112385931,-6.36081470620222));
#70135=CARTESIAN_POINT('Ctrl Pts',(-3.60245812268296,4.13939033126021,-4.98901945731978));
#70136=CARTESIAN_POINT('Ctrl Pts',(-3.50330424270952,6.02068664039774,-2.40337259661961));
#70137=CARTESIAN_POINT('Ctrl Pts',(-3.40415036273608,6.43712191918314,0.767025982361597));
#70138=CARTESIAN_POINT('Ctrl Pts',(-3.30499648276265,5.28737552962418,3.75080357640562));
#70139=CARTESIAN_POINT('Ctrl Pts',(-3.20584260278921,2.85118610976127,5.82199323492824));
#70140=CARTESIAN_POINT('Ctrl Pts',(-3.10668872281577,-0.278710136569954,
6.47666489173394));
#70141=CARTESIAN_POINT('Ctrl Pts',(-3.00753484284234,-3.34079491184971,
5.55553389126599));
#70142=CARTESIAN_POINT('Ctrl Pts',(-2.9083809628689,-5.59004876450166,3.28271568530374));
#70143=CARTESIAN_POINT('Ctrl Pts',(-2.80922708289547,-6.47921778265285,
0.211197502355245));
#70144=CARTESIAN_POINT('Ctrl Pts',(-2.71007320292203,-5.79196301330962,
-2.91170601409193));
#70145=CARTESIAN_POINT('Ctrl Pts',(-2.61091932294859,-3.69549673468289,
-5.3261779301854));
#70146=CARTESIAN_POINT('Ctrl Pts',(-2.51176544297515,-0.699898932068888,
-6.4447660116512));
#70147=CARTESIAN_POINT('Ctrl Pts',(-2.41261156300172,2.46598753228901,-5.99531258156246));
#70148=CARTESIAN_POINT('Ctrl Pts',(-2.31345768302828,5.03188777362273,-4.0871717475183));
#70149=CARTESIAN_POINT('Ctrl Pts',(-2.21430380305485,6.37350634262576,-1.18460303923088));
#70150=CARTESIAN_POINT('Ctrl Pts',(-2.11514992308141,6.16442120860435,2.00618509189823));
#70151=CARTESIAN_POINT('Ctrl Pts',(-2.01599604310798,4.45550375602798,4.708859069888));
#70152=CARTESIAN_POINT('Ctrl Pts',(-1.91684216313454,1.66254154035103,6.26584575988373));
#70153=CARTESIAN_POINT('Ctrl Pts',(-1.8176882831611,-1.53492475588388,6.29832306680283));
#70154=CARTESIAN_POINT('Ctrl Pts',(-1.71853440318767,-4.35893672810028,
4.79838911098967));
#70155=CARTESIAN_POINT('Ctrl Pts',(-1.61938052321423,-6.12239914373944,
2.1309847922462));
#70156=CARTESIAN_POINT('Ctrl Pts',(-1.5202266432408,-6.3962534044302,-1.05489802652235));
#70157=CARTESIAN_POINT('Ctrl Pts',(-1.42107276326736,-5.11386949628186,
-3.98411925462125));
#70158=CARTESIAN_POINT('Ctrl Pts',(-1.32191888329392,-2.58725738181136,
-5.9439857587572));
#70159=CARTESIAN_POINT('Ctrl Pts',(-1.22276500332049,0.568846473464286,
-6.45765291337906));
#70160=CARTESIAN_POINT('Ctrl Pts',(-1.12361112334705,3.58654733901449,-5.40014311338634));
#70161=CARTESIAN_POINT('Ctrl Pts',(-1.02445724337361,5.73162457469774,-3.02875340606772));
#70162=CARTESIAN_POINT('Ctrl Pts',(-0.925303363400179,6.4821709235304,0.0795460758479203));
#70163=CARTESIAN_POINT('Ctrl Pts',(-0.826149483426742,5.65557497197356,
3.16849162795677));
#70164=CARTESIAN_POINT('Ctrl Pts',(-0.726995603453303,3.45295135521813,
5.4865284468909));
#70165=CARTESIAN_POINT('Ctrl Pts',(-0.627841723479869,0.410208632109992,
6.46966740553085));
#70166=CARTESIAN_POINT('Ctrl Pts',(-0.528687843506432,-2.73233975692668,
5.87870622779908));
#70167=CARTESIAN_POINT('Ctrl Pts',(-0.429533963532995,-5.21009718927287,
3.85742851370921));
#70168=CARTESIAN_POINT('Ctrl Pts',(-0.330380083559561,-6.42021377054019,
0.897620521496703));
#70169=CARTESIAN_POINT('Ctrl Pts',(-0.231226203586124,-6.06826251457938,
-2.28058271373709));
#70170=CARTESIAN_POINT('Ctrl Pts',(-0.132072323612687,-4.2398747970514,
-4.9039095796491));
#70171=CARTESIAN_POINT('Ctrl Pts',(-0.0329184436392546,-1.37990584390503,
-6.33409246238185));
#70172=CARTESIAN_POINT('Ctrl Pts',(0.0662354363341833,1.81580061179276,
-6.22316122226147));
#70173=CARTESIAN_POINT('Ctrl Pts',(0.165389316307621,4.56971434284393,-4.59810594537058));
#70174=CARTESIAN_POINT('Ctrl Pts',(0.264543196281055,6.21179534442574,-1.85431013021464));
#70175=CARTESIAN_POINT('Ctrl Pts',(0.363697076254493,6.34251768011774,1.34064795432643));
#70176=CARTESIAN_POINT('Ctrl Pts',(0.462850956227929,4.93007599833982,4.20942016323384));
#70177=CARTESIAN_POINT('Ctrl Pts',(0.562004836201364,2.31812392215191,6.05402089041596));
#70178=CARTESIAN_POINT('Ctrl Pts',(0.6611587161748,-0.857838473773044,6.42565020935318));
#70179=CARTESIAN_POINT('Ctrl Pts',(0.76031259614824,-3.82508478370621,5.23388898024262));
#70180=CARTESIAN_POINT('Ctrl Pts',(0.859466476121671,-5.86167019528809,
2.768698246779));
#70181=CARTESIAN_POINT('Ctrl Pts',(0.95862035609511,-6.47208401636734,-0.37012963286943));
#70182=CARTESIAN_POINT('Ctrl Pts',(1.05777423606854,-5.50780972843139,-3.4189032533025));
#70183=CARTESIAN_POINT('Ctrl Pts',(1.15692811604198,-3.20345974553442,-5.63584182875872));
#70184=CARTESIAN_POINT('Ctrl Pts',(1.25608199601542,-0.119693124002174,
-6.48155390443623));
#70185=CARTESIAN_POINT('Ctrl Pts',(1.35523587598885,2.99319539066687,-5.75027380333636));
#70186=CARTESIAN_POINT('Ctrl Pts',(1.45438975596229,5.3778255610804,-3.61992537141806));
#70187=CARTESIAN_POINT('Ctrl Pts',(1.55354363593573,6.45400578832633,-0.608832279282255));
#70188=CARTESIAN_POINT('Ctrl Pts',(1.65269751590916,5.95989642342674,2.55039253489949));
#70189=CARTESIAN_POINT('Ctrl Pts',(1.7518513958826,4.01571657038161,5.08909499679543));
#70190=CARTESIAN_POINT('Ctrl Pts',(1.85100527585604,1.09449421965509,6.38959700319101));
#70191=CARTESIAN_POINT('Ctrl Pts',(1.95015915582947,-2.09302365948521,6.13548037409304));
#70192=CARTESIAN_POINT('Ctrl Pts',(2.04931303580291,-4.77129915855997,4.38857286592929));
#70193=CARTESIAN_POINT('Ctrl Pts',(2.14846691577634,-6.28869540598436,1.57390519117164));
#70194=CARTESIAN_POINT('Ctrl Pts',(2.24762079574978,-6.27602284528152,-1.62370092860426));
#70195=CARTESIAN_POINT('Ctrl Pts',(2.34677467572321,-4.7363647693443,-4.42625306910482));
#70196=CARTESIAN_POINT('Ctrl Pts',(2.44592855569665,-2.04432714095016,-6.15187727452525));
#70197=CARTESIAN_POINT('Ctrl Pts',(2.54508243567009,1.14510477831697,-6.38072115882848));
#70198=CARTESIAN_POINT('Ctrl Pts',(2.64423631564352,4.05592738512275,-5.05710594180675));
#70199=CARTESIAN_POINT('Ctrl Pts',(2.74339019561696,5.97992401621031,-2.50307335497727));
#70200=CARTESIAN_POINT('Ctrl Pts',(2.84254407559039,6.44897735278439,0.659968607828769));
#70201=CARTESIAN_POINT('Ctrl Pts',(2.94169795556383,5.3489645389414,3.6624371422857));
#70202=CARTESIAN_POINT('Ctrl Pts',(3.04085183553727,2.94752380269873,5.77381770517306));
#70203=CARTESIAN_POINT('Ctrl Pts',(3.1400057155107,-0.171063168266469,6.48040159654536));
#70204=CARTESIAN_POINT('Ctrl Pts',(3.23915959548414,-3.2480296756728,5.61027367300375));
#70205=CARTESIAN_POINT('Ctrl Pts',(3.33831347545758,-5.53473547337747,3.37514010076197));
#70206=CARTESIAN_POINT('Ctrl Pts',(3.43746735543101,-6.47481441728861,0.318819261871086));
#70207=CARTESIAN_POINT('Ctrl Pts',(3.53662123540445,-5.83954093294827,-2.81507178459683));
#70208=CARTESIAN_POINT('Ctrl Pts',(3.63577511537788,-3.78348001045424,-5.26404278768421));
#70209=CARTESIAN_POINT('Ctrl Pts',(3.73492899535132,-0.806880824200139,
-6.43224772498744));
#70210=CARTESIAN_POINT('Ctrl Pts',(3.83408287532476,2.36603621511411,-6.03545690802462));
#70211=CARTESIAN_POINT('Ctrl Pts',(3.93323675529819,4.96328565132639,-4.17021138600364));
#70212=CARTESIAN_POINT('Ctrl Pts',(4.03239063527163,6.35294463007415,-1.29033405986049));
#70213=CARTESIAN_POINT('Ctrl Pts',(4.13154451524507,6.1969026663707,1.90348753754495));
#70214=CARTESIAN_POINT('Ctrl Pts',(4.2306983952185,4.53312549379163,4.63418177409014));
#70215=CARTESIAN_POINT('Ctrl Pts',(4.32985227519194,1.76641783014358,6.23735805526417));
#70216=CARTESIAN_POINT('Ctrl Pts',(4.42900615516537,-1.430067500749,6.32295614497614));
#70217=CARTESIAN_POINT('Ctrl Pts',(4.52816003513881,-4.27861075952717,4.87014962817609));
#70218=CARTESIAN_POINT('Ctrl Pts',(4.62731391511224,-6.08614815354451,2.23241308398294));
#70219=CARTESIAN_POINT('Ctrl Pts',(4.72646779508569,-6.41289740662767,-0.948479940158207));
#70220=CARTESIAN_POINT('Ctrl Pts',(4.82562167505912,-5.17935896716503,-3.89860337811007));
#70221=CARTESIAN_POINT('Ctrl Pts',(4.92477555503255,-2.68565835263266,-5.90017852214549));
#70222=CARTESIAN_POINT('Ctrl Pts',(5.02392943500599,0.461475268377732,-6.46621278210156));
#70223=CARTESIAN_POINT('Ctrl Pts',(5.12308331497942,3.49633009875934,-5.45898750668426));
#70224=CARTESIAN_POINT('Ctrl Pts',(5.22223719495286,5.68051101877298,-3.1235650642522));
#70225=CARTESIAN_POINT('Ctrl Pts',(5.3213910749263,6.48259829111145,-0.0281650120223385));
#70226=CARTESIAN_POINT('Ctrl Pts',(5.42054495489973,5.70743720286374,3.07408826420326));
#70227=CARTESIAN_POINT('Ctrl Pts',(5.51969883487318,3.54363415642518,5.42840052706632));
#70228=CARTESIAN_POINT('Ctrl Pts',(5.6188527148466,0.51764065242096,6.46195977050514));
#70229=CARTESIAN_POINT('Ctrl Pts',(5.71800659482005,-2.63428210857727,5.92329021374989));
#70230=CARTESIAN_POINT('Ctrl Pts',(5.81716047479348,-5.14530108213061,3.94346431515829));
#70231=CARTESIAN_POINT('Ctrl Pts',(5.91631435476693,-6.40438765899599,1.00416033849484));
#70232=CARTESIAN_POINT('Ctrl Pts',(6.01546823474035,-6.1053669147665,-2.17943165310192));
#70233=CARTESIAN_POINT('Ctrl Pts',(6.11462211471379,-4.32066869986243,-4.83281386773501));
#70234=CARTESIAN_POINT('Ctrl Pts',(6.21377599468721,-1.48514838165934,-6.31023980632529));
#70235=CARTESIAN_POINT('Ctrl Pts',(6.31292987466067,1.71255611161507,-6.25258431622468));
#70236=CARTESIAN_POINT('Ctrl Pts',(6.37903246130962,3.56527434498162,-5.19956251072807));
#70237=CARTESIAN_POINT('Ctrl Pts',(6.4120837546341,4.31013622305522,-4.48350268219026));
#70238=CARTESIAN_POINT('',(6.,4.80478746383271,-4.99805026259201));
#70239=CARTESIAN_POINT('Ctrl Pts',(6.,-6.00216240205939,-1.62981090527766));
#70240=CARTESIAN_POINT('Ctrl Pts',(6.,-5.96859682269621,-1.78822123507159));
#70241=CARTESIAN_POINT('Ctrl Pts',(6.,-5.92885555292031,-1.945098465166));
#70242=CARTESIAN_POINT('Ctrl Pts',(6.,-5.88298849091183,-2.10007140217548));
#70243=CARTESIAN_POINT('Ctrl Pts',(6.,-5.83372654272929,-2.26651478133168));
#70244=CARTESIAN_POINT('Ctrl Pts',(6.,-5.7773991931668,-2.43076229796916));
#70245=CARTESIAN_POINT('Ctrl Pts',(5.99999999999999,-5.71430111965253,-2.59245179083645));
#70246=CARTESIAN_POINT('Ctrl Pts',(5.99999999999999,-5.67435241911292,-2.69482076616652));
#70247=CARTESIAN_POINT('Ctrl Pts',(5.99999999999999,-5.63168865089157,-2.79616427521172));
#70248=CARTESIAN_POINT('Ctrl Pts',(5.99999999999999,-5.58637415866202,-2.89638792850598));
#70249=CARTESIAN_POINT('Ctrl Pts',(5.99999999999999,-5.55452143940101,-2.96683770593091));
#70250=CARTESIAN_POINT('Ctrl Pts',(5.99999999999999,-5.52135881807792,-3.03673411555926));
#70251=CARTESIAN_POINT('Ctrl Pts',(5.99999999999999,-5.48690640354643,-3.10604349782801));
#70252=CARTESIAN_POINT('Ctrl Pts',(5.99999999999999,-5.47044569052808,-3.13915821174632));
#70253=CARTESIAN_POINT('Ctrl Pts',(5.99999999999999,-5.45368794282186,-3.17214368538622));
#70254=CARTESIAN_POINT('Ctrl Pts',(5.99999999999999,-5.43665014407369,-3.20496799833295));
#70255=CARTESIAN_POINT('Ctrl Pts',(5.99999999999999,-5.35517751507704,-3.36192976964539));
#70256=CARTESIAN_POINT('Ctrl Pts',(5.99999999999999,-5.26725451919283,-3.51531432515741));
#70257=CARTESIAN_POINT('Ctrl Pts',(5.99999999999999,-5.17318806361391,-3.66474910658035));
#70258=CARTESIAN_POINT('Ctrl Pts',(5.99999999999999,-5.0788139147758,-3.81467269216468));
#70259=CARTESIAN_POINT('Ctrl Pts',(5.99999999999999,-4.9782557256485,-3.96062128997224));
#70260=CARTESIAN_POINT('Ctrl Pts',(5.99999999999999,-4.87177383449923,-4.10220114978652));
#70261=CARTESIAN_POINT('Ctrl Pts',(5.99999999999999,-4.78110005633049,-4.22276231435077));
#70262=CARTESIAN_POINT('Ctrl Pts',(6.,-4.68612992217677,-4.34015554248365));
#70263=CARTESIAN_POINT('Ctrl Pts',(6.,-4.58699864840819,-4.45412220713425));
#70264=CARTESIAN_POINT('Ctrl Pts',(6.,-4.57093126098927,-4.47259414322636));
#70265=CARTESIAN_POINT('Ctrl Pts',(6.,-4.55475451123802,-4.49097602501803));
#70266=CARTESIAN_POINT('Ctrl Pts',(6.,-4.53846892138093,-4.50926670696808));
#70267=CARTESIAN_POINT('Ctrl Pts',(6.,-4.52235362822714,-4.52736612517732));
#70268=CARTESIAN_POINT('Ctrl Pts',(6.,-4.50613731235933,-4.54536998089995));
#70269=CARTESIAN_POINT('Ctrl Pts',(6.,-4.4898234190663,-4.56327440675413));
#70270=CARTESIAN_POINT('Ctrl Pts',(6.,-4.42090782396902,-4.6389089680727));
#70271=CARTESIAN_POINT('Ctrl Pts',(5.99999999999999,-4.3502361725157,-4.7127864089364));
#70272=CARTESIAN_POINT('Ctrl Pts',(5.99999999999999,-4.27786563021268,-4.7848380789645));
#70273=CARTESIAN_POINT('Ctrl Pts',(5.99999999999999,-4.15309584140503,-4.90905811886697));
#70274=CARTESIAN_POINT('Ctrl Pts',(6.,-4.02327896890847,-5.0278531787929));
#70275=CARTESIAN_POINT('Ctrl Pts',(6.,-3.88886714141271,-5.14107396648211));
#70276=CARTESIAN_POINT('Ctrl Pts',(6.,-3.7527080452692,-5.25576655271977));
#70277=CARTESIAN_POINT('Ctrl Pts',(6.,-3.61183326584496,-5.36473945133278));
#70278=CARTESIAN_POINT('Ctrl Pts',(6.,-3.46666982118827,-5.46780534772134));
#70279=CARTESIAN_POINT('Ctrl Pts',(6.,-3.3185456493242,-5.57297335738167));
#70280=CARTESIAN_POINT('Ctrl Pts',(6.,-3.16595557716371,-5.67199151916148));
#70281=CARTESIAN_POINT('Ctrl Pts',(6.,-3.00931638963617,-5.76461974490931));
#70282=CARTESIAN_POINT('Ctrl Pts',(6.,-2.89183699899052,-5.83409091422019));
#70283=CARTESIAN_POINT('Ctrl Pts',(5.99999999999999,-2.77207915436557,-5.89996693969506));
#70284=CARTESIAN_POINT('Ctrl Pts',(5.99999999999999,-2.65020825097159,-5.96212891564935));
#70285=CARTESIAN_POINT('Ctrl Pts',(5.99999999999999,-2.61706538543952,-5.9790339024254));
#70286=CARTESIAN_POINT('Ctrl Pts',(5.99999999999999,-2.58376620188423,-5.99566411633581));
#70287=CARTESIAN_POINT('Ctrl Pts',(5.99999999999999,-2.55031393882262,-6.01201695390139));
#70288=CARTESIAN_POINT('Ctrl Pts',(5.99999999999999,-2.53181089617986,-6.02106199968047));
#70289=CARTESIAN_POINT('Ctrl Pts',(5.99999999999999,-2.51326444296905,-6.03002048154811));
#70290=CARTESIAN_POINT('Ctrl Pts',(5.99999999999999,-2.49468259592518,-6.03888858495449));
#70291=CARTESIAN_POINT('Ctrl Pts',(5.99999999999999,-2.33019094700295,-6.11739148882));
#70292=CARTESIAN_POINT('Ctrl Pts',(5.99999999999999,-2.16275731640371,-6.18889923399487));
#70293=CARTESIAN_POINT('Ctrl Pts',(5.99999999999999,-1.99283559035297,-6.25323756185287));
#70294=CARTESIAN_POINT('Ctrl Pts',(5.99999999999999,-1.83382494091869,-6.31344457324564));
#70295=CARTESIAN_POINT('Ctrl Pts',(5.99999999999999,-1.6726346722028,-6.3673732853798));
#70296=CARTESIAN_POINT('Ctrl Pts',(5.99999999999999,-1.50961068395816,-6.4148488107241));
#70297=CARTESIAN_POINT('Ctrl Pts',(5.99999999999999,-1.33618843229499,-6.46535249789769));
#70298=CARTESIAN_POINT('Ctrl Pts',(6.,-1.16069077253835,-6.50855444745417));
#70299=CARTESIAN_POINT('Ctrl Pts',(6.,-0.983584177924514,-6.54449336584105));
#70300=CARTESIAN_POINT('Ctrl Pts',(6.,-0.805527961020956,-6.58062498398619));
#70301=CARTESIAN_POINT('Ctrl Pts',(5.99999999999999,-0.625844808076049,
-6.60941559586448));
#70302=CARTESIAN_POINT('Ctrl Pts',(5.99999999999999,-0.444994705161226,
-6.63085379932921));
#70303=CARTESIAN_POINT('Ctrl Pts',(5.99999999999999,-0.352078520882111,
-6.64186820314562));
#70304=CARTESIAN_POINT('Ctrl Pts',(6.,-0.25885414203866,-6.65094100308522));
#70305=CARTESIAN_POINT('Ctrl Pts',(6.,-0.165383456909019,-6.65806532413613));
#70306=CARTESIAN_POINT('Ctrl Pts',(6.,-0.138106596290388,-6.66014436220072));
#70307=CARTESIAN_POINT('Ctrl Pts',(5.99999999999999,-0.110808760073336,
-6.66205744319297));
#70308=CARTESIAN_POINT('Ctrl Pts',(5.99999999999999,-0.0834914876766973,
-6.6638043373535));
#70309=CARTESIAN_POINT('Ctrl Pts',(5.99999999999999,-0.0594801003657474,
-6.66533982565814));
#70310=CARTESIAN_POINT('Ctrl Pts',(5.99999999999999,-0.0354607393562745,
-6.66674643599058));
#70311=CARTESIAN_POINT('Ctrl Pts',(5.99999999999999,-0.0114427696453575,
-6.66802386946623));
#70312=CARTESIAN_POINT('Ctrl Pts',(5.99999999999999,0.17232643902647,-6.67779792371714));
#70313=CARTESIAN_POINT('Ctrl Pts',(5.99999999999999,0.356162228661273,-6.68002334405103));
#70314=CARTESIAN_POINT('Ctrl Pts',(5.99999999999999,0.539578749421798,-6.67477763109705));
#70315=CARTESIAN_POINT('Ctrl Pts',(5.99999999999999,0.724243247873377,-6.66949622597797));
#70316=CARTESIAN_POINT('Ctrl Pts',(6.,0.908483469211453,-6.65664177842282));
#70317=CARTESIAN_POINT('Ctrl Pts',(6.,1.09181827093861,-6.63624254656122));
#70318=CARTESIAN_POINT('Ctrl Pts',(6.,1.27479461914379,-6.61588319897929));
#70319=CARTESIAN_POINT('Ctrl Pts',(6.,1.45686982323424,-6.58800858408027));
#70320=CARTESIAN_POINT('Ctrl Pts',(6.,1.63756918901508,-6.55259533222835));
#70321=CARTESIAN_POINT('Ctrl Pts',(6.,1.68713774842448,-6.54288094352135));
#70322=CARTESIAN_POINT('Ctrl Pts',(5.99999999999999,1.73660276294476,-6.53259898060699));
#70323=CARTESIAN_POINT('Ctrl Pts',(5.99999999999999,1.78595436777605,-6.52174827503316));
#70324=CARTESIAN_POINT('Ctrl Pts',(5.99999999999999,1.92478260633383,-6.49122476223002));
#70325=CARTESIAN_POINT('Ctrl Pts',(6.,2.06271376773678,-6.4562019664384));
#70326=CARTESIAN_POINT('Ctrl Pts',(6.,2.19956587504128,-6.41677751371926));
#70327=CARTESIAN_POINT('Ctrl Pts',(6.,2.25943867198699,-6.39952931565464));
#70328=CARTESIAN_POINT('Ctrl Pts',(6.,2.31910486823453,-6.38143838211038));
#70329=CARTESIAN_POINT('Ctrl Pts',(6.,2.37854887132776,-6.36251183496192));
#70330=CARTESIAN_POINT('Ctrl Pts',(6.,2.41133386438944,-6.35207332670784));
#70331=CARTESIAN_POINT('Ctrl Pts',(6.,2.44405126586026,-6.34138062840303));
#70332=CARTESIAN_POINT('Ctrl Pts',(6.,2.47669842477198,-6.33043485420982));
#70333=CARTESIAN_POINT('Ctrl Pts',(6.,2.49986116879962,-6.32266896663266));
#70334=CARTESIAN_POINT('Ctrl Pts',(6.,2.52298992297603,-6.31477515716261));
#70335=CARTESIAN_POINT('Ctrl Pts',(6.,2.54606625141156,-6.30676003981754));
#70336=CARTESIAN_POINT('Ctrl Pts',(6.,2.72031866926523,-6.24623682527488));
#70337=CARTESIAN_POINT('Ctrl Pts',(6.,2.89180656871482,-6.17872697332531));
#70338=CARTESIAN_POINT('Ctrl Pts',(6.,3.06015974003863,-6.10454067443522));
#70339=CARTESIAN_POINT('Ctrl Pts',(6.,3.23153292294491,-6.02902358100085));
#70340=CARTESIAN_POINT('Ctrl Pts',(6.,3.3996585561246,-5.94658821955142));
#70341=CARTESIAN_POINT('Ctrl Pts',(6.,3.56414018751553,-5.85750818319925));
#70342=CARTESIAN_POINT('Ctrl Pts',(6.,3.72893847172068,-5.76825665387267));
#70343=CARTESIAN_POINT('Ctrl Pts',(6.,3.89007937659884,-5.67233455879464));
#70344=CARTESIAN_POINT('Ctrl Pts',(6.,4.04714827512776,-5.56996716740956));
#70345=CARTESIAN_POINT('Ctrl Pts',(5.99999999999999,4.20261003215418,-5.46864720734118));
#70346=CARTESIAN_POINT('Ctrl Pts',(6.,4.35408329610926,-5.36101281708549));
#70347=CARTESIAN_POINT('Ctrl Pts',(6.,4.5011410535457,-5.24723848450609));
#70348=CARTESIAN_POINT('Ctrl Pts',(6.,4.6045951656092,-5.16719903090768));
#70349=CARTESIAN_POINT('Ctrl Pts',(6.,4.70586353074338,-5.08411998909903));
#70350=CARTESIAN_POINT('Ctrl Pts',(6.,4.80478746383271,-4.99805026259201));
#70351=CARTESIAN_POINT('Ctrl Pts',(6.,4.80478746383271,-4.99805026259201));
#70352=CARTESIAN_POINT('Ctrl Pts',(5.96694870667552,3.97444177895361,-5.79628844103034));
#70353=CARTESIAN_POINT('Ctrl Pts',(5.93389741335104,2.94176938984478,-6.38322417906209));
#70354=CARTESIAN_POINT('Ctrl Pts',(5.90084612002656,1.83131854449184,-6.68740409837522));
#70355=CARTESIAN_POINT('Ctrl Pts',(5.86779482670209,0.720867699138943,-6.99158401768835));
#70356=CARTESIAN_POINT('Ctrl Pts',(5.83474353337761,-0.467361602457999,
-7.01300811828287));
#70357=CARTESIAN_POINT('Ctrl Pts',(5.80169224005313,-1.58829921867574,-6.74922313565156));
#70358=CARTESIAN_POINT('Ctrl Pts',(5.76864094672865,-2.7092368348935,-6.48543815302024));
#70359=CARTESIAN_POINT('Ctrl Pts',(5.73558965340417,-3.76288276573208,-5.93644408716305));
#70360=CARTESIAN_POINT('Ctrl Pts',(5.70253836007969,-4.62129214226549,-5.16896427511983));
#70361=CARTESIAN_POINT('Ctrl Pts',(5.66948706675521,-5.47970151879887,-4.40148446307664));
#70362=CARTESIAN_POINT('Ctrl Pts',(5.63643577343074,-6.14287434102713,-3.41551890484744));
#70363=CARTESIAN_POINT('Ctrl Pts',(5.60338448010626,-6.53001704429179,-2.33104349458117));
#70364=CARTESIAN_POINT('Ctrl Pts',(5.58064687460627,-6.79635149518946,-1.58497967762262));
#70365=CARTESIAN_POINT('Ctrl Pts',(5.55790926910627,-6.93204810038981,-0.792293720665733));
#70366=CARTESIAN_POINT('Ctrl Pts',(5.53517166360628,-6.93272540515737,0.000163154062267218));
#70367=CARTESIAN_POINT('Origin',(10.5,5.,0.));
#70368=CARTESIAN_POINT('Origin',(10.5,5.,0.));
#70369=CARTESIAN_POINT('Origin',(-13.9,0.,0.));
#70370=CARTESIAN_POINT('',(-13.9,-6.65,-8.1439012143299E-16));
#70371=CARTESIAN_POINT('Origin',(-3.775,0.,0.));
#70372=CARTESIAN_POINT('Origin',(6.,0.,0.));
#70373=CARTESIAN_POINT('Origin',(6.,11.5,0.));
#70374=CARTESIAN_POINT('',(6.,-11.5,-1.40834381901946E-15));
#70375=CARTESIAN_POINT('Origin',(6.,0.,0.));
#70376=CARTESIAN_POINT('Origin',(6.25,0.,0.));
#70377=CARTESIAN_POINT('',(6.25,-11.75,-1.43895998899814E-15));
#70378=CARTESIAN_POINT('Origin',(14.75,0.,0.));
#70379=CARTESIAN_POINT('',(15.,-11.5,-1.40834381901946E-15));
#70380=CARTESIAN_POINT('Origin',(15.,0.,0.));
#70381=CARTESIAN_POINT('',(14.75,-11.75,-1.43895998899814E-15));
#70382=CARTESIAN_POINT('Origin',(15.,8.,0.));
#70383=CARTESIAN_POINT('',(15.,-8.,-9.79717439317883E-16));
#70384=CARTESIAN_POINT('Origin',(15.,0.,0.));
#70385=CARTESIAN_POINT('Origin',(15.8,0.,0.));
#70386=CARTESIAN_POINT('',(16.6,-8.,-9.79717439317883E-16));
#70387=CARTESIAN_POINT('Origin',(16.6,0.,0.));
#70388=CARTESIAN_POINT('',(15.8,-8.,-9.79717439317883E-16));
#70389=CARTESIAN_POINT('Origin',(16.8,0.,0.));
#70390=CARTESIAN_POINT('',(16.8,-7.8,-9.55224503334935E-16));
#70391=CARTESIAN_POINT('',(0.,0.,0.));
#70392=CARTESIAN_POINT('Origin',(10.45,0.,0.));
#70393=CARTESIAN_POINT('',(-17.3782112878558,-4.95980655637472,0.00244053657197804));
#70394=CARTESIAN_POINT('',(-17.4835887121441,-4.95607622547182,0.00160660521679311));
#70395=CARTESIAN_POINT('',(10.45,-4.954,-6.06690024297599E-16));
#70396=CARTESIAN_POINT('',(-17.6184,2.11971615148618,4.48120317648902));
#70397=CARTESIAN_POINT('Ctrl Pts',(-17.3782112878558,-4.95980655637472,
0.00244053657197804));
#70398=CARTESIAN_POINT('Ctrl Pts',(-17.3820545464539,-4.96088006034128,
0.161384750450865));
#70399=CARTESIAN_POINT('Ctrl Pts',(-17.385897805052,-4.95392904526419,0.320240835458518));
#70400=CARTESIAN_POINT('Ctrl Pts',(-17.3897410636502,-4.93865078209299,
0.478296092362431));
#70401=CARTESIAN_POINT('Ctrl Pts',(-17.4294963877892,-4.78060981525614,
2.11324669733806));
#70402=CARTESIAN_POINT('Ctrl Pts',(-17.4692517119283,-3.73153769965044,
3.66250719470835));
#70403=CARTESIAN_POINT('Ctrl Pts',(-17.5090070360673,-2.27033074934917,
4.41321306777073));
#70404=CARTESIAN_POINT('Ctrl Pts',(-17.5454713573782,-0.93008460895497,
5.10177443050972));
#70405=CARTESIAN_POINT('Ctrl Pts',(-17.5819356786891,0.756886402755601,
5.11851985816336));
#70406=CARTESIAN_POINT('Ctrl Pts',(-17.6184,2.1230376970401,4.48323345254421));
#70407=CARTESIAN_POINT('',(-17.6184,-2.11639460593172,4.47917290043409));
#70408=CARTESIAN_POINT('Origin',(-17.6184,0.,0.));
#70409=CARTESIAN_POINT('Ctrl Pts',(-17.6184,-2.11639460593172,4.47917290043409));
#70410=CARTESIAN_POINT('Ctrl Pts',(-17.5985223379305,-2.8622965430514,4.1267366646904));
#70411=CARTESIAN_POINT('Ctrl Pts',(-17.578644675861,-3.51256081769737,3.58433682878205));
#70412=CARTESIAN_POINT('Ctrl Pts',(-17.5587670137914,-4.00026620400954,
2.91790966066576));
#70413=CARTESIAN_POINT('Ctrl Pts',(-17.5388893517219,-4.48797159032172,
2.25148249254946));
#70414=CARTESIAN_POINT('Ctrl Pts',(-17.5190116896524,-4.81311808830011,
1.46102799222521));
#70415=CARTESIAN_POINT('Ctrl Pts',(-17.4991340275828,-4.91815019368021,
0.644120288275306));
#70416=CARTESIAN_POINT('Ctrl Pts',(-17.4939522557699,-4.94553029508281,
0.431166204476148));
#70417=CARTESIAN_POINT('Ctrl Pts',(-17.488770483957,-4.95795236637979,0.216414474409738));
#70418=CARTESIAN_POINT('Ctrl Pts',(-17.4835887121441,-4.95607622547182,
0.00160660521679311));
#70419=CARTESIAN_POINT('Origin',(10.45,0.,0.));
#70420=CARTESIAN_POINT('',(-16.6282112878558,-4.94754111804637,0.00290217464796599));
#70421=CARTESIAN_POINT('',(-16.7335887121441,-4.9466458171129,0.00209310800741799));
#70422=CARTESIAN_POINT('',(10.45,-4.954,-6.06690024297599E-16));
#70423=CARTESIAN_POINT('Ctrl Pts',(-16.6282112878558,-4.94754111804637,
0.00290217464796599));
#70424=CARTESIAN_POINT('Ctrl Pts',(-16.6435226016196,-4.95093641568814,
0.640262719595125));
#70425=CARTESIAN_POINT('Ctrl Pts',(-16.6588339153834,-4.83671955758367,
1.27645309649682));
#70426=CARTESIAN_POINT('Ctrl Pts',(-16.6741452291472,-4.59927446317422,
1.86273610510442));
#70427=CARTESIAN_POINT('Ctrl Pts',(-16.7139005532862,-3.9827560612203,3.38500071309082));
#70428=CARTESIAN_POINT('Ctrl Pts',(-16.7536558774253,-2.53547700879338,
4.57080771208592));
#70429=CARTESIAN_POINT('Ctrl Pts',(-16.7934112015644,-0.921670863964594,
4.87584539304171));
#70430=CARTESIAN_POINT('Ctrl Pts',(-16.8331665257034,0.692135280864182,
5.18088307399749));
#70431=CARTESIAN_POINT('Ctrl Pts',(-16.8729218498425,2.47246851809482,4.60515143691398));
#70432=CARTESIAN_POINT('Ctrl Pts',(-16.9126771739815,3.6020671352805,3.41297586664233));
#70433=CARTESIAN_POINT('Ctrl Pts',(-16.9524324981206,4.73166575246619,2.22080029637068));
#70434=CARTESIAN_POINT('Ctrl Pts',(-16.9921878222596,5.21052974960693,0.412180792910897));
#70435=CARTESIAN_POINT('Ctrl Pts',(-17.0319431463987,4.81906279122762,-1.18287422808977));
#70436=CARTESIAN_POINT('Ctrl Pts',(-17.0716984705377,4.4275958328483,-2.77792924909044));
#70437=CARTESIAN_POINT('Ctrl Pts',(-17.1114537946768,3.16579791894893,-4.15941978763199));
#70438=CARTESIAN_POINT('Ctrl Pts',(-17.1512091188158,1.61244706364669,-4.69300265883637));
#70439=CARTESIAN_POINT('Ctrl Pts',(-17.1909644429549,0.0590962083444407,
-5.22658553004074));
#70440=CARTESIAN_POINT('Ctrl Pts',(-17.230719767094,-1.78580758836068,-4.91226073390795));
#70441=CARTESIAN_POINT('Ctrl Pts',(-17.270475091233,-3.07475457767925,-3.89477797955106));
#70442=CARTESIAN_POINT('Ctrl Pts',(-17.3063871567739,-4.23909544928865,
-2.97565813453576));
#70443=CARTESIAN_POINT('Ctrl Pts',(-17.3422992223148,-4.94977555174121,
-1.48276137748618));
#70444=CARTESIAN_POINT('Ctrl Pts',(-17.3782112878558,-4.95980655637472,
0.00244053657197804));
#70445=CARTESIAN_POINT('Ctrl Pts',(-17.4835887121441,-4.95607622547182,
0.00160660521679311));
#70446=CARTESIAN_POINT('Ctrl Pts',(-17.449015159818,-4.94355833425728,-1.43162345078241));
#70447=CARTESIAN_POINT('Ctrl Pts',(-17.4144416074918,-4.29451879539502,
-2.86735268421774));
#70448=CARTESIAN_POINT('Ctrl Pts',(-17.3798680551657,-3.2049418960497,-3.78830498722671));
#70449=CARTESIAN_POINT('Ctrl Pts',(-17.3401127310266,-1.95206274729191,
-4.8472866324265));
#70450=CARTESIAN_POINT('Ctrl Pts',(-17.3003574068876,-0.116697809409273,
-5.22562170042369));
#70451=CARTESIAN_POINT('Ctrl Pts',(-17.2606020827485,1.45422416551184,-4.74511164472302));
#70452=CARTESIAN_POINT('Ctrl Pts',(-17.2208467586095,3.02514614043297,-4.26460158902235));
#70453=CARTESIAN_POINT('Ctrl Pts',(-17.1810914344704,4.33162515239257,-2.92524640962383));
#70454=CARTESIAN_POINT('Ctrl Pts',(-17.1413361103314,4.77626420482008,-1.34400114385843));
#70455=CARTESIAN_POINT('Ctrl Pts',(-17.1015807861923,5.22090325724759,0.237244121906955));
#70456=CARTESIAN_POINT('Ctrl Pts',(-17.0618254620532,4.80370235014301,2.06037947403921));
#70457=CARTESIAN_POINT('Ctrl Pts',(-17.0220701379142,3.71497358052998,3.28973911961942));
#70458=CARTESIAN_POINT('Ctrl Pts',(-16.9823148137751,2.62624481091696,4.51909876519962));
#70459=CARTESIAN_POINT('Ctrl Pts',(-16.9425594896361,0.865988178795493,
5.15468270422777));
#70460=CARTESIAN_POINT('Ctrl Pts',(-16.902804165497,-0.757234442789558,
4.90416721199705));
#70461=CARTESIAN_POINT('Ctrl Pts',(-16.863048841358,-2.38045706437461,4.65365171976634));
#70462=CARTESIAN_POINT('Ctrl Pts',(-16.8232935172189,-3.86664567542324,
3.51703679627675));
#70463=CARTESIAN_POINT('Ctrl Pts',(-16.7835381930799,-4.53397860724609,
2.01633239046266));
#70464=CARTESIAN_POINT('Ctrl Pts',(-16.7668883661013,-4.81346262838259,
1.38782616534876));
#70465=CARTESIAN_POINT('Ctrl Pts',(-16.7502385391227,-4.9493196071233,0.695458753409945));
#70466=CARTESIAN_POINT('Ctrl Pts',(-16.7335887121441,-4.9466458171129,0.00209310800741799));
#70467=CARTESIAN_POINT('Origin',(10.45,0.,0.));
#70468=CARTESIAN_POINT('',(-15.8782112878558,-4.94963099410875,-0.0039542947945842));
#70469=CARTESIAN_POINT('',(-15.9835887121441,-4.95109393512768,-0.00433887822852018));
#70470=CARTESIAN_POINT('',(10.45,-4.954,-6.06690024297599E-16));
#70471=CARTESIAN_POINT('Ctrl Pts',(-15.8782112878558,-4.94963099410875,
-0.0039542947945842));
#70472=CARTESIAN_POINT('Ctrl Pts',(-15.9049906567853,-4.94133152292927,
1.10960955975419));
#70473=CARTESIAN_POINT('Ctrl Pts',(-15.9317700257147,-4.56971376715886,
2.22819216688661));
#70474=CARTESIAN_POINT('Ctrl Pts',(-15.9585493946442,-3.88008016453715,
3.09324852781628));
#70475=CARTESIAN_POINT('Ctrl Pts',(-15.9983047187833,-2.85628429086991,
4.37746833590356));
#70476=CARTESIAN_POINT('Ctrl Pts',(-16.0380600429223,-1.13161646218319,
5.10294417703389));
#70477=CARTESIAN_POINT('Ctrl Pts',(-16.0778153670614,0.502316997631763,
4.93668818591454));
#70478=CARTESIAN_POINT('Ctrl Pts',(-16.1175706912004,2.13625045744672,4.77043219479518));
#70479=CARTESIAN_POINT('Ctrl Pts',(-16.1573260153395,3.67944954838991,3.71244437142615));
#70480=CARTESIAN_POINT('Ctrl Pts',(-16.1970813394785,4.4235971230862,2.24833338328714));
#70481=CARTESIAN_POINT('Ctrl Pts',(-16.2368366636176,5.16774469778249,0.784222395148121));
#70482=CARTESIAN_POINT('Ctrl Pts',(-16.2765919877566,5.11284075623187,-1.08601175776088));
#70483=CARTESIAN_POINT('Ctrl Pts',(-16.3163473118957,4.28408994860642,-2.50395072399457));
#70484=CARTESIAN_POINT('Ctrl Pts',(-16.3561026360347,3.45533914098097,-3.92188969022827));
#70485=CARTESIAN_POINT('Ctrl Pts',(-16.3958579601738,1.85274146728066,-4.88753346978664));
#70486=CARTESIAN_POINT('Ctrl Pts',(-16.4356132843129,0.211867270152115,
-4.95765464081455));
#70487=CARTESIAN_POINT('Ctrl Pts',(-16.4753686084519,-1.42900692697643,
-5.02777581184246));
#70488=CARTESIAN_POINT('Ctrl Pts',(-16.515123932591,-3.10815764753321,-4.2023743743399));
#70489=CARTESIAN_POINT('Ctrl Pts',(-16.55487925673,-4.05485413207113,-2.86031254709977));
#70490=CARTESIAN_POINT('Ctrl Pts',(-16.5793232671053,-4.63694116547867,
-2.03513066417666));
#70491=CARTESIAN_POINT('Ctrl Pts',(-16.6037672774805,-4.94212063669103,
-1.01462303669556));
#70492=CARTESIAN_POINT('Ctrl Pts',(-16.6282112878558,-4.94754111804637,
0.00290217464796599));
#70493=CARTESIAN_POINT('Ctrl Pts',(-16.7335887121441,-4.9466458171129,0.00209310800741799));
#70494=CARTESIAN_POINT('Ctrl Pts',(-16.7104832149836,-4.94293531323964,
-0.960112563655588));
#70495=CARTESIAN_POINT('Ctrl Pts',(-16.6873777178232,-4.67244225281239,
-1.9242406333381));
#70496=CARTESIAN_POINT('Ctrl Pts',(-16.6642722206627,-4.14878639781746,
-2.72229021995792));
#70497=CARTESIAN_POINT('Ctrl Pts',(-16.6245168965236,-3.24778400396889,
-4.0954145364258));
#70498=CARTESIAN_POINT('Ctrl Pts',(-16.5847615723846,-1.59730196367469,
-4.97686928122295));
#70499=CARTESIAN_POINT('Ctrl Pts',(-16.5450062482455,0.0450125217207269,
-4.96198750357192));
#70500=CARTESIAN_POINT('Ctrl Pts',(-16.5052509241065,1.68732700711615,-4.9471057259209));
#70501=CARTESIAN_POINT('Ctrl Pts',(-16.4654955999674,3.32147393761279,-4.03588742582169));
#70502=CARTESIAN_POINT('Ctrl Pts',(-16.4257402758284,4.1974416845951,-2.64661961403913));
#70503=CARTESIAN_POINT('Ctrl Pts',(-16.3859849516893,5.07340943157741,-1.25735180225659));
#70504=CARTESIAN_POINT('Ctrl Pts',(-16.3462296275503,5.1911979950454,0.609965521209312));
#70505=CARTESIAN_POINT('Ctrl Pts',(-16.3064743034112,4.49671841016726,2.09827407943552));
#70506=CARTESIAN_POINT('Ctrl Pts',(-16.2667189792721,3.80223882528911,3.58658263766173));
#70507=CARTESIAN_POINT('Ctrl Pts',(-16.2269636551331,2.29549109206482,4.69588243064825));
#70508=CARTESIAN_POINT('Ctrl Pts',(-16.187208330994,0.668072464940804,4.91700184303135));
#70509=CARTESIAN_POINT('Ctrl Pts',(-16.147453006855,-0.95934616218321,5.13812125541445));
#70510=CARTESIAN_POINT('Ctrl Pts',(-16.1076976827159,-2.70743568320695,
4.47106028719414));
#70511=CARTESIAN_POINT('Ctrl Pts',(-16.0679423585769,-3.77384519331976,
3.22200078380499));
#70512=CARTESIAN_POINT('Ctrl Pts',(-16.0398244764326,-4.52808824308058,
2.33857425747055));
#70513=CARTESIAN_POINT('Ctrl Pts',(-16.0117065942884,-4.94133066842602,
1.16401133176273));
#70514=CARTESIAN_POINT('Ctrl Pts',(-15.9835887121441,-4.95109393512768,
-0.00433887822852018));
#70515=CARTESIAN_POINT('Origin',(10.45,0.,0.));
#70516=CARTESIAN_POINT('',(-15.1282112878558,-4.96185087269624,-0.00115664513161418));
#70517=CARTESIAN_POINT('',(-15.2335887121441,-4.9621737197389,-0.000131629710198743));
#70518=CARTESIAN_POINT('',(10.45,-4.954,-6.06690024297599E-16));
#70519=CARTESIAN_POINT('Ctrl Pts',(-15.1282112878558,-4.96185087269624,
-0.00115664513161418));
#70520=CARTESIAN_POINT('Ctrl Pts',(-15.1664587119509,-4.9568780428024,1.57919865857407));
#70521=CARTESIAN_POINT('Ctrl Pts',(-15.2047061360461,-4.13630119926,3.16399456753119));
#70522=CARTESIAN_POINT('Ctrl Pts',(-15.2429535601412,-2.8407735100365,4.06856442895952));
#70523=CARTESIAN_POINT('Ctrl Pts',(-15.2827088842803,-1.4941697992068,5.00879684717528));
#70524=CARTESIAN_POINT('Ctrl Pts',(-15.3224642084193,0.365572742064798,
5.21411026979585));
#70525=CARTESIAN_POINT('Ctrl Pts',(-15.3622195325584,1.88484852979504,4.59026760960427));
#70526=CARTESIAN_POINT('Ctrl Pts',(-15.4019748566974,3.40412431752528,3.9664249494127));
#70527=CARTESIAN_POINT('Ctrl Pts',(-15.4417301808365,4.58293335171415,2.513426206409));
#70528=CARTESIAN_POINT('Ctrl Pts',(-15.4814855049755,4.88021251791395,0.898185164615993));
#70529=CARTESIAN_POINT('Ctrl Pts',(-15.5212408291146,5.17749168411375,-0.717055877177018));
#70530=CARTESIAN_POINT('Ctrl Pts',(-15.5609961532537,4.59324098232445,-2.49453921775932));
#70531=CARTESIAN_POINT('Ctrl Pts',(-15.6007514773927,3.39562647972561,-3.61841556400534));
#70532=CARTESIAN_POINT('Ctrl Pts',(-15.6405068015318,2.19801197712677,-4.74229191025135));
#70533=CARTESIAN_POINT('Ctrl Pts',(-15.6802621256708,0.387033673718383,
-5.21256126216107));
#70534=CARTESIAN_POINT('Ctrl Pts',(-15.7200174498099,-1.20608535228746,
-4.81337397416404));
#70535=CARTESIAN_POINT('Ctrl Pts',(-15.7597727739489,-2.7992043782933,-4.41418668616701));
#70536=CARTESIAN_POINT('Ctrl Pts',(-15.799528098088,-4.1744641268966,-3.14554275826323));
#70537=CARTESIAN_POINT('Ctrl Pts',(-15.839283422227,-4.70063204187437,-1.58973890678923));
#70538=CARTESIAN_POINT('Ctrl Pts',(-15.8522593774366,-4.87237083272382,
-1.08193167520928));
#70539=CARTESIAN_POINT('Ctrl Pts',(-15.8652353326462,-4.9536525065862,-0.543532159294824));
#70540=CARTESIAN_POINT('Ctrl Pts',(-15.8782112878558,-4.94963099410875,
-0.0039542947945842));
#70541=CARTESIAN_POINT('Ctrl Pts',(-15.9835887121441,-4.95109393512768,
-0.00433887822852018));
#70542=CARTESIAN_POINT('Ctrl Pts',(-15.9719512701493,-4.95513476044081,
-0.487896200526849));
#70543=CARTESIAN_POINT('Ctrl Pts',(-15.9603138281545,-4.89006080214088,
-0.970389303042811));
#70544=CARTESIAN_POINT('Ctrl Pts',(-15.9486763861597,-4.75144255109529,
-1.43073717552031));
#70545=CARTESIAN_POINT('Ctrl Pts',(-15.9089210620207,-4.27790089955613,
-3.00335759289846));
#70546=CARTESIAN_POINT('Ctrl Pts',(-15.8691657378816,-2.94608809727594,
-4.31754038909679));
#70547=CARTESIAN_POINT('Ctrl Pts',(-15.8294104137426,-1.36729653084616,
-4.77008526960488));
#70548=CARTESIAN_POINT('Ctrl Pts',(-15.7896550896035,0.211495035583636,
-5.22263015011297));
#70549=CARTESIAN_POINT('Ctrl Pts',(-15.7498997654644,2.03726536616302,-4.81353711493081));
#70550=CARTESIAN_POINT('Ctrl Pts',(-15.7101444413254,3.27200281351365,-3.73057727440859));
#70551=CARTESIAN_POINT('Ctrl Pts',(-15.6703891171863,4.50674026086427,-2.64761743388638));
#70552=CARTESIAN_POINT('Ctrl Pts',(-15.6306337930473,5.15044482498614,-0.890790788024123));
#70553=CARTESIAN_POINT('Ctrl Pts',(-15.5908784689082,4.90766119087328,0.733535065939904));
#70554=CARTESIAN_POINT('Ctrl Pts',(-15.5511231447692,4.66487755676042,2.35786091990394));
#70555=CARTESIAN_POINT('Ctrl Pts',(-15.5113678206301,3.53560572441281,3.84968598196975));
#70556=CARTESIAN_POINT('Ctrl Pts',(-15.471612496491,2.0381718980976,4.52427528766509));
#70557=CARTESIAN_POINT('Ctrl Pts',(-15.431857172352,0.54073807178239,5.19886459336044));
#70558=CARTESIAN_POINT('Ctrl Pts',(-15.3921018482129,-1.32485774850043,
5.05621814268532));
#70559=CARTESIAN_POINT('Ctrl Pts',(-15.3523465240739,-2.70232349767177,
4.16180955481897));
#70560=CARTESIAN_POINT('Ctrl Pts',(-15.312760586764,-4.07392023280467,3.27121180331023));
#70561=CARTESIAN_POINT('Ctrl Pts',(-15.273174649454,-4.96153761937937,1.63524438301617));
#70562=CARTESIAN_POINT('Ctrl Pts',(-15.2335887121441,-4.9621737197389,-0.000131629710198743));
#70563=CARTESIAN_POINT('Origin',(10.45,0.,0.));
#70564=CARTESIAN_POINT('',(-14.3782112878558,-4.95311312927936,0.00456086744855991));
#70565=CARTESIAN_POINT('',(-14.4835887121441,-4.95148814634774,0.00440770772639709));
#70566=CARTESIAN_POINT('',(10.45,-4.954,-6.06690024297599E-16));
#70567=CARTESIAN_POINT('Ctrl Pts',(-14.3782112878558,-4.95311312927936,
0.00456086744855991));
#70568=CARTESIAN_POINT('Ctrl Pts',(-14.3881714429775,-4.95686762720455,
0.417995751918769));
#70569=CARTESIAN_POINT('Ctrl Pts',(-14.3981315980993,-4.90944555725122,
0.830581339778542));
#70570=CARTESIAN_POINT('Ctrl Pts',(-14.4080917532211,-4.80751544623729,
1.22922980986666));
#70571=CARTESIAN_POINT('Ctrl Pts',(-14.4478470773601,-4.40066790688175,
2.82040976159881));
#70572=CARTESIAN_POINT('Ctrl Pts',(-14.4876024014992,-3.12542206198846,
4.18954963958238));
#70573=CARTESIAN_POINT('Ctrl Pts',(-14.5273577256382,-1.56710463410095,
4.70822617933687));
#70574=CARTESIAN_POINT('Ctrl Pts',(-14.5671130497773,-0.00878720621342921,
5.22690271909136));
#70575=CARTESIAN_POINT('Ctrl Pts',(-14.6068683739163,1.83260180466831,4.89511592061677));
#70576=CARTESIAN_POINT('Ctrl Pts',(-14.6466236980554,3.11188090056794,3.86515303077406));
#70577=CARTESIAN_POINT('Ctrl Pts',(-14.6863790221945,4.39115999646756,2.83519014093136));
#70578=CARTESIAN_POINT('Ctrl Pts',(-14.7261343463335,5.10832917738507,1.10705115972054));
#70579=CARTESIAN_POINT('Ctrl Pts',(-14.7658896704726,4.93421404221,-0.52606318972133));
#70580=CARTESIAN_POINT('Ctrl Pts',(-14.8056449946116,4.76009890703493,-2.15917753916319));
#70581=CARTESIAN_POINT('Ctrl Pts',(-14.8454003187507,3.6946994557673,-3.69726725683611));
#70582=CARTESIAN_POINT('Ctrl Pts',(-14.8851556428897,2.22702474783851,-4.43436257622917));
#70583=CARTESIAN_POINT('Ctrl Pts',(-14.9249109670288,0.759350039909706,
-5.17145789562223));
#70584=CARTESIAN_POINT('Ctrl Pts',(-14.9646662911678,-1.11059992468025,
-5.10755881673543));
#70585=CARTESIAN_POINT('Ctrl Pts',(-15.0044216153069,-2.52453442237049,
-4.27199445713027));
#70586=CARTESIAN_POINT('Ctrl Pts',(-15.0441769394459,-3.93846892006073,
-3.43643009752511));
#70587=CARTESIAN_POINT('Ctrl Pts',(-15.083932263585,-4.89638795085125,-1.8292004572016));
#70588=CARTESIAN_POINT('Ctrl Pts',(-15.1236875877241,-4.95861502605261,
-0.188009930134371));
#70589=CARTESIAN_POINT('Ctrl Pts',(-15.125195487768,-4.96097526864804,-0.125760374347325));
#70590=CARTESIAN_POINT('Ctrl Pts',(-15.1267033878119,-4.96204692591009,
-0.0634619608025481));
#70591=CARTESIAN_POINT('Ctrl Pts',(-15.1282112878558,-4.96185087269624,
-0.00115664513161418));
#70592=CARTESIAN_POINT('Ctrl Pts',(-15.2335887121441,-4.9621737197389,-0.000131629710198743));
#70593=CARTESIAN_POINT('Ctrl Pts',(-15.233419325315,-4.9621764415899,-0.00712934597106935));
#70594=CARTESIAN_POINT('Ctrl Pts',(-15.2332499384858,-4.96216292322238,
-0.0141270514035398));
#70595=CARTESIAN_POINT('Ctrl Pts',(-15.2330805516567,-4.96213313306282,
-0.0211246875646397));
#70596=CARTESIAN_POINT('Ctrl Pts',(-15.1933252275177,-4.95514134122268,
-1.66347961702442));
#70597=CARTESIAN_POINT('Ctrl Pts',(-15.1535699033786,-4.05182207948253,
-3.30201875088644));
#70598=CARTESIAN_POINT('Ctrl Pts',(-15.1138145792396,-2.66679105273963,
-4.18466687585192));
#70599=CARTESIAN_POINT('Ctrl Pts',(-15.0740592551005,-1.28176002599674,
-5.0673150008174));
#70600=CARTESIAN_POINT('Ctrl Pts',(-15.0343039309615,0.584982765748895,
-5.19407211688634));
#70601=CARTESIAN_POINT('Ctrl Pts',(-14.9945486068224,2.07661868124458,-4.5067578339041));
#70602=CARTESIAN_POINT('Ctrl Pts',(-14.9547932826833,3.56825459674025,-3.81944355092187));
#70603=CARTESIAN_POINT('Ctrl Pts',(-14.9150379585443,4.68478363598596,-2.31805786888846));
#70604=CARTESIAN_POINT('Ctrl Pts',(-14.8752826344052,4.91372869508898,-0.691723712375354));
#70605=CARTESIAN_POINT('Ctrl Pts',(-14.8355273102662,5.142673754192,0.934610444137763));
#70606=CARTESIAN_POINT('Ctrl Pts',(-14.7957719861271,4.48403483315231,2.68589307513059));
#70607=CARTESIAN_POINT('Ctrl Pts',(-14.7560166619881,3.24012145917152,3.75830071895447));
#70608=CARTESIAN_POINT('Ctrl Pts',(-14.716261337849,1.99620808519072,4.83070836277836));
#70609=CARTESIAN_POINT('Ctrl Pts',(-14.6765060137099,0.167020258268824,
5.22424101943332));
#70610=CARTESIAN_POINT('Ctrl Pts',(-14.6367506895709,-1.40786076327547,
4.75827063427213));
#70611=CARTESIAN_POINT('Ctrl Pts',(-14.5969953654318,-2.98274178481976,
4.29230024911094));
#70612=CARTESIAN_POINT('Ctrl Pts',(-14.5572400412928,-4.30331600098644,
2.96682682213362));
#70613=CARTESIAN_POINT('Ctrl Pts',(-14.5174847171537,-4.76345136071661,
1.3902310961853));
#70614=CARTESIAN_POINT('Ctrl Pts',(-14.5061860488172,-4.89422420516193,
0.942154452513536));
#70615=CARTESIAN_POINT('Ctrl Pts',(-14.4948873804806,-4.95549718832007,
0.473794014340802));
#70616=CARTESIAN_POINT('Ctrl Pts',(-14.4835887121441,-4.95148814634774,
0.00440770772639709));
#70617=CARTESIAN_POINT('Origin',(10.45,0.,0.));
#70618=CARTESIAN_POINT('',(-13.6282112878558,-4.94601675291934,-0.00105820789737976));
#70619=CARTESIAN_POINT('',(-13.7335887121441,-4.94651950398206,-0.00192876730649404));
#70620=CARTESIAN_POINT('',(10.45,-4.954,-6.06690024297599E-16));
#70621=CARTESIAN_POINT('Ctrl Pts',(-13.6282112878558,-4.94601675291934,
-0.00105820789737976));
#70622=CARTESIAN_POINT('Ctrl Pts',(-13.6496394981432,-4.944317184649,0.891622090528033));
#70623=CARTESIAN_POINT('Ctrl Pts',(-13.6710677084306,-4.71383143873792,
1.78512061197043));
#70624=CARTESIAN_POINT('Ctrl Pts',(-13.6924959187181,-4.25979883424053,
2.54505885641213));
#70625=CARTESIAN_POINT('Ctrl Pts',(-13.7322512428571,-3.41744134757363,
3.95495687534098));
#70626=CARTESIAN_POINT('Ctrl Pts',(-13.7720065669962,-1.80562152001957,
4.90513202435166));
#70627=CARTESIAN_POINT('Ctrl Pts',(-13.8117618911352,-0.164150596859296,
4.95946219587632));
#70628=CARTESIAN_POINT('Ctrl Pts',(-13.8515172152743,1.47732032630098,5.01379236740099));
#70629=CARTESIAN_POINT('Ctrl Pts',(-13.8912725394134,3.14844234506749,4.17227756143964));
#70630=CARTESIAN_POINT('Ctrl Pts',(-13.9310278635524,4.08218502554369,2.82116573564903));
#70631=CARTESIAN_POINT('Ctrl Pts',(-13.9707831876915,5.01592770601988,1.47005390985843));
#70632=CARTESIAN_POINT('Ctrl Pts',(-14.0105385118305,5.21229104820577,-0.390654935761419));
#70633=CARTESIAN_POINT('Ctrl Pts',(-14.0502938359696,4.58114599036622,-1.90691166701902));
#70634=CARTESIAN_POINT('Ctrl Pts',(-14.0900491601086,3.95000093252669,-3.42316839827661));
#70635=CARTESIAN_POINT('Ctrl Pts',(-14.1298044842477,2.49134747466172,-4.59497301517194));
#70636=CARTESIAN_POINT('Ctrl Pts',(-14.1695598083867,0.874694834058384,
-4.88447741707956));
#70637=CARTESIAN_POINT('Ctrl Pts',(-14.2093151325258,-0.741957806544973,
-5.17398181898719));
#70638=CARTESIAN_POINT('Ctrl Pts',(-14.2490704566648,-2.51660962988671,
-4.58118600590708));
#70639=CARTESIAN_POINT('Ctrl Pts',(-14.2888257808039,-3.63471092464868,
-3.37817808662665));
#70640=CARTESIAN_POINT('Ctrl Pts',(-14.3186209498212,-4.47268716499728,
-2.47656742037406));
#70641=CARTESIAN_POINT('Ctrl Pts',(-14.3484161188385,-4.94188178811161,
-1.2322032300823));
#70642=CARTESIAN_POINT('Ctrl Pts',(-14.3782112878558,-4.95311312927936,
0.00456086744855991));
#70643=CARTESIAN_POINT('Ctrl Pts',(-14.4835887121441,-4.95148814634774,
0.00440770772639709));
#70644=CARTESIAN_POINT('Ctrl Pts',(-14.4551320563416,-4.94139103365212,
-1.17778157050275));
#70645=CARTESIAN_POINT('Ctrl Pts',(-14.4266754005391,-4.51719240613835,
-2.3664782092933));
#70646=CARTESIAN_POINT('Ctrl Pts',(-14.3982187447366,-3.74627668568719,
-3.25401634256688));
#70647=CARTESIAN_POINT('Ctrl Pts',(-14.3584634205975,-2.66927014763396,
-4.49395003045146));
#70648=CARTESIAN_POINT('Ctrl Pts',(-14.3187080964585,-0.915560568233825,
-5.14609938130129));
#70649=CARTESIAN_POINT('Ctrl Pts',(-14.2789527723194,0.709914648923431,
-4.91113353046451));
#70650=CARTESIAN_POINT('Ctrl Pts',(-14.2391974481804,2.33538986608067,-4.67616767962773));
#70651=CARTESIAN_POINT('Ctrl Pts',(-14.1994421240413,3.83263072099504,-3.55408662710436));
#70652=CARTESIAN_POINT('Ctrl Pts',(-14.1596867999022,4.51441671742681,-2.05991579087256));
#70653=CARTESIAN_POINT('Ctrl Pts',(-14.1199314757632,5.19620271385857,-0.565744954640754));
#70654=CARTESIAN_POINT('Ctrl Pts',(-14.0801761516241,5.06253385180771,1.30051566529948));
#70655=CARTESIAN_POINT('Ctrl Pts',(-14.0404208274851,4.17476297344876,2.68226871864855));
#70656=CARTESIAN_POINT('Ctrl Pts',(-14.000665503346,3.28699209508979,4.06402177199765));
#70657=CARTESIAN_POINT('Ctrl Pts',(-13.960910179207,1.64511920042269,4.96126725875556));
#70658=CARTESIAN_POINT('Ctrl Pts',(-13.9211548550679,0.00274963038812914,
4.96217732482585));
#70659=CARTESIAN_POINT('Ctrl Pts',(-13.8813995309289,-1.63961993964642,
4.96308739089613));
#70660=CARTESIAN_POINT('Ctrl Pts',(-13.8416442067898,-3.28248618504843,
4.06766203627881));
#70661=CARTESIAN_POINT('Ctrl Pts',(-13.8018888826508,-4.17178782544991,
2.68689369032047));
#70662=CARTESIAN_POINT('Ctrl Pts',(-13.7791221591485,-4.68106513598758,
1.89616762195546));
#70663=CARTESIAN_POINT('Ctrl Pts',(-13.7563554356463,-4.94320932191155,
0.946272281090748));
#70664=CARTESIAN_POINT('Ctrl Pts',(-13.7335887121441,-4.94651950398206,
-0.00192876730649404));
#70665=CARTESIAN_POINT('Origin',(10.45,0.,0.));
#70666=CARTESIAN_POINT('',(-12.8782112878558,-4.9570073981747,-0.00414712514969162));
#70667=CARTESIAN_POINT('',(-12.9835887121441,-4.95857558632536,-0.00363955744209949));
#70668=CARTESIAN_POINT('',(10.45,-4.954,-6.06690024297599E-16));
#70669=CARTESIAN_POINT('Ctrl Pts',(-12.8782112878558,-4.9570073981747,-0.00414712514969162));
#70670=CARTESIAN_POINT('Ctrl Pts',(-12.9111075533089,-4.94478592313273,
1.35858830385809));
#70671=CARTESIAN_POINT('Ctrl Pts',(-12.944003818762,-4.3605420522345,2.73052896938504));
#70672=CARTESIAN_POINT('Ctrl Pts',(-12.9769000842151,-3.3606514679749,3.65092213030985));
#70673=CARTESIAN_POINT('Ctrl Pts',(-13.0166554083541,-2.15227800267999,
4.76322250677954));
#70674=CARTESIAN_POINT('Ctrl Pts',(-13.0564107324932,-0.336858325563938,
5.21604406791286));
#70675=CARTESIAN_POINT('Ctrl Pts',(-13.0961660566323,1.25234576260349,4.80154566589518));
#70676=CARTESIAN_POINT('Ctrl Pts',(-13.1359213807713,2.84154985077095,4.38704726387748));
#70677=CARTESIAN_POINT('Ctrl Pts',(-13.1756767049104,4.20453834998979,3.10522889870875));
#70678=CARTESIAN_POINT('Ctrl Pts',(-13.2154320290494,4.71571142480423,1.54443402214475));
#70679=CARTESIAN_POINT('Ctrl Pts',(-13.2551873531885,5.22688449961866,-0.0163608544192304));
#70680=CARTESIAN_POINT('Ctrl Pts',(-13.2949426773275,4.88624215002873,-1.85613224237847));
#70681=CARTESIAN_POINT('Ctrl Pts',(-13.3346980014666,3.85013624398807,-3.13044111804054));
#70682=CARTESIAN_POINT('Ctrl Pts',(-13.3744533256057,2.8140303379474,-4.4047499937026));
#70683=CARTESIAN_POINT('Ctrl Pts',(-13.4142086497447,1.08246087545601,-5.1135963570675));
#70684=CARTESIAN_POINT('Ctrl Pts',(-13.4539639738837,-0.549796860028286,
-4.93162590871302));
#70685=CARTESIAN_POINT('Ctrl Pts',(-13.4937192980228,-2.1820545955126,-4.74965546035853));
#70686=CARTESIAN_POINT('Ctrl Pts',(-13.5334746221619,-3.71500060398981,
-3.67686820028464));
#70687=CARTESIAN_POINT('Ctrl Pts',(-13.5732299463009,-4.44502603533852,
-2.20566412582418));
#70688=CARTESIAN_POINT('Ctrl Pts',(-13.5915570601525,-4.78156609593791,
-1.52744239941352));
#70689=CARTESIAN_POINT('Ctrl Pts',(-13.6098841740042,-4.94747035920615,
-0.764549570119788));
#70690=CARTESIAN_POINT('Ctrl Pts',(-13.6282112878558,-4.94601675291934,
-0.00105820789737976));
#70691=CARTESIAN_POINT('Ctrl Pts',(-13.7335887121441,-4.94651950398206,
-0.00192876730649404));
#70692=CARTESIAN_POINT('Ctrl Pts',(-13.7166001115073,-4.94898957224751,
-0.709479369969114));
#70693=CARTESIAN_POINT('Ctrl Pts',(-13.6996115108704,-4.80733591544937,
-1.41608655817256));
#70694=CARTESIAN_POINT('Ctrl Pts',(-13.6826229102336,-4.51669681609159,
-2.05491149081309));
#70695=CARTESIAN_POINT('Ctrl Pts',(-13.6428675860945,-3.83656713093088,
-3.5498369886889));
#70696=CARTESIAN_POINT('Ctrl Pts',(-13.6031122619555,-2.34057072520854,
-4.67357664714119));
#70697=CARTESIAN_POINT('Ctrl Pts',(-13.5633569378164,-0.715356903585403,
-4.91034376231061));
#70698=CARTESIAN_POINT('Ctrl Pts',(-13.5236016136774,0.909856918037765,
-5.14711087748003));
#70699=CARTESIAN_POINT('Ctrl Pts',(-13.4838462895383,2.66428815556175,-4.49690544936654));
#70700=CARTESIAN_POINT('Ctrl Pts',(-13.4440909653993,3.74266817014626,-3.25816609947485));
#70701=CARTESIAN_POINT('Ctrl Pts',(-13.4043356412602,4.82104818473077,-2.01942674958316));
#70702=CARTESIAN_POINT('Ctrl Pts',(-13.3645803171212,5.22337697637581,-0.192153477913265));
#70703=CARTESIAN_POINT('Ctrl Pts',(-13.3248249929821,4.76498913815175,1.3849512182294));
#70704=CARTESIAN_POINT('Ctrl Pts',(-13.285069668843,4.3066012999277,2.96205591437203));
#70705=CARTESIAN_POINT('Ctrl Pts',(-13.245314344704,2.98749683183458,4.28899203498746));
#70706=CARTESIAN_POINT('Ctrl Pts',(-13.2055590205649,1.41313318172271,4.75670747201202));
#70707=CARTESIAN_POINT('Ctrl Pts',(-13.1658036964259,-0.161230468389194,
5.22442290903659));
#70708=CARTESIAN_POINT('Ctrl Pts',(-13.1260483722868,-1.99085330051983,
4.83291766247028));
#70709=CARTESIAN_POINT('Ctrl Pts',(-13.0862930481478,-3.2359543896031,3.76188922643825));
#70710=CARTESIAN_POINT('Ctrl Pts',(-13.0520582694799,-4.30815694679576,
2.83958706317767));
#70711=CARTESIAN_POINT('Ctrl Pts',(-13.017823490812,-4.94690340106977,1.41337982358395));
#70712=CARTESIAN_POINT('Ctrl Pts',(-12.9835887121441,-4.95857558632536,
-0.00363955744209949));
#70713=CARTESIAN_POINT('Origin',(10.45,0.,0.));
#70714=CARTESIAN_POINT('',(-12.1282112878558,-4.95954504035343,0.00318967636549851));
#70715=CARTESIAN_POINT('',(-12.2335887121441,-4.95809108523107,0.00382194074085128));
#70716=CARTESIAN_POINT('',(10.45,-4.954,-6.06690024297599E-16));
#70717=CARTESIAN_POINT('Ctrl Pts',(-12.1282112878558,-4.95954504035343,
0.00318967636549851));
#70718=CARTESIAN_POINT('Ctrl Pts',(-12.1328202843355,-4.9609705376935,0.193864214572376));
#70719=CARTESIAN_POINT('Ctrl Pts',(-12.1374292808152,-4.95093040129845,
0.384387214448792));
#70720=CARTESIAN_POINT('Ctrl Pts',(-12.1420382772949,-4.92892361674062,
0.57351780366819));
#70721=CARTESIAN_POINT('Ctrl Pts',(-12.181793601434,-4.73910206725498,2.20488114102573));
#70722=CARTESIAN_POINT('Ctrl Pts',(-12.2215489255731,-3.65895183048629,
3.73264795448116));
#70723=CARTESIAN_POINT('Ctrl Pts',(-12.2613042497121,-2.18425244586393,
4.45558659926224));
#70724=CARTESIAN_POINT('Ctrl Pts',(-12.3010595738512,-0.70955306124158,
5.17852524404332));
#70725=CARTESIAN_POINT('Ctrl Pts',(-12.3408148979902,1.15969547123444,5.09663572015007));
#70726=CARTESIAN_POINT('Ctrl Pts',(-12.3805702221293,2.56552437558869,4.24750460494725));
#70727=CARTESIAN_POINT('Ctrl Pts',(-12.4203255462683,3.97135327994293,3.39837348974444));
#70728=CARTESIAN_POINT('Ctrl Pts',(-12.4600808704074,4.91376255617541,1.78200078323208));
#70729=CARTESIAN_POINT('Ctrl Pts',(-12.4998361945464,4.96019456459868,0.140287462424448));
#70730=CARTESIAN_POINT('Ctrl Pts',(-12.5395915186855,5.00662657302196,-1.50142585838318));
#70731=CARTESIAN_POINT('Ctrl Pts',(-12.5793468428246,4.15708131363603,-3.16847979348607));
#70732=CARTESIAN_POINT('Ctrl Pts',(-12.6191021669636,2.80149265219899,-4.09571112390302));
#70733=CARTESIAN_POINT('Ctrl Pts',(-12.6588574911027,1.44590399076196,-5.02294245431997));
#70734=CARTESIAN_POINT('Ctrl Pts',(-12.6986128152417,-0.415728072726164,
-5.21035118005097));
#70735=CARTESIAN_POINT('Ctrl Pts',(-12.7383681393808,-1.9289306551374,-4.57191833024815));
#70736=CARTESIAN_POINT('Ctrl Pts',(-12.7781234635198,-3.44213323754866,
-3.93348548044531));
#70737=CARTESIAN_POINT('Ctrl Pts',(-12.8178787876589,-4.60690633888303,
-2.46921105510862));
#70738=CARTESIAN_POINT('Ctrl Pts',(-12.8576341117979,-4.88862926281331,
-0.851184246537236));
#70739=CARTESIAN_POINT('Ctrl Pts',(-12.8644931704839,-4.93723543343982,
-0.572023125963481));
#70740=CARTESIAN_POINT('Ctrl Pts',(-12.8713522291698,-4.9595556453203,-0.288285222658431));
#70741=CARTESIAN_POINT('Ctrl Pts',(-12.8782112878558,-4.9570073981747,-0.00414712514969162));
#70742=CARTESIAN_POINT('Ctrl Pts',(-12.9835887121441,-4.95857558632536,
-0.00363955744209949));
#70743=CARTESIAN_POINT('Ctrl Pts',(-12.9780681666729,-4.9604577900947,-0.232141689801689));
#70744=CARTESIAN_POINT('Ctrl Pts',(-12.9725476212018,-4.94603397597445,
-0.46040490726145));
#70745=CARTESIAN_POINT('Ctrl Pts',(-12.9670270757306,-4.91449226833891,
-0.686277719308069));
#70746=CARTESIAN_POINT('Ctrl Pts',(-12.9272717515915,-4.68734971195556,
-2.31286460352462));
#70747=CARTESIAN_POINT('Ctrl Pts',(-12.8875164274525,-3.57248525315302,
-3.81548674645999));
#70748=CARTESIAN_POINT('Ctrl Pts',(-12.8477611033134,-2.08161195655509,
-4.5044536878415));
#70749=CARTESIAN_POINT('Ctrl Pts',(-12.8080057791744,-0.590738659957164,
-5.19342062922301));
#70750=CARTESIAN_POINT('Ctrl Pts',(-12.7682504550353,1.27614347443615,-5.06873236905063));
#70751=CARTESIAN_POINT('Ctrl Pts',(-12.7284951308963,2.66215182673351,-4.18761973142282));
#70752=CARTESIAN_POINT('Ctrl Pts',(-12.6887398067572,4.04816017903089,-3.30650709379501));
#70753=CARTESIAN_POINT('Ctrl Pts',(-12.6489844826182,4.95329474923234,-1.66897007871172));
#70754=CARTESIAN_POINT('Ctrl Pts',(-12.6092291584791,4.9621066626716,-0.0266238962620294));
#70755=CARTESIAN_POINT('Ctrl Pts',(-12.56947383434,4.97091857611086,1.61572228618765));
#70756=CARTESIAN_POINT('Ctrl Pts',(-12.529718510201,4.08340783278798,3.26287763600375));
#70757=CARTESIAN_POINT('Ctrl Pts',(-12.4899631860619,2.70693412451721,4.15881221132986));
#70758=CARTESIAN_POINT('Ctrl Pts',(-12.4502078619229,1.33046041624645,5.05474678665596));
#70759=CARTESIAN_POINT('Ctrl Pts',(-12.4104525377838,-0.534976256972191,
5.19946058749209));
#70760=CARTESIAN_POINT('Ctrl Pts',(-12.3706972136448,-2.0331567293218,4.52653124120398));
#70761=CARTESIAN_POINT('Ctrl Pts',(-12.3309418895057,-3.53133720167143,
3.85360189491585));
#70762=CARTESIAN_POINT('Ctrl Pts',(-12.2911865653667,-4.66226147315203,
2.36302940150349));
#70763=CARTESIAN_POINT('Ctrl Pts',(-12.2514312412276,-4.9068451651669,0.738973537185428));
#70764=CARTESIAN_POINT('Ctrl Pts',(-12.2454837315331,-4.9434355819445,0.496010155383642));
#70765=CARTESIAN_POINT('Ctrl Pts',(-12.2395362218386,-4.9601887995945,0.250059280658444));
#70766=CARTESIAN_POINT('Ctrl Pts',(-12.2335887121441,-4.95809108523107,
0.00382194074085128));
#70767=CARTESIAN_POINT('Origin',(10.45,0.,0.));
#70768=CARTESIAN_POINT('',(-11.3782112878558,-4.94702647513278,0.00247992552970894));
#70769=CARTESIAN_POINT('',(-11.4835887121441,-4.94632723583785,0.00165774955501003));
#70770=CARTESIAN_POINT('',(10.45,-4.954,-6.06690024297599E-16));
#70771=CARTESIAN_POINT('Ctrl Pts',(-11.3782112878558,-4.94702647513278,
0.00247992552970894));
#70772=CARTESIAN_POINT('Ctrl Pts',(-11.3942883395012,-4.95004983254863,
0.671894317539847));
#70773=CARTESIAN_POINT('Ctrl Pts',(-11.4103653911466,-4.82370826570512,
1.340215185172));
#70774=CARTESIAN_POINT('Ctrl Pts',(-11.426442442792,-4.56258483798423,1.95090499178823));
#70775=CARTESIAN_POINT('Ctrl Pts',(-11.466197766931,-3.91687897484982,3.46101839727712));
#70776=CARTESIAN_POINT('Ctrl Pts',(-11.5059530910701,-2.44701747748665,
4.61873302051397));
#70777=CARTESIAN_POINT('Ctrl Pts',(-11.5457084152091,-0.827653955533048,
4.8926679450662));
#70778=CARTESIAN_POINT('Ctrl Pts',(-11.5854637393482,0.791709566420588,
5.16660286961844));
#70779=CARTESIAN_POINT('Ctrl Pts',(-11.6252190634872,2.56057511296464,4.55675809548603));
#70780=CARTESIAN_POINT('Ctrl Pts',(-11.6649743876263,3.66704882329549,3.34304705595883));
#70781=CARTESIAN_POINT('Ctrl Pts',(-11.7047297117653,4.77352253362632,2.12933601643165));
#70782=CARTESIAN_POINT('Ctrl Pts',(-11.7444850359044,5.21760440774395,0.311758711509695));
#70783=CARTESIAN_POINT('Ctrl Pts',(-11.7842403600434,4.79546473796103,-1.27543272568967));
#70784=CARTESIAN_POINT('Ctrl Pts',(-11.8239956841825,4.37332506817812,-2.86262416288903));
#70785=CARTESIAN_POINT('Ctrl Pts',(-11.8637510083216,3.08496385449466,-4.21942973236582));
#70786=CARTESIAN_POINT('Ctrl Pts',(-11.9035063324606,1.52172765907916,-4.72308750949856));
#70787=CARTESIAN_POINT('Ctrl Pts',(-11.9432616565997,-0.0415085363363632,
-5.2267452866313));
#70788=CARTESIAN_POINT('Ctrl Pts',(-11.9830169807387,-1.87961971348394,
-4.87725527141997));
#70789=CARTESIAN_POINT('Ctrl Pts',(-12.0227723048778,-3.14892887095642,
-3.83503033318447));
#70790=CARTESIAN_POINT('Ctrl Pts',(-12.0579186325371,-4.27108185337152,
-2.91363477253381));
#70791=CARTESIAN_POINT('Ctrl Pts',(-12.0930649601964,-4.94867477893918,
-1.45081659714675));
#70792=CARTESIAN_POINT('Ctrl Pts',(-12.1282112878558,-4.95954504035343,
0.00318967636549851));
#70793=CARTESIAN_POINT('Ctrl Pts',(-12.2335887121441,-4.95809108523107,
0.00382194074085128));
#70794=CARTESIAN_POINT('Ctrl Pts',(-12.1997808976995,-4.94616691165269,
-1.39588091387461));
#70795=CARTESIAN_POINT('Ctrl Pts',(-12.165973083255,-4.32513137411095,-2.80484003252773));
#70796=CARTESIAN_POINT('Ctrl Pts',(-12.1321652688104,-3.2761353178338,-3.72694898580919));
#70797=CARTESIAN_POINT('Ctrl Pts',(-12.0924099446714,-2.04259866593666,
-4.81127640926203));
#70798=CARTESIAN_POINT('Ctrl Pts',(-12.0526546205323,-0.217282249593205,
-5.22239202094398));
#70799=CARTESIAN_POINT('Ctrl Pts',(-12.0128992963933,1.36200961342418,-4.77159734014955));
#70800=CARTESIAN_POINT('Ctrl Pts',(-11.9731439722542,2.94130147644158,-4.32080265935511));
#70801=CARTESIAN_POINT('Ctrl Pts',(-11.9333886481152,4.27456878613291,-3.00809768608432));
#70802=CARTESIAN_POINT('Ctrl Pts',(-11.8936333239761,4.74985347385727,-1.43600255587105));
#70803=CARTESIAN_POINT('Ctrl Pts',(-11.8538779998371,5.22513816158162,0.136092574342198));
#70804=CARTESIAN_POINT('Ctrl Pts',(-11.814122675698,4.842440227339,1.96757786149789));
#70805=CARTESIAN_POINT('Ctrl Pts',(-11.7743673515589,3.77741468570125,3.21781752991537));
#70806=CARTESIAN_POINT('Ctrl Pts',(-11.7346120274199,2.71238914406348,4.46805719833287));
#70807=CARTESIAN_POINT('Ctrl Pts',(-11.6948567032808,0.965035995030541,
5.13705124801214));
#70808=CARTESIAN_POINT('Ctrl Pts',(-11.6551013791418,-0.662624903456663,
4.91773724398744));
#70809=CARTESIAN_POINT('Ctrl Pts',(-11.6153460550027,-2.29028580194385,
4.69842323996274));
#70810=CARTESIAN_POINT('Ctrl Pts',(-11.5755907308637,-3.79825444988532,
3.59080118223412));
#70811=CARTESIAN_POINT('Ctrl Pts',(-11.5358354067246,-4.49438638783357,
2.10325993648869));
#70812=CARTESIAN_POINT('Ctrl Pts',(-11.5184198418644,-4.79934003062556,
1.45161461328974));
#70813=CARTESIAN_POINT('Ctrl Pts',(-11.5010042770043,-4.94849878013362,
0.727061193394733));
#70814=CARTESIAN_POINT('Ctrl Pts',(-11.4835887121441,-4.94632723583785,
0.00165774955501003));
#70815=CARTESIAN_POINT('Origin',(10.45,0.,0.));
#70816=CARTESIAN_POINT('',(-10.6282112878558,-4.95044820539071,-0.00419555124727688));
#70817=CARTESIAN_POINT('',(-10.7335887121441,-4.95199589610219,-0.00447753941358037));
#70818=CARTESIAN_POINT('',(10.45,-4.954,-6.06690024297599E-16));
#70819=CARTESIAN_POINT('Ctrl Pts',(-10.6282112878558,-4.95044820539071,
-0.00419555124727689));
#70820=CARTESIAN_POINT('Ctrl Pts',(-10.6557563946668,-4.94128684808288,
1.14073304265234));
#70821=CARTESIAN_POINT('Ctrl Pts',(-10.6833015014779,-4.54618067767775,
2.29136724379881));
#70822=CARTESIAN_POINT('Ctrl Pts',(-10.710846608289,-3.81983564793575,3.1673437315118));
#70823=CARTESIAN_POINT('Ctrl Pts',(-10.750601932428,-2.77151580324431,4.43162378844124));
#70824=CARTESIAN_POINT('Ctrl Pts',(-10.7903572565671,-1.03320570459301,
5.12377548511912));
#70825=CARTESIAN_POINT('Ctrl Pts',(-10.8301125807061,0.597225471344212,
4.92610722854929));
#70826=CARTESIAN_POINT('Ctrl Pts',(-10.8698679048452,2.22765664728147,4.72843897197945));
#70827=CARTESIAN_POINT('Ctrl Pts',(-10.9096232289842,3.75020890050466,3.64095076216186));
#70828=CARTESIAN_POINT('Ctrl Pts',(-10.9493785531233,4.46604402391554,2.16279020416594));
#70829=CARTESIAN_POINT('Ctrl Pts',(-10.9891338772624,5.18187914732642,0.684629646170029));
#70830=CARTESIAN_POINT('Ctrl Pts',(-11.0288892014014,5.09099714092502,-1.1842032600042));
#70831=CARTESIAN_POINT('Ctrl Pts',(-11.0686445255405,4.2351120531301,-2.58593050722946));
#70832=CARTESIAN_POINT('Ctrl Pts',(-11.1083998496795,3.37922696533518,-3.98765775445471));
#70833=CARTESIAN_POINT('Ctrl Pts',(-11.1481551738186,1.75833879614674,-4.92227934273101));
#70834=CARTESIAN_POINT('Ctrl Pts',(-11.1879104979576,0.11642108057116,-4.96081211323171));
#70835=CARTESIAN_POINT('Ctrl Pts',(-11.2276658220967,-1.52549663500446,
-4.99934488373241));
#70836=CARTESIAN_POINT('Ctrl Pts',(-11.2674211462357,-3.18844389696722,
-4.14178883645749));
#70837=CARTESIAN_POINT('Ctrl Pts',(-11.3071764703748,-4.10914241349577,
-2.78175471894954));
#70838=CARTESIAN_POINT('Ctrl Pts',(-11.3308547428684,-4.65751048320689,
-1.971718349421));
#70839=CARTESIAN_POINT('Ctrl Pts',(-11.3545330153621,-4.94257367605512,
-0.983433209217081));
#70840=CARTESIAN_POINT('Ctrl Pts',(-11.3782112878558,-4.94702647513278,
0.00247992552970894));
#70841=CARTESIAN_POINT('Ctrl Pts',(-11.4835887121441,-4.94632723583785,
0.00165774955501003));
#70842=CARTESIAN_POINT('Ctrl Pts',(-11.4612489528652,-4.94354169444311,
-0.928851162762755));
#70843=CARTESIAN_POINT('Ctrl Pts',(-11.4389091935863,-4.69175135052043,
-1.86075873782794));
#70844=CARTESIAN_POINT('Ctrl Pts',(-11.4165694343075,-4.20037955308557,
-2.64197331053946));
#70845=CARTESIAN_POINT('Ctrl Pts',(-11.3768141101684,-3.32594555243426,
-4.03220487805994));
#70846=CARTESIAN_POINT('Ctrl Pts',(-11.3370587860293,-1.69278232317659,
-4.94520757933866));
#70847=CARTESIAN_POINT('Ctrl Pts',(-11.2973034618903,-0.0504975458483708,
-4.96192113615739));
#70848=CARTESIAN_POINT('Ctrl Pts',(-11.2575481377512,1.59178723147983,-4.97863469297612));
#70849=CARTESIAN_POINT('Ctrl Pts',(-11.2177928136122,3.24319355687857,-4.0990591053349));
#70850=CARTESIAN_POINT('Ctrl Pts',(-11.1780374894731,4.14574032776884,-2.72691189778716));
#70851=CARTESIAN_POINT('Ctrl Pts',(-11.1382821653341,5.04828709865911,-1.35476469023944));
#70852=CARTESIAN_POINT('Ctrl Pts',(-11.098526841195,5.20197431504088,0.509954137214785));
#70853=CARTESIAN_POINT('Ctrl Pts',(-11.058771517056,4.53626088479547,2.01135490370464));
#70854=CARTESIAN_POINT('Ctrl Pts',(-11.0190161929169,3.87054745455005,3.51275567019453));
#70855=CARTESIAN_POINT('Ctrl Pts',(-10.9792608687779,2.38543337767741,4.65083837572004));
#70856=CARTESIAN_POINT('Ctrl Pts',(-10.9395055446388,0.762573064803474,
4.90323298288164));
#70857=CARTESIAN_POINT('Ctrl Pts',(-10.8997502204998,-0.86028724807043,
5.15562759004323));
#70858=CARTESIAN_POINT('Ctrl Pts',(-10.8599948963607,-2.62089379694564,
4.52233409884093));
#70859=CARTESIAN_POINT('Ctrl Pts',(-10.8202395722216,-3.71114352892745,
3.29402869921955));
#70860=CARTESIAN_POINT('Ctrl Pts',(-10.7913559521958,-4.5032477231154,2.40162228054039));
#70861=CARTESIAN_POINT('Ctrl Pts',(-10.7624723321699,-4.94150234199152,
1.19513729087675));
#70862=CARTESIAN_POINT('Ctrl Pts',(-10.7335887121441,-4.95199589610219,
-0.00447753941358037));
#70863=CARTESIAN_POINT('Origin',(10.45,0.,0.));
#70864=CARTESIAN_POINT('',(-9.87821128785577,-4.96209602020563,-0.000574989514468549));
#70865=CARTESIAN_POINT('',(-9.98358871214408,-4.96212480437208,0.0004625561064964));
#70866=CARTESIAN_POINT('',(10.45,-4.954,-6.06690024297599E-16));
#70867=CARTESIAN_POINT('Ctrl Pts',(-9.87821128785577,-4.96209602020563,
-0.000574989514468549));
#70868=CARTESIAN_POINT('Ctrl Pts',(-9.9172244498325,-4.9594571116787,1.61120643364145));
#70869=CARTESIAN_POINT('Ctrl Pts',(-9.95623761180925,-4.10092863156834,
3.22539966553874));
#70870=CARTESIAN_POINT('Ctrl Pts',(-9.99525077378598,-2.76195239279821,
4.12247858341363));
#70871=CARTESIAN_POINT('Ctrl Pts',(-10.035006097925,-1.39750430170163,5.03662297344527));
#70872=CARTESIAN_POINT('Ctrl Pts',(-10.0747614220641,0.465844896295108,
5.20610965909354));
#70873=CARTESIAN_POINT('Ctrl Pts',(-10.1145167462031,1.97283416829854,4.55314572962272));
#70874=CARTESIAN_POINT('Ctrl Pts',(-10.1542720703422,3.479823440302,3.9001818001519));
#70875=CARTESIAN_POINT('Ctrl Pts',(-10.1940273944813,4.63045278631214,2.42476725556195));
#70876=CARTESIAN_POINT('Ctrl Pts',(-10.2337827186203,4.8965933703576,0.804104505744015));
#70877=CARTESIAN_POINT('Ctrl Pts',(-10.2735380427594,5.16273395440306,-0.8165582440739));
#70878=CARTESIAN_POINT('Ctrl Pts',(-10.3132933668984,4.54438577648385,-2.58246919911981));
#70879=CARTESIAN_POINT('Ctrl Pts',(-10.3530486910375,3.32536525807565,-3.68309063032276));
#70880=CARTESIAN_POINT('Ctrl Pts',(-10.3928040151765,2.10634473966745,-4.7837120615257));
#70881=CARTESIAN_POINT('Ctrl Pts',(-10.4325593393156,0.286651880770261,
-5.2190439688857));
#70882=CARTESIAN_POINT('Ctrl Pts',(-10.4723146634546,-1.29849016467224,
-4.7892728031547));
#70883=CARTESIAN_POINT('Ctrl Pts',(-10.5120699875937,-2.88363221011477,
-4.3595016374237));
#70884=CARTESIAN_POINT('Ctrl Pts',(-10.5518253117327,-4.2342234421026,-3.06462739860169));
#70885=CARTESIAN_POINT('Ctrl Pts',(-10.5915806358718,-4.7303542627307,-1.49898607060017));
#70886=CARTESIAN_POINT('Ctrl Pts',(-10.6037908531998,-4.88273297612754,
-1.01812416627471));
#70887=CARTESIAN_POINT('Ctrl Pts',(-10.6160010705278,-4.95450925930186,
-0.511720428621469));
#70888=CARTESIAN_POINT('Ctrl Pts',(-10.6282112878558,-4.95044820539071,
-0.00419555124727689));
#70889=CARTESIAN_POINT('Ctrl Pts',(-10.7335887121441,-4.95199589610219,
-0.00447753941358037));
#70890=CARTESIAN_POINT('Ctrl Pts',(-10.7227170080309,-4.95594563700326,
-0.456008804298611));
#70891=CARTESIAN_POINT('Ctrl Pts',(-10.7118453039177,-4.89929249921127,
-0.90656674208727));
#70892=CARTESIAN_POINT('Ctrl Pts',(-10.7009735998045,-4.77809508776449,
-1.33903648040781));
#70893=CARTESIAN_POINT('Ctrl Pts',(-10.6612182756654,-4.3349039995313,-2.92047895237324));
#70894=CARTESIAN_POINT('Ctrl Pts',(-10.6214629515264,-3.02862890797651,
-4.26004658826364));
#70895=CARTESIAN_POINT('Ctrl Pts',(-10.5817076273873,-1.45883868899695,
-4.74288952465349));
#70896=CARTESIAN_POINT('Ctrl Pts',(-10.5419523032482,0.110951529982599,
-5.22573246104334));
#70897=CARTESIAN_POINT('Ctrl Pts',(-10.5021969791092,1.94425687638693,-4.85185069793267));
#70898=CARTESIAN_POINT('Ctrl Pts',(-10.4624416549701,3.1996061832117,-3.79285270422351));
#70899=CARTESIAN_POINT('Ctrl Pts',(-10.4226863308311,4.45495549003649,-2.73385471051433));
#70900=CARTESIAN_POINT('Ctrl Pts',(-10.382931006692,5.13234875728171,-0.989740486206656));
#70901=CARTESIAN_POINT('Ctrl Pts',(-10.343175682553,4.92086838236267,0.638956748963116));
#70902=CARTESIAN_POINT('Ctrl Pts',(-10.3034203584139,4.70938800744364,2.26765398413285));
#70903=CARTESIAN_POINT('Ctrl Pts',(-10.2636650342749,3.60903399036037,3.78093423016469));
#70904=CARTESIAN_POINT('Ctrl Pts',(-10.2239097101358,2.12485922952337,4.48421505040642));
#70905=CARTESIAN_POINT('Ctrl Pts',(-10.1841543859968,0.640684468686361,
5.18749587064816));
#70906=CARTESIAN_POINT('Ctrl Pts',(-10.1443990618577,-1.22731103590437,
5.08077726509979));
#70907=CARTESIAN_POINT('Ctrl Pts',(-10.1046437377186,-2.62173363714599,
4.21304214308846));
#70908=CARTESIAN_POINT('Ctrl Pts',(-10.0648884135796,-4.01615623838763,
3.34530702107711));
#70909=CARTESIAN_POINT('Ctrl Pts',(-10.0251330894405,-4.93700593628012,
1.71655538260276));
#70910=CARTESIAN_POINT('Ctrl Pts',(-9.98537776530148,-4.9616207495878,0.0743700265021302));
#70911=CARTESIAN_POINT('Ctrl Pts',(-9.98478141424902,-4.9619899849076,0.0497363708430052));
#70912=CARTESIAN_POINT('Ctrl Pts',(-9.98418506319655,-4.96215755304679,
0.0250996923825981));
#70913=CARTESIAN_POINT('Ctrl Pts',(-9.98358871214408,-4.96212480437208,
0.0004625561064964));
#70914=CARTESIAN_POINT('Origin',(10.45,0.,0.));
#70915=CARTESIAN_POINT('',(-9.12821128785577,-4.95217176878245,0.00449694065580375));
#70916=CARTESIAN_POINT('',(-9.23358871214408,-4.95061007082821,0.00423510493672524));
#70917=CARTESIAN_POINT('',(10.45,-4.954,-6.06690024297599E-16));
#70918=CARTESIAN_POINT('Ctrl Pts',(-9.12821128785577,-4.95217176878245,
0.00449694065580375));
#70919=CARTESIAN_POINT('Ctrl Pts',(-9.13893718085912,-4.95609640839351,
0.449932082821765));
#70920=CARTESIAN_POINT('Ctrl Pts',(-9.14966307386248,-4.90097753069107,
0.894412768863136));
#70921=CARTESIAN_POINT('Ctrl Pts',(-9.16038896686583,-4.78297000480896,
1.32151754581074));
#70922=CARTESIAN_POINT('Ctrl Pts',(-9.20014429100488,-4.34557729160315,
2.90457350614757));
#70923=CARTESIAN_POINT('Ctrl Pts',(-9.23989961514394,-3.0442200017842,4.24891913675094));
#70924=CARTESIAN_POINT('Ctrl Pts',(-9.27965493928299,-1.47620978313698,
4.73751151628769));
#70925=CARTESIAN_POINT('Ctrl Pts',(-9.31941026342205,0.0918004355102117,
5.22610389582444));
#70926=CARTESIAN_POINT('Ctrl Pts',(-9.3591655875611,1.92646358298569,4.85894302429461));
#70927=CARTESIAN_POINT('Ctrl Pts',(-9.39892091170016,3.18568527343389,3.8045525399729));
#70928=CARTESIAN_POINT('Ctrl Pts',(-9.43867623583921,4.4449069638821,2.7501620556512));
#70929=CARTESIAN_POINT('Ctrl Pts',(-9.47843155997827,5.12868719730307,1.00854195853761));
#70930=CARTESIAN_POINT('Ctrl Pts',(-9.51818688411732,4.92317680933377,-0.620919314263967));
#70931=CARTESIAN_POINT('Ctrl Pts',(-9.55794220825638,4.71766642136447,-2.25038058706556));
#70932=CARTESIAN_POINT('Ctrl Pts',(-9.59769753239543,3.62286541200492,-3.7676830355551));
#70933=CARTESIAN_POINT('Ctrl Pts',(-9.63745285653448,2.14127789754436,-4.47639806722725));
#70934=CARTESIAN_POINT('Ctrl Pts',(-9.67720818067354,0.659690383083816,
-5.18511309889938));
#70935=CARTESIAN_POINT('Ctrl Pts',(-9.7169635048126,-1.20868363647773,-5.08524071375409));
#70936=CARTESIAN_POINT('Ctrl Pts',(-9.75671882895165,-2.60627677896655,
-4.22262146565467));
#70937=CARTESIAN_POINT('Ctrl Pts',(-9.79647415309071,-4.0038699214554,-3.36000221755523));
#70938=CARTESIAN_POINT('Ctrl Pts',(-9.83622947722975,-4.93068218687153,
-1.73463610650163));
#70939=CARTESIAN_POINT('Ctrl Pts',(-9.87598480136881,-4.96131482748137,
-0.0925520037673158));
#70940=CARTESIAN_POINT('Ctrl Pts',(-9.87672696353113,-4.96188668514534,
-0.0618971741366425));
#70941=CARTESIAN_POINT('Ctrl Pts',(-9.87746912569345,-4.96214622116242,
-0.0312365182290158));
#70942=CARTESIAN_POINT('Ctrl Pts',(-9.87821128785577,-4.96209602020563,
-0.000574989514468549));
#70943=CARTESIAN_POINT('Ctrl Pts',(-9.98358871214408,-4.96212480437208,
0.0004625561064964));
#70944=CARTESIAN_POINT('Ctrl Pts',(-9.94442973905749,-4.9599743856448,-1.61731769660458));
#70945=CARTESIAN_POINT('Ctrl Pts',(-9.9052707659709,-4.09409792840036,-3.23707195902456));
#70946=CARTESIAN_POINT('Ctrl Pts',(-9.86611179288432,-2.7468265476734,-4.13257247735339));
#70947=CARTESIAN_POINT('Ctrl Pts',(-9.82635646874526,-1.3790376037284,-5.04171055138142));
#70948=CARTESIAN_POINT('Ctrl Pts',(-9.78660114460621,0.484920212884461,
-5.20436762571052));
#70949=CARTESIAN_POINT('Ctrl Pts',(-9.74684582046715,1.98950651863428,-4.54588552164414));
#70950=CARTESIAN_POINT('Ctrl Pts',(-9.7070904963281,3.49409282438405,-3.88740341757779));
#70951=CARTESIAN_POINT('Ctrl Pts',(-9.66733517218905,4.63930761927079,-2.40778213511593));
#70952=CARTESIAN_POINT('Ctrl Pts',(-9.62757984804999,4.89950729907218,-0.786154940148899));
#70953=CARTESIAN_POINT('Ctrl Pts',(-9.58782452391094,5.15970697887357,0.835472254818157));
#70954=CARTESIAN_POINT('Ctrl Pts',(-9.54806919977187,4.53489154358963,2.59910536229043));
#70955=CARTESIAN_POINT('Ctrl Pts',(-9.50831387563282,3.3118458294299,3.69525216536976));
#70956=CARTESIAN_POINT('Ctrl Pts',(-9.46855855149377,2.08880011527016,4.79139896844909));
#70957=CARTESIAN_POINT('Ctrl Pts',(-9.42880322735472,0.267524122234651,
5.22005946713543));
#70958=CARTESIAN_POINT('Ctrl Pts',(-9.38904790321567,-1.31603235096888,
4.78448223058519));
#70959=CARTESIAN_POINT('Ctrl Pts',(-9.34929257907661,-2.89958882417239,
4.34890499403496));
#70960=CARTESIAN_POINT('Ctrl Pts',(-9.30953725493755,-4.2454257775439,3.04909002224817));
#70961=CARTESIAN_POINT('Ctrl Pts',(-9.26978193079849,-4.73581578560452,
1.4816410524824));
#70962=CARTESIAN_POINT('Ctrl Pts',(-9.25771752458035,-4.88463268977224,
1.00597291225268));
#70963=CARTESIAN_POINT('Ctrl Pts',(-9.24565311836222,-4.95466988245972,
0.505657855859816));
#70964=CARTESIAN_POINT('Ctrl Pts',(-9.23358871214408,-4.95061007082821,
0.00423510493672523));
#70965=CARTESIAN_POINT('Origin',(10.45,0.,0.));
#70966=CARTESIAN_POINT('',(-8.37821128785577,-4.94626828646249,-0.0015636080438286));
#70967=CARTESIAN_POINT('',(-8.48358871214408,-4.94693680463334,-0.00239458277972477));
#70968=CARTESIAN_POINT('',(10.45,-4.954,-6.06690024297599E-16));
#70969=CARTESIAN_POINT('Ctrl Pts',(-8.37821128785577,-4.94626828646249,
-0.0015636080438286));
#70970=CARTESIAN_POINT('Ctrl Pts',(-8.4004052360248,-4.94365983576389,0.922899349173829));
#70971=CARTESIAN_POINT('Ctrl Pts',(-8.42259918419382,-4.69535029940576,
1.84866339909468));
#70972=CARTESIAN_POINT('Ctrl Pts',(-8.44479313236284,-4.21003313165683,
2.62656271981837));
#70973=CARTESIAN_POINT('Ctrl Pts',(-8.4845484565019,-3.34069969142485,4.01998940566081));
#70974=CARTESIAN_POINT('Ctrl Pts',(-8.52430378064095,-1.71089326297385,
4.93897089408532));
#70975=CARTESIAN_POINT('Ctrl Pts',(-8.56405910478,-0.0686807845416902,4.96170269571067));
#70976=CARTESIAN_POINT('Ctrl Pts',(-8.60381442891905,1.57353169389047,4.98443449733603));
#70977=CARTESIAN_POINT('Ctrl Pts',(-8.64356975305811,3.22815022230378,4.11091661216223));
#70978=CARTESIAN_POINT('Ctrl Pts',(-8.68332507719717,4.13571932494693,2.74208613213524));
#70979=CARTESIAN_POINT('Ctrl Pts',(-8.72308040133623,5.04328842759009,1.37325565210822));
#70980=CARTESIAN_POINT('Ctrl Pts',(-8.76283572547528,5.20380810446308,-0.490887422771993));
#70981=CARTESIAN_POINT('Ctrl Pts',(-8.80259104961434,4.5436012236629,-1.99471767704526));
#70982=CARTESIAN_POINT('Ctrl Pts',(-8.84234637375339,3.88339434286273,-3.49854793131853));
#70983=CARTESIAN_POINT('Ctrl Pts',(-8.88210169789244,2.40246090438938,-4.64206536498485));
#70984=CARTESIAN_POINT('Ctrl Pts',(-8.9218570220315,0.780536442300002,-4.90040544782057));
#70985=CARTESIAN_POINT('Ctrl Pts',(-8.96161234617055,-0.841388019789334,
-5.15874553065628));
#70986=CARTESIAN_POINT('Ctrl Pts',(-9.0013676703096,-2.6043035054947,-4.53190826266146));
#70987=CARTESIAN_POINT('Ctrl Pts',(-9.04112299444866,-3.69904718005105,
-3.30760648362894));
#70988=CARTESIAN_POINT('Ctrl Pts',(-9.07015242558436,-4.49843158453039,
-2.41361844672019));
#70989=CARTESIAN_POINT('Ctrl Pts',(-9.09918185672007,-4.94154980422565,
-1.20106503734346));
#70990=CARTESIAN_POINT('Ctrl Pts',(-9.12821128785577,-4.95217176878245,
0.00449694065580375));
#70991=CARTESIAN_POINT('Ctrl Pts',(-9.23358871214408,-4.95061007082821,
0.00423510493672523));
#70992=CARTESIAN_POINT('Ctrl Pts',(-9.20589779422316,-4.9412917580468,-1.14665918595834));
#70993=CARTESIAN_POINT('Ctrl Pts',(-9.17820687630225,-4.54161511541906,
-2.30338904052803));
#70994=CARTESIAN_POINT('Ctrl Pts',(-9.15051595838133,-3.80820292464108,
-3.18132077105363));
#70995=CARTESIAN_POINT('Ctrl Pts',(-9.11076063424228,-2.75525699286724,
-4.44175065707925));
#70996=CARTESIAN_POINT('Ctrl Pts',(-9.07100531010322,-1.01442206656976,
-5.12752746138567));
#70997=CARTESIAN_POINT('Ctrl Pts',(-9.03124998596417,0.615273803705024,
-4.92388561098412));
#70998=CARTESIAN_POINT('Ctrl Pts',(-8.99149466182511,2.24496967397974,-4.72024376058259));
#70999=CARTESIAN_POINT('Ctrl Pts',(-8.95173933768606,3.76352648823178,-3.62718325547323));
#71000=CARTESIAN_POINT('Ctrl Pts',(-8.911984013547,4.47393991100926,-2.14640933567216));
#71001=CARTESIAN_POINT('Ctrl Pts',(-8.87222868940795,5.18435333378674,-0.665635415871093));
#71002=CARTESIAN_POINT('Ctrl Pts',(-8.83247336526889,5.08662336508962,1.20285191862169));
#71003=CARTESIAN_POINT('Ctrl Pts',(-8.79271804112984,4.22560720831403,2.60143327506715));
#71004=CARTESIAN_POINT('Ctrl Pts',(-8.75296271699079,3.36459105153842,4.00001463151265));
#71005=CARTESIAN_POINT('Ctrl Pts',(-8.71320739285173,1.74028870668433,4.92869000991082));
#71006=CARTESIAN_POINT('Ctrl Pts',(-8.67345206871267,0.0982407856159575,
4.96120550991629));
#71007=CARTESIAN_POINT('Ctrl Pts',(-8.63369674457362,-1.54380713545237,
4.99372100992175));
#71008=CARTESIAN_POINT('Ctrl Pts',(-8.59394142043456,-3.20360063273498,
4.13007663153452));
#71009=CARTESIAN_POINT('Ctrl Pts',(-8.5541860962955,-4.11930896489686,2.76667761318562));
#71010=CARTESIAN_POINT('Ctrl Pts',(-8.53065363491169,-4.66134632547929,
1.95963766457907));
#71011=CARTESIAN_POINT('Ctrl Pts',(-8.50712117352789,-4.942668242245,0.977491748450743));
#71012=CARTESIAN_POINT('Ctrl Pts',(-8.48358871214408,-4.94693680463334,
-0.00239458277972477));
#71013=CARTESIAN_POINT('Origin',(10.45,0.,0.));
#71014=CARTESIAN_POINT('',(-7.62821128785578,-4.95792182903176,-0.00387990541073024));
#71015=CARTESIAN_POINT('',(-7.73358871214408,-4.95939673491496,-0.00326695968845118));
#71016=CARTESIAN_POINT('',(10.45,-4.954,-6.06690024297599E-16));
#71017=CARTESIAN_POINT('Ctrl Pts',(-7.62821128785578,-4.95792182903176,
-0.00387990541073024));
#71018=CARTESIAN_POINT('Ctrl Pts',(-7.66187329119047,-4.94592861234691,
1.38990971447958));
#71019=CARTESIAN_POINT('Ctrl Pts',(-7.69553529452516,-4.33087130523565,
2.79296473185555));
#71020=CARTESIAN_POINT('Ctrl Pts',(-7.72919729785985,-3.28977114370411,
3.71491810311339));
#71021=CARTESIAN_POINT('Ctrl Pts',(-7.76895262199891,-2.0602164445561,4.80375867956457));
#71022=CARTESIAN_POINT('Ctrl Pts',(-7.80870794613796,-0.236418894111356,
5.22156062460434));
#71023=CARTESIAN_POINT('Ctrl Pts',(-7.84846327027702,1.34451433606028,4.77655648882291));
#71024=CARTESIAN_POINT('Ctrl Pts',(-7.88821859441607,2.92544756623186,4.33155235304148));
#71025=CARTESIAN_POINT('Ctrl Pts',(-7.92797391855513,4.26351647613036,3.02374213643891));
#71026=CARTESIAN_POINT('Ctrl Pts',(-7.96772924269418,4.74455910449121,1.45339932392216));
#71027=CARTESIAN_POINT('Ctrl Pts',(-8.00748456683323,5.22560173285208,-0.11694348859464));
#71028=CARTESIAN_POINT('Ctrl Pts',(-8.04723989097229,4.84961807967525,-1.94981889702563));
#71029=CARTESIAN_POINT('Ctrl Pts',(-8.08699521511134,3.78918136307401,-3.20395307214704));
#71030=CARTESIAN_POINT('Ctrl Pts',(-8.1267505392504,2.72874464647277,-4.45808724726844));
#71031=CARTESIAN_POINT('Ctrl Pts',(-8.16650586338946,0.983854866447135,
-5.13348018908026));
#71032=CARTESIAN_POINT('Ctrl Pts',(-8.20626118752851,-0.644598783955043,
-4.92013242692831));
#71033=CARTESIAN_POINT('Ctrl Pts',(-8.24601651166757,-2.27305243435722,
-4.70678466477637));
#71034=CARTESIAN_POINT('Ctrl Pts',(-8.28577183580661,-3.78506995513594,
-3.60469619866064));
#71035=CARTESIAN_POINT('Ctrl Pts',(-8.32552715994567,-4.48664848951884,
-2.11971602397259));
#71036=CARTESIAN_POINT('Ctrl Pts',(-8.3430885359157,-4.79656130450954,-1.46374614520803));
#71037=CARTESIAN_POINT('Ctrl Pts',(-8.36064991188574,-4.94833227179167,
-0.733062187675864));
#71038=CARTESIAN_POINT('Ctrl Pts',(-8.37821128785577,-4.94626828646249,
-0.0015636080438286));
#71039=CARTESIAN_POINT('Ctrl Pts',(-8.48358871214408,-4.94693680463334,
-0.00239458277972477));
#71040=CARTESIAN_POINT('Ctrl Pts',(-8.46736584938883,-4.94987947606319,
-0.677910892273384));
#71041=CARTESIAN_POINT('Ctrl Pts',(-8.45114298663359,-4.82115310072354,
-1.35235333861075));
#71042=CARTESIAN_POINT('Ctrl Pts',(-8.43492012387834,-4.55540492895606,
-1.96761207986355));
#71043=CARTESIAN_POINT('Ctrl Pts',(-8.39516479973929,-3.90416939381222,
-3.47534909625313));
#71044=CARTESIAN_POINT('Ctrl Pts',(-8.35540947560023,-2.43007515648339,
-4.62766947072172));
#71045=CARTESIAN_POINT('Ctrl Pts',(-8.31565415146118,-0.809718617341338,
-4.8956681999818));
#71046=CARTESIAN_POINT('Ctrl Pts',(-8.27589882732213,0.810637921800733,
-5.16366692924188));
#71047=CARTESIAN_POINT('Ctrl Pts',(-8.23614350318307,2.57725676275602,-4.54734401329347));
#71048=CARTESIAN_POINT('Ctrl Pts',(-8.19638817904401,3.6792752629942,-3.32958629602854));
#71049=CARTESIAN_POINT('Ctrl Pts',(-8.15663285490496,4.78129376323237,-2.11182857876362));
#71050=CARTESIAN_POINT('Ctrl Pts',(-8.1168775307659,5.21871192275341,-0.292636060182249));
#71051=CARTESIAN_POINT('Ctrl Pts',(-8.07712220662685,4.79075862076016,1.29299775761381));
#71052=CARTESIAN_POINT('Ctrl Pts',(-8.03736688248779,4.3628053187669,2.87863157540991));
#71053=CARTESIAN_POINT('Ctrl Pts',(-7.99761155834874,3.06948055525926,4.23070669242067));
#71054=CARTESIAN_POINT('Ctrl Pts',(-7.95785623420969,1.50440911849139,4.72863242045542));
#71055=CARTESIAN_POINT('Ctrl Pts',(-7.91810091007063,-0.060662318276431,
5.22655814849016));
#71056=CARTESIAN_POINT('Ctrl Pts',(-7.87834558593158,-1.89748042830445,
4.87033448754899));
#71057=CARTESIAN_POINT('Ctrl Pts',(-7.83859026179252,-3.16296171671753,
3.82346499162231));
#71058=CARTESIAN_POINT('Ctrl Pts',(-7.80358974524304,-4.27708918863134,
2.90180295236524));
#71059=CARTESIAN_POINT('Ctrl Pts',(-7.76858922869356,-4.94837290551537,
1.44482061973698));
#71060=CARTESIAN_POINT('Ctrl Pts',(-7.73358871214408,-4.95939673491496,
-0.00326695968845118));
#71061=CARTESIAN_POINT('Origin',(10.45,0.,0.));
#71062=CARTESIAN_POINT('',(-6.87821128785577,-4.9587369089069,0.00357303255080571));
#71063=CARTESIAN_POINT('',(-6.98358871214407,-4.95718456603373,0.00410112652448823));
#71064=CARTESIAN_POINT('',(10.45,-4.954,-6.06690024297599E-16));
#71065=CARTESIAN_POINT('Ctrl Pts',(-6.87821128785577,-4.9587369089069,0.00357303255080571));
#71066=CARTESIAN_POINT('Ctrl Pts',(-6.88358602221708,-4.9605454351019,0.226020979139462));
#71067=CARTESIAN_POINT('Ctrl Pts',(-6.88896075657839,-4.94687668270747,
0.448245317794466));
#71068=CARTESIAN_POINT('Ctrl Pts',(-6.8943354909397,-4.91697415180519,0.668263332278103));
#71069=CARTESIAN_POINT('Ctrl Pts',(-6.93409081507876,-4.69579395410926,
2.29567166434186));
#71070=CARTESIAN_POINT('Ctrl Pts',(-6.97384613921781,-3.58644354271542,
3.80236925676953));
#71071=CARTESIAN_POINT('Ctrl Pts',(-7.01360146335687,-2.09810508257134,
4.49679505351046));
#71072=CARTESIAN_POINT('Ctrl Pts',(-7.05335678749592,-0.609766622427246,
5.1912208502514));
#71073=CARTESIAN_POINT('Ctrl Pts',(-7.09311211163498,1.25755988646708,5.0733748513056));
#71074=CARTESIAN_POINT('Ctrl Pts',(-7.13286743577403,2.64678786019961,4.19734734253526));
#71075=CARTESIAN_POINT('Ctrl Pts',(-7.17262275991308,4.03601583393218,3.3213198337649));
#71076=CARTESIAN_POINT('Ctrl Pts',(-7.21237808405213,4.94714527250291,1.68711081516997));
#71077=CARTESIAN_POINT('Ctrl Pts',(-7.25213340819119,4.96197570894114,0.0448079754724352));
#71078=CARTESIAN_POINT('Ctrl Pts',(-7.29188873233025,4.97680614537936,-1.5974948642251));
#71079=CARTESIAN_POINT('Ctrl Pts',(-7.33164405646931,4.09533757968508,-3.24789152502519));
#71080=CARTESIAN_POINT('Ctrl Pts',(-7.37139938060836,2.72215639683076,-4.148864331595));
#71081=CARTESIAN_POINT('Ctrl Pts',(-7.41115470474741,1.34897521397647,-5.04983713816479));
#71082=CARTESIAN_POINT('Ctrl Pts',(-7.45091002888646,-0.515918586037916,
-5.20138609050432));
#71083=CARTESIAN_POINT('Ctrl Pts',(-7.49066535302552,-2.01655501146214,
-4.53395154104395));
#71084=CARTESIAN_POINT('Ctrl Pts',(-7.53042067716457,-3.51719143688638,
-3.86651699158356));
#71085=CARTESIAN_POINT('Ctrl Pts',(-7.57017600130363,-4.65357048772051,
-2.38009894032327));
#71086=CARTESIAN_POINT('Ctrl Pts',(-7.60993132544269,-4.90410408921195,
-0.756950310761838));
#71087=CARTESIAN_POINT('Ctrl Pts',(-7.61602464624705,-4.94250351467808,
-0.508169410913484));
#71088=CARTESIAN_POINT('Ctrl Pts',(-7.62211796705141,-4.96009277875244,
-0.25617645482694));
#71089=CARTESIAN_POINT('Ctrl Pts',(-7.62821128785578,-4.95792182903176,
-0.00387990541073024));
#71090=CARTESIAN_POINT('Ctrl Pts',(-7.73358871214408,-4.95939673491496,
-0.00326695968845118));
#71091=CARTESIAN_POINT('Ctrl Pts',(-7.72883390455451,-4.96089431817551,
-0.199989136725148));
#71092=CARTESIAN_POINT('Ctrl Pts',(-7.72407909696493,-4.95020672280133,
-0.396547159981269));
#71093=CARTESIAN_POINT('Ctrl Pts',(-7.71932428937536,-4.9267888600081,-0.591576615902107));
#71094=CARTESIAN_POINT('Ctrl Pts',(-7.6795689652363,-4.73099024808745,-2.22223339658757));
#71095=CARTESIAN_POINT('Ctrl Pts',(-7.63981364109725,-3.64524855744802,
-3.74603162704625));
#71096=CARTESIAN_POINT('Ctrl Pts',(-7.60005831695819,-2.16790975608666,
-4.46356120749413));
#71097=CARTESIAN_POINT('Ctrl Pts',(-7.56030299281914,-0.690570954725322,
-5.18109078794199));
#71098=CARTESIAN_POINT('Ctrl Pts',(-7.52054766868008,1.17836495735796,-5.09235171837907));
#71099=CARTESIAN_POINT('Ctrl Pts',(-7.48079234454102,2.58107269422186,-4.23807445790236));
#71100=CARTESIAN_POINT('Ctrl Pts',(-7.44103702040197,3.98378043108578,-3.38379719742564));
#71101=CARTESIAN_POINT('Ctrl Pts',(-7.40128169626292,4.92025999273031,-1.76398174603515));
#71102=CARTESIAN_POINT('Ctrl Pts',(-7.36152637212387,4.96067542675493,-0.122109270622357));
#71103=CARTESIAN_POINT('Ctrl Pts',(-7.32177104798481,5.00109086077955,1.51976320479041));
#71104=CARTESIAN_POINT('Ctrl Pts',(-7.28201572384575,4.14544216718425,3.18369270422544));
#71105=CARTESIAN_POINT('Ctrl Pts',(-7.2422603997067,2.78646463480541,4.10595009742701));
#71106=CARTESIAN_POINT('Ctrl Pts',(-7.20250507556765,1.42748710242655,5.0282074906286));
#71107=CARTESIAN_POINT('Ctrl Pts',(-7.16274975142859,-0.434819268735898,
5.20879277759671));
#71108=CARTESIAN_POINT('Ctrl Pts',(-7.12299442728954,-1.94567209421158,
4.56481888637309));
#71109=CARTESIAN_POINT('Ctrl Pts',(-7.08323910315048,-3.45652491968723,
3.92084499514948));
#71110=CARTESIAN_POINT('Ctrl Pts',(-7.04348377901142,-4.61592419947615,
2.45231192573416));
#71111=CARTESIAN_POINT('Ctrl Pts',(-7.00372845487237,-4.89171577447908,
0.83326355092171));
#71112=CARTESIAN_POINT('Ctrl Pts',(-6.99701520729627,-4.93828707436135,
0.559864382051187));
#71113=CARTESIAN_POINT('Ctrl Pts',(-6.99030195972017,-4.95966222198897,
0.282173255866473));
#71114=CARTESIAN_POINT('Ctrl Pts',(-6.98358871214407,-4.95718456603373,
0.00410112652448823));
#71115=CARTESIAN_POINT('Origin',(10.45,0.,0.));
#71116=CARTESIAN_POINT('',(-6.12821128785577,-4.94659179946477,0.00201959180113259));
#71117=CARTESIAN_POINT('',(-6.23358871214408,-4.94605717997479,0.00115570248479588));
#71118=CARTESIAN_POINT('',(10.45,-4.954,-6.06690024297599E-16));
#71119=CARTESIAN_POINT('Ctrl Pts',(-6.12821128785577,-4.94659179946477,
0.00201959180113259));
#71120=CARTESIAN_POINT('Ctrl Pts',(-6.14505407738275,-4.94915812932308,
0.703471731949359));
#71121=CARTESIAN_POINT('Ctrl Pts',(-6.16189686690973,-4.81001858480067,
1.40395201041217));
#71122=CARTESIAN_POINT('Ctrl Pts',(-6.17873965643671,-4.52419690513961,
2.03834566605201));
#71123=CARTESIAN_POINT('Ctrl Pts',(-6.21849498057577,-3.84955013699639,
3.53575352544014));
#71124=CARTESIAN_POINT('Ctrl Pts',(-6.25825030471482,-2.3576818810049,4.6649678881952));
#71125=CARTESIAN_POINT('Ctrl Pts',(-6.29800562885388,-0.733346657108161,
4.90768920891453));
#71126=CARTESIAN_POINT('Ctrl Pts',(-6.33776095299293,0.890988566788603,
5.15041052963386));
#71127=CARTESIAN_POINT('Ctrl Pts',(-6.37751627713199,2.6477907585907,4.50663880831747));
#71128=CARTESIAN_POINT('Ctrl Pts',(-6.41727160127105,3.73070303212477,3.2718596511591));
#71129=CARTESIAN_POINT('Ctrl Pts',(-6.4570269254101,4.81361530565883,2.03708049400074));
#71130=CARTESIAN_POINT('Ctrl Pts',(-6.49678224954915,5.22263766092491,0.211293901000479));
#71131=CARTESIAN_POINT('Ctrl Pts',(-6.5365375736882,4.7700324036586,-1.36748000308405));
#71132=CARTESIAN_POINT('Ctrl Pts',(-6.57629289782726,4.3174271463923,-2.94625390716858));
#71133=CARTESIAN_POINT('Ctrl Pts',(-6.61604822196632,3.00319427659351,-4.27801512233737));
#71134=CARTESIAN_POINT('Ctrl Pts',(-6.65580354610537,1.43055522097884,-4.75149686420164));
#71135=CARTESIAN_POINT('Ctrl Pts',(-6.69555887024443,-0.142083834635853,
-5.22497860606591));
#71136=CARTESIAN_POINT('Ctrl Pts',(-6.73531419438348,-1.97312907606641,
-4.84018087462572));
#71137=CARTESIAN_POINT('Ctrl Pts',(-6.77506951852254,-3.22214670478274,
-3.77372247305569));
#71138=CARTESIAN_POINT('Ctrl Pts',(-6.80945010830028,-4.30230297688017,
-2.85144427225017));
#71139=CARTESIAN_POINT('Ctrl Pts',(-6.84383069807803,-4.94716830048226,
-1.41936084370118));
#71140=CARTESIAN_POINT('Ctrl Pts',(-6.87821128785577,-4.9587369089069,0.00357303255080571));
#71141=CARTESIAN_POINT('Ctrl Pts',(-6.98358871214407,-4.95718456603373,
0.00410112652448823));
#71142=CARTESIAN_POINT('Ctrl Pts',(-6.95054663558112,-4.94498973829323,
-1.36454802332293));
#71143=CARTESIAN_POINT('Ctrl Pts',(-6.91750455901817,-4.35495335507998,
-2.74242709267509));
#71144=CARTESIAN_POINT('Ctrl Pts',(-6.88446248245521,-3.34724968835376,
-3.66321319163897));
#71145=CARTESIAN_POINT('Ctrl Pts',(-6.84470715831616,-2.13480815700861,
-4.77107787917753));
#71146=CARTESIAN_POINT('Ctrl Pts',(-6.80495183417709,-0.317741224101409,
-5.21724357404503));
#71147=CARTESIAN_POINT('Ctrl Pts',(-6.76519651003804,1.26993323355469,-4.79692411300152));
#71148=CARTESIAN_POINT('Ctrl Pts',(-6.72544118589898,2.8576076912108,-4.37660465195801));
#71149=CARTESIAN_POINT('Ctrl Pts',(-6.68568586175993,4.21588967361574,-3.08980003500352));
#71150=CARTESIAN_POINT('Ctrl Pts',(-6.64593053762088,4.72133959548887,-1.5271423599819));
#71151=CARTESIAN_POINT('Ctrl Pts',(-6.60617521348182,5.22678951736199,0.0355153150397139));
#71152=CARTESIAN_POINT('Ctrl Pts',(-6.56641988934277,4.87940737870325,1.87402604812845));
#71153=CARTESIAN_POINT('Ctrl Pts',(-6.52666456520372,3.83863855187625,3.14452944518438));
#71154=CARTESIAN_POINT('Ctrl Pts',(-6.48690924106466,2.79786972504925,4.4150328422403));
#71155=CARTESIAN_POINT('Ctrl Pts',(-6.4471539169256,1.06371421005396,5.11752890326346));
#71156=CARTESIAN_POINT('Ctrl Pts',(-6.40739859278654,-0.567865734104478,
4.92957806222927));
#71157=CARTESIAN_POINT('Ctrl Pts',(-6.36764326864749,-2.19944567826289,
4.74162722119508));
#71158=CARTESIAN_POINT('Ctrl Pts',(-6.32788794450843,-3.72845005158446,
3.66322947810363));
#71159=CARTESIAN_POINT('Ctrl Pts',(-6.28813262036938,-4.45307918011037,
2.18935999306868));
#71160=CARTESIAN_POINT('Ctrl Pts',(-6.26995131762761,-4.78447382589796,
1.51531524838128));
#71161=CARTESIAN_POINT('Ctrl Pts',(-6.25177001488584,-4.94763279638995,
0.758557297392875));
#71162=CARTESIAN_POINT('Ctrl Pts',(-6.23358871214408,-4.94605717997479,
0.00115570248479588));
#71163=CARTESIAN_POINT('Origin',(10.45,0.,0.));
#71164=CARTESIAN_POINT('',(-5.37821128785577,-4.95131745647145,-0.00437947150781604));
#71165=CARTESIAN_POINT('',(-5.48358871214407,-4.95293198292091,-0.00455366204130441));
#71166=CARTESIAN_POINT('',(10.45,-4.954,-6.06690024297599E-16));
#71167=CARTESIAN_POINT('Ctrl Pts',(-5.37821128785577,-4.95131745647145,
-0.00437947150781604));
#71168=CARTESIAN_POINT('Ctrl Pts',(-5.40652213254842,-4.9413622877759,1.17185497477651));
#71169=CARTESIAN_POINT('Ctrl Pts',(-5.43483297724108,-4.52190080861264,
2.35447063781816));
#71170=CARTESIAN_POINT('Ctrl Pts',(-5.46314382193373,-3.75817622776498,
3.24026575018933));
#71171=CARTESIAN_POINT('Ctrl Pts',(-5.50289914607278,-2.68572082792868,
4.48413791986167));
#71172=CARTESIAN_POINT('Ctrl Pts',(-5.54265447021184,-0.934412930545154,
5.1427095703667));
#71173=CARTESIAN_POINT('Ctrl Pts',(-5.58240979435089,0.691912411438593,
4.91370205707316));
#71174=CARTESIAN_POINT('Ctrl Pts',(-5.62216511848994,2.31823775342232,4.68469454377963));
#71175=CARTESIAN_POINT('Ctrl Pts',(-5.661920442629,3.81958054000623,3.56810786668746));
#71176=CARTESIAN_POINT('Ctrl Pts',(-5.70167576676805,4.50683752432629,2.07644557359742));
#71177=CARTESIAN_POINT('Ctrl Pts',(-5.74143109090711,5.19409450864639,0.584783280507319));
#71178=CARTESIAN_POINT('Ctrl Pts',(-5.78118641504617,5.06726569070262,-1.28195462858072));
#71179=CARTESIAN_POINT('Ctrl Pts',(-5.82094173918522,4.18456439194428,-2.6669517319329));
#71180=CARTESIAN_POINT('Ctrl Pts',(-5.86069706332428,3.30186309318596,-4.05194883528503));
#71181=CARTESIAN_POINT('Ctrl Pts',(-5.90045238746333,1.66328931361312,-4.95520513290133));
#71182=CARTESIAN_POINT('Ctrl Pts',(-5.94020771160238,0.020934129174502,
-4.96213386085296));
#71183=CARTESIAN_POINT('Ctrl Pts',(-5.97996303574144,-1.62142105526411,
-4.9690625888046));
#71184=CARTESIAN_POINT('Ctrl Pts',(-6.01971835988049,-3.2675576445685,-4.07966374709158));
#71185=CARTESIAN_POINT('Ctrl Pts',(-6.05947368401955,-4.16191329907318,
-2.70216364822446));
#71186=CARTESIAN_POINT('Ctrl Pts',(-6.08238621863162,-4.67736513686141,
-1.90825693567869));
#71187=CARTESIAN_POINT('Ctrl Pts',(-6.1052987532437,-4.94310062470359,-0.95221939658693));
#71188=CARTESIAN_POINT('Ctrl Pts',(-6.12821128785577,-4.94659179946477,
0.00201959180113259));
#71189=CARTESIAN_POINT('Ctrl Pts',(-6.23358871214408,-4.94605717997479,
0.00115570248479588));
#71190=CARTESIAN_POINT('Ctrl Pts',(-6.21201469074679,-4.94418754594816,
-0.897580677793857));
#71191=CARTESIAN_POINT('Ctrl Pts',(-6.19044066934951,-4.71036650847862,
-1.79722332865776));
#71192=CARTESIAN_POINT('Ctrl Pts',(-6.16886664795222,-4.25044360325777,
-2.56065236592303));
#71193=CARTESIAN_POINT('Ctrl Pts',(-6.12911132381317,-3.40292501414906,
-3.96745401290124));
#71194=CARTESIAN_POINT('Ctrl Pts',(-6.08935599967411,-1.78763395220142,
-4.91171607987924));
#71195=CARTESIAN_POINT('Ctrl Pts',(-6.04960067553505,-0.14597492900625,
-4.96003051237427));
#71196=CARTESIAN_POINT('Ctrl Pts',(-6.00984535139599,1.49568409418894,-5.0083449448693));
#71197=CARTESIAN_POINT('Ctrl Pts',(-5.97009002725694,3.16371107863165,-4.16071174288138));
#71198=CARTESIAN_POINT('Ctrl Pts',(-5.93033470311789,4.09249618417905,-2.80618715449666));
#71199=CARTESIAN_POINT('Ctrl Pts',(-5.89057937897884,5.02128128972644,-1.45166256611195));
#71200=CARTESIAN_POINT('Ctrl Pts',(-5.85082405483978,5.2108245163785,0.409753408669569));
#71201=CARTESIAN_POINT('Ctrl Pts',(-5.81106873070073,4.57412717597807,1.92368706955186));
#71202=CARTESIAN_POINT('Ctrl Pts',(-5.77131340656167,3.93742983557762,3.43762073043419));
#71203=CARTESIAN_POINT('Ctrl Pts',(-5.73155808242261,2.47449192812468,4.60407207741728));
#71204=CARTESIAN_POINT('Ctrl Pts',(-5.69180275828356,0.856789195864615,
4.88765011405602));
#71205=CARTESIAN_POINT('Ctrl Pts',(-5.6520474341445,-0.760913536395409,
5.17122815069474));
#71206=CARTESIAN_POINT('Ctrl Pts',(-5.61229211000545,-2.53338109346257,
4.57193287698912));
#71207=CARTESIAN_POINT('Ctrl Pts',(-5.5725367858664,-3.64706632311371,3.36483559752805));
#71208=CARTESIAN_POINT('Ctrl Pts',(-5.54288742795896,-4.47764820579843,
2.46458739070536));
#71209=CARTESIAN_POINT('Ctrl Pts',(-5.51323807005152,-4.94180776187748,
1.22627270001379));
#71210=CARTESIAN_POINT('Ctrl Pts',(-5.48358871214407,-4.95293198292091,
-0.00455366204130441));
#71211=CARTESIAN_POINT('Origin',(10.45,0.,0.));
#71212=CARTESIAN_POINT('',(-4.62821128785577,-4.96217793349678,1.83253063722107E-5));
#71213=CARTESIAN_POINT('',(-4.73358871214408,-4.96190938845054,0.00104730840813116));
#71214=CARTESIAN_POINT('',(10.45,-4.954,-6.06690024297599E-16));
#71215=CARTESIAN_POINT('Ctrl Pts',(-4.62821128785577,-4.96217793349678,
1.83253063722107E-5));
#71216=CARTESIAN_POINT('Ctrl Pts',(-4.66799018771409,-4.96226779169355,
1.64336216035063));
#71217=CARTESIAN_POINT('Ctrl Pts',(-4.70776908757242,-4.06471490519605,
3.28662169090852));
#71218=CARTESIAN_POINT('Ctrl Pts',(-4.74754798743074,-2.68210834911436,
4.1748659253201));
#71219=CARTESIAN_POINT('Ctrl Pts',(-4.7873033115698,-1.3003212210245,5.06258372494367));
#71220=CARTESIAN_POINT('Ctrl Pts',(-4.82705863570885,0.565944505497547,
5.1961809116512));
#71221=CARTESIAN_POINT('Ctrl Pts',(-4.8668139598479,2.06008913639825,4.51433754175314));
#71222=CARTESIAN_POINT('Ctrl Pts',(-4.90656928398696,3.55423376729897,3.83249417185506));
#71223=CARTESIAN_POINT('Ctrl Pts',(-4.94632460812601,4.67625730257835,2.33521024535137));
#71224=CARTESIAN_POINT('Ctrl Pts',(-4.98607993226507,4.91116072393883,0.70972602772372));
#71225=CARTESIAN_POINT('Ctrl Pts',(-5.02583525640412,5.14606414529932,-0.91575818990395));
#71226=CARTESIAN_POINT('Ctrl Pts',(-5.06559058054318,4.49384745274089,-2.66944269865558));
#71227=CARTESIAN_POINT('Ctrl Pts',(-5.10534590468223,3.25387242061459,-3.74640160169083));
#71228=CARTESIAN_POINT('Ctrl Pts',(-5.14510122882129,2.01389738848831,-4.82336050472606));
#71229=CARTESIAN_POINT('Ctrl Pts',(-5.18485655296034,0.186164016794188,
-5.22359380204494));
#71230=CARTESIAN_POINT('Ctrl Pts',(-5.2246118770994,-1.39041401526609,-4.76339790033747));
#71231=CARTESIAN_POINT('Ctrl Pts',(-5.26436720123845,-2.96699204732638,
-4.30320199863));
#71232=CARTESIAN_POINT('Ctrl Pts',(-5.30412252537751,-4.29241473975282,
-2.98257689789619));
#71233=CARTESIAN_POINT('Ctrl Pts',(-5.34387784951656,-4.75832463482155,
-1.40767800310946));
#71234=CARTESIAN_POINT('Ctrl Pts',(-5.35532232896297,-4.89244745568799,
-0.954307330831556));
#71235=CARTESIAN_POINT('Ctrl Pts',(-5.36676680840937,-4.95534177029036,
-0.479864787851824));
#71236=CARTESIAN_POINT('Ctrl Pts',(-5.37821128785577,-4.95131745647145,
-0.00437947150781604));
#71237=CARTESIAN_POINT('Ctrl Pts',(-5.48358871214407,-4.95293198292091,
-0.00455366204130441));
#71238=CARTESIAN_POINT('Ctrl Pts',(-5.47348274591246,-4.95672366713103,
-0.424080104763632));
#71239=CARTESIAN_POINT('Ctrl Pts',(-5.46337677968084,-4.9078824662274,-0.842736566029038));
#71240=CARTESIAN_POINT('Ctrl Pts',(-5.45327081344923,-4.80297856458869,
-1.24683931269579));
#71241=CARTESIAN_POINT('Ctrl Pts',(-5.41351548931017,-4.39030267417733,
-2.83651765824206));
#71242=CARTESIAN_POINT('Ctrl Pts',(-5.37376016517112,-3.11004799111942,
-4.20097506411805));
#71243=CARTESIAN_POINT('Ctrl Pts',(-5.33400484103207,-1.54984025071783,
-4.71393747952145));
#71244=CARTESIAN_POINT('Ctrl Pts',(-5.29424951689301,0.0103674896837219,
-5.22689989492483));
#71245=CARTESIAN_POINT('Ctrl Pts',(-5.25449419275395,1.85052828742895,-4.88836731985566));
#71246=CARTESIAN_POINT('Ctrl Pts',(-5.2147388686149,3.12602438312975,-3.85372325416089));
#71247=CARTESIAN_POINT('Ctrl Pts',(-5.17498354447584,4.40152047883059,-2.81907918846609));
#71248=CARTESIAN_POINT('Ctrl Pts',(-5.1352282203368,5.11235187248696,-1.08832363214565));
#71249=CARTESIAN_POINT('Ctrl Pts',(-5.09547289619774,4.93225315308238,0.544141707178393));
#71250=CARTESIAN_POINT('Ctrl Pts',(-5.05571757205869,4.7521544336778,2.17660704650244));
#71251=CARTESIAN_POINT('Ctrl Pts',(-5.01596224791963,3.68112560121227,3.71078216883009));
#71252=CARTESIAN_POINT('Ctrl Pts',(-4.97620692378057,2.2107595500815,4.4424940714992));
#71253=CARTESIAN_POINT('Ctrl Pts',(-4.93645159964152,0.74039349895078,5.1742059741683));
#71254=CARTESIAN_POINT('Ctrl Pts',(-4.89669627550247,-1.12930977084514,
5.10345465717892));
#71255=CARTESIAN_POINT('Ctrl Pts',(-4.85694095136341,-2.54017276286649,
4.2627143580556));
#71256=CARTESIAN_POINT('Ctrl Pts',(-4.81718562722436,-3.95103575488788,
3.42197405893225));
#71257=CARTESIAN_POINT('Ctrl Pts',(-4.7774303030853,-4.90305846913465,1.81124477767492));
#71258=CARTESIAN_POINT('Ctrl Pts',(-4.73767497894624,-4.95927078170297,
0.169837208318289));
#71259=CARTESIAN_POINT('Ctrl Pts',(-4.73631289001219,-4.96119671667055,
0.113599631719194));
#71260=CARTESIAN_POINT('Ctrl Pts',(-4.73495080107814,-4.96207108588767,
0.0573260427708458));
#71261=CARTESIAN_POINT('Ctrl Pts',(-4.73358871214408,-4.96190938845054,
0.00104730840813116));
#71262=CARTESIAN_POINT('Origin',(10.45,0.,0.));
#71263=CARTESIAN_POINT('',(-3.87821128785577,-4.95126260644063,0.00436986867149824));
#71264=CARTESIAN_POINT('',(-3.98358871214407,-4.94978226424517,0.00400445798880121));
#71265=CARTESIAN_POINT('',(10.45,-4.954,-6.06690024297599E-16));
#71266=CARTESIAN_POINT('Ctrl Pts',(-3.87821128785577,-4.95126260644063,
0.00436986867149824));
#71267=CARTESIAN_POINT('Ctrl Pts',(-3.88970291874071,-4.95529130462732,
0.481827588074343));
#71268=CARTESIAN_POINT('Ctrl Pts',(-3.90119454962565,-4.89186792492517,
0.958237191039586));
#71269=CARTESIAN_POINT('Ctrl Pts',(-3.91268618051059,-4.75665313243704,
1.41331584172282));
#71270=CARTESIAN_POINT('Ctrl Pts',(-3.95244150464964,-4.28887723904272,
2.98766150665242));
#71271=CARTESIAN_POINT('Ctrl Pts',(-3.9921968287887,-2.96189047760415,4.30671499505008));
#71272=CARTESIAN_POINT('Ctrl Pts',(-4.03195215292775,-1.38476819988259,
4.76504225829968));
#71273=CARTESIAN_POINT('Ctrl Pts',(-4.07170747706681,0.192354077838921,
5.22336952154927));
#71274=CARTESIAN_POINT('Ctrl Pts',(-4.11146280120586,2.0196118718434,4.82097055965087));
#71275=CARTESIAN_POINT('Ctrl Pts',(-4.15121812534491,3.25830978894152,3.74254298707118));
#71276=CARTESIAN_POINT('Ctrl Pts',(-4.19097344948397,4.49700770603967,2.66411541449148));
#71277=CARTESIAN_POINT('Ctrl Pts',(-4.23072877362303,5.14714574623144,0.909659231230486));
#71278=CARTESIAN_POINT('Ctrl Pts',(-4.27048409776208,4.91031621847561,-0.715545474000941));
#71279=CARTESIAN_POINT('Ctrl Pts',(-4.31023942190114,4.67348669071978,-2.34075017923237));
#71280=CARTESIAN_POINT('Ctrl Pts',(-4.34999474604019,3.54968959501634,-3.83670340643423));
#71281=CARTESIAN_POINT('Ctrl Pts',(-4.38975007017924,2.05473799843147,-4.51677566950028));
#71282=CARTESIAN_POINT('Ctrl Pts',(-4.4295053943183,0.559786401846604,-5.19684793256633));
#71283=CARTESIAN_POINT('Ctrl Pts',(-4.46926071845735,-1.30631969561969,
-5.06103923149656));
#71284=CARTESIAN_POINT('Ctrl Pts',(-4.50901604259641,-2.68705386825844,
-4.17168457578772));
#71285=CARTESIAN_POINT('Ctrl Pts',(-4.54874779101619,-4.06696923732954,
-3.28285732555593));
#71286=CARTESIAN_POINT('Ctrl Pts',(-4.58847953943598,-4.96208818181233,
-1.64137759196963));
#71287=CARTESIAN_POINT('Ctrl Pts',(-4.62821128785577,-4.96217793349678,
1.83253063722107E-5));
#71288=CARTESIAN_POINT('Ctrl Pts',(-4.73358871214408,-4.96190938845054,
0.00104730840813116));
#71289=CARTESIAN_POINT('Ctrl Pts',(-4.69519547693908,-4.95735161870378,
-1.58528279927264));
#71290=CARTESIAN_POINT('Ctrl Pts',(-4.65680224173408,-4.12963019580917,
-3.17570098185821));
#71291=CARTESIAN_POINT('Ctrl Pts',(-4.61840900652908,-2.82584471571655,
-4.0789475365882));
#71292=CARTESIAN_POINT('Ctrl Pts',(-4.57865368239002,-1.47580442627195,
-5.01423885468211));
#71293=CARTESIAN_POINT('Ctrl Pts',(-4.53889835825097,0.384678063507157,
-5.212735633414));
#71294=CARTESIAN_POINT('Ctrl Pts',(-4.49914303411192,1.90165751480054,-4.58332958229983));
#71295=CARTESIAN_POINT('Ctrl Pts',(-4.45938770997286,3.41863696609391,-3.95392353118567));
#71296=CARTESIAN_POINT('Ctrl Pts',(-4.4196323858338,4.59211337890157,-2.49661465022554));
#71297=CARTESIAN_POINT('Ctrl Pts',(-4.37987706169475,4.88347131282572,-0.88029500759142));
#71298=CARTESIAN_POINT('Ctrl Pts',(-4.34012173755569,5.17482924674987,0.736024635042727));
#71299=CARTESIAN_POINT('Ctrl Pts',(-4.30036641341664,4.58406870179042,2.5113550393509));
#71300=CARTESIAN_POINT('Ctrl Pts',(-4.26061108927758,3.3823436164673,3.63083503119117));
#71301=CARTESIAN_POINT('Ctrl Pts',(-4.22085576513853,2.18061853114421,4.75031502303142));
#71302=CARTESIAN_POINT('Ctrl Pts',(-4.18110044099947,0.367928905457532,
5.21394460240387));
#71303=CARTESIAN_POINT('Ctrl Pts',(-4.14134511686042,-1.22371652962239,
4.80892183537132));
#71304=CARTESIAN_POINT('Ctrl Pts',(-4.10158979272137,-2.81536196470231,
4.40389906833878));
#71305=CARTESIAN_POINT('Ctrl Pts',(-4.06183446858231,-4.18596320917542,
3.13022395490121));
#71306=CARTESIAN_POINT('Ctrl Pts',(-4.02207914444326,-4.70642624389953,
1.57250226528164));
#71307=CARTESIAN_POINT('Ctrl Pts',(-4.00924900034353,-4.87439407911917,
1.06978233586574));
#71308=CARTESIAN_POINT('Ctrl Pts',(-3.9964188562438,-4.95381732933038,0.537478056608055));
#71309=CARTESIAN_POINT('Ctrl Pts',(-3.98358871214407,-4.94978226424517,
0.00400445798880121));
#71310=CARTESIAN_POINT('Origin',(10.45,0.,0.));
#71311=CARTESIAN_POINT('',(-3.12821128785576,-4.94661592217658,-0.00204876029963219));
#71312=CARTESIAN_POINT('',(-3.23358871214408,-4.94744349501179,-0.00282914305488679));
#71313=CARTESIAN_POINT('',(10.45,-4.954,-6.06690024297599E-16));
#71314=CARTESIAN_POINT('Ctrl Pts',(-3.12821128785576,-4.94661592217658,
-0.00204876029963219));
#71315=CARTESIAN_POINT('Ctrl Pts',(-3.15117097390638,-4.94306604476936,
0.954142296727101));
#71316=CARTESIAN_POINT('Ctrl Pts',(-3.17413065995699,-4.67616316064024,
1.91216596896721));
#71317=CARTESIAN_POINT('Ctrl Pts',(-3.1970903460076,-4.15870819221125,2.70709380384627));
#71318=CARTESIAN_POINT('Ctrl Pts',(-3.23684567014666,-3.26272076660311,
4.08353308411823));
#71319=CARTESIAN_POINT('Ctrl Pts',(-3.27660099428571,-1.61553135584163,
4.97098055600742));
#71320=CARTESIAN_POINT('Ctrl Pts',(-3.31635631842476,0.0268144645398234,
4.96210556873584));
#71321=CARTESIAN_POINT('Ctrl Pts',(-3.35611164256382,1.66916028492123,4.95323058146427));
#71322=CARTESIAN_POINT('Ctrl Pts',(-3.39586696670287,3.30666251492261,4.04803313503198));
#71323=CARTESIAN_POINT('Ctrl Pts',(-3.43562229084193,4.18772191050428,2.66199096374692));
#71324=CARTESIAN_POINT('Ctrl Pts',(-3.47537761498098,5.06878130608597,1.27594879246181));
#71325=CARTESIAN_POINT('Ctrl Pts',(-3.51513293912004,5.1933978672479,-0.590938103676095));
#71326=CARTESIAN_POINT('Ctrl Pts',(-3.55488826325909,4.50437367911208,-2.08178491917636));
#71327=CARTESIAN_POINT('Ctrl Pts',(-3.59464358739815,3.81534949097627,-3.57263173467662));
#71328=CARTESIAN_POINT('Ctrl Pts',(-3.6343989115372,2.3126845535427,-4.68743846953923));
#71329=CARTESIAN_POINT('Ctrl Pts',(-3.67415423567626,0.686088969385792,
-4.91451855392519));
#71330=CARTESIAN_POINT('Ctrl Pts',(-3.71390955981531,-0.940506614771073,
-5.14159863831115));
#71331=CARTESIAN_POINT('Ctrl Pts',(-3.75366488395437,-2.69103284565128,
-4.4809520722205));
#71332=CARTESIAN_POINT('Ctrl Pts',(-3.79342020809342,-3.76201344841635,
-3.23580986844443));
#71333=CARTESIAN_POINT('Ctrl Pts',(-3.82168390134754,-4.52341755951813,
-2.35058711985895));
#71334=CARTESIAN_POINT('Ctrl Pts',(-3.84994759460165,-4.94135401375244,
-1.16993851785152));
#71335=CARTESIAN_POINT('Ctrl Pts',(-3.87821128785577,-4.95126260644063,
0.00436986867149824));
#71336=CARTESIAN_POINT('Ctrl Pts',(-3.98358871214407,-4.94978226424517,
0.00400445798880121));
#71337=CARTESIAN_POINT('Ctrl Pts',(-3.95666353210474,-4.94131432709302,
-1.11553656800441));
#71338=CARTESIAN_POINT('Ctrl Pts',(-3.92973835206541,-4.56529016919644,
-2.24022735773114));
#71339=CARTESIAN_POINT('Ctrl Pts',(-3.90281317202609,-3.86871874929071,
-3.10744695891477));
#71340=CARTESIAN_POINT('Ctrl Pts',(-3.86305784788703,-2.84022339498269,
-4.38790622769));
#71341=CARTESIAN_POINT('Ctrl Pts',(-3.82330252374798,-1.11290786139162,
-5.10705649943884));
#71342=CARTESIAN_POINT('Ctrl Pts',(-3.78354719960893,0.520405084295247,
-4.93481407064357));
#71343=CARTESIAN_POINT('Ctrl Pts',(-3.74379187546987,2.15371802998204,-4.76257164184831));
#71344=CARTESIAN_POINT('Ctrl Pts',(-3.70403655133082,3.69302838776461,-3.698936512509));
#71345=CARTESIAN_POINT('Ctrl Pts',(-3.66428122719176,4.43180612668787,-2.23210793176182));
#71346=CARTESIAN_POINT('Ctrl Pts',(-3.6245259030527,5.17058386561115,-0.76527935101459));
#71347=CARTESIAN_POINT('Ctrl Pts',(-3.58477057891365,5.10882898567509,1.10474268114056));
#71348=CARTESIAN_POINT('Ctrl Pts',(-3.5450152547746,4.27488643824851,2.5196343591206));
#71349=CARTESIAN_POINT('Ctrl Pts',(-3.50525993063554,3.44094389082193,3.93452603710064));
#71350=CARTESIAN_POINT('Ctrl Pts',(-3.46550460649649,1.8348136759048,4.89428736090561));
#71351=CARTESIAN_POINT('Ctrl Pts',(-3.42574928235743,0.193695556186975,
4.95839625232752));
#71352=CARTESIAN_POINT('Ctrl Pts',(-3.38599395821838,-1.44742256353083,
5.02250514374942));
#71353=CARTESIAN_POINT('Ctrl Pts',(-3.34623863407933,-3.1235285880493,4.19096160278835));
#71354=CARTESIAN_POINT('Ctrl Pts',(-3.30648330994027,-4.06530446828262,
2.84543686342598));
#71355=CARTESIAN_POINT('Ctrl Pts',(-3.28218511067487,-4.64091184910068,
2.02306076810869));
#71356=CARTESIAN_POINT('Ctrl Pts',(-3.25788691140947,-4.94220462071748,
1.00868308784557));
#71357=CARTESIAN_POINT('Ctrl Pts',(-3.23358871214408,-4.94744349501179,
-0.00282914305488679));
#71358=CARTESIAN_POINT('Origin',(10.45,0.,0.));
#71359=CARTESIAN_POINT('',(-2.37821128785577,-4.95878862246057,-0.00355106645011816));
#71360=CARTESIAN_POINT('',(-2.48358871214407,-4.9601430818857,-0.00283985261795904));
#71361=CARTESIAN_POINT('',(10.45,-4.954,-6.06690024297599E-16));
#71362=CARTESIAN_POINT('Ctrl Pts',(-2.37821128785577,-4.95878862246057,
-0.00355106645011816));
#71363=CARTESIAN_POINT('Ctrl Pts',(-2.41263902907205,-4.9472554647168,1.42129552477773));
#71364=CARTESIAN_POINT('Ctrl Pts',(-2.44706677028833,-4.30040375105269,
2.85527758425018));
#71365=CARTESIAN_POINT('Ctrl Pts',(-2.48149451150461,-3.21767241276599,
3.77753821091363));
#71366=CARTESIAN_POINT('Ctrl Pts',(-2.52124983564367,-1.96739186026945,
4.84251572202474));
#71367=CARTESIAN_POINT('Ctrl Pts',(-2.56100515978272,-0.135891902052169,
5.22514331295018));
#71368=CARTESIAN_POINT('Ctrl Pts',(-2.60076048392178,1.43618495231579,4.74979825608725));
#71369=CARTESIAN_POINT('Ctrl Pts',(-2.64051580806083,3.00826180668371,4.27445319922434));
#71370=CARTESIAN_POINT('Ctrl Pts',(-2.68027113219989,4.32091555720235,2.94113549457312));
#71371=CARTESIAN_POINT('Ctrl Pts',(-2.72002645633894,4.77164957913437,1.36182634162164));
#71372=CARTESIAN_POINT('Ctrl Pts',(-2.75978178047799,5.22238360106641,-0.2174828113299));
#71373=CARTESIAN_POINT('Ctrl Pts',(-2.79953710461705,4.8111978944118,-2.04278341258168));
#71374=CARTESIAN_POINT('Ctrl Pts',(-2.8392924287561,3.72682311285719,-3.27627840335056));
#71375=CARTESIAN_POINT('Ctrl Pts',(-2.87904775289516,2.64244833130259,-4.50977339411943));
#71376=CARTESIAN_POINT('Ctrl Pts',(-2.91880307703422,0.884884474847997,
-5.15146277440537));
#71377=CARTESIAN_POINT('Ctrl Pts',(-2.95855840117327,-0.739161972899706,
-4.90681671438896));
#71378=CARTESIAN_POINT('Ctrl Pts',(-2.99831372531233,-2.36320842064736,
-4.66217065437255));
#71379=CARTESIAN_POINT('Ctrl Pts',(-3.03806904945138,-3.85373745968816,
-3.53118915405384));
#71380=CARTESIAN_POINT('Ctrl Pts',(-3.07782437359043,-4.52660925898116,
-2.03298285956715));
#71381=CARTESIAN_POINT('Ctrl Pts',(-3.09462001167887,-4.81088089971325,
-1.40002787180222));
#71382=CARTESIAN_POINT('Ctrl Pts',(-3.11141564976732,-4.94921275455742,
-0.701528661802854));
#71383=CARTESIAN_POINT('Ctrl Pts',(-3.12821128785576,-4.94661592217658,
-0.00204876029963219));
#71384=CARTESIAN_POINT('Ctrl Pts',(-3.23358871214408,-4.94744349501179,
-0.00282914305488679));
#71385=CARTESIAN_POINT('Ctrl Pts',(-3.21813158727042,-4.95077616725141,
-0.646295380757791));
#71386=CARTESIAN_POINT('Ctrl Pts',(-3.20267446239676,-4.83430243494921,
-1.28860203505834));
#71387=CARTESIAN_POINT('Ctrl Pts',(-3.1872173375231,-4.59242589231839,-1.87958393990419));
#71388=CARTESIAN_POINT('Ctrl Pts',(-3.14746201338405,-3.97032570017272,
-3.39957406610822));
#71389=CARTESIAN_POINT('Ctrl Pts',(-3.107706689245,-2.51867957993331,-4.5800483807526));
#71390=CARTESIAN_POINT('Ctrl Pts',(-3.06795136510594,-0.903780441982408,
-4.87917946752035));
#71391=CARTESIAN_POINT('Ctrl Pts',(-3.02819604096689,0.711118695968514,
-5.17831055428811));
#71392=CARTESIAN_POINT('Ctrl Pts',(-2.98844071682783,2.48927085163095,-4.59609841317917));
#71393=CARTESIAN_POINT('Ctrl Pts',(-2.94868539268878,3.61451969159798,-3.39977333989084));
#71394=CARTESIAN_POINT('Ctrl Pts',(-2.90893006854972,4.73976853156503,-2.20344826660249));
#71395=CARTESIAN_POINT('Ctrl Pts',(-2.86917474441066,5.2121140558367,-0.393010261134748));
#71396=CARTESIAN_POINT('Ctrl Pts',(-2.82941942027161,4.8147537877728,1.20056541958762));
#71397=CARTESIAN_POINT('Ctrl Pts',(-2.78966409613256,4.41739351970892,2.79414110030994));
#71398=CARTESIAN_POINT('Ctrl Pts',(-2.7499087719935,3.15032745930952,4.17085445628686));
#71399=CARTESIAN_POINT('Ctrl Pts',(-2.71015344785445,1.59512787908609,4.6988060624955));
#71400=CARTESIAN_POINT('Ctrl Pts',(-2.67039812371539,0.0399282988626437,
5.22675766870414));
#71401=CARTESIAN_POINT('Ctrl Pts',(-2.63064279957634,-1.80340480118489,
4.90594752514445));
#71402=CARTESIAN_POINT('Ctrl Pts',(-2.59088747543728,-3.08879760257501,
3.88362469014566));
#71403=CARTESIAN_POINT('Ctrl Pts',(-2.55512122100621,-4.2452134279769,2.96388225516099));
#71404=CARTESIAN_POINT('Ctrl Pts',(-2.51935496657514,-4.95003952369581,
1.47634443515309));
#71405=CARTESIAN_POINT('Ctrl Pts',(-2.48358871214407,-4.9601430818857,-0.00283985261795904));
#71406=CARTESIAN_POINT('Origin',(10.45,0.,0.));
#71407=CARTESIAN_POINT('',(-1.62821128785576,-4.95786674368922,0.00389817196716477));
#71408=CARTESIAN_POINT('',(-1.73358871214408,-4.95624245093516,0.0043165021388984));
#71409=CARTESIAN_POINT('',(10.45,-4.954,-6.06690024297599E-16));
#71410=CARTESIAN_POINT('Ctrl Pts',(-1.62821128785576,-4.95786674368922,
0.00389817196716477));
#71411=CARTESIAN_POINT('Ctrl Pts',(-1.63435176009866,-4.96006131004143,
0.258154385410107));
#71412=CARTESIAN_POINT('Ctrl Pts',(-1.64049223234156,-4.94219726502405,
0.512101374217645));
#71413=CARTESIAN_POINT('Ctrl Pts',(-1.64663270458446,-4.90320362582084,
0.762761361452733));
#71414=CARTESIAN_POINT('Ctrl Pts',(-1.68638802872351,-4.6507466966851,2.38561195779698));
#71415=CARTESIAN_POINT('Ctrl Pts',(-1.72614335286257,-3.51260697205389,
3.87068230545853));
#71416=CARTESIAN_POINT('Ctrl Pts',(-1.76589867700162,-2.01118066059901,
4.53633806513804));
#71417=CARTESIAN_POINT('Ctrl Pts',(-1.80565400114068,-0.509754349144126,
5.20199382481756));
#71418=CARTESIAN_POINT('Ctrl Pts',(-1.84540932527974,1.35495854913438,5.04823499651502));
#71419=CARTESIAN_POINT('Ctrl Pts',(-1.88516464941879,2.72707107480563,4.14563554159628));
#71420=CARTESIAN_POINT('Ctrl Pts',(-1.92491997355785,4.09918360047684,3.24303608667757));
#71421=CARTESIAN_POINT('Ctrl Pts',(-1.9646752976969,4.97869575354077,1.59159600514272));
#71422=CARTESIAN_POINT('Ctrl Pts',(-2.00443062183595,4.96191912536181,-0.0506881066571491));
#71423=CARTESIAN_POINT('Ctrl Pts',(-2.04418594597501,4.94514249718285,-1.69297221845702));
#71424=CARTESIAN_POINT('Ctrl Pts',(-2.08394127011406,4.03207708776091,-3.32610036052202));
#71425=CARTESIAN_POINT('Ctrl Pts',(-2.12369659425312,2.64181195780517,-4.20048095703164));
#71426=CARTESIAN_POINT('Ctrl Pts',(-2.16345191839217,1.25154682784939,-5.07486155354129));
#71427=CARTESIAN_POINT('Ctrl Pts',(-2.20320724253123,-0.61591802264022,
-5.19049460449564));
#71428=CARTESIAN_POINT('Ctrl Pts',(-2.24296256667028,-2.10343251216577,
-4.49430554786297));
#71429=CARTESIAN_POINT('Ctrl Pts',(-2.28271789080934,-3.59094700169127,
-3.79811649123032));
#71430=CARTESIAN_POINT('Ctrl Pts',(-2.32247321494839,-4.69851113025268,
-2.29010532701072));
#71431=CARTESIAN_POINT('Ctrl Pts',(-2.36222853908745,-4.91776262114551,
-0.662436029252524));
#71432=CARTESIAN_POINT('Ctrl Pts',(-2.36755612201022,-4.9471443586604,-0.444313215706146));
#71433=CARTESIAN_POINT('Ctrl Pts',(-2.37288370493299,-4.96057334176166,
-0.224041522658353));
#71434=CARTESIAN_POINT('Ctrl Pts',(-2.37821128785577,-4.95878862246057,
-0.00355106645011816));
#71435=CARTESIAN_POINT('Ctrl Pts',(-2.48358871214407,-4.9601430818857,-0.00283985261795904));
#71436=CARTESIAN_POINT('Ctrl Pts',(-2.47959964243609,-4.96126994849667,
-0.167815730823135));
#71437=CARTESIAN_POINT('Ctrl Pts',(-2.4756105727281,-4.9537549453676,-0.332687696842427));
#71438=CARTESIAN_POINT('Ctrl Pts',(-2.47162150302012,-4.93726075563198,
-0.496656414917237));
#71439=CARTESIAN_POINT('Ctrl Pts',(-2.43186617888106,-4.77287860456607,
-2.13077915854342));
#71440=CARTESIAN_POINT('Ctrl Pts',(-2.39211085474201,-3.71666179970155,
-3.67518911935791));
#71441=CARTESIAN_POINT('Ctrl Pts',(-2.35235553060295,-2.25340464393075,
-4.42101559308418));
#71442=CARTESIAN_POINT('Ctrl Pts',(-2.3126002064639,-0.790147488159902,
-5.16684206681047));
#71443=CARTESIAN_POINT('Ctrl Pts',(-2.27284488232484,1.0801500185172,-5.11408505344847));
#71444=CARTESIAN_POINT('Ctrl Pts',(-2.23308955818579,2.49903763011426,-4.28695956207369));
#71445=CARTESIAN_POINT('Ctrl Pts',(-2.19333423404673,3.91792524171126,-3.45983407069895));
#71446=CARTESIAN_POINT('Ctrl Pts',(-2.15357890990768,4.88540295822824,-1.85834010131145));
#71447=CARTESIAN_POINT('Ctrl Pts',(-2.11382358576863,4.95740694449176,-0.217549420332463));
#71448=CARTESIAN_POINT('Ctrl Pts',(-2.07406826162957,5.02941093075529,1.42324126064658));
#71449=CARTESIAN_POINT('Ctrl Pts',(-2.03431293749051,4.20594118676532,3.10332865321719));
#71450=CARTESIAN_POINT('Ctrl Pts',(-1.99455761335146,2.86496314409989,4.05156729507624));
#71451=CARTESIAN_POINT('Ctrl Pts',(-1.9548022892124,1.52398510143443,4.99980593693532));
#71452=CARTESIAN_POINT('Ctrl Pts',(-1.91504696507335,-0.334501239906424,
5.21619582808284));
#71453=CARTESIAN_POINT('Ctrl Pts',(-1.8752916409343,-1.85746685582874,4.60141589546955));
#71454=CARTESIAN_POINT('Ctrl Pts',(-1.83553631679524,-3.38043247175097,
3.98663596285629));
#71455=CARTESIAN_POINT('Ctrl Pts',(-1.79578099265619,-4.56787736225463,
2.54068620648225));
#71456=CARTESIAN_POINT('Ctrl Pts',(-1.75602566851713,-4.87477467748886,
0.927244955389617));
#71457=CARTESIAN_POINT('Ctrl Pts',(-1.74854668305945,-4.93250985151514,
0.623715707041817));
#71458=CARTESIAN_POINT('Ctrl Pts',(-1.74106769760176,-4.95908142667506,
0.314258740644999));
#71459=CARTESIAN_POINT('Ctrl Pts',(-1.73358871214408,-4.95624245093516,
0.0043165021388984));
#71460=CARTESIAN_POINT('Origin',(10.45,0.,0.));
#71461=CARTESIAN_POINT('',(-0.878211287855769,-4.9462499908807,0.00153300580362309));
#71462=CARTESIAN_POINT('',(-0.983588712144078,-4.94588532464384,0.00063872631976612));
#71463=CARTESIAN_POINT('',(10.45,-4.954,-6.06690024297599E-16));
#71464=CARTESIAN_POINT('Ctrl Pts',(-0.878211287855769,-4.9462499908807,
0.00153300580362309));
#71465=CARTESIAN_POINT('Ctrl Pts',(-0.895819815264337,-4.94827859092613,
0.735002394484792));
#71466=CARTESIAN_POINT('Ctrl Pts',(-0.913428342672905,-4.79565751940137,
1.46766899677298));
#71467=CARTESIAN_POINT('Ctrl Pts',(-0.931036870081473,-4.48413338106601,
2.1250314142613));
#71468=CARTESIAN_POINT('Ctrl Pts',(-0.970792194220528,-3.78079557153196,
3.60917914437558));
#71469=CARTESIAN_POINT('Ctrl Pts',(-1.01054751835958,-2.26747308842599,
4.70947502840552));
#71470=CARTESIAN_POINT('Ctrl Pts',(-1.05030284249864,-0.638767754849003,
4.92089285050518));
#71471=CARTESIAN_POINT('Ctrl Pts',(-1.09005816663769,0.989937578727986,
5.13231067260483));
#71472=CARTESIAN_POINT('Ctrl Pts',(-1.12981349077675,2.73402576277599,4.4548504327742));
#71473=CARTESIAN_POINT('Ctrl Pts',(-1.1695688149158,3.79297552981071,3.19946047343064));
#71474=CARTESIAN_POINT('Ctrl Pts',(-1.20932413905486,4.85192529684539,1.94407051408712));
#71475=CARTESIAN_POINT('Ctrl Pts',(-1.24907946319391,5.22573664686682,0.110750835230702));
#71476=CARTESIAN_POINT('Ctrl Pts',(-1.28883478733297,4.7428334299669,-1.45902081766377));
#71477=CARTESIAN_POINT('Ctrl Pts',(-1.32859011147202,4.25993021306696,-3.02879247055829));
#71478=CARTESIAN_POINT('Ctrl Pts',(-1.36834543561108,2.92031242924562,-4.33501609749086));
#71479=CARTESIAN_POINT('Ctrl Pts',(-1.40810075975013,1.33885295939138,-4.77814644437744));
#71480=CARTESIAN_POINT('Ctrl Pts',(-1.44785608388919,-0.242606510462868,
-5.22127679126403));
#71481=CARTESIAN_POINT('Ctrl Pts',(-1.48761140802824,-2.06590766635002,
-4.80131385810463));
#71482=CARTESIAN_POINT('Ctrl Pts',(-1.5273667321673,-3.29417117747345,-3.71101696901146));
#71483=CARTESIAN_POINT('Ctrl Pts',(-1.56098158406345,-4.33272128139038,
-2.78912363161815));
#71484=CARTESIAN_POINT('Ctrl Pts',(-1.59459643595961,-4.94585300598505,
-1.38797929616193));
#71485=CARTESIAN_POINT('Ctrl Pts',(-1.62821128785576,-4.95786674368922,
0.00389817196716477));
#71486=CARTESIAN_POINT('Ctrl Pts',(-1.73358871214408,-4.95624245093516,
0.0043165021388984));
#71487=CARTESIAN_POINT('Ctrl Pts',(-1.70131237346271,-4.94399055620857,
-1.33327142583419));
#71488=CARTESIAN_POINT('Ctrl Pts',(-1.66903603478134,-4.38398371281437,
-2.67989727357355));
#71489=CARTESIAN_POINT('Ctrl Pts',(-1.63675969609996,-3.41712436432993,
-3.59812068200678));
#71490=CARTESIAN_POINT('Ctrl Pts',(-1.59700437196091,-2.22622699597197,
-4.72911232249915));
#71491=CARTESIAN_POINT('Ctrl Pts',(-1.55724904782185,-0.418082519291285,
-5.21016285767256));
#71492=CARTESIAN_POINT('Ctrl Pts',(-1.5174937236828,1.17738651850033,-4.82047428679334));
#71493=CARTESIAN_POINT('Ctrl Pts',(-1.47773839954375,2.77285555629184,-4.43078571591415));
#71494=CARTESIAN_POINT('Ctrl Pts',(-1.4379830754047,4.15564915519426,-3.17035803898244));
#71495=CARTESIAN_POINT('Ctrl Pts',(-1.39822775126564,4.69107711170357,-1.61771656838675));
#71496=CARTESIAN_POINT('Ctrl Pts',(-1.35847242712659,5.22650506821291,-0.0650750977909698));
#71497=CARTESIAN_POINT('Ctrl Pts',(-1.31871710298753,4.91456738232895,1.77978016646891));
#71498=CARTESIAN_POINT('Ctrl Pts',(-1.27896177884847,3.89844073167842,3.07007674581154));
#71499=CARTESIAN_POINT('Ctrl Pts',(-1.23920645470942,2.88231408102786,4.36037332515421));
#71500=CARTESIAN_POINT('Ctrl Pts',(-1.19945113057036,1.16199846561071,5.09611121957971));
#71501=CARTESIAN_POINT('Ctrl Pts',(-1.1596958064313,-0.472896248786042,
4.93959315141097));
#71502=CARTESIAN_POINT('Ctrl Pts',(-1.11994048229225,-2.10779096318271,
4.78307508324224));
#71503=CARTESIAN_POINT('Ctrl Pts',(-1.0801851581532,-3.65726477655895,3.73430105247941));
#71504=CARTESIAN_POINT('Ctrl Pts',(-1.04042983401414,-4.41012272047075,
2.27464919360542));
#71505=CARTESIAN_POINT('Ctrl Pts',(-1.02148279339079,-4.76892824792712,
1.57899185298591));
#71506=CARTESIAN_POINT('Ctrl Pts',(-1.00253575276743,-4.94679104943383,
0.79000803331864));
#71507=CARTESIAN_POINT('Ctrl Pts',(-0.983588712144078,-4.94588532464384,
0.00063872631976612));
#71508=CARTESIAN_POINT('Origin',(10.45,0.,0.));
#71509=CARTESIAN_POINT('',(-0.12821128785577,-4.95222891719584,-0.00450272491899106));
#71510=CARTESIAN_POINT('',(-0.23358871214408,-4.95389107247016,-0.00456502003026654));
#71511=CARTESIAN_POINT('',(10.45,-4.954,-6.06690024297599E-16));
#71512=CARTESIAN_POINT('Ctrl Pts',(-0.12821128785577,-4.95222891719584,
-0.00450272491899106));
#71513=CARTESIAN_POINT('Ctrl Pts',(-0.157287870430009,-4.94156622804037,
1.20298200617453));
#71514=CARTESIAN_POINT('Ctrl Pts',(-0.186364453004247,-4.49686831089669,
2.41749706190262));
#71515=CARTESIAN_POINT('Ctrl Pts',(-0.215441035578485,-3.69512492141951,
3.31198769712273));
#71516=CARTESIAN_POINT('Ctrl Pts',(-0.255196359717539,-2.59893116331091,
4.53499129638443));
#71517=CARTESIAN_POINT('Ctrl Pts',(-0.294951683856594,-0.8352740853285,
5.15973899071356));
#71518=CARTESIAN_POINT('Ctrl Pts',(-0.334707007995648,0.786343093374425,
4.89947703640809));
#71519=CARTESIAN_POINT('Ctrl Pts',(-0.374462332134704,2.40796027207744,
4.6392150821026));
#71520=CARTESIAN_POINT('Ctrl Pts',(-0.41421765627376,3.88753755150096,3.4939434791624));
#71521=CARTESIAN_POINT('Ctrl Pts',(-0.453972980412816,4.54596186276556,
1.98933190621096));
#71522=CARTESIAN_POINT('Ctrl Pts',(-0.49372830455187,5.20438617403012,0.484720333259615));
#71523=CARTESIAN_POINT('Ctrl Pts',(-0.533483628690924,5.04165751713587,
-1.37923120970292));
#71524=CARTESIAN_POINT('Ctrl Pts',(-0.573238952829979,4.13246692655254,
-2.74698521869653));
#71525=CARTESIAN_POINT('Ctrl Pts',(-0.612994276969034,3.22327633596919,
-4.11473922769018));
#71526=CARTESIAN_POINT('Ctrl Pts',(-0.65274960110809,1.56762381169672,-4.98629570271487));
#71527=CARTESIAN_POINT('Ctrl Pts',(-0.692504925247145,-0.0745605754309484,
-4.96161782197896));
#71528=CARTESIAN_POINT('Ctrl Pts',(-0.732260249386201,-1.71674496255866,
-4.93693994124305));
#71529=CARTESIAN_POINT('Ctrl Pts',(-0.772015573525258,-3.34546121254158,
-4.01602770474649));
#71530=CARTESIAN_POINT('Ctrl Pts',(-0.811770897664314,-4.21314276955191,
-2.62157179839887));
#71531=CARTESIAN_POINT('Ctrl Pts',(-0.833917694394799,-4.69650864534464,
-1.84475178305996));
#71532=CARTESIAN_POINT('Ctrl Pts',(-0.856064491125284,-4.94369855703214,
-0.920974429500177));
#71533=CARTESIAN_POINT('Ctrl Pts',(-0.878211287855769,-4.9462499908807,
0.00153300580362309));
#71534=CARTESIAN_POINT('Ctrl Pts',(-0.983588712144078,-4.94588532464384,
0.00063872631976612));
#71535=CARTESIAN_POINT('Ctrl Pts',(-0.962780428628378,-4.94489062691812,
-0.866273456175758));
#71536=CARTESIAN_POINT('Ctrl Pts',(-0.941972145112679,-4.72828002074546,
-1.73365058181824));
#71537=CARTESIAN_POINT('Ctrl Pts',(-0.921163861596979,-4.29893345005872,
-2.47838305262693));
#71538=CARTESIAN_POINT('Ctrl Pts',(-0.881408537457925,-3.47864416128752,
-3.90123375300017));
#71539=CARTESIAN_POINT('Ctrl Pts',(-0.841653213318871,-1.88182350929776,
-4.87640546676153));
#71540=CARTESIAN_POINT('Ctrl Pts',(-0.801897889179817,-0.241398248577849,
-4.95630288109652));
#71541=CARTESIAN_POINT('Ctrl Pts',(-0.762142565040761,1.39902701214211,
-5.03620029543151));
#71542=CARTESIAN_POINT('Ctrl Pts',(-0.722387240901707,3.08305688159219,
-4.22082341034007));
#71543=CARTESIAN_POINT('Ctrl Pts',(-0.682631916762651,4.0377363349613,-2.88442310573802));
#71544=CARTESIAN_POINT('Ctrl Pts',(-0.642876592623596,4.99241578833041,
-1.54802280113598));
#71545=CARTESIAN_POINT('Ctrl Pts',(-0.603121268484537,5.21774482561852,
0.309400922976757));
#71546=CARTESIAN_POINT('Ctrl Pts',(-0.563365944345481,4.61029938364994,
1.83530677454728));
#71547=CARTESIAN_POINT('Ctrl Pts',(-0.523610620206427,4.00285394168137,
3.36121262611776));
#71548=CARTESIAN_POINT('Ctrl Pts',(-0.483855296067373,2.56263402045623,
4.55560060514614));
#71549=CARTESIAN_POINT('Ctrl Pts',(-0.444099971928319,0.950688004649234,
4.87025704469468));
#71550=CARTESIAN_POINT('Ctrl Pts',(-0.404344647789265,-0.661258011157765,
5.18491348424322));
#71551=CARTESIAN_POINT('Ctrl Pts',(-0.364589323650211,-2.44493012154658,
4.61983838431192));
#71552=CARTESIAN_POINT('Ctrl Pts',(-0.324833999511157,-3.58163838202674,
3.43439628813785));
#71553=CARTESIAN_POINT('Ctrl Pts',(-0.294418903722131,-4.45128518721321,
2.52746531251895));
#71554=CARTESIAN_POINT('Ctrl Pts',(-0.264003807933106,-4.94225598096154,
1.25742579567596));
#71555=CARTESIAN_POINT('Ctrl Pts',(-0.23358871214408,-4.95389107247016,
-0.00456502003026654));
#71556=CARTESIAN_POINT('Origin',(10.45,0.,0.));
#71557=CARTESIAN_POINT('',(0.621788712144221,-4.9620854618724,0.000611260038189503));
#71558=CARTESIAN_POINT('',(0.516411287855919,-4.96154487360443,0.00161152755429558));
#71559=CARTESIAN_POINT('',(10.45,-4.954,-6.06690024297599E-16));
#71560=CARTESIAN_POINT('Ctrl Pts',(0.621788712144221,-4.9620854618724,0.000611260038189503));
#71561=CARTESIAN_POINT('Ctrl Pts',(0.620999398543369,-4.96214205437354,
0.0332209798384553));
#71562=CARTESIAN_POINT('Ctrl Pts',(0.620210084942517,-4.96184848967099,
0.0658296534178576));
#71563=CARTESIAN_POINT('Ctrl Pts',(0.619420771341666,-4.96120166556195,
0.0984313182539327));
#71564=CARTESIAN_POINT('Ctrl Pts',(0.579665447202611,-4.92862310352016,
1.7404779669271));
#71565=CARTESIAN_POINT('Ctrl Pts',(0.539910123063554,-3.9998853575048,3.36474462281019));
#71566=CARTESIAN_POINT('Ctrl Pts',(0.500154798924499,-2.60127095405371,
4.2257070549654));
#71567=CARTESIAN_POINT('Ctrl Pts',(0.460399474785444,-1.20265655060261,
5.08666948712061));
#71568=CARTESIAN_POINT('Ctrl Pts',(0.420644150646389,0.665834510284238,
5.18432769554799));
#71569=CARTESIAN_POINT('Ctrl Pts',(0.380888826507334,2.14658112548541,4.47385741418942));
#71570=CARTESIAN_POINT('Ctrl Pts',(0.34113350236828,3.62732774068654,3.76338713283087));
#71571=CARTESIAN_POINT('Ctrl Pts',(0.301378178229225,4.72032991020208,2.24478836168642));
#71572=CARTESIAN_POINT('Ctrl Pts',(0.261622854090171,4.92390916954468,0.61508469405576));
#71573=CARTESIAN_POINT('Ctrl Pts',(0.221867529951116,5.12748842888729,-1.01461897357494));
#71574=CARTESIAN_POINT('Ctrl Pts',(0.182112205812063,4.441644778057,-2.7554275376918));
#71575=CARTESIAN_POINT('Ctrl Pts',(0.142356881673009,3.18117447201399,-3.80832504775976));
#71576=CARTESIAN_POINT('Ctrl Pts',(0.102601557533955,1.92070416597101,-4.86122255782768));
#71577=CARTESIAN_POINT('Ctrl Pts',(0.0628462333949009,0.0856072047153433,
-5.22620901384664));
#71578=CARTESIAN_POINT('Ctrl Pts',(0.023090909255847,-1.48182290915536,
-4.73575881529985));
#71579=CARTESIAN_POINT('Ctrl Pts',(-0.0166644148832092,-3.04925302302614,
-4.24530861675302));
#71580=CARTESIAN_POINT('Ctrl Pts',(-0.0564197390222663,-4.34901628951197,
-2.8994217636403));
#71581=CARTESIAN_POINT('Ctrl Pts',(-0.0961750631613226,-4.78453270363744,
-1.31584858498675));
#71582=CARTESIAN_POINT('Ctrl Pts',(-0.106853804726138,-4.90151746817901,
-0.890482446235984));
#71583=CARTESIAN_POINT('Ctrl Pts',(-0.117532546290954,-4.95614492422956,
-0.447966717081306));
#71584=CARTESIAN_POINT('Ctrl Pts',(-0.12821128785577,-4.95222891719584,
-0.00450272491899106));
#71585=CARTESIAN_POINT('Ctrl Pts',(-0.23358871214408,-4.95389107247016,
-0.00456502003026654));
#71586=CARTESIAN_POINT('Ctrl Pts',(-0.224248483794051,-4.95746411436744,
-0.392112127430431));
#71587=CARTESIAN_POINT('Ctrl Pts',(-0.214908255444021,-4.91583320599101,
-0.778900198764109));
#71588=CARTESIAN_POINT('Ctrl Pts',(-0.205568027093992,-4.82608320001309,
-1.15418036291281));
#71589=CARTESIAN_POINT('Ctrl Pts',(-0.165812702954937,-4.44407534694778,
-2.75150582537247));
#71590=CARTESIAN_POINT('Ctrl Pts',(-0.126057378815881,-3.19031523024568,
-4.14034765787489));
#71591=CARTESIAN_POINT('Ctrl Pts',(-0.0863020546768254,-1.64026781029323,
-4.68323957043604));
#71592=CARTESIAN_POINT('Ctrl Pts',(-0.0465467305377712,-0.09022039034083,
-5.22613148299718));
#71593=CARTESIAN_POINT('Ctrl Pts',(-0.00679140639871754,1.75611433286191,
-4.92307347561709));
#71594=CARTESIAN_POINT('Ctrl Pts',(0.0329639177403364,3.05128482198043,
-3.91316653092275));
#71595=CARTESIAN_POINT('Ctrl Pts',(0.0727192418793914,4.346455311099,-2.90325958622838));
#71596=CARTESIAN_POINT('Ctrl Pts',(0.112474566018447,5.09046156613332,-1.18650370421971));
#71597=CARTESIAN_POINT('Ctrl Pts',(0.152229890157502,4.94181120398959,0.449125135908776));
#71598=CARTESIAN_POINT('Ctrl Pts',(0.191985214296558,4.79316084184586,2.08475397603727));
#71599=CARTESIAN_POINT('Ctrl Pts',(0.231740538435613,3.75185386252406,3.63925577428558));
#71600=CARTESIAN_POINT('Ctrl Pts',(0.271495862574668,2.2958410890108,4.39912776099897));
#71601=CARTESIAN_POINT('Ctrl Pts',(0.311251186713722,0.839828315497573,
5.15899974771234));
#71602=CARTESIAN_POINT('Ctrl Pts',(0.351006510852776,-1.03089025220709,
5.12424192289083));
#71603=CARTESIAN_POINT('Ctrl Pts',(0.39076183499183,-2.45767110477701,4.31080782502842));
#71604=CARTESIAN_POINT('Ctrl Pts',(0.430517159130886,-3.88445195734698,
3.49737372716599));
#71605=CARTESIAN_POINT('Ctrl Pts',(0.470272483269942,-4.86729509478217,
1.90526335626261));
#71606=CARTESIAN_POINT('Ctrl Pts',(0.510027807408997,-4.95508408769899,
0.265241488863219));
#71607=CARTESIAN_POINT('Ctrl Pts',(0.512155634224638,-4.95978282371214,
0.177462491124867));
#71608=CARTESIAN_POINT('Ctrl Pts',(0.514283461040279,-4.96191748152808,
0.0895462404344866));
#71609=CARTESIAN_POINT('Ctrl Pts',(0.516411287855919,-4.96154487360443,
0.00161152755429558));
#71610=CARTESIAN_POINT('Origin',(10.45,0.,0.));
#71611=CARTESIAN_POINT('',(1.37178871214422,-4.95039628575946,0.0041823139770486));
#71612=CARTESIAN_POINT('',(1.26641128785591,-4.94901391678264,0.00371957698114467));
#71613=CARTESIAN_POINT('',(10.45,-4.954,-6.06690024297599E-16));
#71614=CARTESIAN_POINT('Ctrl Pts',(1.37178871214422,-4.95039628575946,0.0041823139770486));
#71615=CARTESIAN_POINT('Ctrl Pts',(1.3595313433777,-4.95445714983158,0.513680565467405));
#71616=CARTESIAN_POINT('Ctrl Pts',(1.34727397461118,-4.88211365660348,1.02205349190173));
#71617=CARTESIAN_POINT('Ctrl Pts',(1.33501660584465,-4.72857457585134,1.50459069896108));
#71618=CARTESIAN_POINT('Ctrl Pts',(1.2952612817056,-4.2305887487475,3.06964299046034));
#71619=CARTESIAN_POINT('Ctrl Pts',(1.25550595756654,-2.87846398134063,4.36291580918494));
#71620=CARTESIAN_POINT('Ctrl Pts',(1.21575063342749,-1.29281375092011,4.79080820908328));
#71621=CARTESIAN_POINT('Ctrl Pts',(1.17599530928843,0.292836479500444,5.21870060898162));
#71622=CARTESIAN_POINT('Ctrl Pts',(1.13623998514938,2.1120121729346,4.78121259005364));
#71623=CARTESIAN_POINT('Ctrl Pts',(1.09648466101033,3.32972754987639,3.67914733795509));
#71624=CARTESIAN_POINT('Ctrl Pts',(1.05672933687127,4.54744292681818,2.57708208585653));
#71625=CARTESIAN_POINT('Ctrl Pts',(1.01697401273221,5.16369798726756,0.810439600587436));
#71626=CARTESIAN_POINT('Ctrl Pts',(0.977218688593158,4.89563703241488,-0.80990662278798));
#71627=CARTESIAN_POINT('Ctrl Pts',(0.937463364454104,4.62757607756223,-2.4302528461633));
#71628=CARTESIAN_POINT('Ctrl Pts',(0.89770804031505,3.47519910740752,-3.90430280764505));
#71629=CARTESIAN_POINT('Ctrl Pts',(0.857952716175997,1.96743710216473,-4.55548042908906));
#71630=CARTESIAN_POINT('Ctrl Pts',(0.81819739203694,0.459675096921814,-5.20665805053313));
#71631=CARTESIAN_POINT('Ctrl Pts',(0.778442067897883,-1.40347194340927,
-5.03496333193943));
#71632=CARTESIAN_POINT('Ctrl Pts',(0.738686743758827,-2.76683577454069,
-4.11920265191089));
#71633=CARTESIAN_POINT('Ctrl Pts',(0.699720733220624,-4.10313098937657,
-3.22162374691569));
#71634=CARTESIAN_POINT('Ctrl Pts',(0.660754722682423,-4.95929166230605,
-1.60923137286915));
#71635=CARTESIAN_POINT('Ctrl Pts',(0.621788712144221,-4.9620854618724,0.000611260038189503));
#71636=CARTESIAN_POINT('Ctrl Pts',(0.516411287855919,-4.96154487360443,
0.00161152755429558));
#71637=CARTESIAN_POINT('Ctrl Pts',(0.554038785179335,-4.95495584880843,
-1.55338493607397));
#71638=CARTESIAN_POINT('Ctrl Pts',(0.591666282502749,-4.16432635838302,
-3.11415466245088));
#71639=CARTESIAN_POINT('Ctrl Pts',(0.629293779826165,-2.90381629787506,
-4.02381190810124));
#71640=CARTESIAN_POINT('Ctrl Pts',(0.669049103965218,-1.57202466673599,
-4.98491007377075));
#71641=CARTESIAN_POINT('Ctrl Pts',(0.708804428104274,0.284293443940589,
-5.21917304121447));
#71642=CARTESIAN_POINT('Ctrl Pts',(0.748559752243328,1.81310420902785,-4.61907615122198));
#71643=CARTESIAN_POINT('Ctrl Pts',(0.788315076382382,3.3419149741151,-4.01897926122949));
#71644=CARTESIAN_POINT('Ctrl Pts',(0.828070400521436,4.5432183936131,-2.58452251380076));
#71645=CARTESIAN_POINT('Ctrl Pts',(0.867825724660489,4.8656266737133,-0.974109047094721));
#71646=CARTESIAN_POINT('Ctrl Pts',(0.907581048799544,5.1880349538135,0.636304419611366));
#71647=CARTESIAN_POINT('Ctrl Pts',(0.947336372938597,4.63154809451592,2.42267460559471));
#71648=CARTESIAN_POINT('Ctrl Pts',(0.987091697077652,3.45158871149887,3.56507317319515));
#71649=CARTESIAN_POINT('Ctrl Pts',(1.02684702121671,2.27162932848182,4.70747174079558));
#71650=CARTESIAN_POINT('Ctrl Pts',(1.06660234535576,0.468197421745252,5.20589869001297));
#71651=CARTESIAN_POINT('Ctrl Pts',(1.10635766949482,-1.1309474900082,4.83158039759521));
#71652=CARTESIAN_POINT('Ctrl Pts',(1.14611299363387,-2.73009240176166,4.45726210517745));
#71653=CARTESIAN_POINT('Ctrl Pts',(1.18586831777293,-4.12495031853205,3.21019857112453));
#71654=CARTESIAN_POINT('Ctrl Pts',(1.22562364191198,-4.67529362011846,1.66278108278323));
#71655=CARTESIAN_POINT('Ctrl Pts',(1.23921952389329,-4.86350495381055,1.13358138430474));
#71656=CARTESIAN_POINT('Ctrl Pts',(1.2528154058746,-4.95294485682679,0.56925335383431));
#71657=CARTESIAN_POINT('Ctrl Pts',(1.26641128785591,-4.94901391678264,0.00371957698114467));
#71658=CARTESIAN_POINT('Origin',(10.45,0.,0.));
#71659=CARTESIAN_POINT('',(2.12178871214422,-4.94705618274164,-0.00250727351567559));
#71660=CARTESIAN_POINT('',(2.01641128785591,-4.94803441261571,-0.00322654717566177));
#71661=CARTESIAN_POINT('',(10.45,-4.954,-6.06690024297599E-16));
#71662=CARTESIAN_POINT('Ctrl Pts',(2.12178871214422,-4.94705618274164,-0.00250727351567559));
#71663=CARTESIAN_POINT('Ctrl Pts',(2.09806328821203,-4.94254372780371,0.985354310079251));
#71664=CARTESIAN_POINT('Ctrl Pts',(2.07433786427983,-4.65626453545947,1.97562456187682));
#71665=CARTESIAN_POINT('Ctrl Pts',(2.05061244034764,-4.10584302471708,2.78662228283094));
#71666=CARTESIAN_POINT('Ctrl Pts',(2.01085711620858,-3.18353345354946,4.14556437654064));
#71667=CARTESIAN_POINT('Ctrl Pts',(1.97110179206953,-1.51957111706592,5.00114915495334));
#71668=CARTESIAN_POINT('Ctrl Pts',(1.93134646793047,0.12229978255891,4.96067066574409));
#71669=CARTESIAN_POINT('Ctrl Pts',(1.89159114379142,1.76417068218369,4.92019217653484));
#71670=CARTESIAN_POINT('Ctrl Pts',(1.85183581965237,3.38395014494975,3.98365041970373));
#71671=CARTESIAN_POINT('Ctrl Pts',(1.81208049551331,4.23817352243036,2.58090989469956));
#71672=CARTESIAN_POINT('Ctrl Pts',(1.77232517137425,5.09239689991098,1.17816936969535));
#71673=CARTESIAN_POINT('Ctrl Pts',(1.7325698472352,5.18106419210611,-0.690769923481942));
#71674=CARTESIAN_POINT('Ctrl Pts',(1.69281452309614,4.46347788510464,-2.16808114699834));
#71675=CARTESIAN_POINT('Ctrl Pts',(1.65305919895709,3.7458915781032,-3.64539237051469));
#71676=CARTESIAN_POINT('Ctrl Pts',(1.61330387481804,2.22205167190523,-4.73107552437016));
#71677=CARTESIAN_POINT('Ctrl Pts',(1.57354855067898,0.591387395095607,-4.92681150844132));
#71678=CARTESIAN_POINT('Ctrl Pts',(1.53379322653993,-1.03927688171411,-5.1225474925125));
#71679=CARTESIAN_POINT('Ctrl Pts',(1.49403790240087,-2.77676552913547,-4.42833630679926));
#71680=CARTESIAN_POINT('Ctrl Pts',(1.45428257826181,-3.82358640944574,-3.16281483180562));
#71681=CARTESIAN_POINT('Ctrl Pts',(1.42678462288928,-4.54765128561477,-2.28747916806827));
#71682=CARTESIAN_POINT('Ctrl Pts',(1.39928666751675,-4.94128621808051,-1.13881668105428));
#71683=CARTESIAN_POINT('Ctrl Pts',(1.37178871214422,-4.95039628575946,0.0041823139770486));
#71684=CARTESIAN_POINT('Ctrl Pts',(1.26641128785591,-4.94901391678264,0.00371957698114467));
#71685=CARTESIAN_POINT('Ctrl Pts',(1.29257073001366,-4.94145050906464,-1.08440755917517));
#71686=CARTESIAN_POINT('Ctrl Pts',(1.3187301721714,-4.58822364743875,-2.17699842775093));
#71687=CARTESIAN_POINT('Ctrl Pts',(1.34488961432915,-3.9278017470013,-3.03242226608294));
#71688=CARTESIAN_POINT('Ctrl Pts',(1.3846449384682,-2.92413788589535,-4.33243668397807));
#71689=CARTESIAN_POINT('Ctrl Pts',(1.42440026260725,-1.21098147728112,-5.08469407713871));
#71690=CARTESIAN_POINT('Ctrl Pts',(1.46415558674631,0.425343626546647,-4.94391486202365));
#71691=CARTESIAN_POINT('Ctrl Pts',(1.50391091088537,2.0616687303745,-4.80313564690857));
#71692=CARTESIAN_POINT('Ctrl Pts',(1.54366623502442,3.62116252941581,-3.76931982351759));
#71693=CARTESIAN_POINT('Ctrl Pts',(1.58342155916348,4.38803096918357,-2.31697983959033));
#71694=CARTESIAN_POINT('Ctrl Pts',(1.62317688330253,5.15489940895132,-0.864639855663081));
#71695=CARTESIAN_POINT('Ctrl Pts',(1.66293220744159,5.12914248944555,1.0062242888005));
#71696=CARTESIAN_POINT('Ctrl Pts',(1.70268753158064,4.32258241211102,2.43690226601122));
#71697=CARTESIAN_POINT('Ctrl Pts',(1.7424428557197,3.51602233477653,3.86758024322186));
#71698=CARTESIAN_POINT('Ctrl Pts',(1.78219817985875,1.92865909961348,4.8580720531797));
#71699=CARTESIAN_POINT('Ctrl Pts',(1.8219535039978,0.289078589258305,4.95375059251216));
#71700=CARTESIAN_POINT('Ctrl Pts',(1.86170882813686,-1.35050192109691,5.04942913184462));
#71701=CARTESIAN_POINT('Ctrl Pts',(1.90146415227591,-3.04229970664424,4.25029440055156));
#71702=CARTESIAN_POINT('Ctrl Pts',(1.94121947641497,-4.00979433682249,2.92314227159206));
#71703=CARTESIAN_POINT('Ctrl Pts',(1.96628341356195,-4.61975602436926,2.08643276751731));
#71704=CARTESIAN_POINT('Ctrl Pts',(1.99134735070893,-4.94182652830635,1.03985043263421));
#71705=CARTESIAN_POINT('Ctrl Pts',(2.01641128785591,-4.94803441261571,-0.00322654717566177));
#71706=CARTESIAN_POINT('Origin',(10.45,0.,0.));
#71707=CARTESIAN_POINT('',(2.87178871214422,-4.95959242193685,-0.00316426722878071));
#71708=CARTESIAN_POINT('',(2.76641128785591,-4.96079845433821,-0.0023638398085009));
#71709=CARTESIAN_POINT('',(10.45,-4.954,-6.06690024297599E-16));
#71710=CARTESIAN_POINT('Ctrl Pts',(2.87178871214422,-4.95959242193685,-0.00316426722878071));
#71711=CARTESIAN_POINT('Ctrl Pts',(2.83659523304635,-4.94877395635362,1.45275619981814));
#71712=CARTESIAN_POINT('Ctrl Pts',(2.80140175394849,-4.26913298345277,2.91745981281874));
#71713=CARTESIAN_POINT('Ctrl Pts',(2.76620827485063,-3.14438197780049,3.83875926159369));
#71714=CARTESIAN_POINT('Ctrl Pts',(2.72645295071157,-1.87383862853134,4.87947928001902));
#71715=CARTESIAN_POINT('Ctrl Pts',(2.68669762657252,-0.0353145807779898,
5.22679080605831));
#71716=CARTESIAN_POINT('Ctrl Pts',(2.64694230243346,1.52732366004471,4.72128087792449));
#71717=CARTESIAN_POINT('Ctrl Pts',(2.60718697829441,3.08996190086745,4.21577094979066));
#71718=CARTESIAN_POINT('Ctrl Pts',(2.56743165415535,4.37671433475958,2.85743956748367));
#71719=CARTESIAN_POINT('Ctrl Pts',(2.5276763300163,4.79697281544771,1.26974899040854));
#71720=CARTESIAN_POINT('Ctrl Pts',(2.48792100587724,5.21723129613585,-0.31794158666663));
#71721=CARTESIAN_POINT('Ctrl Pts',(2.44816568173819,4.77099582362001,-2.13499135850988));
#71722=CARTESIAN_POINT('Ctrl Pts',(2.40841035759913,3.66308458847222,-3.34739032508686));
#71723=CARTESIAN_POINT('Ctrl Pts',(2.36865503346008,2.5551733533245,-4.55978929166377));
#71724=CARTESIAN_POINT('Ctrl Pts',(2.32889970932102,0.785586355544888,-5.16753745297437));
#71725=CARTESIAN_POINT('Ctrl Pts',(2.28914438518197,-0.833451404237114,
-4.89168370273089));
#71726=CARTESIAN_POINT('Ctrl Pts',(2.24938906104291,-2.45248916401921,-4.6158299524874));
#71727=CARTESIAN_POINT('Ctrl Pts',(2.20963373690386,-3.92097768580372,-3.45637429068971));
#71728=CARTESIAN_POINT('Ctrl Pts',(2.1698784127648,-4.56489354377007,-1.9454967552875));
#71729=CARTESIAN_POINT('Ctrl Pts',(2.15384851255794,-4.82452938295254,-1.33628989704205));
#71730=CARTESIAN_POINT('Ctrl Pts',(2.13781861235108,-4.95010498821503,-0.669948354799339));
#71731=CARTESIAN_POINT('Ctrl Pts',(2.12178871214422,-4.94705618274164,-0.00250727351567559));
#71732=CARTESIAN_POINT('Ctrl Pts',(2.01641128785591,-4.94803441261571,-0.00322654717566177));
#71733=CARTESIAN_POINT('Ctrl Pts',(2.03110267484798,-4.95167320369055,-0.61463278726675));
#71734=CARTESIAN_POINT('Ctrl Pts',(2.04579406184006,-4.8467881316361,-1.22483465985581));
#71735=CARTESIAN_POINT('Ctrl Pts',(2.06048544883214,-4.62774599501834,-1.79085967322227));
#71736=CARTESIAN_POINT('Ctrl Pts',(2.10024077297119,-4.03501154822675,-3.32253996245104));
#71737=CARTESIAN_POINT('Ctrl Pts',(2.13999609711024,-2.60635117983441,-4.5307310142827));
#71738=CARTESIAN_POINT('Ctrl Pts',(2.17975142124929,-0.997507540568686,
-4.86088367172994));
#71739=CARTESIAN_POINT('Ctrl Pts',(2.21950674538835,0.611336098697178,-5.19103632917721));
#71740=CARTESIAN_POINT('Ctrl Pts',(2.25926206952741,2.40036300883642,-4.64315059223988));
#71741=CARTESIAN_POINT('Ctrl Pts',(2.29901739366647,3.54842543896859,-3.46870123643745));
#71742=CARTESIAN_POINT('Ctrl Pts',(2.33877271780552,4.69648786910072,-2.29425188063505));
#71743=CARTESIAN_POINT('Ctrl Pts',(2.37852804194458,5.20358581922579,-0.493238905967473));
#71744=CARTESIAN_POINT('Ctrl Pts',(2.41828336608364,4.83696575228884,1.10768843758836));
#71745=CARTESIAN_POINT('Ctrl Pts',(2.45803869022269,4.47034568535192,2.7086157811441));
#71746=CARTESIAN_POINT('Ctrl Pts',(2.49779401436174,3.23000760135317,4.10945749358819));
#71747=CARTESIAN_POINT('Ctrl Pts',(2.53754933850079,1.68525586471242,4.66723944468617));
#71748=CARTESIAN_POINT('Ctrl Pts',(2.57730466263984,0.140504128071592,5.22502139578419));
#71749=CARTESIAN_POINT('Ctrl Pts',(2.6170599867789,-1.70866126121123,4.93974358553597));
#71750=CARTESIAN_POINT('Ctrl Pts',(2.65681531091796,-3.01348951475503,3.94234604113384));
#71751=CARTESIAN_POINT('Ctrl Pts',(2.69334730323061,-4.21252327337962,3.02581674062289));
#71752=CARTESIAN_POINT('Ctrl Pts',(2.72987929554326,-4.95191040088857,1.50796260801061));
#71753=CARTESIAN_POINT('Ctrl Pts',(2.76641128785591,-4.96079845433821,-0.0023638398085009));
#71754=CARTESIAN_POINT('Origin',(10.45,0.,0.));
#71755=CARTESIAN_POINT('',(3.62178871214421,-4.95694986960482,0.0041615016535472));
#71756=CARTESIAN_POINT('',(3.5164112878559,-4.95527909032578,0.00446627358905836));
#71757=CARTESIAN_POINT('',(10.45,-4.954,-6.06690024297599E-16));
#71758=CARTESIAN_POINT('Ctrl Pts',(3.62178871214421,-4.95694986960482,0.0041615016535472));
#71759=CARTESIAN_POINT('Ctrl Pts',(3.61488250201974,-4.95952078581773,0.290261447214077));
#71760=CARTESIAN_POINT('Ctrl Pts',(3.60797629189526,-4.93689050256876,0.575954920042386));
#71761=CARTESIAN_POINT('Ctrl Pts',(3.60107008177079,-4.88761713886894,0.856976892700365));
#71762=CARTESIAN_POINT('Ctrl Pts',(3.56131475763173,-4.60397697878091,2.47466871091201));
#71763=CARTESIAN_POINT('Ctrl Pts',(3.52155943349267,-3.43746946477165,3.93756179998155));
#71764=CARTESIAN_POINT('Ctrl Pts',(3.48180410935361,-1.92351137346157,4.57420098891072));
#71765=CARTESIAN_POINT('Ctrl Pts',(3.44204878521456,-0.40955328215158,5.21084017783985));
#71766=CARTESIAN_POINT('Ctrl Pts',(3.40229346107551,1.4518553864592,5.0212254666287));
#71767=CARTESIAN_POINT('Ctrl Pts',(3.36253813693645,2.80634428554344,4.09238835422367));
#71768=CARTESIAN_POINT('Ctrl Pts',(3.3227828127974,4.16083318462772,3.16355124181862));
#71769=CARTESIAN_POINT('Ctrl Pts',(3.28302748865834,5.00840231418543,1.49549172821964));
#71770=CARTESIAN_POINT('Ctrl Pts',(3.24327216451929,4.96002483481713,-0.146165415831287));
#71771=CARTESIAN_POINT('Ctrl Pts',(3.20351684038023,4.91164735544884,-1.78782255988222));
#71772=CARTESIAN_POINT('Ctrl Pts',(3.16376151624118,3.96732326715453,-3.40307733438511));
#71773=CARTESIAN_POINT('Ctrl Pts',(3.12400619210212,2.56048909166029,-4.25054188336929));
#71774=CARTESIAN_POINT('Ctrl Pts',(3.08425086796307,1.15365491616609,-5.09800643235344));
#71775=CARTESIAN_POINT('Ctrl Pts',(3.04449554382401,-0.715689346528007,
-5.17768075581891));
#71776=CARTESIAN_POINT('Ctrl Pts',(3.00474021968496,-2.18953098111131,-4.45299503408005));
#71777=CARTESIAN_POINT('Ctrl Pts',(2.9649848955459,-3.66337261569465,-3.72830931234117));
#71778=CARTESIAN_POINT('Ctrl Pts',(2.92522957140685,-4.74171162216717,-2.1992635453979));
#71779=CARTESIAN_POINT('Ctrl Pts',(2.88547424726779,-4.92959980001093,-0.567676406520532));
#71780=CARTESIAN_POINT('Ctrl Pts',(2.8809124022266,-4.9511595978734,-0.380455000081328));
#71781=CARTESIAN_POINT('Ctrl Pts',(2.87635055718541,-4.96099473182037,-0.191883420129216));
#71782=CARTESIAN_POINT('Ctrl Pts',(2.87178871214422,-4.95959242193685,-0.00316426722878071));
#71783=CARTESIAN_POINT('Ctrl Pts',(2.76641128785591,-4.96079845433821,-0.0023638398085009));
#71784=CARTESIAN_POINT('Ctrl Pts',(2.76963461968231,-4.9615826750649,-0.135624661333186));
#71785=CARTESIAN_POINT('Ctrl Pts',(2.77285795150872,-4.95667989894731,-0.268826879197462));
#71786=CARTESIAN_POINT('Ctrl Pts',(2.77608128333513,-4.94590407681699,-0.401552271201664));
#71787=CARTESIAN_POINT('Ctrl Pts',(2.81583660747418,-4.81299926753041,-2.03853576057897));
#71788=CARTESIAN_POINT('Ctrl Pts',(2.85559193161323,-3.78669853115255,-3.60298546077758));
#71789=CARTESIAN_POINT('Ctrl Pts',(2.89534725575229,-2.33806495601783,-4.37683260189643));
#71790=CARTESIAN_POINT('Ctrl Pts',(2.93510257989134,-0.889431380883065,
-5.15067974301529));
#71791=CARTESIAN_POINT('Ctrl Pts',(2.9748579040304,0.981535033008546,-5.13392432505433));
#71792=CARTESIAN_POINT('Ctrl Pts',(3.01461322816945,2.41607701709231,-4.33425693874514));
#71793=CARTESIAN_POINT('Ctrl Pts',(3.05436855230851,3.85061900117604,-3.53458955243598));
#71794=CARTESIAN_POINT('Ctrl Pts',(3.09412387644756,4.84873655545191,-1.95201019777866));
#71795=CARTESIAN_POINT('Ctrl Pts',(3.13387920058661,4.95230242640418,-0.312908997974529));
#71796=CARTESIAN_POINT('Ctrl Pts',(3.17363452472567,5.05586829735645,1.3261922018296));
#71797=CARTESIAN_POINT('Ctrl Pts',(3.21338984886473,4.26488248498501,3.02181524678059));
#71798=CARTESIAN_POINT('Ctrl Pts',(3.25314517300378,2.94240057952509,3.99568394560838));
#71799=CARTESIAN_POINT('Ctrl Pts',(3.29290049714284,1.61991867406513,4.96955264443619));
#71800=CARTESIAN_POINT('Ctrl Pts',(3.33265582128189,-0.234059324483335,
5.22166699714087));
#71801=CARTESIAN_POINT('Ctrl Pts',(3.37241114542095,-1.76857368205384,4.63630871434686));
#71802=CARTESIAN_POINT('Ctrl Pts',(3.41216646956,-3.30308803962434,4.05095043155286));
#71803=CARTESIAN_POINT('Ctrl Pts',(3.45192179369905,-4.51813875621684,2.62811951326019));
#71804=CARTESIAN_POINT('Ctrl Pts',(3.49167711783811,-4.85602814853717,1.02088294343515));
#71805=CARTESIAN_POINT('Ctrl Pts',(3.49992184117737,-4.92610189637556,0.687563541671297));
#71806=CARTESIAN_POINT('Ctrl Pts',(3.50816656451664,-4.95844961896943,0.346312996487832));
#71807=CARTESIAN_POINT('Ctrl Pts',(3.5164112878559,-4.95527909032578,0.00446627358905836));
#71808=CARTESIAN_POINT('Origin',(10.45,0.,0.));
#71809=CARTESIAN_POINT('',(4.37178871214421,-4.94600446667643,0.00102657243331056));
#71810=CARTESIAN_POINT('',(4.26641128785591,-4.9458133698942,0.00011351553366993));
#71811=CARTESIAN_POINT('',(10.45,-4.954,-6.06690024297599E-16));
#71812=CARTESIAN_POINT('Ctrl Pts',(4.37178871214421,-4.94600446667643,0.00102657243331056));
#71813=CARTESIAN_POINT('Ctrl Pts',(4.35341444685407,-4.94741804923094,0.766486964319902));
#71814=CARTESIAN_POINT('Ctrl Pts',(4.33504018156392,-4.78062055825104,1.53136381525057));
#71815=CARTESIAN_POINT('Ctrl Pts',(4.31666591627377,-4.44240910377579,2.21093013129719));
#71816=CARTESIAN_POINT('Ctrl Pts',(4.27691059213471,-3.71064074254432,3.6812680600143));
#71817=CARTESIAN_POINT('Ctrl Pts',(4.23715526799566,-2.17642450967098,4.75223795738543));
#71818=CARTESIAN_POINT('Ctrl Pts',(4.1973999438566,-0.543952277199825,4.93227397970926));
#71819=CARTESIAN_POINT('Ctrl Pts',(4.15764461971755,1.08851995527132,5.11231000203308));
#71820=CARTESIAN_POINT('Ctrl Pts',(4.11788929557849,2.81924818734023,4.40141214930961));
#71821=CARTESIAN_POINT('Ctrl Pts',(4.07813397143944,3.85384325297807,3.12587633668757));
#71822=CARTESIAN_POINT('Ctrl Pts',(4.03837864730038,4.88843831861585,1.8503405240656));
#71823=CARTESIAN_POINT('Ctrl Pts',(3.99862332316133,5.22690021782261,0.0101667515450213));
#71824=CARTESIAN_POINT('Ctrl Pts',(3.95886799902227,4.71387789035592,-1.55002126617717));
#71825=CARTESIAN_POINT('Ctrl Pts',(3.91911267488322,4.20085556288919,-3.11020928389944));
#71826=CARTESIAN_POINT('Ctrl Pts',(3.87935735074416,2.83634900874898,-4.39041154682338));
#71827=CARTESIAN_POINT('Ctrl Pts',(3.83960202660511,1.24665483736224,-4.80302638003053));
#71828=CARTESIAN_POINT('Ctrl Pts',(3.79984670246605,-0.343039334024497,
-5.21564121323768));
#71829=CARTESIAN_POINT('Ctrl Pts',(3.760091378327,-2.1579211226577,-4.76066861672802));
#71830=CARTESIAN_POINT('Ctrl Pts',(3.72033605418794,-3.36497561389084,-3.64693704479633));
#71831=CARTESIAN_POINT('Ctrl Pts',(3.68748694017336,-4.362343173155,-2.7266805463195));
#71832=CARTESIAN_POINT('Ctrl Pts',(3.65463782615879,-4.94472140880247,-1.3566615202199));
#71833=CARTESIAN_POINT('Ctrl Pts',(3.62178871214421,-4.95694986960482,0.0041615016535472));
#71834=CARTESIAN_POINT('Ctrl Pts',(3.5164112878559,-4.95527909032578,0.00446627358905836));
#71835=CARTESIAN_POINT('Ctrl Pts',(3.54792188865569,-4.94316161126636,-1.30204155896344));
#71836=CARTESIAN_POINT('Ctrl Pts',(3.57943248945548,-4.41222884013198,-2.61725776269742));
#71837=CARTESIAN_POINT('Ctrl Pts',(3.61094309025527,-3.48573346682789,-3.53169556471366));
#71838=CARTESIAN_POINT('Ctrl Pts',(3.65069841439433,-2.31682132475008,-4.68539528168019));
#71839=CARTESIAN_POINT('Ctrl Pts',(3.69045373853338,-0.518268972546314,
-5.20115249425582));
#71840=CARTESIAN_POINT('Ctrl Pts',(3.73020906267244,1.0844037440602,-4.84223913943233));
#71841=CARTESIAN_POINT('Ctrl Pts',(3.76996438681149,2.68707646066668,-4.48332578460886));
#71842=CARTESIAN_POINT('Ctrl Pts',(3.80971971095054,4.09386954167586,-3.24974186238633));
#71843=CARTESIAN_POINT('Ctrl Pts',(3.8494750350896,4.65907723057969,-1.70769163582773));
#71844=CARTESIAN_POINT('Ctrl Pts',(3.88923035922865,5.22428491948354,-0.165641409269088));
#71845=CARTESIAN_POINT('Ctrl Pts',(3.92898568336772,4.94790721628189,1.68487512162573));
#71846=CARTESIAN_POINT('Ctrl Pts',(3.96874100750677,3.95679907664445,2.99448700625796));
#71847=CARTESIAN_POINT('Ctrl Pts',(4.00849633164583,2.96569093700703,4.30409889089015));
#71848=CARTESIAN_POINT('Ctrl Pts',(4.04825165578488,1.2598523609339,5.0728061292599));
#71849=CARTESIAN_POINT('Ctrl Pts',(4.08800697992393,-0.377751620602646,
4.94777880232274));
#71850=CARTESIAN_POINT('Ctrl Pts',(4.12776230406299,-2.01535560213924,4.82275147538557));
#71851=CARTESIAN_POINT('Ctrl Pts',(4.16751762820205,-3.58472498913921,3.80398958314144));
#71852=CARTESIAN_POINT('Ctrl Pts',(4.2072729523411,-4.36553291836083,2.35909595020848));
#71853=CARTESIAN_POINT('Ctrl Pts',(4.22698573084604,-4.75269851434006,1.64264177039663));
#71854=CARTESIAN_POINT('Ctrl Pts',(4.24669850935098,-4.9459807075739,0.821414689135449));
#71855=CARTESIAN_POINT('Ctrl Pts',(4.26641128785591,-4.9458133698942,0.00011351553366993));
#71856=CARTESIAN_POINT('Origin',(10.45,0.,0.));
#71857=CARTESIAN_POINT('',(5.12178871214421,-4.95317189454166,-0.0045626926160558));
#71858=CARTESIAN_POINT('',(5.01641128785591,-4.95486112143639,-0.00451032264997429));
#71859=CARTESIAN_POINT('',(10.45,-4.954,-6.06690024297599E-16));
#71860=CARTESIAN_POINT('Ctrl Pts',(5.12178871214421,-4.95317189454166,-0.0045626926160558));
#71861=CARTESIAN_POINT('Ctrl Pts',(5.09194639168839,-4.94190686525697,1.23412115705393));
#71862=CARTESIAN_POINT('Ctrl Pts',(5.06210407123257,-4.47107698524871,2.48044077126415));
#71863=CARTESIAN_POINT('Ctrl Pts',(5.03226175077675,-3.63070508071573,3.38248300921865));
#71864=CARTESIAN_POINT('Ctrl Pts',(4.9925064266377,-2.51117895299637,4.58416508384454));
#71865=CARTESIAN_POINT('Ctrl Pts',(4.95275110249865,-0.73582588621741,5.17485743910726));
#71866=CARTESIAN_POINT('Ctrl Pts',(4.91299577835959,0.880482543602865,4.88343743496305));
#71867=CARTESIAN_POINT('Ctrl Pts',(4.87324045422053,2.49679097342314,4.59201743081884));
#71868=CARTESIAN_POINT('Ctrl Pts',(4.83348513008148,3.95405476628473,3.41848506726771));
#71869=CARTESIAN_POINT('Ctrl Pts',(4.79372980594242,4.58340254905962,1.90148146561086));
#71870=CARTESIAN_POINT('Ctrl Pts',(4.75397448180337,5.2127503318345,0.38447786395402));
#71871=CARTESIAN_POINT('Ctrl Pts',(4.71421915766431,5.01418210452267,-1.47599697580854));
#71872=CARTESIAN_POINT('Ctrl Pts',(4.67446383352526,4.07883895188329,-2.8260013261475));
#71873=CARTESIAN_POINT('Ctrl Pts',(4.63470850938621,3.14349579924394,-4.17600567648642));
#71874=CARTESIAN_POINT('Ctrl Pts',(4.59495318524715,1.47137772127709,-5.0155395374018));
#71875=CARTESIAN_POINT('Ctrl Pts',(4.55519786110809,-0.170027665622429,
-4.95926418773096));
#71876=CARTESIAN_POINT('Ctrl Pts',(4.51544253696904,-1.811433052522,-4.90298883806013));
#71877=CARTESIAN_POINT('Ctrl Pts',(4.47568721282998,-3.42212574835423,-3.95090427780303));
#71878=CARTESIAN_POINT('Ctrl Pts',(4.43593188869093,-4.26281185147555,-2.54000901764294));
#71879=CARTESIAN_POINT('Ctrl Pts',(4.41455082984202,-4.71494648837151,-1.78120663732256));
#71880=CARTESIAN_POINT('Ctrl Pts',(4.39316977099312,-4.94435956325806,-0.889694957216481));
#71881=CARTESIAN_POINT('Ctrl Pts',(4.37178871214421,-4.94600446667643,0.00102657243331056));
#71882=CARTESIAN_POINT('Ctrl Pts',(4.26641128785591,-4.9458133698942,0.00011351553366993));
#71883=CARTESIAN_POINT('Ctrl Pts',(4.28645383349003,-4.94564323288989,-0.834926874492772));
#71884=CARTESIAN_POINT('Ctrl Pts',(4.30649637912414,-4.74549715038149,-1.67004385651608));
#71885=CARTESIAN_POINT('Ctrl Pts',(4.32653892475826,-4.34583113468504,-2.39519584008996));
#71886=CARTESIAN_POINT('Ctrl Pts',(4.36629424889731,-3.55307495034434,-3.83356862383383));
#71887=CARTESIAN_POINT('Ctrl Pts',(4.40604957303637,-1.9753161102196,-4.83928881769982));
#71888=CARTESIAN_POINT('Ctrl Pts',(4.44580489717543,-0.336732163378222,
-4.95073962289765));
#71889=CARTESIAN_POINT('Ctrl Pts',(4.48556022131448,1.3018517834632,-5.06219042809548));
#71890=CARTESIAN_POINT('Ctrl Pts',(4.52531554545354,3.00126083702131,-4.27937184462509));
#71891=CARTESIAN_POINT('Ctrl Pts',(4.5650708695926,3.9814810610906,-2.96159077587687));
#71892=CARTESIAN_POINT('Ctrl Pts',(4.60482619373165,4.96170128515981,-1.64380970712876));
#71893=CARTESIAN_POINT('Ctrl Pts',(4.6445815178707,5.22273267974038,0.208933846896972));
#71894=CARTESIAN_POINT('Ctrl Pts',(4.68433684200975,4.64476411099516,1.74624675140529));
#71895=CARTESIAN_POINT('Ctrl Pts',(4.72409216614881,4.06679554224988,3.28355965591373));
#71896=CARTESIAN_POINT('Ctrl Pts',(4.76384749028786,2.64982701017859,4.50544191090461));
#71897=CARTESIAN_POINT('Ctrl Pts',(4.80360281442692,1.04423471459389,4.85106021653197));
#71898=CARTESIAN_POINT('Ctrl Pts',(4.84335813856597,-0.561357580990757,
5.19667852215931));
#71899=CARTESIAN_POINT('Ctrl Pts',(4.88311346270503,-2.35557364008884,4.66603287842319));
#71900=CARTESIAN_POINT('Ctrl Pts',(4.92286878684409,-3.51488393769876,3.50268500840274));
#71901=CARTESIAN_POINT('Ctrl Pts',(4.95404962051469,-4.42415237771845,2.59024982590285));
#71902=CARTESIAN_POINT('Ctrl Pts',(4.9852304541853,-4.94285510384131,1.28860444610743));
#71903=CARTESIAN_POINT('Ctrl Pts',(5.01641128785591,-4.95486112143639,-0.00451032264997429));
#71904=CARTESIAN_POINT('Origin',(10.45,0.,0.));
#71905=CARTESIAN_POINT('',(5.87178871214421,-4.96183083301335,0.00119183136441884));
#71906=CARTESIAN_POINT('',(5.76641128785591,-4.96104854467068,0.00214542622588053));
#71907=CARTESIAN_POINT('',(10.45,-4.954,-6.06690024297599E-16));
#71908=CARTESIAN_POINT('Ctrl Pts',(5.87178871214421,-4.96183083301335,0.00119183136441884));
#71909=CARTESIAN_POINT('Ctrl Pts',(5.87023366066177,-4.96203861228002,0.0654461038831422));
#71910=CARTESIAN_POINT('Ctrl Pts',(5.86867860917934,-4.9608988621157,0.129692834246658));
#71911=CARTESIAN_POINT('Ctrl Pts',(5.86712355769691,-4.95838874209328,0.193885979561458));
#71912=CARTESIAN_POINT('Ctrl Pts',(5.82736823355785,-4.89421682479881,1.83500161355999));
#71913=CARTESIAN_POINT('Ctrl Pts',(5.7876129094188,-3.93439383172108,3.44109494591861));
#71914=CARTESIAN_POINT('Ctrl Pts',(5.74785758527974,-2.51947014672649,4.27498314272019));
#71915=CARTESIAN_POINT('Ctrl Pts',(5.70810226114069,-1.10454646173199,5.10887133952172));
#71916=CARTESIAN_POINT('Ctrl Pts',(5.66834693700163,0.765477915179317,5.17055440076632));
#71917=CARTESIAN_POINT('Ctrl Pts',(5.62859161286258,2.23227810220183,4.43172033923825));
#71918=CARTESIAN_POINT('Ctrl Pts',(5.58883628872352,3.69907828922439,3.69288627771017));
#71919=CARTESIAN_POINT('Ctrl Pts',(5.54908096458447,4.76265428635814,2.15353509340939));
#71920=CARTESIAN_POINT('Ctrl Pts',(5.50932564044541,4.93483398563358,0.520215556306828));
#71921=CARTESIAN_POINT('Ctrl Pts',(5.46957031630636,5.10701368490903,-1.11310398079573));
#71922=CARTESIAN_POINT('Ctrl Pts',(5.4298149921673,4.38779708632616,-2.84039187070006));
#71923=CARTESIAN_POINT('Ctrl Pts',(5.39005966802825,3.10729833684114,-3.86883803442999));
#71924=CARTESIAN_POINT('Ctrl Pts',(5.35030434388919,1.82679958735616,-4.89728419815988));
#71925=CARTESIAN_POINT('Ctrl Pts',(5.31054901975014,-0.0149813130309392,
-5.22688863571542));
#71926=CARTESIAN_POINT('Ctrl Pts',(5.27079369561108,-1.57268299194724,-4.70636578451226));
#71927=CARTESIAN_POINT('Ctrl Pts',(5.23103837147203,-3.13038467086359,-4.18584293330909));
#71928=CARTESIAN_POINT('Ctrl Pts',(5.19128304733297,-4.40400712830913,-2.81519279334715));
#71929=CARTESIAN_POINT('Ctrl Pts',(5.15152772319392,-4.80896876270199,-1.22353182637166));
#71930=CARTESIAN_POINT('Ctrl Pts',(5.14161471951068,-4.90994608486552,-0.826650619394185));
#71931=CARTESIAN_POINT('Ctrl Pts',(5.13170171582745,-4.95691390505175,-0.416027933139852));
#71932=CARTESIAN_POINT('Ctrl Pts',(5.12178871214421,-4.95317189454166,-0.0045626926160558));
#71933=CARTESIAN_POINT('Ctrl Pts',(5.01641128785591,-4.95486112143639,-0.00451032264997429));
#71934=CARTESIAN_POINT('Ctrl Pts',(5.02498577832435,-4.95816268432983,-0.360106981047611));
#71935=CARTESIAN_POINT('Ctrl Pts',(5.0335602687928,-4.92314744283978,-0.7150585479163));
#71936=CARTESIAN_POINT('Ctrl Pts',(5.04213475926125,-4.84740043695557,-1.06109394842542));
#71937=CARTESIAN_POINT('Ctrl Pts',(5.0818900834003,-4.49620210248069,-2.6654749389285));
#71938=CARTESIAN_POINT('Ctrl Pts',(5.12164540753936,-3.26940089740912,-4.07818682362985));
#71939=CARTESIAN_POINT('Ctrl Pts',(5.16140073167841,-1.73008787677899,-4.65080716674047));
#71940=CARTESIAN_POINT('Ctrl Pts',(5.20115605581747,-0.19077485614891,-5.22342750985107));
#71941=CARTESIAN_POINT('Ctrl Pts',(5.24091137995653,1.66104998003982,-4.95595631137092));
#71942=CARTESIAN_POINT('Ctrl Pts',(5.28066670409558,2.97541518046736,-3.97116051897005));
#71943=CARTESIAN_POINT('Ctrl Pts',(5.32042202823464,4.28978038089491,-2.98636472656919));
#71944=CARTESIAN_POINT('Ctrl Pts',(5.36017735237369,5.06668594556141,-1.28424434024762));
#71945=CARTESIAN_POINT('Ctrl Pts',(5.39993267651274,4.94953899514414,0.353942225694542));
#71946=CARTESIAN_POINT('Ctrl Pts',(5.4396880006518,4.83239204472687,1.99212879163675));
#71947=CARTESIAN_POINT('Ctrl Pts',(5.47944332479086,3.82119257922581,3.56638153719948));
#71948=CARTESIAN_POINT('Ctrl Pts',(5.51919864892991,2.38007233533071,4.35413218014515));
#71949=CARTESIAN_POINT('Ctrl Pts',(5.55895397306896,0.938952091435656,5.1418828230908));
#71950=CARTESIAN_POINT('Ctrl Pts',(5.59870929720802,-0.932088930853352,
5.14313136341939));
#71951=CARTESIAN_POINT('Ctrl Pts',(5.63846462134707,-2.37425921836786,4.35730473200778));
#71952=CARTESIAN_POINT('Ctrl Pts',(5.67821994548612,-3.81642950588238,3.57147810059616));
#71953=CARTESIAN_POINT('Ctrl Pts',(5.71797526962518,-4.82972905862235,1.99857629744435));
#71954=CARTESIAN_POINT('Ctrl Pts',(5.75773059376423,-4.94906221816879,0.360547534003953));
#71955=CARTESIAN_POINT('Ctrl Pts',(5.76062415846146,-4.95774780243076,0.241324705223826));
#71956=CARTESIAN_POINT('Ctrl Pts',(5.76351772315868,-4.96169754703925,0.121756862533341));
#71957=CARTESIAN_POINT('Ctrl Pts',(5.76641128785591,-4.96104854467068,0.00214542622588053));
#71958=CARTESIAN_POINT('Origin',(10.45,0.,0.));
#71959=CARTESIAN_POINT('',(6.6217887121442,-4.94958263022186,0.00393761749848148));
#71960=CARTESIAN_POINT('',(6.5164112878559,-4.94831334867398,0.00338484824665104));
#71961=CARTESIAN_POINT('',(10.45,-4.954,-6.06690024297599E-16));
#71962=CARTESIAN_POINT('Ctrl Pts',(6.6217887121442,-4.94958263022186,0.00393761749848148));
#71963=CARTESIAN_POINT('Ctrl Pts',(6.6087656054961,-4.95359906417513,0.545489558835211));
#71964=CARTESIAN_POINT('Ctrl Pts',(6.595742498848,-4.87171144893763,1.08586043165447));
#71965=CARTESIAN_POINT('Ctrl Pts',(6.58271939219989,-4.69874473428602,1.59530831277444));
#71966=CARTESIAN_POINT('Ctrl Pts',(6.54296406806084,-4.17073340856723,3.15048759473392));
#71967=CARTESIAN_POINT('Ctrl Pts',(6.50320874392178,-2.7939714110088,4.4175007645021));
#71968=CARTESIAN_POINT('Ctrl Pts',(6.46345341978272,-1.20038049269541,4.81479982590597));
#71969=CARTESIAN_POINT('Ctrl Pts',(6.42369809564367,0.393210425618072,5.21209888730986));
#71970=CARTESIAN_POINT('Ctrl Pts',(6.38394277150462,2.20363026468645,4.73968384034942));
#71971=CARTESIAN_POINT('Ctrl Pts',(6.34418744736557,3.39991210580398,3.61438907197266));
#71972=CARTESIAN_POINT('Ctrl Pts',(6.30443212322651,4.59619394692144,2.48909430359597));
#71973=CARTESIAN_POINT('Ctrl Pts',(6.26467679908746,5.17833779008799,0.710919813803045));
#71974=CARTESIAN_POINT('Ctrl Pts',(6.2249214749484,4.87914468776635,-0.903967812828126));
#71975=CARTESIAN_POINT('Ctrl Pts',(6.18516615080935,4.5799515854447,-2.51885543945934));
#71976=CARTESIAN_POINT('Ctrl Pts',(6.14541082667029,3.39942153763477,-3.97045620292885));
#71977=CARTESIAN_POINT('Ctrl Pts',(6.10565550253123,1.87940754169061,-4.59249801121615));
#71978=CARTESIAN_POINT('Ctrl Pts',(6.06590017839218,0.3593935457465,-5.21453981950343));
#71979=CARTESIAN_POINT('Ctrl Pts',(6.02614485425313,-1.50010439833188,-5.00702267260859));
#71980=CARTESIAN_POINT('Ctrl Pts',(5.98638953011408,-2.84559294961542,-4.06519513134202));
#71981=CARTESIAN_POINT('Ctrl Pts',(5.94818925745746,-4.13845197236205,-3.16020769504152));
#71982=CARTESIAN_POINT('Ctrl Pts',(5.90998898480083,-4.95672667747323,-1.57723226410399));
#71983=CARTESIAN_POINT('Ctrl Pts',(5.87178871214421,-4.96183083301335,0.00119183136441884));
#71984=CARTESIAN_POINT('Ctrl Pts',(5.76641128785591,-4.96104854467068,0.00214542622588053));
#71985=CARTESIAN_POINT('Ctrl Pts',(5.80327304729774,-4.95278076022806,-1.52161106551157));
#71986=CARTESIAN_POINT('Ctrl Pts',(5.84013480673957,-4.19819269721077,-3.05244226706159));
#71987=CARTESIAN_POINT('Ctrl Pts',(5.8769965661814,-2.98071241642748,-3.96718601204142));
#71988=CARTESIAN_POINT('Ctrl Pts',(5.91675189032046,-1.66766268878702,-4.95373507091722));
#71989=CARTESIAN_POINT('Ctrl Pts',(5.95650721445951,0.183803532846682,-5.22367746493987));
#71990=CARTESIAN_POINT('Ctrl Pts',(5.99626253859856,1.72387939810757,-4.65311198923499));
#71991=CARTESIAN_POINT('Ctrl Pts',(6.03601786273762,3.26395526336846,-4.08254651353011));
#71992=CARTESIAN_POINT('Ctrl Pts',(6.07577318687667,4.4926407722565,-2.67147316809771));
#71993=CARTESIAN_POINT('Ctrl Pts',(6.11552851101573,4.84597999071355,-1.06756231349089));
#71994=CARTESIAN_POINT('Ctrl Pts',(6.15528383515478,5.19931920917062,0.536348541116021));
#71995=CARTESIAN_POINT('Ctrl Pts',(6.19503915929383,4.67731213719657,2.33309690489733));
#71996=CARTESIAN_POINT('Ctrl Pts',(6.23479448343289,3.51955546876279,3.49799094708435));
#71997=CARTESIAN_POINT('Ctrl Pts',(6.27454980757194,2.36179880032908,4.66288498927131));
#71998=CARTESIAN_POINT('Ctrl Pts',(6.314305131711,0.568292535435575,5.19592470986405));
#71999=CARTESIAN_POINT('Ctrl Pts',(6.35406045585006,-1.03775959026624,4.8524495253833));
#72000=CARTESIAN_POINT('Ctrl Pts',(6.39381577998912,-2.64381171596806,4.50897434090254));
#72001=CARTESIAN_POINT('Ctrl Pts',(6.43357110412817,-4.0624097024783,3.28898425134839));
#72002=CARTESIAN_POINT('Ctrl Pts',(6.47332642826722,-4.64242944460635,1.7524440691315));
#72003=CARTESIAN_POINT('Ctrl Pts',(6.48768804813011,-4.85196170801539,1.19736857977379));
#72004=CARTESIAN_POINT('Ctrl Pts',(6.502049667993,-4.9520580628245,0.6009827568366));
#72005=CARTESIAN_POINT('Ctrl Pts',(6.5164112878559,-4.94831334867398,0.00338484824665104));
#72006=CARTESIAN_POINT('Origin',(10.45,0.,0.));
#72007=CARTESIAN_POINT('',(7.3717887121442,-4.94758462196668,-0.0029330133969574));
#72008=CARTESIAN_POINT('',(7.2664112878559,-4.94870345086251,-0.00358126079844738));
#72009=CARTESIAN_POINT('',(10.45,-4.954,-6.06690024297599E-16));
#72010=CARTESIAN_POINT('Ctrl Pts',(7.3717887121442,-4.94758462196668,-0.0029330133969574));
#72011=CARTESIAN_POINT('Ctrl Pts',(7.34729755033043,-4.94210089569579,1.01653919561904));
#72012=CARTESIAN_POINT('Ctrl Pts',(7.32280638851666,-4.63564882247797,2.03903518839942));
#72013=CARTESIAN_POINT('Ctrl Pts',(7.29831522670288,-4.05145720843067,2.86511870243504));
#72014=CARTESIAN_POINT('Ctrl Pts',(7.25855990256383,-3.10316708024632,4.20606030888607));
#72015=CARTESIAN_POINT('Ctrl Pts',(7.21880457842477,-1.42304808668591,5.02946551761624));
#72016=CARTESIAN_POINT('Ctrl Pts',(7.17904925428572,0.217739805369029,4.95739851816915));
#72017=CARTESIAN_POINT('Ctrl Pts',(7.13929393014666,1.85852769742402,4.88533151872206));
#72018=CARTESIAN_POINT('Ctrl Pts',(7.09953860600761,3.45998448797345,3.91779231109747));
#72019=CARTESIAN_POINT('Ctrl Pts',(7.05978328186855,4.28705547535841,2.49887295435108));
#72020=CARTESIAN_POINT('Ctrl Pts',(7.0200279577295,5.11412646274337,1.07995359760469));
#72021=CARTESIAN_POINT('Ctrl Pts',(6.98027263359043,5.16681164696395,-0.790345908263659));
#72022=CARTESIAN_POINT('Ctrl Pts',(6.94051730945138,4.42092898789413,-2.25357439965606));
#72023=CARTESIAN_POINT('Ctrl Pts',(6.90076198531233,3.67504632882437,-3.71680289104838));
#72024=CARTESIAN_POINT('Ctrl Pts',(6.86100666117328,2.13059582646437,-4.7729603679649));
#72025=CARTESIAN_POINT('Ctrl Pts',(6.82125133703422,0.4964667933065,-4.9372797585241));
#72026=CARTESIAN_POINT('Ctrl Pts',(6.78149601289517,-1.13766223985146,-5.10159914908331));
#72027=CARTESIAN_POINT('Ctrl Pts',(6.74174068875611,-2.86146980380727,-4.37408045328508));
#72028=CARTESIAN_POINT('Ctrl Pts',(6.70198536461705,-3.88374325884562,-3.08864840831052));
#72029=CARTESIAN_POINT('Ctrl Pts',(6.6752531471261,-4.57113889520683,-2.22430005396414));
#72030=CARTESIAN_POINT('Ctrl Pts',(6.64852092963515,-4.94133819293988,-1.10769301485678));
#72031=CARTESIAN_POINT('Ctrl Pts',(6.6217887121442,-4.94958263022186,0.00393761749848148));
#72032=CARTESIAN_POINT('Ctrl Pts',(6.5164112878559,-4.94831334867398,0.00338484824665104));
#72033=CARTESIAN_POINT('Ctrl Pts',(6.54180499213206,-4.94169207860521,-1.05326647045278));
#72034=CARTESIAN_POINT('Ctrl Pts',(6.56719869640822,-4.6104215531534,-2.11370726000965));
#72035=CARTESIAN_POINT('Ctrl Pts',(6.59259240068438,-3.98543003566754,-2.95627447886375));
#72036=CARTESIAN_POINT('Ctrl Pts',(6.63234772482344,-3.00696938685488,-4.27536256976238));
#72037=CARTESIAN_POINT('Ctrl Pts',(6.6721030489625,-1.30860659148386,-5.06044847667997));
#72038=CARTESIAN_POINT('Ctrl Pts',(6.71185837310155,0.330124637624449,-4.95118461453574));
#72039=CARTESIAN_POINT('Ctrl Pts',(6.75161369724061,1.96885586673271,-4.84192075239152));
#72040=CARTESIAN_POINT('Ctrl Pts',(6.79136902137966,3.5479555295782,-3.83830712118545));
#72041=CARTESIAN_POINT('Ctrl Pts',(6.83112434551871,4.34263065115712,-2.40099362581679));
#72042=CARTESIAN_POINT('Ctrl Pts',(6.87087966965777,5.13730577273608,-0.963680130448044));
#72043=CARTESIAN_POINT('Ctrl Pts',(6.91063499379683,5.14755635304839,0.907333229083402));
#72044=CARTESIAN_POINT('Ctrl Pts',(6.95039031793589,4.36867746511897,2.35326763657341));
#72045=CARTESIAN_POINT('Ctrl Pts',(6.99014564207494,3.58979857718957,3.79920204406338));
#72046=CARTESIAN_POINT('Ctrl Pts',(7.02990096621399,2.02179022101859,4.82005749951193));
#72047=CARTESIAN_POINT('Ctrl Pts',(7.06965629035304,0.384354558565735,4.94727025104672));
#72048=CARTESIAN_POINT('Ctrl Pts',(7.1094116144921,-1.25308110388707,5.0744830025815));
#72049=CARTESIAN_POINT('Ctrl Pts',(7.14916693863116,-2.95994407262174,4.30805305020248));
#72050=CARTESIAN_POINT('Ctrl Pts',(7.18892226277021,-3.95279912936723,2.99976505854306));
#72051=CARTESIAN_POINT('Ctrl Pts',(7.21475193779878,-4.59787306654607,2.14974925814021));
#72052=CARTESIAN_POINT('Ctrl Pts',(7.24058161282734,-4.94154210184746,1.07099836052273));
#72053=CARTESIAN_POINT('Ctrl Pts',(7.2664112878559,-4.94870345086251,-0.00358126079844738));
#72054=CARTESIAN_POINT('Origin',(10.45,0.,0.));
#72055=CARTESIAN_POINT('',(8.1217887121442,-4.96031738439419,-0.00272426264678605));
#72056=CARTESIAN_POINT('',(8.01641128785589,-4.96134628578967,-0.00184569647040522));
#72057=CARTESIAN_POINT('',(10.45,-4.954,-6.06690024297599E-16));
#72058=CARTESIAN_POINT('Ctrl Pts',(8.1217887121442,-4.96031738439419,-0.00272426264678605));
#72059=CARTESIAN_POINT('Ctrl Pts',(8.08582949516476,-4.95049138164272,1.48430270424084));
#72060=CARTESIAN_POINT('Ctrl Pts',(8.04987027818531,-4.23705260128488,2.97950340891386));
#72061=CARTESIAN_POINT('Ctrl Pts',(8.01391106120587,-3.06992698280977,3.89855858119438));
#72062=CARTESIAN_POINT('Ctrl Pts',(7.97415573706681,-1.77959139791648,4.91463566364519));
#72063=CARTESIAN_POINT('Ctrl Pts',(7.93440041292776,0.0652758196799033,
5.22650249375973));
#72064=CARTESIAN_POINT('Ctrl Pts',(7.8946450887887,1.61789670492097,4.69101491609158));
#72065=CARTESIAN_POINT('Ctrl Pts',(7.85488976464965,3.17051759016195,4.15552733842346));
#72066=CARTESIAN_POINT('Ctrl Pts',(7.8151344405106,4.43089214304765,2.77268535297278));
#72067=CARTESIAN_POINT('Ctrl Pts',(7.77537911637154,4.82051943466333,1.17720137224732));
#72068=CARTESIAN_POINT('Ctrl Pts',(7.73562379223248,5.21014672627902,-0.418282608478192));
#72069=CARTESIAN_POINT('Ctrl Pts',(7.69586846809343,4.72902675662464,-2.22640858447849));
#72070=CARTESIAN_POINT('Ctrl Pts',(7.65611314395437,3.59798939625515,-3.41726250019271));
#72071=CARTESIAN_POINT('Ctrl Pts',(7.61635781981532,2.46695203588565,-4.60811641590694));
#72072=CARTESIAN_POINT('Ctrl Pts',(7.57660249567626,0.685997284801031,-5.18169827133508));
#72073=CARTESIAN_POINT('Ctrl Pts',(7.53684717153721,-0.927432156732568,
-4.87473899664856));
#72074=CARTESIAN_POINT('Ctrl Pts',(7.49709184739816,-2.54086159826608,-4.56777972196205));
#72075=CARTESIAN_POINT('Ctrl Pts',(7.4573365232591,-3.98676573024859,-3.380279317161));
#72076=CARTESIAN_POINT('Ctrl Pts',(7.41758119912005,-4.60148716483585,-1.85729011267458));
#72077=CARTESIAN_POINT('Ctrl Pts',(7.40231703679476,-4.83751109283982,-1.27253436132866));
#72078=CARTESIAN_POINT('Ctrl Pts',(7.38705287446948,-4.95100236460309,-0.63832097101446));
#72079=CARTESIAN_POINT('Ctrl Pts',(7.3717887121442,-4.94758462196668,-0.0029330133969574));
#72080=CARTESIAN_POINT('Ctrl Pts',(7.2664112878559,-4.94870345086251,-0.00358126079844738));
#72081=CARTESIAN_POINT('Ctrl Pts',(7.28033693696639,-4.95256437568759,-0.58292338303811));
#72082=CARTESIAN_POINT('Ctrl Pts',(7.29426258607689,-4.85861423275224,-1.16105306049541));
#72083=CARTESIAN_POINT('Ctrl Pts',(7.30818823518738,-4.6613521558272,-1.70147213992685));
#72084=CARTESIAN_POINT('Ctrl Pts',(7.34794355932643,-4.09820298078534,-3.24427531579696));
#72085=CARTESIAN_POINT('Ctrl Pts',(7.38769888346549,-2.69305748594547,-4.47973563659737));
#72086=CARTESIAN_POINT('Ctrl Pts',(7.42745420760454,-1.0908652001314,-4.84078758868063));
#72087=CARTESIAN_POINT('Ctrl Pts',(7.4672095317436,0.511327085682714,-5.20183954076389));
#72088=CARTESIAN_POINT('Ctrl Pts',(7.50696485588265,2.31056616247103,-4.68848312412996));
#72089=CARTESIAN_POINT('Ctrl Pts',(7.54672018002171,3.48101698391448,-3.53634445738549));
#72090=CARTESIAN_POINT('Ctrl Pts',(7.58647550416076,4.65146780535801,-2.38420579064096));
#72091=CARTESIAN_POINT('Ctrl Pts',(7.62623082829981,5.19313037145658,-0.593284873785803));
#72092=CARTESIAN_POINT('Ctrl Pts',(7.66598615243887,4.85738628783773,1.01440120973319));
#72093=CARTESIAN_POINT('Ctrl Pts',(7.70574147657793,4.52164220421889,2.62208729325209));
#72094=CARTESIAN_POINT('Ctrl Pts',(7.74549680071698,3.30849147088272,4.04653854343484));
#72095=CARTESIAN_POINT('Ctrl Pts',(7.78525212485604,1.77475969537718,4.63394425810743));
#72096=CARTESIAN_POINT('Ctrl Pts',(7.82500744899509,0.241027919871597,5.22134997278003));
#72097=CARTESIAN_POINT('Ctrl Pts',(7.86476277313414,-1.61328489780338,4.97171015194241));
#72098=CARTESIAN_POINT('Ctrl Pts',(7.9045180972732,-2.93706534452188,3.99960729642182));
#72099=CARTESIAN_POINT('Ctrl Pts',(7.94181582746743,-4.17901235432128,3.08759787852779));
#72100=CARTESIAN_POINT('Ctrl Pts',(7.97911355766166,-4.95399246532965,1.53968697513372));
#72101=CARTESIAN_POINT('Ctrl Pts',(8.01641128785589,-4.96134628578967,-0.00184569647040522));
#72102=CARTESIAN_POINT('Origin',(10.45,0.,0.));
#72103=CARTESIAN_POINT('',(8.87178871214419,-4.95600107193163,0.00436047568620729));
#72104=CARTESIAN_POINT('',(8.76641128785588,-4.95430821334551,0.00454960891578283));
#72105=CARTESIAN_POINT('',(10.45,-4.954,-6.06690024297599E-16));
#72106=CARTESIAN_POINT('Ctrl Pts',(8.87178871214419,-4.95600107193163,0.00436047568620729));
#72107=CARTESIAN_POINT('Ctrl Pts',(8.86411676413813,-4.95892682062427,0.32233931392055));
#72108=CARTESIAN_POINT('Ctrl Pts',(8.85644481613207,-4.93095453643991,0.639805423207782));
#72109=CARTESIAN_POINT('Ctrl Pts',(8.84877286812601,-4.87022046359406,0.950875032155887));
#72110=CARTESIAN_POINT('Ctrl Pts',(8.80901754398696,-4.55550212212915,2.56280894043786));
#72111=CARTESIAN_POINT('Ctrl Pts',(8.76926221984791,-3.36105884895625,4.00298297070627));
#72112=CARTESIAN_POINT('Ctrl Pts',(8.72950689570886,-1.83512969054333,4.61036980183522));
#72113=CARTESIAN_POINT('Ctrl Pts',(8.6897515715698,-0.309200532130504,5.21775663296414));
#72114=CARTESIAN_POINT('Ctrl Pts',(8.64999624743074,1.54821451152233,4.99235626495374));
#72115=CARTESIAN_POINT('Ctrl Pts',(8.61024092329168,2.88457813261785,4.03762550115916));
#72116=CARTESIAN_POINT('Ctrl Pts',(8.57048559915263,4.22094175371341,3.08289473736455));
#72117=CARTESIAN_POINT('Ctrl Pts',(8.53073027501358,5.03625395225163,1.39883357778585));
#72118=CARTESIAN_POINT('Ctrl Pts',(8.49097495087453,4.95629353888058,-0.241588590869826));
#72119=CARTESIAN_POINT('Ctrl Pts',(8.45121962673548,4.87633312550953,-1.88201075952545));
#72120=CARTESIAN_POINT('Ctrl Pts',(8.41146430259642,3.90110010022918,-3.47879393725799));
#72121=CARTESIAN_POINT('Ctrl Pts',(8.37170897845736,2.47821791730663,-4.29902856993627));
#72122=CARTESIAN_POINT('Ctrl Pts',(8.33195365431831,1.05533573438403,-5.11926320261456));
#72123=CARTESIAN_POINT('Ctrl Pts',(8.29219833017925,-0.815195606180847,
-5.16294929023855));
#72124=CARTESIAN_POINT('Ctrl Pts',(8.2524430060402,-2.27481853068622,-4.41003529954517));
#72125=CARTESIAN_POINT('Ctrl Pts',(8.21268768190114,-3.7344414551916,-3.65712130885178));
#72126=CARTESIAN_POINT('Ctrl Pts',(8.17293235776209,-4.78315596363752,-2.10760723984099));
#72127=CARTESIAN_POINT('Ctrl Pts',(8.13317703362303,-4.93961124176535,-0.472706537942125));
#72128=CARTESIAN_POINT('Ctrl Pts',(8.12938092646342,-4.95455064961378,-0.316595164330307));
#72129=CARTESIAN_POINT('Ctrl Pts',(8.12558481930381,-4.96135468616349,-0.159705259167466));
#72130=CARTESIAN_POINT('Ctrl Pts',(8.1217887121442,-4.96031738439419,-0.00272426264678605));
#72131=CARTESIAN_POINT('Ctrl Pts',(8.01641128785589,-4.96134628578967,-0.00184569647040522));
#72132=CARTESIAN_POINT('Ctrl Pts',(8.01886888180072,-4.96183083818843,-0.103419206165346));
#72133=CARTESIAN_POINT('Ctrl Pts',(8.02132647574554,-4.95898262098761,-0.204965023769395));
#72134=CARTESIAN_POINT('Ctrl Pts',(8.02378406969036,-4.95271562240422,-0.306299407729264));
#72135=CARTESIAN_POINT('Ctrl Pts',(8.06353939382942,-4.85133737780601,-1.9455373661562));
#72136=CARTESIAN_POINT('Ctrl Pts',(8.10329471796847,-3.85533281284763,-3.52944739280642));
#72137=CARTESIAN_POINT('Ctrl Pts',(8.14305004210753,-2.42185933737396,-4.33102859763783));
#72138=CARTESIAN_POINT('Ctrl Pts',(8.18280536624658,-0.988385861900328,
-5.13260980246921));
#72139=CARTESIAN_POINT('Ctrl Pts',(8.22256069038564,0.882556524088673,-5.15186218548167));
#72140=CARTESIAN_POINT('Ctrl Pts',(8.26231601452469,2.33222158062585,-4.37994907075929));
#72141=CARTESIAN_POINT('Ctrl Pts',(8.30207133866375,3.78188663716307,-3.60803595603689));
#72142=CARTESIAN_POINT('Ctrl Pts',(8.3418266628028,4.81027436424862,-2.04495734357959));
#72143=CARTESIAN_POINT('Ctrl Pts',(8.38158198694186,4.94536376301241,-0.408152685971623));
#72144=CARTESIAN_POINT('Ctrl Pts',(8.42133731108091,5.0804531617762,1.22865197163634));
#72145=CARTESIAN_POINT('Ctrl Pts',(8.46109263521996,4.3222442322183,2.93918267439492));
#72146=CARTESIAN_POINT('Ctrl Pts',(8.50084795935901,3.01874826118703,3.93832074610009));
#72147=CARTESIAN_POINT('Ctrl Pts',(8.54060328349807,1.71525229015575,4.93745881780527));
#72148=CARTESIAN_POINT('Ctrl Pts',(8.58035860763713,-0.133530722348902,
5.22520425845695));
#72149=CARTESIAN_POINT('Ctrl Pts',(8.62011393177619,-1.67902549555258,4.66948442002611));
#72150=CARTESIAN_POINT('Ctrl Pts',(8.65986925591524,-3.22452026875627,4.11376458159526));
#72151=CARTESIAN_POINT('Ctrl Pts',(8.69962458005429,-4.46672680265902,2.71457946408189));
#72152=CARTESIAN_POINT('Ctrl Pts',(8.73937990419334,-4.83548313062843,1.1141428350934));
#72153=CARTESIAN_POINT('Ctrl Pts',(8.74839036541419,-4.91906098252792,0.751407214287453));
#72154=CARTESIAN_POINT('Ctrl Pts',(8.75740082663503,-4.95777032957647,0.378333449008531));
#72155=CARTESIAN_POINT('Ctrl Pts',(8.76641128785588,-4.95430821334551,0.00454960891578283));
#72156=CARTESIAN_POINT('Origin',(10.45,0.,0.));
#72157=CARTESIAN_POINT('',(9.62178871214419,-4.94585766451186,0.000506886091347358));
#72158=CARTESIAN_POINT('',(9.51641128785588,-4.94584202552434,-0.00041315751885764));
#72159=CARTESIAN_POINT('',(10.45,-4.954,-6.06690024297599E-16));
#72160=CARTESIAN_POINT('Ctrl Pts',(9.62178871214419,-4.94585766451186,0.000506886091347358));
#72161=CARTESIAN_POINT('Ctrl Pts',(9.60264870897246,-4.94658353356567,0.797926455850933));
#72162=CARTESIAN_POINT('Ctrl Pts',(9.58350870580073,-4.76490303293466,1.59503395194384));
#72163=CARTESIAN_POINT('Ctrl Pts',(9.564368702629,-4.39903952636143,2.29601000352735));
#72164=CARTESIAN_POINT('Ctrl Pts',(9.52461337848995,-3.63911163272578,3.75199357335154));
#72165=CARTESIAN_POINT('Ctrl Pts',(9.4848580543509,-2.08456986568594,4.7932408373652));
#72166=CARTESIAN_POINT('Ctrl Pts',(9.44510273021185,-0.448935340223443,
4.94182838138743));
#72167=CARTESIAN_POINT('Ctrl Pts',(9.40534740607279,1.18669918523901,5.09041592540966));
#72168=CARTESIAN_POINT('Ctrl Pts',(9.36559208193373,2.90342646912413,4.34634374944051));
#72169=CARTESIAN_POINT('Ctrl Pts',(9.32583675779467,3.9132836585268,3.05113449370803));
#72170=CARTESIAN_POINT('Ctrl Pts',(9.28608143365562,4.9231408479295,1.75592523797551));
#72171=CARTESIAN_POINT('Ctrl Pts',(9.24632610951657,5.22612794284971,-0.090421097520369));
#72172=CARTESIAN_POINT('Ctrl Pts',(9.20657078537752,4.68317650886116,-1.64044764550375));
#72173=CARTESIAN_POINT('Ctrl Pts',(9.16681546123846,4.14022507487263,-3.19047419348709));
#72174=CARTESIAN_POINT('Ctrl Pts',(9.1270601370994,2.7513351119754,-4.44418095395794));
#72175=CARTESIAN_POINT('Ctrl Pts',(9.08730481296035,1.15399500158496,-4.82612745657476));
#72176=CARTESIAN_POINT('Ctrl Pts',(9.04754948882129,-0.443345108805517,
-5.20807395919159));
#72177=CARTESIAN_POINT('Ctrl Pts',(9.00779416468224,-2.24913536668921,-4.71826020395433));
#72178=CARTESIAN_POINT('Ctrl Pts',(8.96803884054319,-3.43453379075257,-3.58150643318794));
#72179=CARTESIAN_POINT('Ctrl Pts',(8.93595546441019,-4.39117505403748,-2.66412242015528));
#72180=CARTESIAN_POINT('Ctrl Pts',(8.90387208827719,-4.94376586182561,-1.32539758072267));
#72181=CARTESIAN_POINT('Ctrl Pts',(8.87178871214419,-4.95600107193163,0.00436047568620729));
#72182=CARTESIAN_POINT('Ctrl Pts',(8.76641128785588,-4.95430821334551,0.00454960891578283));
#72183=CARTESIAN_POINT('Ctrl Pts',(8.79715615077409,-4.94249502350775,-1.2708493571334));
#72184=CARTESIAN_POINT('Ctrl Pts',(8.8279010136923,-4.43969511014743,-2.55451546117548));
#72185=CARTESIAN_POINT('Ctrl Pts',(8.85864587661051,-3.55305158563404,-3.4639624411078));
#72186=CARTESIAN_POINT('Ctrl Pts',(8.89840120074957,-2.40655759063403,-4.63994294785716));
#72187=CARTESIAN_POINT('Ctrl Pts',(8.93815652488862,-0.618263478597702,
-5.19021582089223));
#72188=CARTESIAN_POINT('Ctrl Pts',(8.97791184902767,0.991019347533268,-4.86221061004117));
#72189=CARTESIAN_POINT('Ctrl Pts',(9.01766717316673,2.60030217366424,-4.53420539919011));
#72190=CARTESIAN_POINT('Ctrl Pts',(9.05742249730579,4.03057371388998,-3.32792210445298));
#72191=CARTESIAN_POINT('Ctrl Pts',(9.09717782144485,4.62535180366144,-1.79703423894704));
#72192=CARTESIAN_POINT('Ctrl Pts',(9.1369331455839,5.22012989343289,-0.266146373441135));
#72193=CARTESIAN_POINT('Ctrl Pts',(9.17668846972296,4.9794145327501,1.58934606283357));
#72194=CARTESIAN_POINT('Ctrl Pts',(9.21644379386201,4.01369197305335,2.91778822210064));
#72195=CARTESIAN_POINT('Ctrl Pts',(9.25619911800106,3.04796941335657,4.24623038136774));
#72196=CARTESIAN_POINT('Ctrl Pts',(9.29595444214012,1.35723965464579,5.04762226362717));
#72197=CARTESIAN_POINT('Ctrl Pts',(9.33570976627917,-0.282467087522345,
4.95413198330936));
#72198=CARTESIAN_POINT('Ctrl Pts',(9.37546509041823,-1.92217382969048,4.86064170299156));
#72199=CARTESIAN_POINT('Ctrl Pts',(9.41522041455728,-3.51085755531596,3.87226926009653));
#72200=CARTESIAN_POINT('Ctrl Pts',(9.45497573869634,-4.31932628815499,2.44266898699667));
#72201=CARTESIAN_POINT('Ctrl Pts',(9.47545425508285,-4.73577969538968,1.70626214708662));
#72202=CARTESIAN_POINT('Ctrl Pts',(9.49593277146937,-4.94520911289263,0.852778928698556));
#72203=CARTESIAN_POINT('Ctrl Pts',(9.51641128785588,-4.94584202552434,-0.00041315751885764));
#72204=CARTESIAN_POINT('Origin',(10.45,0.,0.));
#72205=CARTESIAN_POINT('',(10.3717887121442,-4.95413490991508,-0.00455749466325095));
#72206=CARTESIAN_POINT('',(10.2664112878559,-4.95582936423354,-0.0043891145566411));
#72207=CARTESIAN_POINT('',(10.45,-4.954,-6.06690024297599E-16));
#72208=CARTESIAN_POINT('Ctrl Pts',(10.3717887121442,-4.95413490991508,-0.00455749466325095));
#72209=CARTESIAN_POINT('Ctrl Pts',(10.3411806538068,-4.94239235035036,1.26527993119002));
#72210=CARTESIAN_POINT('Ctrl Pts',(10.3105725954694,-4.44452057764309,2.54329575077959));
#72211=CARTESIAN_POINT('Ctrl Pts',(10.279964537132,-3.56494056432348,3.45172557768268));
#72212=CARTESIAN_POINT('Ctrl Pts',(10.2402092129929,-2.42249669708122,4.63164107013291));
#72213=CARTESIAN_POINT('Ctrl Pts',(10.2004538888539,-0.636105165059572,
5.18805931624687));
#72214=CARTESIAN_POINT('Ctrl Pts',(10.1606985647148,0.974295896435707,4.86558919319915));
#72215=CARTESIAN_POINT('Ctrl Pts',(10.1209432405758,2.58469695793099,4.54311907015144));
#72216=CARTESIAN_POINT('Ctrl Pts',(10.0811879164367,4.01910754889984,3.34176057794207));
#72217=CARTESIAN_POINT('Ctrl Pts',(10.0414325922977,4.61914571659599,1.81292678827382));
#72218=CARTESIAN_POINT('Ctrl Pts',(10.0016772681586,5.2191838842921,0.28409299860565));
#72219=CARTESIAN_POINT('Ctrl Pts',(9.96192194401955,4.98484962871553,-1.57221608852144));
#72220=CARTESIAN_POINT('Ctrl Pts',(9.9221666198805,4.02370032970805,-2.90397078971107));
#72221=CARTESIAN_POINT('Ctrl Pts',(9.88241129574144,3.06255103070049,-4.23572549090081));
#72222=CARTESIAN_POINT('Ctrl Pts',(9.84265597160239,1.37458668826192,-5.04292580615308));
#72223=CARTESIAN_POINT('Ctrl Pts',(9.80290064746333,-0.265431784004649,
-4.95507382980597));
#72224=CARTESIAN_POINT('Ctrl Pts',(9.76314532332428,-1.90545025627113,-4.86722185345886));
#72225=CARTESIAN_POINT('Ctrl Pts',(9.72338999918523,-3.49752285836557,-3.88431758551248));
#72226=CARTESIAN_POINT('Ctrl Pts',(9.68363467504617,-4.31090214929706,-2.45750551372196));
#72227=CARTESIAN_POINT('Ctrl Pts',(9.66301935407884,-4.73268402414932,-1.71762502080647));
#72228=CARTESIAN_POINT('Ctrl Pts',(9.64240403311151,-4.94507584523051,-0.858378048708709));
#72229=CARTESIAN_POINT('Ctrl Pts',(9.62178871214419,-4.94585766451186,0.000506886091347358));
#72230=CARTESIAN_POINT('Ctrl Pts',(9.51641128785588,-4.94584202552434,-0.00041315751885764));
#72231=CARTESIAN_POINT('Ctrl Pts',(9.53568809560842,-4.94643779793751,-0.803538711713373));
#72232=CARTESIAN_POINT('Ctrl Pts',(9.55496490336096,-4.76202302770542,-1.60640629932515));
#72233=CARTESIAN_POINT('Ctrl Pts',(9.57424171111351,-4.39111928801005,-2.31112153770593));
#72234=CARTESIAN_POINT('Ctrl Pts',(9.61399703525256,-3.62618981497348,-3.76448368600399));
#72235=CARTESIAN_POINT('Ctrl Pts',(9.65375235939162,-2.06807712884795,-4.80037987929536));
#72236=CARTESIAN_POINT('Ctrl Pts',(9.69350768353067,-0.43194136533549,-4.94334279819782));
#72237=CARTESIAN_POINT('Ctrl Pts',(9.73326300766973,1.20419439817692,-5.08630571710027));
#72238=CARTESIAN_POINT('Ctrl Pts',(9.77301833180877,2.91835323907617,-4.33633536161367));
#72239=CARTESIAN_POINT('Ctrl Pts',(9.81277365594783,3.92375119738988,-3.03766158493069));
#72240=CARTESIAN_POINT('Ctrl Pts',(9.85252898008688,4.92914915570359,-1.7389878082477));
#72241=CARTESIAN_POINT('Ctrl Pts',(9.89228430422595,5.22578623143186,0.108389389631662));
#72242=CARTESIAN_POINT('Ctrl Pts',(9.932039628365,4.67750859358339,1.65653998458705));
#72243=CARTESIAN_POINT('Ctrl Pts',(9.97179495250406,4.12923095573491,3.20469057954244));
#72244=CARTESIAN_POINT('Ctrl Pts',(10.0115502766431,2.73603860430971,4.4536145715738));
#72245=CARTESIAN_POINT('Ctrl Pts',(10.0513056007822,1.13739467953943,4.83006673934611));
#72246=CARTESIAN_POINT('Ctrl Pts',(10.0910609249212,-0.461249245230903,
5.20651890711843));
#72247=CARTESIAN_POINT('Ctrl Pts',(10.1308162490603,-2.26534474334642,4.71049925063156));
#72248=CARTESIAN_POINT('Ctrl Pts',(10.1705715731993,-3.44682771344815,3.56967646676669));
#72249=CARTESIAN_POINT('Ctrl Pts',(10.2025181447515,-4.3962434473012,2.65293443328137));
#72250=CARTESIAN_POINT('Ctrl Pts',(10.2344647163037,-4.94361315650885,1.31981701000383));
#72251=CARTESIAN_POINT('Ctrl Pts',(10.2664112878559,-4.95582936423354,-0.0043891145566411));
#72252=CARTESIAN_POINT('Origin',(10.45,0.,0.));
#72253=CARTESIAN_POINT('',(11.1217887121442,-4.96143148149888,0.00174928188396612));
#72254=CARTESIAN_POINT('',(11.0164112878559,-4.96043743303216,0.00264048323268159));
#72255=CARTESIAN_POINT('',(10.45,-4.954,-6.06690024297599E-16));
#72256=CARTESIAN_POINT('Ctrl Pts',(11.1217887121442,-4.96143148149888,0.00174928188396612));
#72257=CARTESIAN_POINT('Ctrl Pts',(11.1194679227802,-4.96186820307519,0.097664209125269));
#72258=CARTESIAN_POINT('Ctrl Pts',(11.1171471334162,-4.95932850373442,0.193555553937918));
#72259=CARTESIAN_POINT('Ctrl Pts',(11.1148263440521,-4.95373941917952,0.289268832843753));
#72260=CARTESIAN_POINT('Ctrl Pts',(11.0750710199131,-4.85799791348065,1.92884564507605));
#72261=CARTESIAN_POINT('Ctrl Pts',(11.035315695774,-3.8674451554344,3.51617081775305));
#72262=CARTESIAN_POINT('Ctrl Pts',(10.995560371635,-2.43673622305456,4.3226759385873));
#72263=CARTESIAN_POINT('Ctrl Pts',(10.9558050474959,-1.00602729067465,5.1291810594216));
#72264=CARTESIAN_POINT('Ctrl Pts',(10.9160497233569,0.864837816038947,5.15486612841308));
#72265=CARTESIAN_POINT('Ctrl Pts',(10.8762943992178,2.31714832763268,4.38794192287648));
#72266=CARTESIAN_POINT('Ctrl Pts',(10.8365390750788,3.76945883922638,3.62101771733989));
#72267=CARTESIAN_POINT('Ctrl Pts',(10.7967837509397,4.8032147557003,2.06148423727525));
#72268=CARTESIAN_POINT('Ctrl Pts',(10.7570284268006,4.94393112606734,0.425153750413206));
#72269=CARTESIAN_POINT('Ctrl Pts',(10.7172731026616,5.08464749643438,-1.21117673644879));
#72270=CARTESIAN_POINT('Ctrl Pts',(10.6775177785225,4.3323243206947,-2.92430423010813));
#72271=CARTESIAN_POINT('Ctrl Pts',(10.6377624543835,3.03227137601965,-3.92791814998222));
#72272=CARTESIAN_POINT('Ctrl Pts',(10.5980071302444,1.73221843134455,-4.93153206985633));
#72273=CARTESIAN_POINT('Ctrl Pts',(10.5582518061054,-0.115564282265953,
-5.22563241594505));
#72274=CARTESIAN_POINT('Ctrl Pts',(10.5184964819663,-1.66296061250703,-4.67522969404051));
#72275=CARTESIAN_POINT('Ctrl Pts',(10.4787411578273,-3.2103569427481,-4.12482697213597));
#72276=CARTESIAN_POINT('Ctrl Pts',(10.4389858336882,-4.45736688961978,-2.72992118223817));
#72277=CARTESIAN_POINT('Ctrl Pts',(10.3992305095492,-4.83162376182417,-1.13076191789604));
#72278=CARTESIAN_POINT('Ctrl Pts',(10.3900832437475,-4.91773617977793,-0.762812840208963));
#72279=CARTESIAN_POINT('Ctrl Pts',(10.3809359779458,-4.95764419208994,-0.384050382814731));
#72280=CARTESIAN_POINT('Ctrl Pts',(10.3717887121442,-4.95413490991508,-0.00455749466325095));
#72281=CARTESIAN_POINT('Ctrl Pts',(10.2664112878559,-4.95582936423354,-0.0043891145566411));
#72282=CARTESIAN_POINT('Ctrl Pts',(10.2742200404428,-4.95881539181137,-0.328066977259775));
#72283=CARTESIAN_POINT('Ctrl Pts',(10.2820287930296,-4.92982769828898,-0.651212418182936));
#72284=CARTESIAN_POINT('Ctrl Pts',(10.2898375456165,-4.86692238031873,-0.967614544916926));
#72285=CARTESIAN_POINT('Ctrl Pts',(10.3295928697555,-4.54666363499955,-2.57845686149303));
#72286=CARTESIAN_POINT('Ctrl Pts',(10.3693481938946,-3.34727570227304,-4.01451558340236));
#72287=CARTESIAN_POINT('Ctrl Pts',(10.4091035180337,-1.81926718422331,-4.61665228016908));
#72288=CARTESIAN_POINT('Ctrl Pts',(10.4488588421727,-0.291258666173671,
-5.21878897693576));
#72289=CARTESIAN_POINT('Ctrl Pts',(10.4886141663118,1.56537043719918,-4.98700364855995));
#72290=CARTESIAN_POINT('Ctrl Pts',(10.5283694904508,2.8984435578328,-4.02768373952569));
#72291=CARTESIAN_POINT('Ctrl Pts',(10.5681248145899,4.23151667846645,-3.0683638304914));
#72292=CARTESIAN_POINT('Ctrl Pts',(10.6078801387289,5.04103381636084,-1.38150934079872));
#72293=CARTESIAN_POINT('Ctrl Pts',(10.647635462868,4.95543366446481,0.25862822868162));
#72294=CARTESIAN_POINT('Ctrl Pts',(10.687390787007,4.86983351256878,1.89876579816191));
#72295=CARTESIAN_POINT('Ctrl Pts',(10.7271461111461,3.88911607088231,3.49218644742981));
#72296=CARTESIAN_POINT('Ctrl Pts',(10.7669014352851,2.46342209297707,4.30752399359709));
#72297=CARTESIAN_POINT('Ctrl Pts',(10.8066567594242,1.03772811507175,5.12286153976442));
#72298=CARTESIAN_POINT('Ctrl Pts',(10.8464120835633,-0.832942399052437,
5.16011598283106));
#72299=CARTESIAN_POINT('Ctrl Pts',(10.8861674077023,-2.28996799624358,4.40218785829981));
#72300=CARTESIAN_POINT('Ctrl Pts',(10.9259227318414,-3.74699359343464,3.64425973376861));
#72301=CARTESIAN_POINT('Ctrl Pts',(10.9656780559804,-4.79037427369275,2.09114904163959));
#72302=CARTESIAN_POINT('Ctrl Pts',(11.0054333801195,-4.94120740338486,0.455720045989624));
#72303=CARTESIAN_POINT('Ctrl Pts',(11.0090926826983,-4.95509092898562,0.30518600631491));
#72304=CARTESIAN_POINT('Ctrl Pts',(11.0127519852771,-4.96141244178186,0.153954533696844));
#72305=CARTESIAN_POINT('Ctrl Pts',(11.0164112878559,-4.96043743303216,0.00264048323268159));
#72306=CARTESIAN_POINT('Origin',(10.45,0.,0.));
#72307=CARTESIAN_POINT('',(11.8717887121442,-4.94883061351211,0.0036397403582919));
#72308=CARTESIAN_POINT('',(11.7664112878559,-4.94768798497716,0.00300517406437754));
#72309=CARTESIAN_POINT('',(10.45,-4.954,-6.06690024297599E-16));
#72310=CARTESIAN_POINT('Ctrl Pts',(11.8717887121442,-4.94883061351211,0.0036397403582919));
#72311=CARTESIAN_POINT('Ctrl Pts',(11.8579998676145,-4.95272244476274,0.577253372849803));
#72312=CARTESIAN_POINT('Ctrl Pts',(11.8442110230848,-4.86065783541348,1.14965663724327));
#72313=CARTESIAN_POINT('Ctrl Pts',(11.8304221785551,-4.66717465558493,1.68543508479369));
#72314=CARTESIAN_POINT('Ctrl Pts',(11.7906668544161,-4.10933338665354,3.23016537769288));
#72315=CARTESIAN_POINT('Ctrl Pts',(11.750911530277,-2.70844405945764,4.47044964480083));
#72316=CARTESIAN_POINT('Ctrl Pts',(11.711156206138,-1.10750265898756,4.83700822318128));
#72317=CARTESIAN_POINT('Ctrl Pts',(11.6714008819989,0.493438741482567,5.20356680156174));
#72318=CARTESIAN_POINT('Ctrl Pts',(11.6316455578599,2.29443221522694,4.69639969121456));
#72319=CARTESIAN_POINT('Ctrl Pts',(11.5918902337208,3.46883746302233,3.54829217313353));
#72320=CARTESIAN_POINT('Ctrl Pts',(11.5521349095817,4.64324271081769,2.40018465505254));
#72321=CARTESIAN_POINT('Ctrl Pts',(11.5123795854427,5.19105973266421,0.611136729237761));
#72322=CARTESIAN_POINT('Ctrl Pts',(11.4726242613036,4.86084529266991,-0.99769420741862));
#72323=CARTESIAN_POINT('Ctrl Pts',(11.4328689371646,4.5306308526756,-2.606525144075));
#72324=CARTESIAN_POINT('Ctrl Pts',(11.3931136130255,3.32238495084048,-4.03513909157292));
#72325=CARTESIAN_POINT('Ctrl Pts',(11.3533582888865,1.79068191982516,-4.62781470597075));
#72326=CARTESIAN_POINT('Ctrl Pts',(11.3136029647474,0.258978888809789,-5.2204903203686));
#72327=CARTESIAN_POINT('Ctrl Pts',(11.2738476406084,-1.59618127138576,-4.97722760166629));
#72328=CARTESIAN_POINT('Ctrl Pts',(11.2340923164693,-2.92329622480781,-4.00968201642128));
#72329=CARTESIAN_POINT('Ctrl Pts',(11.1966577816943,-4.17293842871952,-3.09861866474033));
#72330=CARTESIAN_POINT('Ctrl Pts',(11.1592232469192,-4.95438712439842,-1.54536685667392));
#72331=CARTESIAN_POINT('Ctrl Pts',(11.1217887121442,-4.96143148149888,0.00174928188396612));
#72332=CARTESIAN_POINT('Ctrl Pts',(11.0164112878559,-4.96043743303216,0.00264048323268159));
#72333=CARTESIAN_POINT('Ctrl Pts',(11.0525073094161,-4.95081977062441,-1.48994864005102));
#72334=CARTESIAN_POINT('Ctrl Pts',(11.0886033309764,-4.23123553683844,-2.99057275780401));
#72335=CARTESIAN_POINT('Ctrl Pts',(11.1246993525366,-3.05650459196268,-3.90909082049691));
#72336=CARTESIAN_POINT('Ctrl Pts',(11.1644546766757,-1.76268307172244,-4.92072539216228));
#72337=CARTESIAN_POINT('Ctrl Pts',(11.2042100008148,0.0832455478841035,
-5.22624723632215));
#72338=CARTESIAN_POINT('Ctrl Pts',(11.2439653249538,1.63401612753167,-4.68542449075305));
#72339=CARTESIAN_POINT('Ctrl Pts',(11.2837206490929,3.18478670717929,-4.14460174518394));
#72340=CARTESIAN_POINT('Ctrl Pts',(11.3234759732319,4.44039924686796,-2.75743440988578));
#72341=CARTESIAN_POINT('Ctrl Pts',(11.363231297371,4.82453854021408,-1.16062019522803));
#72342=CARTESIAN_POINT('Ctrl Pts',(11.40298662151,5.20867783356018,0.436194019429668));
#72343=CARTESIAN_POINT('Ctrl Pts',(11.4427419456491,4.72134388056388,2.24265511344687));
#72344=CARTESIAN_POINT('Ctrl Pts',(11.4824972697881,3.58621871594613,3.42961319757489));
#72345=CARTESIAN_POINT('Ctrl Pts',(11.5222525939272,2.4510935513283,4.61657128170297));
#72346=CARTESIAN_POINT('Ctrl Pts',(11.5620079180662,0.668177175088912,5.18402635594168));
#72347=CARTESIAN_POINT('Ctrl Pts',(11.6017632422053,-0.944187343665765,
4.87152148960091));
#72348=CARTESIAN_POINT('Ctrl Pts',(11.6415185663444,-2.55655186242035,4.55901662326017));
#72349=CARTESIAN_POINT('Ctrl Pts',(11.6812738904834,-3.99836452369029,3.36655181634004));
#72350=CARTESIAN_POINT('Ctrl Pts',(11.7210292146225,-4.60784588900943,1.84145801655129));
#72351=CARTESIAN_POINT('Ctrl Pts',(11.7361565723669,-4.83976055330752,1.26114229776651));
#72352=CARTESIAN_POINT('Ctrl Pts',(11.7512839301114,-4.95116280464578,0.632665560951985));
#72353=CARTESIAN_POINT('Ctrl Pts',(11.7664112878559,-4.94768798497716,0.00300517406437754));
#72354=CARTESIAN_POINT('Origin',(10.45,0.,0.));
#72355=CARTESIAN_POINT('',(12.6217887121442,-4.94819583789813,-0.00332016549414282));
#72356=CARTESIAN_POINT('',(12.5164112878559,-4.9494435771879,-0.00388817816282298));
#72357=CARTESIAN_POINT('',(10.45,-4.954,-6.06690024297599E-16));
#72358=CARTESIAN_POINT('Ctrl Pts',(12.6217887121442,-4.94819583789813,-0.00332016549414282));
#72359=CARTESIAN_POINT('Ctrl Pts',(12.5965318124488,-4.94174563760587,1.04770119792139));
#72360=CARTESIAN_POINT('Ctrl Pts',(12.5712749127535,-4.61431031278361,2.1023936236481));
#72361=CARTESIAN_POINT('Ctrl Pts',(12.5460180130581,-3.99557088579909,2.94255399055693));
#72362=CARTESIAN_POINT('Ctrl Pts',(12.5062626889191,-3.02165141135531,4.26499847575186));
#72363=CARTESIAN_POINT('Ctrl Pts',(12.46650736478,-1.32599801317663,5.05591915668782));
#72364=CARTESIAN_POINT('Ctrl Pts',(12.426752040641,0.313099185600184,4.95229033789058));
#72365=CARTESIAN_POINT('Ctrl Pts',(12.3869967165019,1.95219638437709,4.84866151909333));
#72366=CARTESIAN_POINT('Ctrl Pts',(12.3472413923628,3.53473738375218,3.85048320056279));
#72367=CARTESIAN_POINT('Ctrl Pts',(12.3074860682238,4.33434966526403,2.41591052607779));
#72368=CARTESIAN_POINT('Ctrl Pts',(12.2677307440847,5.13396194677585,0.981337851592837));
#72369=CARTESIAN_POINT('Ctrl Pts',(12.2279754199457,5.15064551042452,-0.889629178846445));
#72370=CARTESIAN_POINT('Ctrl Pts',(12.1882200958066,4.3767427459812,-2.33823301368551));
#72371=CARTESIAN_POINT('Ctrl Pts',(12.1484647716676,3.60283998153789,-3.78683684852453));
#72372=CARTESIAN_POINT('Ctrl Pts',(12.1087094475285,2.03835088900258,-4.81307748776327));
#72373=CARTESIAN_POINT('Ctrl Pts',(12.0689541233895,0.40136231901543,-4.94591942713005));
#72374=CARTESIAN_POINT('Ctrl Pts',(12.0291987992504,-1.23562625097182,-5.07876136649683));
#72375=CARTESIAN_POINT('Ctrl Pts',(11.9894434751114,-2.94511429841096,-4.31820460599157));
#72376=CARTESIAN_POINT('Ctrl Pts',(11.9496881509723,-3.94246171679709,-3.01333806639369));
#72377=CARTESIAN_POINT('Ctrl Pts',(11.9237216713629,-4.59388644955471,-2.16105497910461));
#72378=CARTESIAN_POINT('Ctrl Pts',(11.8977551917536,-4.94150170668492,-1.07656148024989));
#72379=CARTESIAN_POINT('Ctrl Pts',(11.8717887121442,-4.94883061351211,0.0036397403582919));
#72380=CARTESIAN_POINT('Ctrl Pts',(11.7664112878559,-4.94768798497716,0.00300517406437754));
#72381=CARTESIAN_POINT('Ctrl Pts',(11.7910392542505,-4.94203083430539,-1.02210807507116));
#72382=CARTESIAN_POINT('Ctrl Pts',(11.815667220645,-4.63188980484689,-2.05035861141485));
#72383=CARTESIAN_POINT('Ctrl Pts',(11.8402951870396,-4.04158227195343,-2.87903179951418));
#72384=CARTESIAN_POINT('Ctrl Pts',(11.8800505111787,-3.08868722020987,-4.2167050231336));
#72385=CARTESIAN_POINT('Ctrl Pts',(11.9198058353177,-1.40574704735437,-5.03432867771487));
#72386=CARTESIAN_POINT('Ctrl Pts',(11.9595611594568,0.234783383036354,-4.95662063573885));
#72387=CARTESIAN_POINT('Ctrl Pts',(11.9993164835959,1.87531381342699,-4.87891259376283));
#72388=CARTESIAN_POINT('Ctrl Pts',(12.0390718077349,3.4734345013528,-3.90587285522962));
#72389=CARTESIAN_POINT('Ctrl Pts',(12.078827131874,4.29562198716748,-2.48411817491548));
#72390=CARTESIAN_POINT('Ctrl Pts',(12.118582456013,5.11780947298219,-1.0623634946013));
#72391=CARTESIAN_POINT('Ctrl Pts',(12.1583377801521,5.16406375668566,0.808106127493931));
#72392=CARTESIAN_POINT('Ctrl Pts',(12.1980931042911,4.41315452540982,2.26876144590765));
#72393=CARTESIAN_POINT('Ctrl Pts',(12.2378484284302,3.66224529413399,3.72941676432133));
#72394=CARTESIAN_POINT('Ctrl Pts',(12.2776037525692,2.11417254787894,4.78025777905362));
#72395=CARTESIAN_POINT('Ctrl Pts',(12.3173590767083,0.47948817749778,4.93895762800431));
#72396=CARTESIAN_POINT('Ctrl Pts',(12.3571144008473,-1.15519619288338,5.09765747695501));
#72397=CARTESIAN_POINT('Ctrl Pts',(12.3968697249864,-2.8764921873906,4.36421616012411));
#72398=CARTESIAN_POINT('Ctrl Pts',(12.4366250491254,-3.89433995478385,3.07527684609959));
#72399=CARTESIAN_POINT('Ctrl Pts',(12.4632204620356,-4.57525709581401,2.21300559023716));
#72400=CARTESIAN_POINT('Ctrl Pts',(12.4898158749457,-4.94135952703255,1.10213190132163));
#72401=CARTESIAN_POINT('Ctrl Pts',(12.5164112878559,-4.9494435771879,-0.00388817816282298));
#72402=CARTESIAN_POINT('Origin',(10.45,0.,0.));
#72403=CARTESIAN_POINT('',(13.3717887121442,-4.96094723257582,-0.00223694760002224));
#72404=CARTESIAN_POINT('',(13.2664112878559,-4.96176967234081,-0.00129340989018459));
#72405=CARTESIAN_POINT('',(10.45,-4.954,-6.06690024297599E-16));
#72406=CARTESIAN_POINT('Ctrl Pts',(13.3717887121442,-4.96094723257582,-0.00223694760002224));
#72407=CARTESIAN_POINT('Ctrl Pts',(13.3350637572832,-4.95241483308039,1.51594650197974));
#72408=CARTESIAN_POINT('Ctrl Pts',(13.2983388024221,-4.2041562175098,3.04140006639481));
#72409=CARTESIAN_POINT('Ctrl Pts',(13.2616138475611,-2.99433500310446,3.95691402231224));
#72410=CARTESIAN_POINT('Ctrl Pts',(13.2218585234221,-1.68468507403037,4.94797185230984));
#72411=CARTESIAN_POINT('Ctrl Pts',(13.182103199283,0.165842044445711,5.22427848283428));
#72412=CARTESIAN_POINT('Ctrl Pts',(13.1423478751439,1.70787054211769,4.65901157995497));
#72413=CARTESIAN_POINT('Ctrl Pts',(13.1025925510049,3.24989903978976,4.09374467707563));
#72414=CARTESIAN_POINT('Ctrl Pts',(13.0628372268658,4.48342891665779,2.68690424079239));
#72415=CARTESIAN_POINT('Ctrl Pts',(13.0230819027268,4.84228071600508,1.08421776327136));
#72416=CARTESIAN_POINT('Ctrl Pts',(12.9833265785877,5.20113251535238,-0.518468714249673));
#72417=CARTESIAN_POINT('Ctrl Pts',(12.9435712544487,4.68530623717908,-2.31700123300836));
#72418=CARTESIAN_POINT('Ctrl Pts',(12.9038159303096,3.53156164500038,-3.48586905066012));
#72419=CARTESIAN_POINT('Ctrl Pts',(12.8640606061706,2.37781705282174,-4.65473686831181));
#72420=CARTESIAN_POINT('Ctrl Pts',(12.8243052820315,0.586154146637735,-5.19393998485644));
#72421=CARTESIAN_POINT('Ctrl Pts',(12.7845499578925,-1.02106942347329,-4.8559888718196));
#72422=CARTESIAN_POINT('Ctrl Pts',(12.7447946337534,-2.62829299358441,-4.51803775878274));
#72423=CARTESIAN_POINT('Ctrl Pts',(12.7050393096143,-4.05107722762262,-3.30293241616428));
#72424=CARTESIAN_POINT('Ctrl Pts',(12.6652839854753,-4.63637656928722,-1.76839560012806));
#72425=CARTESIAN_POINT('Ctrl Pts',(12.6507855610316,-4.84983020011129,-1.20876323477365));
#72426=CARTESIAN_POINT('Ctrl Pts',(12.6362871365879,-4.95189849906051,-0.6066465440279));
#72427=CARTESIAN_POINT('Ctrl Pts',(12.6217887121442,-4.94819583789813,-0.00332016549414282));
#72428=CARTESIAN_POINT('Ctrl Pts',(12.5164112878559,-4.9494435771879,-0.00388817816282298));
#72429=CARTESIAN_POINT('Ctrl Pts',(12.5295711990848,-4.95344371746674,-0.551167745228975));
#72430=CARTESIAN_POINT('Ctrl Pts',(12.5427311103137,-4.8697846040195,-1.09725892699675));
#72431=CARTESIAN_POINT('Ctrl Pts',(12.5558910215426,-4.69323192829556,-1.61145444577539));
#72432=CARTESIAN_POINT('Ctrl Pts',(12.5956463456817,-4.15987659413477,-3.16480911240745));
#72433=CARTESIAN_POINT('Ctrl Pts',(12.6354016698207,-2.77876638553401,-4.42708113445346));
#72434=CARTESIAN_POINT('Ctrl Pts',(12.6751569939598,-1.18381884452863,-4.81889866120061));
#72435=CARTESIAN_POINT('Ctrl Pts',(12.7149123180988,0.41112869647675,-5.21071618794776));
#72436=CARTESIAN_POINT('Ctrl Pts',(12.7546676422379,2.2199135698868,-4.73207921939605));
#72437=CARTESIAN_POINT('Ctrl Pts',(12.794422966377,3.41231929197536,-3.60267795024686));
#72438=CARTESIAN_POINT('Ctrl Pts',(12.834178290516,4.60472501406402,-2.47327668109757));
#72439=CARTESIAN_POINT('Ctrl Pts',(12.8739336146551,5.1807515848311,-0.693111111350794));
#72440=CARTESIAN_POINT('Ctrl Pts',(12.9136889387941,4.87600783142616,0.920738286079608));
#72441=CARTESIAN_POINT('Ctrl Pts',(12.9534442629332,4.57126407802125,2.53458768350987));
#72442=CARTESIAN_POINT('Ctrl Pts',(12.9931995870722,3.3857500004444,3.98212090862372));
#72443=CARTESIAN_POINT('Ctrl Pts',(13.0329549112113,1.86360622225035,4.59893283403573));
#72444=CARTESIAN_POINT('Ctrl Pts',(13.0727102353503,0.341462444056204,5.21574475944778));
#72445=CARTESIAN_POINT('Ctrl Pts',(13.1124655594894,-1.51731103475523,5.00183538515791));
#72446=CARTESIAN_POINT('Ctrl Pts',(13.1522208836284,-2.85955339649474,4.05538724860864));
#72447=CARTESIAN_POINT('Ctrl Pts',(13.1902843517043,-4.14467433041966,3.14921683719545));
#72448=CARTESIAN_POINT('Ctrl Pts',(13.2283478197801,-4.9562924078719,1.57152987054922));
#72449=CARTESIAN_POINT('Ctrl Pts',(13.2664112878559,-4.96176967234081,-0.00129340989018459));
#72450=CARTESIAN_POINT('Origin',(10.45,0.,0.));
#72451=CARTESIAN_POINT('',(14.1217887121442,-4.95503454872885,0.00449354721262798));
#72452=CARTESIAN_POINT('',(14.0164112878559,-4.95334288452853,0.00456658721771082));
#72453=CARTESIAN_POINT('',(10.45,-4.954,-6.06690024297599E-16));
#72454=CARTESIAN_POINT('Ctrl Pts',(14.1217887121442,-4.95503454872885,0.00449354721262798));
#72455=CARTESIAN_POINT('Ctrl Pts',(14.1133510262565,-4.95828270233056,0.35438528685295));
#72456=CARTESIAN_POINT('Ctrl Pts',(14.1049133403689,-4.92438729661826,0.703652274904061));
#72457=CARTESIAN_POINT('Ctrl Pts',(14.0964756544813,-4.85102004306605,1.04442100350354));
#72458=CARTESIAN_POINT('Ctrl Pts',(14.0567203303422,-4.50534007998143,2.65000000257061));
#72459=CARTESIAN_POINT('Ctrl Pts',(14.0169650062031,-3.28340342420688,4.06692158810787));
#72460=CARTESIAN_POINT('Ctrl Pts',(13.9772096820641,-1.74606834507353,4.6448311083526));
#72461=CARTESIAN_POINT('Ctrl Pts',(13.937454357925,-0.208733265940278,5.2227406285973));
#72462=CARTESIAN_POINT('Ctrl Pts',(13.897699033786,1.64400023655164,4.96163808354953));
#72463=CARTESIAN_POINT('Ctrl Pts',(13.8579437096469,2.96174364117349,3.98136726449046));
#72464=CARTESIAN_POINT('Ctrl Pts',(13.8181883855079,4.27948704579556,3.00109644543122));
#72465=CARTESIAN_POINT('Ctrl Pts',(13.7784330613688,5.06224035254725,1.30165735236046));
#72466=CARTESIAN_POINT('Ctrl Pts',(13.7386777372298,4.95072661948288,-0.336922290641983));
#72467=CARTESIAN_POINT('Ctrl Pts',(13.6989224130907,4.83921288641853,-1.97550193364414));
#72468=CARTESIAN_POINT('Ctrl Pts',(13.6591670889517,3.83343211353822,-3.55322212657819));
#72469=CARTESIAN_POINT('Ctrl Pts',(13.6194117648126,2.39502890487168,-4.34592305909999));
#72470=CARTESIAN_POINT('Ctrl Pts',(13.5796564406735,0.956625696205059,-5.13862399162183));
#72471=CARTESIAN_POINT('Ctrl Pts',(13.5399011165345,-0.914399948247869,
-5.14630566373156));
#72472=CARTESIAN_POINT('Ctrl Pts',(13.5001457923954,-2.35926357361136,-4.36544225491741));
#72473=CARTESIAN_POINT('Ctrl Pts',(13.4603904682564,-3.80412719897494,-3.58457884610321));
#72474=CARTESIAN_POINT('Ctrl Pts',(13.4206351441173,-4.82282880524895,-2.01517035636507));
#72475=CARTESIAN_POINT('Ctrl Pts',(13.3808798199783,-4.94779323854984,-0.377561596760541));
#72476=CARTESIAN_POINT('Ctrl Pts',(13.3778494507002,-4.95731871438791,-0.252734057757678));
#72477=CARTESIAN_POINT('Ctrl Pts',(13.3748190814222,-4.96165128575701,-0.127510252943251));
#72478=CARTESIAN_POINT('Ctrl Pts',(13.3717887121442,-4.96094723257582,-0.00223694760002224));
#72479=CARTESIAN_POINT('Ctrl Pts',(13.2664112878559,-4.96176967234081,-0.00129340989018459));
#72480=CARTESIAN_POINT('Ctrl Pts',(13.2681031439191,-4.96201312737973,-0.0712027150045571));
#72481=CARTESIAN_POINT('Ctrl Pts',(13.2697949999824,-4.96066392993926,-0.141102411174969));
#72482=CARTESIAN_POINT('Ctrl Pts',(13.2714868560456,-4.9576928696551,-0.210933102554134));
#72483=CARTESIAN_POINT('Ctrl Pts',(13.3112421801847,-4.88787873640841,-1.85181841835902));
#72484=CARTESIAN_POINT('Ctrl Pts',(13.3509975043237,-3.92253922524754,-3.45460215116033));
#72485=CARTESIAN_POINT('Ctrl Pts',(13.3907528284628,-2.50475675373321,-4.28362054437715));
#72486=CARTESIAN_POINT('Ctrl Pts',(13.4305081526018,-1.08697428221864,-5.11263893759411));
#72487=CARTESIAN_POINT('Ctrl Pts',(13.4702634767409,0.783251149649558,-5.16789199122628));
#72488=CARTESIAN_POINT('Ctrl Pts',(13.5100188008799,2.24750237759368,-4.4240190354804));
#72489=CARTESIAN_POINT('Ctrl Pts',(13.549774125019,3.71175360553764,-3.68014607973459));
#72490=CARTESIAN_POINT('Ctrl Pts',(13.589529449158,4.77003062955761,-2.13714711461092));
#72491=CARTESIAN_POINT('Ctrl Pts',(13.6292847732971,4.93659352413465,-0.503245209668175));
#72492=CARTESIAN_POINT('Ctrl Pts',(13.6690400974362,5.10315641871169,1.13065669527456));
#72493=CARTESIAN_POINT('Ctrl Pts',(13.7087954215752,4.3780051838458,2.85546154003637));
#72494=CARTESIAN_POINT('Ctrl Pts',(13.7485507457143,3.09397791279514,3.87949894170858));
#72495=CARTESIAN_POINT('Ctrl Pts',(13.7883060698533,1.8099506417444,4.90353634338085));
#72496=CARTESIAN_POINT('Ctrl Pts',(13.8280613939924,-0.032952665491161,
5.22680630196345));
#72497=CARTESIAN_POINT('Ctrl Pts',(13.8678167181314,-1.58885546158286,4.70093072548197));
#72498=CARTESIAN_POINT('Ctrl Pts',(13.9075720422705,-3.14475825767447,4.17505514900052));
#72499=CARTESIAN_POINT('Ctrl Pts',(13.9473273664095,-4.41366054262224,2.8000340374551));
#72500=CARTESIAN_POINT('Ctrl Pts',(13.9870826905486,-4.81314723285944,1.20699009043144));
#72501=CARTESIAN_POINT('Ctrl Pts',(13.996858889651,-4.91138467670136,0.815245962008683));
#72502=CARTESIAN_POINT('Ctrl Pts',(14.0066350887534,-4.95704740833786,0.410317704040501));
#72503=CARTESIAN_POINT('Ctrl Pts',(14.0164112878559,-4.95334288452853,0.00456658721771082));
#72504=CARTESIAN_POINT('Origin',(10.45,0.,0.));
#72505=CARTESIAN_POINT('',(14.8717887121442,-4.94581096318579,-1.93332609692235E-5));
#72506=CARTESIAN_POINT('',(14.7664112878559,-4.9459710090011,-0.000934506679922751));
#72507=CARTESIAN_POINT('',(10.45,-4.954,-6.06690024297599E-16));
#72508=CARTESIAN_POINT('Ctrl Pts',(14.8717887121442,-4.94581103525318,-1.93330908274114E-5));
#72509=CARTESIAN_POINT('Ctrl Pts',(14.8518829710909,-4.94578225734086,0.829322250681016));
#72510=CARTESIAN_POINT('Ctrl Pts',(14.8319772300376,-4.74850012339904,1.65867670117964));
#72511=CARTESIAN_POINT('Ctrl Pts',(14.8120714889842,-4.35404071127217,2.38023952058872));
#72512=CARTESIAN_POINT('Ctrl Pts',(14.7723161648452,-3.56623473375009,3.82132949033526));
#72513=CARTESIAN_POINT('Ctrl Pts',(14.7325608407061,-1.99194317595282,4.83246848243075));
#72514=CARTESIAN_POINT('Ctrl Pts',(14.6928055165671,-0.353752134595302,
4.94955251695112));
#72515=CARTESIAN_POINT('Ctrl Pts',(14.653050192428,1.28443890676203,5.06663655147147));
#72516=CARTESIAN_POINT('Ctrl Pts',(14.613294868289,2.9865294316797,4.28966562841695));
#72517=CARTESIAN_POINT('Ctrl Pts',(14.5735395441499,3.97127473198152,2.97526262604042));
#72518=CARTESIAN_POINT('Ctrl Pts',(14.5337842200109,4.95602003228346,1.66085962366375));
#72519=CARTESIAN_POINT('Ctrl Pts',(14.4940288958718,5.22342010796947,-0.19097545803513));
#72520=CARTESIAN_POINT('Ctrl Pts',(14.4542735717327,4.65074065611181,-1.73026646513667));
#72521=CARTESIAN_POINT('Ctrl Pts',(14.4145182475937,4.07806120425415,-3.2695574722382));
#72522=CARTESIAN_POINT('Ctrl Pts',(14.3747629234546,2.66530222485308,-4.49630440474226));
#72523=CARTESIAN_POINT('Ctrl Pts',(14.3350075993156,1.06090776975382,-4.84744111824618));
#72524=CARTESIAN_POINT('Ctrl Pts',(14.2952522751765,-0.543486685345351,
-5.19857783175009));
#72525=CARTESIAN_POINT('Ctrl Pts',(14.2554969510375,-2.33951661614259,-4.67410432625374));
#72526=CARTESIAN_POINT('Ctrl Pts',(14.2157416268984,-3.50281994634389,-3.51474936720718));
#72527=CARTESIAN_POINT('Ctrl Pts',(14.184423988647,-4.41922331270755,-2.601456368126));
#72528=CARTESIAN_POINT('Ctrl Pts',(14.1531063503956,-4.94297857735968,-1.29417804060499));
#72529=CARTESIAN_POINT('Ctrl Pts',(14.1217887121442,-4.95503454872885,0.00449354721262798));
#72530=CARTESIAN_POINT('Ctrl Pts',(14.0164112878559,-4.95334288452853,0.00456658721771082));
#72531=CARTESIAN_POINT('Ctrl Pts',(14.0463904128925,-4.9419828067194,-1.23968624944593));
#72532=CARTESIAN_POINT('Ctrl Pts',(14.0763695379291,-4.46638886767634,-2.4916769872725));
#72533=CARTESIAN_POINT('Ctrl Pts',(14.1063486629658,-3.61905378866574,-3.39494639697394));
#72534=CARTESIAN_POINT('Ctrl Pts',(14.1461039871048,-2.49540255870816,-4.59277215485382));
#72535=CARTESIAN_POINT('Ctrl Pts',(14.1858593112439,-0.718029003266378,
-5.17735688811155));
#72536=CARTESIAN_POINT('Ctrl Pts',(14.2256146353829,0.897267914964357,-4.88038130194328));
#72537=CARTESIAN_POINT('Ctrl Pts',(14.265369959522,2.512564833195,-4.58340571577504));
#72538=CARTESIAN_POINT('Ctrl Pts',(14.305125283661,3.96578511421461,-3.40486981018091));
#72539=CARTESIAN_POINT('Ctrl Pts',(14.3448806078001,4.58991332156997,-1.88571128862735));
#72540=CARTESIAN_POINT('Ctrl Pts',(14.3846359319391,5.21404152892534,-0.366552767073803));
#72541=CARTESIAN_POINT('Ctrl Pts',(14.4243912560782,5.00907766261646,1.49322837043917));
#72542=CARTESIAN_POINT('Ctrl Pts',(14.4641465802172,4.06909834993017,2.84000879966555));
#72543=CARTESIAN_POINT('Ctrl Pts',(14.5039019043563,3.12911903724383,4.186789228892));
#72544=CARTESIAN_POINT('Ctrl Pts',(14.5436572284954,1.45412427817999,5.02056894983181));
#72545=CARTESIAN_POINT('Ctrl Pts',(14.5834125526344,-0.18707793932848,4.95865034139318));
#72546=CARTESIAN_POINT('Ctrl Pts',(14.6231678767735,-1.82828015683685,4.89673173295456));
#72547=CARTESIAN_POINT('Ctrl Pts',(14.6629232009125,-3.43568983278986,3.93911479513759));
#72548=CARTESIAN_POINT('Ctrl Pts',(14.7026785250516,-4.27151994303955,2.52533735168145));
#72549=CARTESIAN_POINT('Ctrl Pts',(14.7239227793197,-4.7181667198327,1.76984992609218));
#72550=CARTESIAN_POINT('Ctrl Pts',(14.7451670335878,-4.94448376706638,0.884102802980237));
#72551=CARTESIAN_POINT('Ctrl Pts',(14.7664112878559,-4.9459710090011,-0.000934506679922751));
#72552=CARTESIAN_POINT('Origin',(10.45,0.,0.));
#72553=CARTESIAN_POINT('',(15.6217887121442,-4.95510573438616,-0.00448604574660338));
#72554=CARTESIAN_POINT('',(15.5164112878559,-4.95678235276575,-0.00420182901399404));
#72555=CARTESIAN_POINT('',(10.45,-4.954,-6.06690024297599E-16));
#72556=CARTESIAN_POINT('Ctrl Pts',(15.6217887121442,-4.95510573438616,-0.00448604574660338));
#72557=CARTESIAN_POINT('Ctrl Pts',(15.5904149159252,-4.94303076991488,1.29646632009306));
#72558=CARTESIAN_POINT('Ctrl Pts',(15.5590411197062,-4.41719278747976,2.60605571081289));
#72559=CARTESIAN_POINT('Ctrl Pts',(15.5276673234872,-3.49785572892943,3.51968975768936));
#72560=CARTESIAN_POINT('Ctrl Pts',(15.4879119993482,-2.33291724011508,4.67740167194192));
#72561=CARTESIAN_POINT('Ctrl Pts',(15.4481566752091,-0.536148854634113,
5.199339732657));
#72562=CARTESIAN_POINT('Ctrl Pts',(15.4084013510701,1.06774840695936,4.84593892142932));
#72563=CARTESIAN_POINT('Ctrl Pts',(15.368646026931,2.67164566855283,4.49253811020164));
#72564=CARTESIAN_POINT('Ctrl Pts',(15.328890702792,4.08267180625871,3.26379842703124));
#72565=CARTESIAN_POINT('Ctrl Pts',(15.2891353786529,4.65317812745874,1.72370067149939));
#72566=CARTESIAN_POINT('Ctrl Pts',(15.2493800545139,5.22368444865877,0.183602915967541));
#72567=CARTESIAN_POINT('Ctrl Pts',(15.2096247303748,4.95367095335283,-1.66785291192591));
#72568=CARTESIAN_POINT('Ctrl Pts',(15.1698694062357,3.96707148128438,-2.98086473245064));
#72569=CARTESIAN_POINT('Ctrl Pts',(15.1301140820967,2.98047200921587,-4.29387655297545));
#72570=CARTESIAN_POINT('Ctrl Pts',(15.0903587579576,1.27728656038484,-5.06844436613168));
#72571=CARTESIAN_POINT('Ctrl Pts',(15.0506034338186,-0.360737596504414,
-4.94904830015389));
#72572=CARTESIAN_POINT('Ctrl Pts',(15.0108481096795,-1.99876175339348,-4.82965223417611));
#72573=CARTESIAN_POINT('Ctrl Pts',(14.9710927855405,-3.5716246183407,-3.81629228906456));
#72574=CARTESIAN_POINT('Ctrl Pts',(14.9313374614014,-4.3573958521909,-2.37409184281009));
#72575=CARTESIAN_POINT('Ctrl Pts',(14.9114878783157,-4.74972648287934,-1.6540102385425));
#72576=CARTESIAN_POINT('Ctrl Pts',(14.8916382952299,-4.94583973197741,-0.827021182931719));
#72577=CARTESIAN_POINT('Ctrl Pts',(14.8717887121442,-4.94581103525318,-1.93330908274114E-5));
#72578=CARTESIAN_POINT('Ctrl Pts',(14.7664112878559,-4.9459710090011,-0.000934506679922751));
#72579=CARTESIAN_POINT('Ctrl Pts',(14.7849223577268,-4.94726690948417,-0.772107138619626));
#72580=CARTESIAN_POINT('Ctrl Pts',(14.8034334275978,-4.77786264413242,-1.54274085058044));
#72581=CARTESIAN_POINT('Ctrl Pts',(14.8219444974687,-4.4347811370167,-2.22619128341277));
#72582=CARTESIAN_POINT('Ctrl Pts',(14.8616998216078,-3.69796167619771,-3.69400452595569));
#72583=CARTESIAN_POINT('Ctrl Pts',(14.9014551457469,-2.16007221001321,-4.75969306194599));
#72584=CARTESIAN_POINT('Ctrl Pts',(14.9412104698859,-0.526990592565549,
-4.9341151465009));
#72585=CARTESIAN_POINT('Ctrl Pts',(14.980965794025,1.10609102488183,-5.10853723105577));
#72586=CARTESIAN_POINT('Ctrl Pts',(15.020721118164,2.83436479359242,-4.3916928641756));
#72587=CARTESIAN_POINT('Ctrl Pts',(15.0604764423031,3.86456812481518,-3.11260735915159));
#72588=CARTESIAN_POINT('Ctrl Pts',(15.1002317664421,4.89477145603799,-1.8335218541275));
#72589=CARTESIAN_POINT('Ctrl Pts',(15.1399870905812,5.22690434977295,0.00780478904030796));
#72590=CARTESIAN_POINT('Ctrl Pts',(15.1797424147202,4.70852070409838,1.56621969808168));
#72591=CARTESIAN_POINT('Ctrl Pts',(15.2194977388593,4.19013705842374,3.12463460712323));
#72592=CARTESIAN_POINT('Ctrl Pts',(15.2592530629984,2.8212368733392,4.40013778203812));
#72593=CARTESIAN_POINT('Ctrl Pts',(15.2990083871374,1.23013339656155,4.80728438832633));
#72594=CARTESIAN_POINT('Ctrl Pts',(15.3387637112765,-0.360970080215911,
5.2144309946145));
#72595=CARTESIAN_POINT('Ctrl Pts',(15.3785190354155,-2.17427684868653,4.75322103227624));
#72596=CARTESIAN_POINT('Ctrl Pts',(15.4182743595546,-3.37749491472365,3.63534585212989));
#72597=CARTESIAN_POINT('Ctrl Pts',(15.4509866689883,-4.36755203398721,2.71551235578195));
#72598=CARTESIAN_POINT('Ctrl Pts',(15.4836989784221,-4.9445380670697,1.35107233960266));
#72599=CARTESIAN_POINT('Ctrl Pts',(15.5164112878559,-4.95678235276575,-0.00420182901399404));
#72600=CARTESIAN_POINT('Origin',(10.45,0.,0.));
#72601=CARTESIAN_POINT('',(16.3717887121442,-4.96090463397887,0.00227414672534738));
#72602=CARTESIAN_POINT('',(16.2664112878559,-4.95972825749042,0.00308940621307957));
#72603=CARTESIAN_POINT('',(10.45,-4.954,-6.06690024297599E-16));
#72604=CARTESIAN_POINT('Ctrl Pts',(16.3717887121442,-4.96090463397887,0.00227414672534738));
#72605=CARTESIAN_POINT('Ctrl Pts',(16.3687021848986,-4.96163172276262,0.129871883079575));
#72606=CARTESIAN_POINT('Ctrl Pts',(16.365615657653,-4.95713685536309,0.257417563448558));
#72607=CARTESIAN_POINT('Ctrl Pts',(16.3625291304074,-4.94725541875388,0.384544551902995));
#72608=CARTESIAN_POINT('Ctrl Pts',(16.3227738062683,-4.81997978367921,2.02197530519914));
#72609=CARTESIAN_POINT('Ctrl Pts',(16.2830184821293,-3.7990641238995,3.5899444330534));
#72610=CARTESIAN_POINT('Ctrl Pts',(16.2432631579902,-2.35309982455023,4.36876777896119));
#72611=CARTESIAN_POINT('Ctrl Pts',(16.2035078338512,-0.907135525201033,
5.14759112486893));
#72612=CARTESIAN_POINT('Ctrl Pts',(16.1637525097121,0.963877413717682,5.13726868883029));
#72613=CARTESIAN_POINT('Ctrl Pts',(16.1239971855731,2.4011603690595,4.34253837897213));
#72614=CARTESIAN_POINT('Ctrl Pts',(16.084241861434,3.83844332440131,3.54780806911397));
#72615=CARTESIAN_POINT('Ctrl Pts',(16.044486537295,4.84199629616623,1.96866988543629));
#72616=CARTESIAN_POINT('Ctrl Pts',(16.0047312131559,4.95119722160954,0.329934483668917));
#72617=CARTESIAN_POINT('Ctrl Pts',(15.9649758890168,5.06039814705285,-1.30880091809855));
#72618=CARTESIAN_POINT('Ctrl Pts',(15.9252205648778,4.27524702617445,-3.00713353795571));
#72619=CARTESIAN_POINT('Ctrl Pts',(15.8854652407387,2.95612137669453,-3.98554351337901));
#72620=CARTESIAN_POINT('Ctrl Pts',(15.8457099165997,1.63699572721468,-4.96395348880225));
#72621=CARTESIAN_POINT('Ctrl Pts',(15.8059545924606,-0.216104450866626,
-5.22244081979172));
#72622=CARTESIAN_POINT('Ctrl Pts',(15.7661992683216,-1.75262233542247,-4.64236207551351));
#72623=CARTESIAN_POINT('Ctrl Pts',(15.7264439441825,-3.28914021997823,-4.06228333123534));
#72624=CARTESIAN_POINT('Ctrl Pts',(15.6866886200435,-4.50907581100856,-2.64363851168958));
#72625=CARTESIAN_POINT('Ctrl Pts',(15.6469332959044,-4.85248931045004,-1.03757321802173));
#72626=CARTESIAN_POINT('Ctrl Pts',(15.6385517679843,-4.92489042642715,-0.698969989602403));
#72627=CARTESIAN_POINT('Ctrl Pts',(15.6301702400643,-4.95833156817253,-0.352036227460802));
#72628=CARTESIAN_POINT('Ctrl Pts',(15.6217887121442,-4.95510573438616,-0.00448604574660338));
#72629=CARTESIAN_POINT('Ctrl Pts',(15.5164112878559,-4.95678235276575,-0.00420182901399404));
#72630=CARTESIAN_POINT('Ctrl Pts',(15.5234543025612,-4.95941856786966,-0.295994614802925));
#72631=CARTESIAN_POINT('Ctrl Pts',(15.5304973172665,-4.93587628816053,-0.587362519495321));
#72632=CARTESIAN_POINT('Ctrl Pts',(15.5375403319717,-4.8846417999139,-0.873776773618994));
#72633=CARTESIAN_POINT('Ctrl Pts',(15.5772956561108,-4.59544125546334,-2.49048382126709));
#72634=CARTESIAN_POINT('Ctrl Pts',(15.6170509802498,-3.42391080295839,-3.94935751860888));
#72635=CARTESIAN_POINT('Ctrl Pts',(15.6568063043889,-1.90777270398753,-4.58078756039857));
#72636=CARTESIAN_POINT('Ctrl Pts',(15.6965616285279,-0.39163460501667,-5.21221760218826));
#72637=CARTESIAN_POINT('Ctrl Pts',(15.736316952667,1.46911114042006,-5.01620398842604));
#72638=CARTESIAN_POINT('Ctrl Pts',(15.7760722768061,2.82039846145153,-4.08271525852881));
#72639=CARTESIAN_POINT('Ctrl Pts',(15.8158276009451,4.17168578248299,-3.14922652863158));
#72640=CARTESIAN_POINT('Ctrl Pts',(15.8555829250842,5.0135146791091,-1.47826268259919));
#72641=CARTESIAN_POINT('Ctrl Pts',(15.8953382492232,4.95949302878925,0.163218445565945));
#72642=CARTESIAN_POINT('Ctrl Pts',(15.9350935733623,4.9054713784694,1.80469957373108));
#72643=CARTESIAN_POINT('Ctrl Pts',(15.9748488975013,3.95559918120381,3.41669798402893));
#72644=CARTESIAN_POINT('Ctrl Pts',(16.0146042216404,2.545859492355,4.25932046326266));
#72645=CARTESIAN_POINT('Ctrl Pts',(16.0543595457795,1.13611980350619,5.10194294249639));
#72646=CARTESIAN_POINT('Ctrl Pts',(16.0941148699185,-0.733487376925646,
5.17518949066586));
#72647=CARTESIAN_POINT('Ctrl Pts',(16.1338701940576,-2.2048286566811,4.44544058089409));
#72648=CARTESIAN_POINT('Ctrl Pts',(16.1736255181966,-3.67616993643647,3.71569167112235));
#72649=CARTESIAN_POINT('Ctrl Pts',(16.2133808423357,-4.74924531551546,2.18294730340928));
#72650=CARTESIAN_POINT('Ctrl Pts',(16.2531361664747,-4.93152255247316,0.550723776525695));
#72651=CARTESIAN_POINT('Ctrl Pts',(16.2575612069351,-4.95181126011202,0.36904609427131));
#72652=CARTESIAN_POINT('Ctrl Pts',(16.2619862473955,-4.96106367538195,0.18613594302839));
#72653=CARTESIAN_POINT('Ctrl Pts',(16.2664112878559,-4.95972825749042,0.00308940621307957));
#72654=CARTESIAN_POINT('Origin',(10.45,0.,0.));
#72655=CARTESIAN_POINT('',(17.1217887121442,-4.94814833252334,0.00329320459974858));
#72656=CARTESIAN_POINT('',(17.0164112878559,-4.94714433343639,0.00258591176320991));
#72657=CARTESIAN_POINT('',(10.45,-4.954,-6.06690024297599E-16));
#72658=CARTESIAN_POINT('Ctrl Pts',(17.1217887121442,-4.94814833252334,0.00329320459974858));
#72659=CARTESIAN_POINT('Ctrl Pts',(17.1072341297329,-4.95183295583228,0.608971087556108));
#72660=CARTESIAN_POINT('Ctrl Pts',(17.0926795473216,-4.84894916378528,1.2134405946199));
#72661=CARTESIAN_POINT('Ctrl Pts',(17.0781249649104,-4.6338760321099,1.7749376354749));
#72662=CARTESIAN_POINT('Ctrl Pts',(17.0383696407713,-4.04641142324979,3.3086468297032));
#72663=CARTESIAN_POINT('Ctrl Pts',(16.9986143166323,-2.62191360277959,4.52174283982081));
#72664=CARTESIAN_POINT('Ctrl Pts',(16.9588589924932,-1.01421464822929,4.85742517575979));
#72665=CARTESIAN_POINT('Ctrl Pts',(16.9191036683542,0.593484306321018,5.19310751169876));
#72666=CARTESIAN_POINT('Ctrl Pts',(16.8793483442151,2.38438439495152,4.65137617345912));
#72667=CARTESIAN_POINT('Ctrl Pts',(16.839593020076,3.53647809418883,3.4808811212264));
#72668=CARTESIAN_POINT('Ctrl Pts',(16.799837695937,4.68857179342601,2.31038606899382));
#72669=CARTESIAN_POINT('Ctrl Pts',(16.7600823717979,5.20185910327026,0.511127302768274));
#72670=CARTESIAN_POINT('Ctrl Pts',(16.7203270476589,4.84074562452872,-1.09105109385122));
#72671=CARTESIAN_POINT('Ctrl Pts',(16.6805717235198,4.47963214578711,-2.69322949047098));
#72672=CARTESIAN_POINT('Ctrl Pts',(16.6408163993808,3.24411787845962,-4.09832751748447));
#72673=CARTESIAN_POINT('Ctrl Pts',(16.6010610752417,1.70129309717905,-4.66141743338641));
#72674=CARTESIAN_POINT('Ctrl Pts',(16.5613057511027,0.158468315898662,-5.22450734928829));
#72675=CARTESIAN_POINT('Ctrl Pts',(16.5215504269636,-1.69166697933467,-4.9455891540786));
#72676=CARTESIAN_POINT('Ctrl Pts',(16.4817951028245,-2.99991682176645,-3.9526838671048));
#72677=CARTESIAN_POINT('Ctrl Pts',(16.4451263059311,-4.206596651372,-3.03686584546993));
#72678=CARTESIAN_POINT('Ctrl Pts',(16.4084575090376,-4.95226661823711,-1.51362223329568));
#72679=CARTESIAN_POINT('Ctrl Pts',(16.3717887121442,-4.96090463397887,0.00227414672534738));
#72680=CARTESIAN_POINT('Ctrl Pts',(16.2664112878559,-4.95972825749042,0.00308940621307957));
#72681=CARTESIAN_POINT('Ctrl Pts',(16.3017415715346,-4.94906605149262,-1.45838560853021));
#72682=CARTESIAN_POINT('Ctrl Pts',(16.3370718552132,-4.26346123593968,-2.92855479447191));
#72683=CARTESIAN_POINT('Ctrl Pts',(16.3724021388919,-3.13116475392864,-3.84954784972692));
#72684=CARTESIAN_POINT('Ctrl Pts',(16.4121574630309,-1.85705062359026,-4.8858932630411));
#72685=CARTESIAN_POINT('Ctrl Pts',(16.45191278717,-0.0173432680774013,-5.22688140361534));
#72686=CARTESIAN_POINT('Ctrl Pts',(16.491668111309,1.54354767925271,-4.7160016884492));
#72687=CARTESIAN_POINT('Ctrl Pts',(16.5314234354481,3.10443862658291,-4.20512197328303));
#72688=CARTESIAN_POINT('Ctrl Pts',(16.5711787595872,4.38651316573016,-2.84237440237626));
#72689=CARTESIAN_POINT('Ctrl Pts',(16.6109340837262,4.8013102633162,-1.25324822719073));
#72690=CARTESIAN_POINT('Ctrl Pts',(16.6506894078653,5.21610736090221,0.335877947994718));
#72691=CARTESIAN_POINT('Ctrl Pts',(16.6904447320043,4.76362701692717,2.15138272745901));
#72692=CARTESIAN_POINT('Ctrl Pts',(16.7302000561434,3.65155376350569,3.35996524919672));
#72693=CARTESIAN_POINT('Ctrl Pts',(16.7699553802824,2.53948051008421,4.56854777093442));
#72694=CARTESIAN_POINT('Ctrl Pts',(16.8097107044215,0.76781434721649,5.17020803494558));
#72695=CARTESIAN_POINT('Ctrl Pts',(16.8494660285605,-0.850265405823871,
4.88878922671466));
#72696=CARTESIAN_POINT('Ctrl Pts',(16.8892213526996,-2.46834515886432,4.60737041848372));
#72697=CARTESIAN_POINT('Ctrl Pts',(16.9289766768386,-3.93283850207731,3.44287253801038));
#72698=CARTESIAN_POINT('Ctrl Pts',(16.9687320009777,-4.57155576176729,1.9297899576468));
#72699=CARTESIAN_POINT('Ctrl Pts',(16.9846250966038,-4.82689752305581,1.32490075951781));
#72700=CARTESIAN_POINT('Ctrl Pts',(17.0005181922298,-4.95026518831848,0.664301361524176));
#72701=CARTESIAN_POINT('Ctrl Pts',(17.0164112878559,-4.94714433343639,0.00258591176320991));
#72702=CARTESIAN_POINT('Origin',(10.45,0.,0.));
#72703=CARTESIAN_POINT('',(17.8717887121442,-4.94888348879255,-0.00366329764976359));
#72704=CARTESIAN_POINT('',(17.7664112878558,-4.95024685397467,-0.00414268332982216));
#72705=CARTESIAN_POINT('',(10.45,-4.954,-6.06690024297599E-16));
#72706=CARTESIAN_POINT('Ctrl Pts',(17.8717887121442,-4.94888348879255,-0.00366329764976359));
#72707=CARTESIAN_POINT('Ctrl Pts',(17.8457660745672,-4.94148610429648,1.07884500791139));
#72708=CARTESIAN_POINT('Ctrl Pts',(17.8197434369903,-4.59224319699392,2.16569540170491));
#72709=CARTESIAN_POINT('Ctrl Pts',(17.7937207994134,-3.93820475500025,3.01889946809781));
#72710=CARTESIAN_POINT('Ctrl Pts',(17.7539654752743,-2.93901663719373,4.32235704867263));
#72711=CARTESIAN_POINT('Ctrl Pts',(17.7142101511353,-1.22845684021116,5.08050027474164));
#72712=CARTESIAN_POINT('Ctrl Pts',(17.6744548269962,0.408342605748216,4.94534801678492));
#72713=CARTESIAN_POINT('Ctrl Pts',(17.6346995028571,2.0451420517074,4.81019575882822));
#72714=CARTESIAN_POINT('Ctrl Pts',(17.5949441787181,3.60818114664354,3.78174801684578));
#72715=CARTESIAN_POINT('Ctrl Pts',(17.555188854579,4.3800385761698,2.3320533360222));
#72716=CARTESIAN_POINT('Ctrl Pts',(17.51543353044,5.1518960056961,0.882358655198545));
#72717=CARTESIAN_POINT('Ctrl Pts',(17.4756782063009,5.13257176981269,-0.988582964466396));
#72718=CARTESIAN_POINT('Ctrl Pts',(17.4359228821619,4.33093552427665,-2.42202563474181));
#72719=CARTESIAN_POINT('Ctrl Pts',(17.3961675580228,3.52929927874056,-3.8554683050173));
#72720=CARTESIAN_POINT('Ctrl Pts',(17.3564122338838,1.94535102355181,-4.85141202590312));
#72721=CARTESIAN_POINT('Ctrl Pts',(17.3166569097447,0.30610919531848,-4.95272731445305));
#72722=CARTESIAN_POINT('Ctrl Pts',(17.2769015856056,-1.33313263291476,-5.05404260300297));
#72723=CARTESIAN_POINT('Ctrl Pts',(17.2371462614666,-3.02766803419248,-4.26072945921708));
#72724=CARTESIAN_POINT('Ctrl Pts',(17.1973909373275,-3.9997200362063,-2.93691169815466));
#72725=CARTESIAN_POINT('Ctrl Pts',(17.1721901955998,-4.61589993108146,-2.09774888880353));
#72726=CARTESIAN_POINT('Ctrl Pts',(17.146989453872,-4.94176853832871,-1.04541650532658));
#72727=CARTESIAN_POINT('Ctrl Pts',(17.1217887121442,-4.94814833252334,0.00329320459974858));
#72728=CARTESIAN_POINT('Ctrl Pts',(17.0164112878559,-4.94714433343639,0.00258591176320991));
#72729=CARTESIAN_POINT('Ctrl Pts',(17.0402735163689,-4.94245861618504,-0.990927601544862));
#72730=CARTESIAN_POINT('Ctrl Pts',(17.0641357448819,-4.65263422909462,-1.98695699151951));
#72731=CARTESIAN_POINT('Ctrl Pts',(17.0879979733949,-4.09623765919655,-2.8007228357983));
#72732=CARTESIAN_POINT('Ctrl Pts',(17.1277532975339,-3.16926112076872,-4.15648576862615));
#72733=CARTESIAN_POINT('Ctrl Pts',(17.167508621673,-1.50236686774581,-5.00634435402793));
#72734=CARTESIAN_POINT('Ctrl Pts',(17.207263945812,0.139355173573051,-4.96022091233652));
#72735=CARTESIAN_POINT('Ctrl Pts',(17.2470192699511,1.78107721489191,-4.9140974706451));
#72736=CARTESIAN_POINT('Ctrl Pts',(17.2867745940901,3.39762704450684,-3.97199200186048));
#72737=CARTESIAN_POINT('Ctrl Pts',(17.3265299182292,4.24702238744387,-2.56632270070089));
#72738=CARTESIAN_POINT('Ctrl Pts',(17.3662852423683,5.0964177303809,-1.1606533995413));
#72739=CARTESIAN_POINT('Ctrl Pts',(17.4060405665073,5.17865858664018,0.708579733993037));
#72740=CARTESIAN_POINT('Ctrl Pts',(17.4457958906464,4.45599712036464,2.18341499190698));
#72741=CARTESIAN_POINT('Ctrl Pts',(17.4855512147854,3.73333565408914,3.65825024982084));
#72742=CARTESIAN_POINT('Ctrl Pts',(17.5253065389245,2.20577186527881,4.73868763211418));
#72743=CARTESIAN_POINT('Ctrl Pts',(17.5650618630635,0.57444421216427,4.92881580206575));
#72744=CARTESIAN_POINT('Ctrl Pts',(17.6048171872026,-1.05688344095027,5.11894397201733));
#72745=CARTESIAN_POINT('Ctrl Pts',(17.6445725113416,-2.79197495836912,4.41876292962717));
#72746=CARTESIAN_POINT('Ctrl Pts',(17.6843278354807,-3.83443846413696,3.14964966755497));
#72747=CARTESIAN_POINT('Ctrl Pts',(17.7116889862724,-4.55190214463446,2.27619686375266));
#72748=CARTESIAN_POINT('Ctrl Pts',(17.7390501370641,-4.94128702106912,1.13325654416073));
#72749=CARTESIAN_POINT('Ctrl Pts',(17.7664112878558,-4.95024685397467,-0.00414268332982216));
#72750=CARTESIAN_POINT('Origin',(10.45,0.,0.));
#72751=CARTESIAN_POINT('',(18.6217887121442,-4.96146530959486,-0.00170939900883904));
#72752=CARTESIAN_POINT('',(18.5164112878559,-4.96205143092805,-0.000716217698562718));
#72753=CARTESIAN_POINT('',(10.45,-4.954,-6.06690024297599E-16));
#72754=CARTESIAN_POINT('Ctrl Pts',(18.6217887121442,-4.96146530959486,-0.00170939900883904));
#72755=CARTESIAN_POINT('Ctrl Pts',(18.5842980194016,-4.95455118100335,1.54769955531428));
#72756=CARTESIAN_POINT('Ctrl Pts',(18.546807326659,-4.17043746833274,3.103141179268));
#72757=CARTESIAN_POINT('Ctrl Pts',(18.5093166339163,-2.91763403509206,4.01380397230112));
#72758=CARTESIAN_POINT('Ctrl Pts',(18.4695613097773,-1.58915480658206,4.979475499551));
#72759=CARTESIAN_POINT('Ctrl Pts',(18.4298059856382,0.266346847597793,5.22011959697153));
#72760=CARTESIAN_POINT('Ctrl Pts',(18.3900506614992,1.79721184873288,4.62528272233839));
#72761=CARTESIAN_POINT('Ctrl Pts',(18.3502953373601,3.32807684986788,4.03044584770528));
#72762=CARTESIAN_POINT('Ctrl Pts',(18.3105400132211,4.53430519795815,2.60012800101859));
#72763=CARTESIAN_POINT('Ctrl Pts',(18.270784689082,4.86224859991823,0.990832601089107));
#72764=CARTESIAN_POINT('Ctrl Pts',(18.231029364943,5.19019200187832,-0.618462798840377));
#72765=CARTESIAN_POINT('Ctrl Pts',(18.1912740408039,4.63985045770823,-2.40673575201266));
#72766=CARTESIAN_POINT('Ctrl Pts',(18.1515187166649,3.46382593703186,-3.5531845672204));
#72767=CARTESIAN_POINT('Ctrl Pts',(18.1117633925258,2.28780141635541,-4.69963338242821));
#72768=CARTESIAN_POINT('Ctrl Pts',(18.0720080683867,0.486093919172618,-5.20425805967141));
#72769=CARTESIAN_POINT('Ctrl Pts',(18.0322527442477,-1.11432852476172,-4.83544027258017));
#72770=CARTESIAN_POINT('Ctrl Pts',(17.9924974201086,-2.71475096869597,-4.46662248548895));
#72771=CARTESIAN_POINT('Ctrl Pts',(17.9527420959696,-4.11388835938179,-3.22436223406338));
#72772=CARTESIAN_POINT('Ctrl Pts',(17.9129867718305,-4.66954883540947,-1.67884614081038));
#72773=CARTESIAN_POINT('Ctrl Pts',(17.8992540852684,-4.8614907027567,-1.14497832448687));
#72774=CARTESIAN_POINT('Ctrl Pts',(17.8855213987063,-4.95278724229807,-0.574925423451077));
#72775=CARTESIAN_POINT('Ctrl Pts',(17.8717887121442,-4.94888348879255,-0.00366329764976359));
#72776=CARTESIAN_POINT('Ctrl Pts',(17.7664112878558,-4.95024685397467,-0.00414268332982216));
#72777=CARTESIAN_POINT('Ctrl Pts',(17.7788054612032,-4.95430551813832,-0.519366743091031));
#72778=CARTESIAN_POINT('Ctrl Pts',(17.7911996345505,-4.88030293042791,-1.03345379940426));
#72779=CARTESIAN_POINT('Ctrl Pts',(17.8035938078979,-4.72337350536271,-1.52083992991365));
#72780=CARTESIAN_POINT('Ctrl Pts',(17.8433491320369,-4.22000954670368,-3.08417078355551));
#72781=CARTESIAN_POINT('Ctrl Pts',(17.883104456176,-2.86344613526889,-4.37278700908486));
#72782=CARTESIAN_POINT('Ctrl Pts',(17.922859780315,-1.2763340472501,-4.79522499611982));
#72783=CARTESIAN_POINT('Ctrl Pts',(17.9626151044541,0.310778040768601,-5.21766298315475));
#72784=CARTESIAN_POINT('Ctrl Pts',(18.0023704285931,2.12843880537138,-4.77392273169524));
#72785=CARTESIAN_POINT('Ctrl Pts',(18.0421257527322,3.34235780617494,-3.66767714760767));
#72786=CARTESIAN_POINT('Ctrl Pts',(18.0818810768712,4.55627680697864,-2.56143156351998));
#72787=CARTESIAN_POINT('Ctrl Pts',(18.1216364010103,5.16645404398317,-0.792680646804141));
#72788=CARTESIAN_POINT('Ctrl Pts',(18.1613917251494,4.89282348633957,0.826734355827807));
#72789=CARTESIAN_POINT('Ctrl Pts',(18.2011470492884,4.61919292869599,2.44614935845966));
#72790=CARTESIAN_POINT('Ctrl Pts',(18.2409023734275,3.46175457640439,3.91622844700751));
#72791=CARTESIAN_POINT('Ctrl Pts',(18.2806576975665,1.95176253994259,4.56221813937683));
#72792=CARTESIAN_POINT('Ctrl Pts',(18.3204130217056,0.441770503480876,5.20820783174611));
#72793=CARTESIAN_POINT('Ctrl Pts',(18.3601683458446,-1.42077521715118,5.03010812793685));
#72794=CARTESIAN_POINT('Ctrl Pts',(18.3999236699837,-2.78098237816365,4.10966523891245));
#72795=CARTESIAN_POINT('Ctrl Pts',(18.4387528759411,-4.10950290072166,3.21066448155629));
#72796=CARTESIAN_POINT('Ctrl Pts',(18.4775820818985,-4.95881666157094,1.60350412336648));
#72797=CARTESIAN_POINT('Ctrl Pts',(18.5164112878559,-4.96205143092805,-0.000716217698562718));
#72798=CARTESIAN_POINT('Origin',(10.45,0.,0.));
#72799=CARTESIAN_POINT('',(19.3717887121442,-4.95406386564724,0.00456011872589132));
#72800=CARTESIAN_POINT('',(19.2664112878559,-4.9523954629479,0.00451814608447948));
#72801=CARTESIAN_POINT('',(10.45,-4.954,-6.06690024297599E-16));
#72802=CARTESIAN_POINT('Ctrl Pts',(19.3717887121442,-4.95406386564724,0.00456011872589132));
#72803=CARTESIAN_POINT('Ctrl Pts',(19.3625852883749,-4.95759204267437,0.386396835530268));
#72804=CARTESIAN_POINT('Ctrl Pts',(19.3533818646057,-4.91718650431454,0.767494781265623));
#72805=CARTESIAN_POINT('Ctrl Pts',(19.3441784408365,-4.83002298839371,1.13758016085729));
#72806=CARTESIAN_POINT('Ctrl Pts',(19.3044231166974,-4.45350943045892,2.73620960504211));
#72807=CARTESIAN_POINT('Ctrl Pts',(19.2646677925584,-3.20453195115239,4.12935397174361));
#72808=CARTESIAN_POINT('Ctrl Pts',(19.2249124684193,-1.65636032200206,4.67757214529986));
#72809=CARTESIAN_POINT('Ctrl Pts',(19.1851571442803,-0.108188692851636,
5.22579031885614));
#72810=CARTESIAN_POINT('Ctrl Pts',(19.1454018201412,1.73917708614262,4.92908229926707));
#72811=CARTESIAN_POINT('Ctrl Pts',(19.1056464960022,3.03781223202891,3.92363448013744));
#72812=CARTESIAN_POINT('Ctrl Pts',(19.0658911718631,4.33644737791506,2.91818666100792));
#72813=CARTESIAN_POINT('Ctrl Pts',(19.0261358477241,5.08635189069337,1.203999042338));
#72814=CARTESIAN_POINT('Ctrl Pts',(18.986380523585,4.94332613840025,-0.432131207154393));
#72815=CARTESIAN_POINT('Ctrl Pts',(18.946625199446,4.80030038610712,-2.06826145664697));
#72816=CARTESIAN_POINT('Ctrl Pts',(18.9068698753069,3.76434436874231,-3.626334336962));
#72817=CARTESIAN_POINT('Ctrl Pts',(18.8671145511678,2.31095286441626,-4.39120798291701));
#72818=CARTESIAN_POINT('Ctrl Pts',(18.8273592270288,0.8575613600903,-5.15608162887199));
#72819=CARTESIAN_POINT('Ctrl Pts',(18.7876039028897,-1.01326563119685,-5.12775604046705));
#72820=CARTESIAN_POINT('Ctrl Pts',(18.7478485787507,-2.44283483464014,-4.31923241577211));
#72821=CARTESIAN_POINT('Ctrl Pts',(18.7080932546116,-3.87240403808351,-3.51070879107711));
#72822=CARTESIAN_POINT('Ctrl Pts',(18.6683379304726,-4.86071545368295,-1.92198713009198));
#72823=CARTESIAN_POINT('Ctrl Pts',(18.6285826063335,-4.95414276006255,-0.282276821059833));
#72824=CARTESIAN_POINT('Ctrl Pts',(18.6263179749371,-4.95946477455733,-0.188871987183443));
#72825=CARTESIAN_POINT('Ctrl Pts',(18.6240533435406,-4.96188295865765,-0.0953016990494065));
#72826=CARTESIAN_POINT('Ctrl Pts',(18.6217887121442,-4.96146530959486,-0.00170939900883904));
#72827=CARTESIAN_POINT('Ctrl Pts',(18.5164112878559,-4.96205143092805,-0.000716217698562718));
#72828=CARTESIAN_POINT('Ctrl Pts',(18.5173374060375,-4.96212858364445,-0.0389785923369267));
#72829=CARTESIAN_POINT('Ctrl Pts',(18.5182635242192,-4.96172442433453,-0.0772392944770803));
#72830=CARTESIAN_POINT('Ctrl Pts',(18.5191896424009,-4.96083397518572,-0.115488675744613));
#72831=CARTESIAN_POINT('Ctrl Pts',(18.5589449665399,-4.92260980980206,-1.75741362713735));
#72832=CARTESIAN_POINT('Ctrl Pts',(18.598700290679,-3.9882928776417,-3.37847745568325));
#72833=CARTESIAN_POINT('Ctrl Pts',(18.638455614818,-2.58672650303079,-4.23462600026262));
#72834=CARTESIAN_POINT('Ctrl Pts',(18.6782109389571,-1.18516012841989,-5.090774544842));
#72835=CARTESIAN_POINT('Ctrl Pts',(18.7179662630961,0.68365568864165,-5.18200780545489));
#72836=CARTESIAN_POINT('Ctrl Pts',(18.7577215872352,2.16195078478016,-4.46645051106252));
#72837=CARTESIAN_POINT('Ctrl Pts',(18.7974769113742,3.64024588091884,-3.75089321667006));
#72838=CARTESIAN_POINT('Ctrl Pts',(18.8372322355133,4.72802025613451,-2.22854536727209));
#72839=CARTESIAN_POINT('Ctrl Pts',(18.8769875596524,4.92599495793533,-0.598151350393721));
#72840=CARTESIAN_POINT('Ctrl Pts',(18.9167428837914,5.12396965973613,1.03224266648446));
#72841=CARTESIAN_POINT('Ctrl Pts',(18.9564982079305,4.43214468812251,2.77068285084289));
#72842=CARTESIAN_POINT('Ctrl Pts',(18.9962535320695,3.16806167213509,3.81924031780284));
#72843=CARTESIAN_POINT('Ctrl Pts',(19.0360088562086,1.90397865614767,4.86779778476279));
#72844=CARTESIAN_POINT('Ctrl Pts',(19.0757641803476,0.0676375957864397,
5.22647253432405));
#72845=CARTESIAN_POINT('Ctrl Pts',(19.1155195044867,-1.49809697571037,4.73063598419384));
#72846=CARTESIAN_POINT('Ctrl Pts',(19.1552748286257,-3.06383154720717,4.23479943406362));
#72847=CARTESIAN_POINT('Ctrl Pts',(19.1950301527648,-4.35895962983965,2.8844515842419));
#72848=CARTESIAN_POINT('Ctrl Pts',(19.2347854769038,-4.78902872760088,1.29939032234185));
#72849=CARTESIAN_POINT('Ctrl Pts',(19.2453274138878,-4.90307034153692,0.879078922532937));
#72850=CARTESIAN_POINT('Ctrl Pts',(19.2558693508718,-4.95628501739502,0.442263563534826));
#72851=CARTESIAN_POINT('Ctrl Pts',(19.2664112878559,-4.9523954629479,0.00451814608447948));
#72852=CARTESIAN_POINT('Origin',(10.45,0.,0.));
#72853=CARTESIAN_POINT('',(20.1217887121442,-4.94586503871743,-0.000545303237105832));
#72854=CARTESIAN_POINT('',(20.0164112878559,-4.94619904628785,-0.00144379608614997));
#72855=CARTESIAN_POINT('',(10.45,-4.954,-6.06690024297599E-16));
#72856=CARTESIAN_POINT('Ctrl Pts',(20.1217887121442,-4.94586503871743,-0.000545303237105832));
#72857=CARTESIAN_POINT('Ctrl Pts',(20.1011172332093,-4.9450216042098,0.8606761091776));
#72858=CARTESIAN_POINT('Ctrl Pts',(20.0804457542744,-4.73140686367877,1.7222891587838));
#72859=CARTESIAN_POINT('Ctrl Pts',(20.0597742753395,-4.30742932436548,2.46358748705707));
#72860=CARTESIAN_POINT('Ctrl Pts',(20.0200189512004,-3.49203703646159,3.88925013156671));
#72861=CARTESIAN_POINT('Ctrl Pts',(19.9802636270614,-1.89857874589106,4.86990636414725));
#72862=CARTESIAN_POINT('Ctrl Pts',(19.9405083029223,-0.258437912571716,
4.9554435256729));
#72863=CARTESIAN_POINT('Ctrl Pts',(19.9007529787833,1.38170292074772,5.04098068719854));
#72864=CARTESIAN_POINT('Ctrl Pts',(19.8609976546442,3.06852629681598,4.23139877766919));
#72865=CARTESIAN_POINT('Ctrl Pts',(19.8212423305052,4.0277949956444,2.8982888337517));
#72866=CARTESIAN_POINT('Ctrl Pts',(19.7814870063661,4.98706369447276,1.56517888983429));
#72867=CARTESIAN_POINT('Ctrl Pts',(19.741731682227,5.21877771606137,-0.291459088471185));
#72868=CARTESIAN_POINT('Ctrl Pts',(19.701976358088,4.61658234511971,-1.81944445958564));
#72869=CARTESIAN_POINT('Ctrl Pts',(19.6622210339489,4.01438697417804,-3.3474298307001));
#72870=CARTESIAN_POINT('Ctrl Pts',(19.6224657098099,2.5782822107061,-4.54676259462353));
#72871=CARTESIAN_POINT('Ctrl Pts',(19.5827103856708,0.967427617855369,-4.86695947127142));
#72872=CARTESIAN_POINT('Ctrl Pts',(19.5429550615318,-0.64342697499545,-5.18715634791932));
#72873=CARTESIAN_POINT('Ctrl Pts',(19.5031997373927,-2.42903139722507,-4.62821733729157));
#72874=CARTESIAN_POINT('Ctrl Pts',(19.4634444132537,-3.56980879005835,-3.44669057114357));
#72875=CARTESIAN_POINT('Ctrl Pts',(19.4328925128838,-4.44649431595391,-2.53868921974274));
#72876=CARTESIAN_POINT('Ctrl Pts',(19.402340612514,-4.94235164683355,-1.26299395917723));
#72877=CARTESIAN_POINT('Ctrl Pts',(19.3717887121442,-4.95406386564724,0.00456011872589132));
#72878=CARTESIAN_POINT('Ctrl Pts',(19.2664112878559,-4.9523954629479,0.00451814608447948));
#72879=CARTESIAN_POINT('Ctrl Pts',(19.2956246750109,-4.9416168878059,-1.20854415686073));
#72880=CARTESIAN_POINT('Ctrl Pts',(19.324838062166,-4.49231642076917,-2.42874868009104));
#72881=CARTESIAN_POINT('Ctrl Pts',(19.354051449321,-3.68371563120667,-3.32467299324095));
#72882=CARTESIAN_POINT('Ctrl Pts',(19.39380677346,-2.58332332416117,-4.54390037294535));
#72883=CARTESIAN_POINT('Ctrl Pts',(19.4335620975991,-0.817528597180191,
-5.16258045837549));
#72884=CARTESIAN_POINT('Ctrl Pts',(19.4733174217382,0.803184168333579,-4.89674448540256));
#72885=CARTESIAN_POINT('Ctrl Pts',(19.5130727458772,2.42389693384726,-4.63090851242965));
#72886=CARTESIAN_POINT('Ctrl Pts',(19.5528280700163,3.89952773789364,-3.4805564810538));
#72887=CARTESIAN_POINT('Ctrl Pts',(19.5925833941553,4.55277490937709,-1.97368994224741));
#72888=CARTESIAN_POINT('Ctrl Pts',(19.6323387182944,5.20602208086054,-0.46682340344102));
#72889=CARTESIAN_POINT('Ctrl Pts',(19.6720940424334,5.03688561978088,1.39655764279609));
#72890=CARTESIAN_POINT('Ctrl Pts',(19.7118493665725,4.12299768685097,2.76117754550548));
#72891=CARTESIAN_POINT('Ctrl Pts',(19.7516046907115,3.20910975392107,4.12579744821486));
#72892=CARTESIAN_POINT('Ctrl Pts',(19.7913600148506,1.55047034914099,4.99165620739672));
#72893=CARTESIAN_POINT('Ctrl Pts',(19.8311153389897,-0.091619504549001,
4.96133220314547));
#72894=CARTESIAN_POINT('Ctrl Pts',(19.8708706631287,-1.73370935823909,4.93100819889422));
#72895=CARTESIAN_POINT('Ctrl Pts',(19.9106259872678,-3.35924966083898,4.00450143120977));
#72896=CARTESIAN_POINT('Ctrl Pts',(19.9503813114068,-4.22213158867454,2.60707042703084));
#72897=CARTESIAN_POINT('Ctrl Pts',(19.9723913035565,-4.69985438100614,1.83340184055148));
#72898=CARTESIAN_POINT('Ctrl Pts',(19.9944012957062,-4.94381231674025,0.915388760842907));
#72899=CARTESIAN_POINT('Ctrl Pts',(20.0164112878559,-4.94619904628785,-0.00144379608614997));
#72900=CARTESIAN_POINT('Origin',(10.45,0.,0.));
#72901=CARTESIAN_POINT('',(20.8717887121442,-4.95607142653195,-0.00434810948939879));
#72902=CARTESIAN_POINT('',(20.7664112878559,-4.95770599871256,-0.00394983957152954));
#72903=CARTESIAN_POINT('',(10.45,-4.954,-6.06690024297599E-16));
#72904=CARTESIAN_POINT('Ctrl Pts',(20.8717887121442,-4.95607142653195,-0.00434810948939879));
#72905=CARTESIAN_POINT('Ctrl Pts',(20.8396491780436,-4.94383012710083,1.32768880656287));
#72906=CARTESIAN_POINT('Ctrl Pts',(20.807509643943,-4.38908727589373,2.66871408325221));
#72907=CARTESIAN_POINT('Ctrl Pts',(20.7753701098425,-3.42947542021679,3.58635037787954));
#72908=CARTESIAN_POINT('Ctrl Pts',(20.7356147857034,-2.2424737589373,4.7214299412772));
#72909=CARTESIAN_POINT('Ctrl Pts',(20.6958594615644,-0.43599397497383,5.20869451049855));
#72910=CARTESIAN_POINT('Ctrl Pts',(20.6561041374253,1.16080546390229,4.82449389737022));
#72911=CARTESIAN_POINT('Ctrl Pts',(20.6163488132863,2.7576049027785,4.44029328424187));
#72912=CARTESIAN_POINT('Ctrl Pts',(20.5765934891472,4.14472399656744,3.1846274887637));
#72913=CARTESIAN_POINT('Ctrl Pts',(20.5368381650081,4.68548717733165,1.63383616126237));
#72914=CARTESIAN_POINT('Ctrl Pts',(20.4970828408691,5.22625035809582,0.0830448337611306));
#72915=CARTESIAN_POINT('Ctrl Pts',(20.45732751673,4.92065762583549,-1.76287202576309));
#72916=CARTESIAN_POINT('Ctrl Pts',(20.417572192591,3.90897337979402,-3.05665467576067));
#72917=CARTESIAN_POINT('Ctrl Pts',(20.377816868452,2.89728913375249,-4.35043732575833));
#72918=CARTESIAN_POINT('Ctrl Pts',(20.3380615443129,1.17951337392963,-5.09208576622906));
#72919=CARTESIAN_POINT('Ctrl Pts',(20.2983062201738,-0.455909805456886,
-4.94118983040281));
#72920=CARTESIAN_POINT('Ctrl Pts',(20.2585508960348,-2.0913329848434,-4.79029389457655));
#72921=CARTESIAN_POINT('Ctrl Pts',(20.2187955718957,-3.64440358379368,-3.74685358245331));
#72922=CARTESIAN_POINT('Ctrl Pts',(20.1790402477566,-4.40227574065016,-2.28979889817227));
#72923=CARTESIAN_POINT('Ctrl Pts',(20.1599564025525,-4.76607896045046,-1.59036538452368));
#72924=CARTESIAN_POINT('Ctrl Pts',(20.1408725573483,-4.9466436948375,-0.795622238602891));
#72925=CARTESIAN_POINT('Ctrl Pts',(20.1217887121442,-4.94586503871743,-0.000545303237105832));
#72926=CARTESIAN_POINT('Ctrl Pts',(20.0164112878559,-4.94619904628785,-0.00144379608614997));
#72927=CARTESIAN_POINT('Ctrl Pts',(20.0341566198452,-4.94812332267574,-0.740630706773701));
#72928=CARTESIAN_POINT('Ctrl Pts',(20.0519019518346,-4.79302084621013,-1.47905025092917));
#72929=CARTESIAN_POINT('Ctrl Pts',(20.069647283824,-4.47680051100919,-2.14043653216113));
#72930=CARTESIAN_POINT('Ctrl Pts',(20.109402607963,-3.76836395243713,-3.62215724650104));
#72931=CARTESIAN_POINT('Ctrl Pts',(20.1491579321021,-2.25126728222178,-4.71724343450763));
#72932=CARTESIAN_POINT('Ctrl Pts',(20.1889132562412,-0.621844642435137,
-4.9230600853795));
#72933=CARTESIAN_POINT('Ctrl Pts',(20.2286685803802,1.00757799735169,-5.1288767362514));
#72934=CARTESIAN_POINT('Ctrl Pts',(20.2684239045193,2.74932660670983,-4.44542384998839));
#72935=CARTESIAN_POINT('Ctrl Pts',(20.3081792286583,3.80395376253568,-3.18640034146257));
#72936=CARTESIAN_POINT('Ctrl Pts',(20.3479345527974,4.85858091836135,-1.92737683293696));
#72937=CARTESIAN_POINT('Ctrl Pts',(20.3876898769364,5.226086620655,-0.0927827021487665));
#72938=CARTESIAN_POINT('Ctrl Pts',(20.4274452010755,4.73778895682836,1.4753193431042));
#72939=CARTESIAN_POINT('Ctrl Pts',(20.4672005252145,4.24949129300169,3.04342138835725));
#72940=CARTESIAN_POINT('Ctrl Pts',(20.5069558493536,2.90539026305463,4.34503134807505));
#72941=CARTESIAN_POINT('Ctrl Pts',(20.5467111734926,1.32241651875205,4.78272160119255));
#72942=CARTESIAN_POINT('Ctrl Pts',(20.5864664976317,-0.260557225550523,
5.22041185431005));
#72943=CARTESIAN_POINT('Ctrl Pts',(20.6262218217707,-2.08240368420862,4.79418240082726));
#72944=CARTESIAN_POINT('Ctrl Pts',(20.6659771459098,-3.30691121976839,3.69966884303881));
#72945=CARTESIAN_POINT('Ctrl Pts',(20.6994551932251,-4.33807175238249,2.77797652965785));
#72946=CARTESIAN_POINT('Ctrl Pts',(20.7329332405405,-4.94563764625562,1.38237978314307));
#72947=CARTESIAN_POINT('Ctrl Pts',(20.7664112878559,-4.95770599871256,-0.00394983957152954));
#72948=CARTESIAN_POINT('Origin',(10.45,0.,0.));
#72949=CARTESIAN_POINT('',(21.6217887121442,-4.96026724855995,0.00275821796382324));
#72950=CARTESIAN_POINT('',(21.5164112878558,-4.95893736719177,0.00348609211932242));
#72951=CARTESIAN_POINT('',(10.45,-4.954,-6.06690024297599E-16));
#72952=CARTESIAN_POINT('Ctrl Pts',(21.6217887121442,-4.96026724855995,0.00275821796382324));
#72953=CARTESIAN_POINT('Ctrl Pts',(21.617936447017,-4.96133041918326,0.162065765024171));
#72954=CARTESIAN_POINT('Ctrl Pts',(21.6140841818898,-4.9543231377804,0.321278587713524));
#72955=CARTESIAN_POINT('Ctrl Pts',(21.6102319167626,-4.93893914224454,0.479677850220928));
#72956=CARTESIAN_POINT('Ctrl Pts',(21.5704765926236,-4.78017651587008,2.11435610222958));
#72957=CARTESIAN_POINT('Ctrl Pts',(21.5307212684845,-3.72927606286137,3.6623884688657));
#72958=CARTESIAN_POINT('Ctrl Pts',(21.4909659443455,-2.26859192696917,4.41324159316915));
#72959=CARTESIAN_POINT('Ctrl Pts',(21.4512106202064,-0.807907791077042,
5.16409471747255));
#72960=CARTESIAN_POINT('Ctrl Pts',(21.4114552960674,1.06256002769845,5.11776859944335));
#72961=CARTESIAN_POINT('Ctrl Pts',(21.3716999719283,2.48428311160319,4.29552652327873));
#72962=CARTESIAN_POINT('Ctrl Pts',(21.3319446477892,3.90600619550817,3.47328444711397));
#72963=CARTESIAN_POINT('Ctrl Pts',(21.2921893236502,4.87898454454212,1.87512641281354));
#72964=CARTESIAN_POINT('Ctrl Pts',(21.2524339995111,4.95662958117358,0.234593021684137));
#72965=CARTESIAN_POINT('Ctrl Pts',(21.2126786753721,5.03427461780502,-1.40594036944508));
#72966=CARTESIAN_POINT('Ctrl Pts',(21.172923351233,4.21658634203401,-3.08884911740338));
#72967=CARTESIAN_POINT('Ctrl Pts',(21.133168027094,2.87887654194239,-4.04169278236751));
#72968=CARTESIAN_POINT('Ctrl Pts',(21.0934127029549,1.54116674185078,-4.99453644733165));
#72969=CARTESIAN_POINT('Ctrl Pts',(21.0536573788158,-0.316564582561406,
-5.21731502930186));
#72970=CARTESIAN_POINT('Ctrl Pts',(21.0139020546768,-1.8416349533865,-4.60777510185263));
#72971=CARTESIAN_POINT('Ctrl Pts',(20.9741467305377,-3.36670532421159,-3.99823517440339));
#72972=CARTESIAN_POINT('Ctrl Pts',(20.9343914063987,-4.55911474144951,-2.55637673753478));
#72973=CARTESIAN_POINT('Ctrl Pts',(20.8946360822596,-4.8715576807707,-0.944000240313443));
#72974=CARTESIAN_POINT('Ctrl Pts',(20.8870202922212,-4.931411294756,-0.635122847617899));
#72975=CARTESIAN_POINT('Ctrl Pts',(20.8794045021827,-4.95897212714491,-0.319987827365635));
#72976=CARTESIAN_POINT('Ctrl Pts',(20.8717887121442,-4.95607142653195,-0.00434810948939879));
#72977=CARTESIAN_POINT('Ctrl Pts',(20.7664112878559,-4.95770599871256,-0.00394983957152954));
#72978=CARTESIAN_POINT('Ctrl Pts',(20.7726885646796,-4.9599688663304,-0.263892563491772));
#72979=CARTESIAN_POINT('Ctrl Pts',(20.7789658415033,-4.94129531995109,-0.52350947525168));
#72980=CARTESIAN_POINT('Ctrl Pts',(20.785243118327,-4.90055213313902,-0.779615388488902));
#72981=CARTESIAN_POINT('Ctrl Pts',(20.824998442466,-4.64251689848844,-2.40158840013364));
#72982=CARTESIAN_POINT('Ctrl Pts',(20.8647537666051,-3.49927781672605,-3.88273676132907));
#72983=CARTESIAN_POINT('Ctrl Pts',(20.9045090907441,-1.99557165697884,-4.54322629036293));
#72984=CARTESIAN_POINT('Ctrl Pts',(20.9442644148832,-0.49186549723137,-5.2037158193969));
#72985=CARTESIAN_POINT('Ctrl Pts',(20.9840197390222,1.37230774050106,-5.04354651626898));
#72986=CARTESIAN_POINT('Ctrl Pts',(21.0237750631613,2.74130879627203,-4.13623469438857));
#72987=CARTESIAN_POINT('Ctrl Pts',(21.0635303873004,4.11030985204285,-3.22892287250826));
#72988=CARTESIAN_POINT('Ctrl Pts',(21.1032857114394,4.98413872585233,-1.57446853187563));
#72989=CARTESIAN_POINT('Ctrl Pts',(21.1430410355785,4.96171558468266,0.0677482125175924));
#72990=CARTESIAN_POINT('Ctrl Pts',(21.1827963597175,4.93929244351299,1.70996495691082));
#72991=CARTESIAN_POINT('Ctrl Pts',(21.2225516838566,4.02061728736416,3.33994410506463));
#72992=CARTESIAN_POINT('Ctrl Pts',(21.2623070079956,2.62735400177417,4.20953944190376));
#72993=CARTESIAN_POINT('Ctrl Pts',(21.3020623321347,1.23409071618409,5.07913477874293));
#72994=CARTESIAN_POINT('Ctrl Pts',(21.3418176562737,-0.633760698847205,
5.18834630426734));
#72995=CARTESIAN_POINT('Ctrl Pts',(21.3815729804128,-2.11887273206807,4.48704688061987));
#72996=CARTESIAN_POINT('Ctrl Pts',(21.4213283045518,-3.60398476528886,3.78574745697245));
#72997=CARTESIAN_POINT('Ctrl Pts',(21.4610836286909,-4.70635741669926,2.27393708415325));
#72998=CARTESIAN_POINT('Ctrl Pts',(21.50083895283,-4.92001125233576,0.645523539827611));
#72999=CARTESIAN_POINT('Ctrl Pts',(21.5060297311719,-4.94790763418439,0.432904628003932));
#73000=CARTESIAN_POINT('Ctrl Pts',(21.5112205095139,-4.96065310509214,0.218297861039164));
#73001=CARTESIAN_POINT('Ctrl Pts',(21.5164112878558,-4.95893736719177,0.00348609211932242));
#73002=CARTESIAN_POINT('Origin',(10.45,0.,0.));
#73003=CARTESIAN_POINT('',(22.3717887121441,-4.9475429831306,0.00290303294213062));
#73004=CARTESIAN_POINT('',(22.2664112878559,-4.94668796515972,0.00213281205902905));
#73005=CARTESIAN_POINT('',(10.45,-4.954,-6.06690024297599E-16));
#73006=CARTESIAN_POINT('Ctrl Pts',(22.3717887121441,-4.9475429831306,0.00290303294213062));
#73007=CARTESIAN_POINT('Ctrl Pts',(22.3564683918513,-4.95093651841198,0.640642072587425));
#73008=CARTESIAN_POINT('Ctrl Pts',(22.3411480715585,-4.83658160029764,1.27721064111222));
#73009=CARTESIAN_POINT('Ctrl Pts',(22.3258277512656,-4.59886119640998,1.8637828164629));
#73010=CARTESIAN_POINT('Ctrl Pts',(22.2860724271265,-3.98199082226831,3.38590288420711));
#73011=CARTESIAN_POINT('Ctrl Pts',(22.2463171029875,-2.53441208857938,4.57136135250474));
#73012=CARTESIAN_POINT('Ctrl Pts',(22.2065617788484,-0.920551010767648,
4.87604312197529));
#73013=CARTESIAN_POINT('Ctrl Pts',(22.1668064547094,0.693310067043993,5.18072489144581));
#73014=CARTESIAN_POINT('Ctrl Pts',(22.1270511305703,2.47345348897841,4.6046299620894));
#73015=CARTESIAN_POINT('Ctrl Pts',(22.0872958064313,3.60280894777447,3.41218088275286));
#73016=CARTESIAN_POINT('Ctrl Pts',(22.0475404822922,4.73216440657066,2.21973180341618));
#73017=CARTESIAN_POINT('Ctrl Pts',(22.0077851581532,5.21073190222835,0.410928574099224));
#73018=CARTESIAN_POINT('Ctrl Pts',(21.9680298340141,4.81885312749869,-1.18400389627061));
#73019=CARTESIAN_POINT('Ctrl Pts',(21.9282745098751,4.42697435276905,-2.77893636664036));
#73020=CARTESIAN_POINT('Ctrl Pts',(21.888519185736,3.16464930765215,-4.15999807806301));
#73021=CARTESIAN_POINT('Ctrl Pts',(21.848763861597,1.61127417998797,-4.69329374828509));
#73022=CARTESIAN_POINT('Ctrl Pts',(21.8090085374579,0.057899052323781,-5.22658941850718));
#73023=CARTESIAN_POINT('Ctrl Pts',(21.7692532133189,-1.7865261578877,-4.91211904752869));
#73024=CARTESIAN_POINT('Ctrl Pts',(21.7294978891798,-3.07542636312338,-3.8942217933489));
#73025=CARTESIAN_POINT('Ctrl Pts',(21.6935948301679,-4.23943297434202,-2.97495812297814));
#73026=CARTESIAN_POINT('Ctrl Pts',(21.657691771156,-4.95035851269461,-1.48198597131669));
#73027=CARTESIAN_POINT('Ctrl Pts',(21.6217887121442,-4.96026724855995,0.00275821796382324));
#73028=CARTESIAN_POINT('Ctrl Pts',(21.5164112878558,-4.95893736719177,0.00348609211932242));
#73029=CARTESIAN_POINT('Ctrl Pts',(21.5509758336529,-4.94751254853715,-1.42691041789185));
#73030=CARTESIAN_POINT('Ctrl Pts',(21.58554037945,-4.29487617807464,-2.86639673660996));
#73031=CARTESIAN_POINT('Ctrl Pts',(21.6201049252471,-3.20466525102918,-3.78857915219258));
#73032=CARTESIAN_POINT('Ctrl Pts',(21.6598602493862,-1.95073039422339,-4.84925158405509));
#73033=CARTESIAN_POINT('Ctrl Pts',(21.6996155735252,-0.117925660749211,
-5.2255797319479));
#73034=CARTESIAN_POINT('Ctrl Pts',(21.7393708976643,1.45250755935842,-4.74483225768718));
#73035=CARTESIAN_POINT('Ctrl Pts',(21.7791262218033,3.02294077946596,-4.26408478342648));
#73036=CARTESIAN_POINT('Ctrl Pts',(21.8188815459424,4.33100248620699,-2.92626168701236));
#73037=CARTESIAN_POINT('Ctrl Pts',(21.8586368700815,4.77630376289404,-1.3454121034636));
#73038=CARTESIAN_POINT('Ctrl Pts',(21.8983921942205,5.22160503958109,0.235437480085154));
#73039=CARTESIAN_POINT('Ctrl Pts',(21.9381475183596,4.80414588621417,2.05931355076854));
#73040=CARTESIAN_POINT('Ctrl Pts',(21.9779028424986,3.71553641381448,3.28907289691194));
#73041=CARTESIAN_POINT('Ctrl Pts',(22.0176581666377,2.62692694141473,4.51883224305541));
#73042=CARTESIAN_POINT('Ctrl Pts',(22.0574134907767,0.867167149982128,5.15447486465883));
#73043=CARTESIAN_POINT('Ctrl Pts',(22.0971688149158,-0.756028561870759,
4.90424634140841));
#73044=CARTESIAN_POINT('Ctrl Pts',(22.1369241390548,-2.37922427372355,4.654017818158));
#73045=CARTESIAN_POINT('Ctrl Pts',(22.1766794631939,-3.86585590599665,3.51791815005386));
#73046=CARTESIAN_POINT('Ctrl Pts',(22.216434787333,-4.5335725033689,2.0174071776118));
#73047=CARTESIAN_POINT('Ctrl Pts',(22.2330936208406,-4.81336847703526,1.38864202457572));
#73048=CARTESIAN_POINT('Ctrl Pts',(22.2497524543482,-4.94937155730909,0.695890067533741));
#73049=CARTESIAN_POINT('Ctrl Pts',(22.2664112878559,-4.94668796515972,0.00213281205902905));
#73050=CARTESIAN_POINT('Origin',(10.45,0.,0.));
#73051=CARTESIAN_POINT('',(23.1217887121442,-4.9496403119333,-0.00395742179621961));
#73052=CARTESIAN_POINT('',(23.0164112878558,-4.95110446228237,-0.0043407105877043));
#73053=CARTESIAN_POINT('',(10.45,-4.954,-6.06690024297599E-16));
#73054=CARTESIAN_POINT('Ctrl Pts',(23.1217887121442,-4.9496403119333,-0.00395742179621961));
#73055=CARTESIAN_POINT('Ctrl Pts',(23.0950003366856,-4.94133049104857,1.1099757704877));
#73056=CARTESIAN_POINT('Ctrl Pts',(23.0682119612271,-4.56944157248637,2.22893581023816));
#73057=CARTESIAN_POINT('Ctrl Pts',(23.0414235857686,-3.87938006227662,3.09412685958389));
#73058=CARTESIAN_POINT('Ctrl Pts',(23.0016682616295,-2.8552933625529,4.37811478420478));
#73059=CARTESIAN_POINT('Ctrl Pts',(22.9619129374905,-1.13046069334654,5.10319976786228));
#73060=CARTESIAN_POINT('Ctrl Pts',(22.9221576133514,0.503434791256329,4.93657412602511));
#73061=CARTESIAN_POINT('Ctrl Pts',(22.8824022892124,2.1373302758592,4.76994848418793));
#73062=CARTESIAN_POINT('Ctrl Pts',(22.8426469650733,3.68028857585867,3.71161221685608));
#73063=CARTESIAN_POINT('Ctrl Pts',(22.8028916409343,4.42410528663325,2.24733244171209));
#73064=CARTESIAN_POINT('Ctrl Pts',(22.7631363167952,5.16792199740791,0.783052666567929));
#73065=CARTESIAN_POINT('Ctrl Pts',(22.7233809926562,5.11259711895761,-1.08717061638829));
#73066=CARTESIAN_POINT('Ctrl Pts',(22.6836256685171,4.2835242880408,-2.5049212292111));
#73067=CARTESIAN_POINT('Ctrl Pts',(22.643870344378,3.45445145712413,-3.92267184203367));
#73068=CARTESIAN_POINT('Ctrl Pts',(22.604115020239,1.85163067374112,-4.8879497847228));
#73069=CARTESIAN_POINT('Ctrl Pts',(22.5643596960999,0.210742700366703,-4.95770089910938));
#73070=CARTESIAN_POINT('Ctrl Pts',(22.5246043719609,-1.4301452730079,-5.02745201349597));
#73071=CARTESIAN_POINT('Ctrl Pts',(22.4848490478218,-3.10910043637404,-4.20167629957976));
#73072=CARTESIAN_POINT('Ctrl Pts',(22.4450937236828,-4.05549701075997,-2.8593976090262));
#73073=CARTESIAN_POINT('Ctrl Pts',(22.4206587198366,-4.63718523582063,-2.03438647714267));
#73074=CARTESIAN_POINT('Ctrl Pts',(22.3962237159904,-4.94213049526692,-1.01425297872966));
#73075=CARTESIAN_POINT('Ctrl Pts',(22.3717887121441,-4.9475429831306,0.00290303294213062));
#73076=CARTESIAN_POINT('Ctrl Pts',(22.2664112878559,-4.94668796515972,0.00213281205902905));
#73077=CARTESIAN_POINT('Ctrl Pts',(22.2895077784873,-4.94296732284056,-0.959720726137945));
#73078=CARTESIAN_POINT('Ctrl Pts',(22.3126042691187,-4.67266055328166,-1.92350666786889));
#73079=CARTESIAN_POINT('Ctrl Pts',(22.3357007597501,-4.14937595511098,-2.72137659039115));
#73080=CARTESIAN_POINT('Ctrl Pts',(22.3754560838892,-3.24866124700948,-4.09472710917176));
#73081=CARTESIAN_POINT('Ctrl Pts',(22.4152114080282,-1.59843026833517,-4.97650586995307));
#73082=CARTESIAN_POINT('Ctrl Pts',(22.4549667321673,0.043875352230013,-4.96198411092265));
#73083=CARTESIAN_POINT('Ctrl Pts',(22.4947220563063,1.68618097279528,-4.94746235189222));
#73084=CARTESIAN_POINT('Ctrl Pts',(22.5344773804454,3.32056123525127,-4.03664007305015));
#73085=CARTESIAN_POINT('Ctrl Pts',(22.5742327045844,4.1968498514374,-2.64757675772997));
#73086=CARTESIAN_POINT('Ctrl Pts',(22.6139880287235,5.07313846762344,-1.25851344240995));
#73087=CARTESIAN_POINT('Ctrl Pts',(22.6537433528625,5.19133543753951,0.608790909388));
#73088=CARTESIAN_POINT('Ctrl Pts',(22.6934986770016,4.49718938270871,2.09725988366587));
#73089=CARTESIAN_POINT('Ctrl Pts',(22.7332540011406,3.80304332787779,3.585728857944));
#73090=CARTESIAN_POINT('Ctrl Pts',(22.7730093252797,2.2965542482996,4.69536245470199));
#73091=CARTESIAN_POINT('Ctrl Pts',(22.8127646494188,0.669187494445402,4.91684852937937));
#73092=CARTESIAN_POINT('Ctrl Pts',(22.8525199735578,-0.958179259408607,
5.13833460405671));
#73093=CARTESIAN_POINT('Ctrl Pts',(22.8922752976969,-2.7064236875387,4.47167315665366));
#73094=CARTESIAN_POINT('Ctrl Pts',(22.9320306218359,-3.77311684267058,3.22285597803218));
#73095=CARTESIAN_POINT('Ctrl Pts',(22.9601575105092,-4.52780216527098,2.33931792326669));
#73096=CARTESIAN_POINT('Ctrl Pts',(22.9882843991825,-4.94133281501348,1.16437824414132));
#73097=CARTESIAN_POINT('Ctrl Pts',(23.0164112878558,-4.95110446228237,-0.0043407105877043));
#73098=CARTESIAN_POINT('Origin',(10.45,0.,0.));
#73099=CARTESIAN_POINT('',(23.8717887121442,-4.96185463563362,-0.00114991572043255));
#73100=CARTESIAN_POINT('',(23.7664112878558,-4.96217415958626,-0.000124643869615789));
#73101=CARTESIAN_POINT('',(10.45,-4.954,-6.06690024297599E-16));
#73102=CARTESIAN_POINT('Ctrl Pts',(23.8717887121442,-4.96185463563362,-0.00114991572043255));
#73103=CARTESIAN_POINT('Ctrl Pts',(23.83353228152,-4.95690705322659,1.57957432325722));
#73104=CARTESIAN_POINT('Ctrl Pts',(23.7952758508957,-4.13589002242756,3.16471783957375));
#73105=CARTESIAN_POINT('Ctrl Pts',(23.7570194202716,-2.83985248590647,4.06920736127795));
#73106=CARTESIAN_POINT('Ctrl Pts',(23.7172640961325,-1.49303597636527,5.00913493761048));
#73107=CARTESIAN_POINT('Ctrl Pts',(23.6775087719935,0.366753005962177,5.2140273764652));
#73108=CARTESIAN_POINT('Ctrl Pts',(23.6377534478545,1.88588753612861,4.58984083513389));
#73109=CARTESIAN_POINT('Ctrl Pts',(23.5979981237154,3.40502206629521,3.96565429380252));
#73110=CARTESIAN_POINT('Ctrl Pts',(23.5582427995763,4.5835021443006,2.51238877228494));
#73111=CARTESIAN_POINT('Ctrl Pts',(23.5184874754372,4.88041569105472,0.897080472028412));
#73112=CARTESIAN_POINT('Ctrl Pts',(23.4787321512982,5.17732923780883,-0.718227828228022));
#73113=CARTESIAN_POINT('Ctrl Pts',(23.4389768271592,4.59267625331161,-2.49557890722352));
#73114=CARTESIAN_POINT('Ctrl Pts',(23.3992215030201,3.39480735909076,-3.61918411875537));
#73115=CARTESIAN_POINT('Ctrl Pts',(23.3594661788811,2.19693846486984,-4.74278933028729));
#73116=CARTESIAN_POINT('Ctrl Pts',(23.319710854742,0.385853660925542,-5.21264867435566));
#73117=CARTESIAN_POINT('Ctrl Pts',(23.2799555306029,-1.20717492095737,-4.81310080935351));
#73118=CARTESIAN_POINT('Ctrl Pts',(23.2402002064639,-2.8002035028401,-4.4135529443514));
#73119=CARTESIAN_POINT('Ctrl Pts',(23.2004448823248,-4.17517586266139,-3.14459787027861));
#73120=CARTESIAN_POINT('Ctrl Pts',(23.1606895581858,-4.70099167745142,-1.58867490045016));
#73121=CARTESIAN_POINT('Ctrl Pts',(23.1477226095052,-4.87249642136824,-1.08118128198365));
#73122=CARTESIAN_POINT('Ctrl Pts',(23.1347556608247,-4.9536626917571,-0.54315826136416));
#73123=CARTESIAN_POINT('Ctrl Pts',(23.1217887121442,-4.9496403119333,-0.00395742179621961));
#73124=CARTESIAN_POINT('Ctrl Pts',(23.0164112878558,-4.95110446228237,-0.0043407105877043));
#73125=CARTESIAN_POINT('Ctrl Pts',(23.0280397233216,-4.95514433213716,-0.487521523813275));
#73126=CARTESIAN_POINT('Ctrl Pts',(23.0396681587874,-4.89017271197347,-0.969639075397733));
#73127=CARTESIAN_POINT('Ctrl Pts',(23.0512965942531,-4.75176572372991,-1.42966215252686));
#73128=CARTESIAN_POINT('Ctrl Pts',(23.0910519183922,-4.27857956752358,-3.00239019462453));
#73129=CARTESIAN_POINT('Ctrl Pts',(23.1308072425312,-2.94706537297713,-4.3168733689798));
#73130=CARTESIAN_POINT('Ctrl Pts',(23.1705625666703,-1.36837654416773,-4.76977536126742));
#73131=CARTESIAN_POINT('Ctrl Pts',(23.2103178908093,0.210312284641578,-5.22267735355501));
#73132=CARTESIAN_POINT('Ctrl Pts',(23.2500732149484,2.03617574771381,-4.81399816377506));
#73133=CARTESIAN_POINT('Ctrl Pts',(23.2898285390874,3.27115843759854,-3.73131797622636));
#73134=CARTESIAN_POINT('Ctrl Pts',(23.3295838632265,4.50614112748327,-2.64863778867767));
#73135=CARTESIAN_POINT('Ctrl Pts',(23.3693391873655,5.1502430441805,-0.89195660336024));
#73136=CARTESIAN_POINT('Ctrl Pts',(23.4090945115046,4.90782702469611,0.732424234473895));
#73137=CARTESIAN_POINT('Ctrl Pts',(23.4488498356436,4.66541100521171,2.35680507230812));
#73138=CARTESIAN_POINT('Ctrl Pts',(23.4886051597827,3.53647704954558,3.84888556265903));
#73139=CARTESIAN_POINT('Ctrl Pts',(23.5283604839218,2.0391959986918,4.52381377186346));
#73140=CARTESIAN_POINT('Ctrl Pts',(23.5681158080608,0.541914947838193,5.1987419810678));
#73141=CARTESIAN_POINT('Ctrl Pts',(23.6078711321999,-1.32371319820299,5.05651790912584));
#73142=CARTESIAN_POINT('Ctrl Pts',(23.6476264563389,-2.70138138925913,4.16242116482061));
#73143=CARTESIAN_POINT('Ctrl Pts',(23.6872214001779,-4.07349181308097,3.27193137146485));
#73144=CARTESIAN_POINT('Ctrl Pts',(23.7268163440169,-4.96157138121483,1.6356230549814));
#73145=CARTESIAN_POINT('Ctrl Pts',(23.7664112878558,-4.96217415958626,-0.000124643869615789));
#73146=CARTESIAN_POINT('Origin',(10.45,0.,0.));
#73147=CARTESIAN_POINT('',(24.6217887121442,-4.95310191319871,0.00456049067516617));
#73148=CARTESIAN_POINT('',(24.5164112878558,-4.95147756391153,0.00440602753503367));
#73149=CARTESIAN_POINT('',(10.45,-4.954,-6.06690024297599E-16));
#73150=CARTESIAN_POINT('Ctrl Pts',(24.6217887121442,-4.95310191319871,0.00456049067516617));
#73151=CARTESIAN_POINT('Ctrl Pts',(24.6118195504934,-4.95685877086284,0.418371613716965));
#73152=CARTESIAN_POINT('Ctrl Pts',(24.6018503888425,-4.90934967455833,0.831332155126853));
#73153=CARTESIAN_POINT('Ctrl Pts',(24.5918812271917,-4.80723707609103,1.23031800159294));
#73154=CARTESIAN_POINT('Ctrl Pts',(24.5521259030527,-4.40002936967154,2.82140581908015));
#73155=CARTESIAN_POINT('Ctrl Pts',(24.5123705789136,-3.12447364079982,4.19025699902268));
#73156=CARTESIAN_POINT('Ctrl Pts',(24.4726152547746,-1.56603884578366,4.70858078663671));
#73157=CARTESIAN_POINT('Ctrl Pts',(24.4328599306355,-0.00760405076757592,
5.22690457425072));
#73158=CARTESIAN_POINT('Ctrl Pts',(24.3931046064965,1.83370981039292,4.89470096953634));
#73159=CARTESIAN_POINT('Ctrl Pts',(24.3533492823574,3.11275573225721,3.86444853013826));
#73160=CARTESIAN_POINT('Ctrl Pts',(24.3135939582184,4.39180165412149,2.83419609074018));
#73161=CARTESIAN_POINT('Ctrl Pts',(24.2738386340793,5.10857963668957,1.1058948166584));
#73162=CARTESIAN_POINT('Ctrl Pts',(24.2340833099402,4.93409483649058,-0.527180078630499));
#73163=CARTESIAN_POINT('Ctrl Pts',(24.1943279858012,4.75961003629158,-2.16025497391949));
#73164=CARTESIAN_POINT('Ctrl Pts',(24.1545726616621,3.69386245332543,-3.69810349041561));
#73165=CARTESIAN_POINT('Ctrl Pts',(24.1148173375231,2.2260209345218,-4.4348665695665));
#73166=CARTESIAN_POINT('Ctrl Pts',(24.075062013384,0.758179415718254,-5.17162964871735));
#73167=CARTESIAN_POINT('Ctrl Pts',(24.035306689245,-1.11175603892272,-5.10730729052307));
#73168=CARTESIAN_POINT('Ctrl Pts',(23.9955513651059,-2.52550136214219,-4.27142289648377));
#73169=CARTESIAN_POINT('Ctrl Pts',(23.9557960409669,-3.93924668536173,-3.43553850244443));
#73170=CARTESIAN_POINT('Ctrl Pts',(23.9160407168278,-4.89680187715972,-1.82809207255998));
#73171=CARTESIAN_POINT('Ctrl Pts',(23.8762853926888,-4.95865745468119,-0.186887500712485));
#73172=CARTESIAN_POINT('Ctrl Pts',(23.8747864991739,-4.96098959323151,-0.125009225473019));
#73173=CARTESIAN_POINT('Ctrl Pts',(23.873287605659,-4.9620484827611,-0.0630829625817651));
#73174=CARTESIAN_POINT('Ctrl Pts',(23.8717887121442,-4.96185463563362,-0.00114991572043255));
#73175=CARTESIAN_POINT('Ctrl Pts',(23.7664112878558,-4.96217415958626,-0.000124643869615789));
#73176=CARTESIAN_POINT('Ctrl Pts',(23.7665716681559,-4.96217660115497,-0.0067502804120735));
#73177=CARTESIAN_POINT('Ctrl Pts',(23.766732048456,-4.96216448211318,-0.0133759077566162));
#73178=CARTESIAN_POINT('Ctrl Pts',(23.7668924287561,-4.96213777564951,-0.0200014763019115));
#73179=CARTESIAN_POINT('Ctrl Pts',(23.8066477528951,-4.9555177349126,-1.66235795645061));
#73180=CARTESIAN_POINT('Ctrl Pts',(23.8464030770342,-4.05256941736739,-3.30110150007939));
#73181=CARTESIAN_POINT('Ctrl Pts',(23.8861584011732,-2.66773822677601,-4.18406311101782));
#73182=CARTESIAN_POINT('Ctrl Pts',(23.9259137253123,-1.2829070361847,-5.06702472195621));
#73183=CARTESIAN_POINT('Ctrl Pts',(23.9656690494514,0.583807027452744,-5.19420440020456));
#73184=CARTESIAN_POINT('Ctrl Pts',(24.0054243735904,2.07559848725656,-4.5072277824934));
#73185=CARTESIAN_POINT('Ctrl Pts',(24.0451796977295,3.56738994706038,-3.82025116478225));
#73186=CARTESIAN_POINT('Ctrl Pts',(24.0849350218685,4.68425880303048,-2.31911825111164));
#73187=CARTESIAN_POINT('Ctrl Pts',(24.1246903460076,4.91357198972193,-0.692835958508393));
#73188=CARTESIAN_POINT('Ctrl Pts',(24.1644456701466,5.14288517641339,0.933446334094952));
#73189=CARTESIAN_POINT('Ctrl Pts',(24.2042009942857,4.48464269382609,2.68487800563082));
#73190=CARTESIAN_POINT('Ctrl Pts',(24.2439563184248,3.24097210138753,3.75756719189555));
#73191=CARTESIAN_POINT('Ctrl Pts',(24.2837116425638,1.99730150894912,4.83025637816016));
#73192=CARTESIAN_POINT('Ctrl Pts',(24.3234669667029,0.168202806659376,5.22420307915372));
#73193=CARTESIAN_POINT('Ctrl Pts',(24.3632222908419,-1.40678365144245,4.75858919445841));
#73194=CARTESIAN_POINT('Ctrl Pts',(24.402977614981,-2.98177010954438,4.29297530976307));
#73195=CARTESIAN_POINT('Ctrl Pts',(24.44273293912,-4.30264432345847,2.96780083937893));
#73196=CARTESIAN_POINT('Ctrl Pts',(24.4824882632591,-4.76313654743402,1.39130930927687));
#73197=CARTESIAN_POINT('Ctrl Pts',(24.4937959381246,-4.89411513859417,0.942905126018314));
#73198=CARTESIAN_POINT('Ctrl Pts',(24.5051036129902,-4.95548762377079,0.474169041233779));
#73199=CARTESIAN_POINT('Ctrl Pts',(24.5164112878558,-4.95147756391153,0.00440602753503367));
#73200=CARTESIAN_POINT('Origin',(10.45,0.,0.));
#73201=CARTESIAN_POINT('',(25.3717887121441,-4.94601914232448,-0.00106424482321954));
#73202=CARTESIAN_POINT('',(25.2664112878558,-4.94652387558086,-0.00193440418662929));
#73203=CARTESIAN_POINT('',(10.45,-4.954,-6.06690024297599E-16));
#73204=CARTESIAN_POINT('Ctrl Pts',(25.3717887121441,-4.94601914232448,-0.00106424482321954));
#73205=CARTESIAN_POINT('Ctrl Pts',(25.3503514953277,-4.94430911377561,0.891990181583246));
#73206=CARTESIAN_POINT('Ctrl Pts',(25.3289142785112,-4.71361814782464,1.78586821550294));
#73207=CARTESIAN_POINT('Ctrl Pts',(25.3074770616947,-4.25922262873376,2.54602303400226));
#73208=CARTESIAN_POINT('Ctrl Pts',(25.2677217375557,-3.41654602087722,3.95573034181289));
#73209=CARTESIAN_POINT('Ctrl Pts',(25.2279664134166,-1.80451115414936,4.90554061694139));
#73210=CARTESIAN_POINT('Ctrl Pts',(25.1882110892775,-0.163027974930276,
4.95949922574628));
#73211=CARTESIAN_POINT('Ctrl Pts',(25.1484557651385,1.47845520428881,5.01345783455117));
#73212=CARTESIAN_POINT('Ctrl Pts',(25.1087004409995,3.14938669599915,4.17156477703208));
#73213=CARTESIAN_POINT('Ctrl Pts',(25.0689451168604,4.08282351654977,2.82024162502009));
#73214=CARTESIAN_POINT('Ctrl Pts',(25.0291897927214,5.01626033710039,1.46891847300811));
#73215=CARTESIAN_POINT('Ctrl Pts',(24.9894344685823,5.21220248649166,-0.391834773496653));
#73216=CARTESIAN_POINT('Ctrl Pts',(24.9496791444432,4.58071422682977,-1.90794860069844));
#73217=CARTESIAN_POINT('Ctrl Pts',(24.9099238203042,3.94922596716785,-3.42406242790032));
#73218=CARTESIAN_POINT('Ctrl Pts',(24.8701684961651,2.49030729845252,-4.595536835799));
#73219=CARTESIAN_POINT('Ctrl Pts',(24.8304131720261,0.873589167397777,-4.88467528679165));
#73220=CARTESIAN_POINT('Ctrl Pts',(24.790657847887,-0.743128963656787,-5.17381373778427));
#73221=CARTESIAN_POINT('Ctrl Pts',(24.750902523748,-2.51764655705084,-4.58061623187108));
#73222=CARTESIAN_POINT('Ctrl Pts',(24.7111471996089,-3.63547551176423,-3.3773552513987));
#73223=CARTESIAN_POINT('Ctrl Pts',(24.6813610371207,-4.47299440012012,-2.47582752256508));
#73224=CARTESIAN_POINT('Ctrl Pts',(24.6515748746324,-4.94187706032252,-1.23183688977808));
#73225=CARTESIAN_POINT('Ctrl Pts',(24.6217887121442,-4.95310191319871,0.00456049067516617));
#73226=CARTESIAN_POINT('Ctrl Pts',(24.5164112878558,-4.95147756391153,0.00440602753503367));
#73227=CARTESIAN_POINT('Ctrl Pts',(24.5448589371293,-4.94138912594368,-1.1774154887533));
#73228=CARTESIAN_POINT('Ctrl Pts',(24.5733065864028,-4.51748403237577,-2.36573660349833));
#73229=CARTESIAN_POINT('Ctrl Pts',(24.6017542356762,-3.74701316495806,-3.2531682565175));
#73230=CARTESIAN_POINT('Ctrl Pts',(24.6415095598153,-2.67028732446968,-4.49334570238973));
#73231=CARTESIAN_POINT('Ctrl Pts',(24.6812648839543,-0.916725409456256,
-5.14589200431422));
#73232=CARTESIAN_POINT('Ctrl Pts',(24.7210202080934,0.708802952698988,-4.9112941001153));
#73233=CARTESIAN_POINT('Ctrl Pts',(24.7607755322324,2.33433131485405,-4.6766961959164));
#73234=CARTESIAN_POINT('Ctrl Pts',(24.8005308563715,3.83182612415081,-3.55495408559414));
#73235=CARTESIAN_POINT('Ctrl Pts',(24.8402861805106,4.51395032174456,-2.06093761584487));
#73236=CARTESIAN_POINT('Ctrl Pts',(24.8800415046496,5.19607451933846,-0.566921146095265));
#73237=CARTESIAN_POINT('Ctrl Pts',(24.9197968287887,5.062828105229,1.29936968308167));
#73238=CARTESIAN_POINT('Ctrl Pts',(24.9595521529278,4.17537002154208,2.68132365573233));
#73239=CARTESIAN_POINT('Ctrl Pts',(24.9993074770668,3.28791193785532,4.06327762838277));
#73240=CARTESIAN_POINT('Ctrl Pts',(25.0390628012058,1.64624218459133,4.96089474450724));
#73241=CARTESIAN_POINT('Ctrl Pts',(25.0788181253449,0.0038728626253081,
4.96217657530616));
#73242=CARTESIAN_POINT('Ctrl Pts',(25.1185734494839,-1.63849645934071,4.96345840610509));
#73243=CARTESIAN_POINT('Ctrl Pts',(25.158328773623,-3.28156535000864,4.0684049515787));
#73244=CARTESIAN_POINT('Ctrl Pts',(25.1980840977621,-4.1711795166362,2.6878379422087));
#73245=CARTESIAN_POINT('Ctrl Pts',(25.2208598277933,-4.68083734310046,1.89691440740134));
#73246=CARTESIAN_POINT('Ctrl Pts',(25.2436355578246,-4.94320253847257,0.946639659339477));
#73247=CARTESIAN_POINT('Ctrl Pts',(25.2664112878558,-4.94652387558086,-0.00193440418662929));
#73248=CARTESIAN_POINT('Origin',(10.45,0.,0.));
#73249=CARTESIAN_POINT('',(26.1217887121441,-4.95701837283973,-0.00414435129742319));
#73250=CARTESIAN_POINT('',(26.0164112878558,-4.95858561828336,-0.00363551008735497));
#73251=CARTESIAN_POINT('',(10.45,-4.954,-6.06690024297599E-16));
#73252=CARTESIAN_POINT('Ctrl Pts',(26.1217887121441,-4.95701837283973,-0.00414435129742319));
#73253=CARTESIAN_POINT('Ctrl Pts',(26.088883440162,-4.94479832228077,1.35895636761934));
#73254=CARTESIAN_POINT('Ctrl Pts',(26.0559781681799,-4.36019767419945,2.73126401776642));
#73255=CARTESIAN_POINT('Ctrl Pts',(26.0230728961977,-3.35982496366235,3.65168274968392));
#73256=CARTESIAN_POINT('Ctrl Pts',(25.9833175720587,-2.15119975038825,4.76370957173509));
#73257=CARTESIAN_POINT('Ctrl Pts',(25.9435622479196,-0.33567761965343,5.21612018511601));
#73258=CARTESIAN_POINT('Ctrl Pts',(25.9038069237805,1.25343260245453,4.80126206344664));
#73259=CARTESIAN_POINT('Ctrl Pts',(25.8640515996415,2.84254282456258,4.38640394177725));
#73260=CARTESIAN_POINT('Ctrl Pts',(25.8242962755024,4.20524113804382,3.10427708505783));
#73261=CARTESIAN_POINT('Ctrl Pts',(25.7845409513634,4.71606090016571,1.54336653997552));
#73262=CARTESIAN_POINT('Ctrl Pts',(25.7447856272243,5.22688066228767,-0.0175440051069695));
#73263=CARTESIAN_POINT('Ctrl Pts',(25.7050303030853,4.88582187304976,-1.85723823855216));
#73264=CARTESIAN_POINT('Ctrl Pts',(25.6652749789462,3.84942754257308,-3.13131254991698));
#73265=CARTESIAN_POINT('Ctrl Pts',(25.6255196548072,2.81303321209658,-4.40538686128159));
#73266=CARTESIAN_POINT('Ctrl Pts',(25.5857643306681,1.08130334038127,-5.11384125056608));
#73267=CARTESIAN_POINT('Ctrl Pts',(25.5460090065291,-0.550913162680595,
-4.93150133103228));
#73268=CARTESIAN_POINT('Ctrl Pts',(25.50625368239,-2.18312966574265,-4.74916141149845));
#73269=CARTESIAN_POINT('Ctrl Pts',(25.4664983582509,-3.71583280015141,-3.6760271831463));
#73270=CARTESIAN_POINT('Ctrl Pts',(25.4267430341119,-4.44552519286334,-2.20465789872378));
#73271=CARTESIAN_POINT('Ctrl Pts',(25.4084249267893,-4.78174641232606,-1.52669334814114));
#73272=CARTESIAN_POINT('Ctrl Pts',(25.3901068194667,-4.94748036216244,-0.764179483516399));
#73273=CARTESIAN_POINT('Ctrl Pts',(25.3717887121441,-4.94601914232448,-0.00106424482321954));
#73274=CARTESIAN_POINT('Ctrl Pts',(25.2664112878558,-4.94652387558086,-0.00193440418662929));
#73275=CARTESIAN_POINT('Ctrl Pts',(25.2833908819636,-4.94899997430159,-0.709108337042042));
#73276=CARTESIAN_POINT('Ctrl Pts',(25.3003704760714,-4.80750232985598,-1.41533704803351));
#73277=CARTESIAN_POINT('Ctrl Pts',(25.3173500701792,-4.5171618476025,-2.05388904426371));
#73278=CARTESIAN_POINT('Ctrl Pts',(25.3571053943183,-3.83737056935426,-3.5489684571522));
#73279=CARTESIAN_POINT('Ctrl Pts',(25.3968607184573,-2.34162857027089,-4.6730467187156));
#73280=CARTESIAN_POINT('Ctrl Pts',(25.4366160425964,-0.716468384594204,
-4.91018170920986));
#73281=CARTESIAN_POINT('Ctrl Pts',(25.4763713667355,0.908691801082482,-5.14731669970413));
#73282=CARTESIAN_POINT('Ctrl Pts',(25.5161266908745,2.66327017335248,-4.49750841912926));
#73283=CARTESIAN_POINT('Ctrl Pts',(25.5558820150136,3.74193055981534,-3.25901320173794));
#73284=CARTESIAN_POINT('Ctrl Pts',(25.5956373391526,4.82059094627832,-2.02051798434648));
#73285=CARTESIAN_POINT('Ctrl Pts',(25.6353926632917,5.22333334693401,-0.193335830138429));
#73286=CARTESIAN_POINT('Ctrl Pts',(25.6751479874307,4.76530251192093,1.38387258570369));
#73287=CARTESIAN_POINT('Ctrl Pts',(25.7149033115698,4.30727167690792,2.96108100154554));
#73288=CARTESIAN_POINT('Ctrl Pts',(25.7546586357088,2.98846760622648,4.28831567902156));
#73289=CARTESIAN_POINT('Ctrl Pts',(25.7944139598479,1.41420986793587,4.75638747507128));
#73290=CARTESIAN_POINT('Ctrl Pts',(25.8341692839869,-0.160047870354837,
5.22445927112102));
#73291=CARTESIAN_POINT('Ctrl Pts',(25.873924608126,-1.98975927625474,4.83336818574436));
#73292=CARTESIAN_POINT('Ctrl Pts',(25.9136799322651,-3.23510277011079,3.76262161669275));
#73293=CARTESIAN_POINT('Ctrl Pts',(25.947923717462,-4.3077962023373,2.84031960293728));
#73294=CARTESIAN_POINT('Ctrl Pts',(25.9821675026589,-4.94691956774523,1.4137491866956));
#73295=CARTESIAN_POINT('Ctrl Pts',(26.0164112878558,-4.95858561828336,-0.00363551008735497));
#73296=CARTESIAN_POINT('Origin',(10.45,0.,0.));
#73297=CARTESIAN_POINT('',(26.8717887121441,-4.9595359561886,0.00319450674940359));
#73298=CARTESIAN_POINT('',(26.7664112878558,-4.95808068667962,0.00382558555664219));
#73299=CARTESIAN_POINT('',(10.45,-4.954,-6.06690024297599E-16));
#73300=CARTESIAN_POINT('Ctrl Pts',(26.8717887121441,-4.9595359561886,0.00319450674940359));
#73301=CARTESIAN_POINT('Ctrl Pts',(26.8671707091353,-4.96096588983627,0.194242562984014));
#73302=CARTESIAN_POINT('Ctrl Pts',(26.8625527061266,-4.9508863525858,0.385138317086643));
#73303=CARTESIAN_POINT('Ctrl Pts',(26.8579347031178,-4.92879366968551,0.574633494025437));
#73304=CARTESIAN_POINT('Ctrl Pts',(26.8181793789788,-4.73860285167671,2.20595382181785));
#73305=CARTESIAN_POINT('Ctrl Pts',(26.7784240548398,-3.65810681917519,3.73347609466237));
#73306=CARTESIAN_POINT('Ctrl Pts',(26.7386687307007,-2.18324382883633,4.45608090979461));
#73307=CARTESIAN_POINT('Ctrl Pts',(26.6989134065617,-0.708380838497551,
5.1786857249268));
#73308=CARTESIAN_POINT('Ctrl Pts',(26.6591580824226,1.16084910967861,5.09637308234685));
#73309=CARTESIAN_POINT('Ctrl Pts',(26.6194027582835,2.56648576974824,4.24692376720699));
#73310=CARTESIAN_POINT('Ctrl Pts',(26.5796474341444,3.97212242981795,3.39747445206709));
#73311=CARTESIAN_POINT('Ctrl Pts',(26.5398921100054,4.91416580178117,1.78088846436712));
#73312=CARTESIAN_POINT('Ctrl Pts',(26.5001367858664,4.96022619281914,0.139164675326781));
#73313=CARTESIAN_POINT('Ctrl Pts',(26.4603814617273,5.0062865838571,-1.50255911371347));
#73314=CARTESIAN_POINT('Ctrl Pts',(26.4206261375882,4.15636399397013,-3.169420704094));
#73315=CARTESIAN_POINT('Ctrl Pts',(26.3808708134492,2.80056548032569,-4.09634516138423));
#73316=CARTESIAN_POINT('Ctrl Pts',(26.3411154893101,1.44476696668117,-5.02326961867452));
#73317=CARTESIAN_POINT('Ctrl Pts',(26.3013601651711,-0.416907470720896,
-5.21025694287418));
#73318=CARTESIAN_POINT('Ctrl Pts',(26.2616048410321,-1.9299654994954,-4.57148158276344));
#73319=CARTESIAN_POINT('Ctrl Pts',(26.221849516893,-3.44302352826974,-3.93270622265277));
#73320=CARTESIAN_POINT('Ctrl Pts',(26.1820941927539,-4.60746514841668,-2.46816817823187));
#73321=CARTESIAN_POINT('Ctrl Pts',(26.1423388686149,-4.88882181058346,-0.850077640660699));
#73322=CARTESIAN_POINT('Ctrl Pts',(26.135488816458,-4.93730104832772,-0.57127210160384));
#73323=CARTESIAN_POINT('Ctrl Pts',(26.128638764301,-4.95956228081091,-0.287907725894975));
#73324=CARTESIAN_POINT('Ctrl Pts',(26.1217887121441,-4.95701837283973,-0.00414435129742319));
#73325=CARTESIAN_POINT('Ctrl Pts',(26.0164112878558,-4.95858561828336,-0.00363551008735497));
#73326=CARTESIAN_POINT('Ctrl Pts',(26.021922826798,-4.96046326970163,-0.231763648006996));
#73327=CARTESIAN_POINT('Ctrl Pts',(26.0274343657401,-4.94608669044165,-0.459653830611601));
#73328=CARTESIAN_POINT('Ctrl Pts',(26.0329459046822,-4.9146474874091,-0.685165263338358));
#73329=CARTESIAN_POINT('Ctrl Pts',(26.0727012288213,-4.6878731290391,-2.31180352159104));
#73330=CARTESIAN_POINT('Ctrl Pts',(26.1124565529603,-3.57334883048701,-3.81467798536976));
#73331=CARTESIAN_POINT('Ctrl Pts',(26.1522118770994,-2.08263152578818,-4.50398238133491));
#73332=CARTESIAN_POINT('Ctrl Pts',(26.1919672012384,-0.591914221089427,
-5.19328677730003));
#73333=CARTESIAN_POINT('Ctrl Pts',(26.2317225253775,1.27499608975594,-5.06902110545165));
#73334=CARTESIAN_POINT('Ctrl Pts',(26.2714778495165,2.66120385411115,-4.1882222255327));
#73335=CARTESIAN_POINT('Ctrl Pts',(26.3112331736556,4.0474116184666,-3.3074233456136));
#73336=CARTESIAN_POINT('Ctrl Pts',(26.3509884977947,4.95291683633171,-1.67009125762339));
#73337=CARTESIAN_POINT('Ctrl Pts',(26.3907438219337,4.96210050899447,-0.0277471119028885));
#73338=CARTESIAN_POINT('Ctrl Pts',(26.4304991460728,4.97128418165723,1.61459703381733));
#73339=CARTESIAN_POINT('Ctrl Pts',(26.4702544702118,4.08414630911817,3.26195323726807));
#73340=CARTESIAN_POINT('Ctrl Pts',(26.5100097943509,2.70787543875327,4.1581993665262));
#73341=CARTESIAN_POINT('Ctrl Pts',(26.5497651184899,1.33160456838828,5.05444549578438));
#73342=CARTESIAN_POINT('Ctrl Pts',(26.589520442629,-0.53379929980252,5.19958155084983));
#73343=CARTESIAN_POINT('Ctrl Pts',(26.629275766768,-2.03213205722407,4.52699134807925));
#73344=CARTESIAN_POINT('Ctrl Pts',(26.6690310909071,-3.53046481464571,3.85440114530863));
#73345=CARTESIAN_POINT('Ctrl Pts',(26.7087864150461,-4.66172646129797,2.36408468470192));
#73346=CARTESIAN_POINT('Ctrl Pts',(26.7485417391852,-4.90667776632238,0.740084225652552));
#73347=CARTESIAN_POINT('Ctrl Pts',(26.7544982554087,-4.94337867252687,0.496761216952243));
#73348=CARTESIAN_POINT('Ctrl Pts',(26.7604547716323,-4.96018293254122,0.250437156483314));
#73349=CARTESIAN_POINT('Ctrl Pts',(26.7664112878558,-4.95808068667962,0.00382558555664219));
#73350=CARTESIAN_POINT('Origin',(10.45,0.,0.));
#73351=CARTESIAN_POINT('',(27.6217887121441,-4.94702083875962,0.0024746876873416));
#73352=CARTESIAN_POINT('',(27.5164112878558,-4.94632349813665,0.00165195671278186));
#73353=CARTESIAN_POINT('',(10.45,-4.954,-6.06690024297599E-16));
#73354=CARTESIAN_POINT('Ctrl Pts',(27.6217887121441,-4.94702083875962,0.0024746876873416));
#73355=CARTESIAN_POINT('Ctrl Pts',(27.6057026539697,-4.95003929944518,0.672266001052461));
#73356=CARTESIAN_POINT('Ctrl Pts',(27.5896165957953,-4.82355113413133,1.34096495790584));
#73357=CARTESIAN_POINT('Ctrl Pts',(27.5735305376208,-4.56214311665504,1.95193772286538));
#73358=CARTESIAN_POINT('Ctrl Pts',(27.5337752134818,-3.91609544266134,3.46190492848642));
#73359=CARTESIAN_POINT('Ctrl Pts',(27.4940198893428,-2.44597192410526,4.61928680603406));
#73360=CARTESIAN_POINT('Ctrl Pts',(27.4542645652037,-0.826546436067746,
4.89285516644541));
#73361=CARTESIAN_POINT('Ctrl Pts',(27.4145092410646,0.79287905196968,5.16642352685675));
#73362=CARTESIAN_POINT('Ctrl Pts',(27.3747539169256,2.56160650948843,4.5561783701319));
#73363=CARTESIAN_POINT('Ctrl Pts',(27.3349985927865,3.66780545734341,3.34221690167914));
#73364=CARTESIAN_POINT('Ctrl Pts',(27.2952432686474,4.77400440519833,2.12825543322646));
#73365=CARTESIAN_POINT('Ctrl Pts',(27.2554879445084,5.2176748433895,0.31057765304573));
#73366=CARTESIAN_POINT('Ctrl Pts',(27.2157326203694,4.7951759097319,-1.27651818847781));
#73367=CARTESIAN_POINT('Ctrl Pts',(27.1759772962303,4.37267697607426,-2.86361403000153));
#73368=CARTESIAN_POINT('Ctrl Pts',(27.1362219720912,3.0840086705678,-4.22012793286816));
#73369=CARTESIAN_POINT('Ctrl Pts',(27.0964666479522,1.52065850784982,-4.72343184488691));
#73370=CARTESIAN_POINT('Ctrl Pts',(27.0567113238131,-0.0426916548680703,
-5.22673575690563));
#73371=CARTESIAN_POINT('Ctrl Pts',(27.0169559996741,-1.88072367479736,-4.87682967807652));
#73372=CARTESIAN_POINT('Ctrl Pts',(26.977200675535,-3.14979688300393,-3.83431744729183));
#73373=CARTESIAN_POINT('Ctrl Pts',(26.9420633544047,-4.27145376344193,-2.91290408119225));
#73374=CARTESIAN_POINT('Ctrl Pts',(26.9069260332744,-4.94865592045064,-1.45044614495815));
#73375=CARTESIAN_POINT('Ctrl Pts',(26.8717887121441,-4.9595359561886,0.00319450674940359));
#73376=CARTESIAN_POINT('Ctrl Pts',(26.7664112878558,-4.95808068667962,0.00382558555664219));
#73377=CARTESIAN_POINT('Ctrl Pts',(26.8002100957713,-4.94615200195839,-1.3955120142548));
#73378=CARTESIAN_POINT('Ctrl Pts',(26.8340089036869,-4.32548676253793,-2.8041066458325));
#73379=CARTESIAN_POINT('Ctrl Pts',(26.8678077116024,-3.27697886146211,-3.72620730839182));
#73380=CARTESIAN_POINT('Ctrl Pts',(26.9075630357414,-2.04368768818079,-4.81081392589505));
#73381=CARTESIAN_POINT('Ctrl Pts',(26.9473183598805,-0.218464378221529,
-5.22234270340963));
#73382=CARTESIAN_POINT('Ctrl Pts',(26.9870736840195,1.36092948566179,-4.77190552071585));
#73383=CARTESIAN_POINT('Ctrl Pts',(27.0268290081586,2.9403233495451,-4.32146833802208));
#73384=CARTESIAN_POINT('Ctrl Pts',(27.0665843322976,4.27388776735247,-3.00906519511995));
#73385=CARTESIAN_POINT('Ctrl Pts',(27.1063396564367,4.74952830040862,-1.4370776900362));
#73386=CARTESIAN_POINT('Ctrl Pts',(27.1460949805758,5.22516883346478,0.134909815047647));
#73387=CARTESIAN_POINT('Ctrl Pts',(27.1858503047148,4.84288548176958,1.96648168231316));
#73388=CARTESIAN_POINT('Ctrl Pts',(27.2256056288539,3.77814297012091,3.2169623965642));
#73389=CARTESIAN_POINT('Ctrl Pts',(27.2653609529929,2.71340045847224,4.46744311081523));
#73390=CARTESIAN_POINT('Ctrl Pts',(27.305116277132,0.966198786870095,5.13683267205178));
#73391=CARTESIAN_POINT('Ctrl Pts',(27.344871601271,-0.661511713564407,4.9178871089523));
#73392=CARTESIAN_POINT('Ctrl Pts',(27.3846269254101,-2.28922221399882,4.69894154585283));
#73393=CARTESIAN_POINT('Ctrl Pts',(27.4243822495492,-3.7974415432656,3.59166085841746));
#73394=CARTESIAN_POINT('Ctrl Pts',(27.4641375736882,-4.49391018137497,2.10427722634554));
#73395=CARTESIAN_POINT('Ctrl Pts',(27.4815621450774,-4.79916910625851,1.45236398349203));
#73396=CARTESIAN_POINT('Ctrl Pts',(27.4989867164666,-4.94848848074252,0.72743191486131));
#73397=CARTESIAN_POINT('Ctrl Pts',(27.5164112878558,-4.94632349813665,0.00165195671278186));
#73398=CARTESIAN_POINT('Origin',(10.45,0.,0.));
#73399=CARTESIAN_POINT('',(28.3717887121441,-4.95045814526779,-0.00419805499302928));
#73400=CARTESIAN_POINT('',(28.2664112878558,-4.95200672834798,-0.00447880390354169));
#73401=CARTESIAN_POINT('',(10.45,-4.954,-6.06690024297599E-16));
#73402=CARTESIAN_POINT('Ctrl Pts',(28.3717887121441,-4.95045814526779,-0.00419805499302928));
#73403=CARTESIAN_POINT('Ctrl Pts',(28.344234598804,-4.9412870202373,1.14109909159698));
#73404=CARTESIAN_POINT('Ctrl Pts',(28.3166804854639,-4.54589945079795,2.29210988530882));
#73405=CARTESIAN_POINT('Ctrl Pts',(28.2891263721238,-3.81911859406739,3.16820830363733));
#73406=CARTESIAN_POINT('Ctrl Pts',(28.2493710479848,-2.77051259536383,4.43225103179432));
#73407=CARTESIAN_POINT('Ctrl Pts',(28.2096157238457,-1.03204586664494,5.12400922901711));
#73408=CARTESIAN_POINT('Ctrl Pts',(28.1698603997067,0.598340523580153,4.92597191512799));
#73409=CARTESIAN_POINT('Ctrl Pts',(28.1301050755676,2.22872691380516,4.72793460123887));
#73410=CARTESIAN_POINT('Ctrl Pts',(28.0903497514285,3.75103296553638,3.64010177623793));
#73411=CARTESIAN_POINT('Ctrl Pts',(28.0505944272895,4.46653347601348,2.16177922055856));
#73412=CARTESIAN_POINT('Ctrl Pts',(28.0108391031504,5.18203398649057,0.683456664879198));
#73413=CARTESIAN_POINT('Ctrl Pts',(27.9710837790114,5.09072895571354,-1.18535562147859));
#73414=CARTESIAN_POINT('Ctrl Pts',(27.9313284548724,4.23452659660065,-2.58688909570347));
#73415=CARTESIAN_POINT('Ctrl Pts',(27.8915731307333,3.37832423748771,-3.98842256992843));
#73416=CARTESIAN_POINT('Ctrl Pts',(27.8518178065942,1.75722455003883,-4.92267723202043));
#73417=CARTESIAN_POINT('Ctrl Pts',(27.8120624824552,0.115298154297456,-4.96083833907168));
#73418=CARTESIAN_POINT('Ctrl Pts',(27.7723071583161,-1.52662824144383,-4.99899944612293));
#73419=CARTESIAN_POINT('Ctrl Pts',(27.7325518341771,-3.18938134547761,-4.14106699813353));
#73420=CARTESIAN_POINT('Ctrl Pts',(27.692796510038,-4.10977198277882,-2.78082450729169));
#73421=CARTESIAN_POINT('Ctrl Pts',(27.6691272440734,-4.65774816603,-1.97097219217775));
#73422=CARTESIAN_POINT('Ctrl Pts',(27.6454579781088,-4.94257943067843,-0.983066242534685));
#73423=CARTESIAN_POINT('Ctrl Pts',(27.6217887121441,-4.94702083875962,0.0024746876873416));
#73424=CARTESIAN_POINT('Ctrl Pts',(27.5164112878558,-4.94632349813665,0.00165195671278186));
#73425=CARTESIAN_POINT('Ctrl Pts',(27.5387420406057,-4.94354892823764,-0.928483564797916));
#73426=CARTESIAN_POINT('Ctrl Pts',(27.5610727933555,-4.69197439851418,-1.86001167153667));
#73427=CARTESIAN_POINT('Ctrl Pts',(27.5834035461053,-4.20097747928438,-2.64102245013698));
#73428=CARTESIAN_POINT('Ctrl Pts',(27.6231588702444,-3.32685819213247,-4.03145191783911));
#73429=CARTESIAN_POINT('Ctrl Pts',(27.6629141943835,-1.69390167087667,-4.94482427653488));
#73430=CARTESIAN_POINT('Ctrl Pts',(27.7026695185225,-0.0516207188824688,
-4.96190957847522));
#73431=CARTESIAN_POINT('Ctrl Pts',(27.7424248426616,1.59066023311174,-4.97899488041556));
#73432=CARTESIAN_POINT('Ctrl Pts',(27.7821801668006,3.24226561584435,-4.09979312560047));
#73433=CARTESIAN_POINT('Ctrl Pts',(27.8219354909397,4.14512296115597,-2.72785025257614));
#73434=CARTESIAN_POINT('Ctrl Pts',(27.8616908150787,5.04798030646763,-1.35590737955174));
#73435=CARTESIAN_POINT('Ctrl Pts',(27.9014461392178,5.20208961435818,0.508776611681977));
#73436=CARTESIAN_POINT('Ctrl Pts',(27.9412014633569,4.53671605638716,2.01032802977551));
#73437=CARTESIAN_POINT('Ctrl Pts',(27.9809567874959,3.87134249841618,3.51187944786895));
#73438=CARTESIAN_POINT('Ctrl Pts',(28.020712111635,2.38648607458373,4.65029829282225));
#73439=CARTESIAN_POINT('Ctrl Pts',(28.060467435774,0.76368293501706,4.90306024216977));
#73440=CARTESIAN_POINT('Ctrl Pts',(28.1002227599131,-0.859120204549604,
5.15582219151729));
#73441=CARTESIAN_POINT('Ctrl Pts',(28.1399780840521,-2.61987005985048,4.52292724525903));
#73442=CARTESIAN_POINT('Ctrl Pts',(28.1797334081912,-3.71039780159122,3.29486866468593));
#73443=CARTESIAN_POINT('Ctrl Pts',(28.2086260347461,-4.50295103747106,2.40236335314786));
#73444=CARTESIAN_POINT('Ctrl Pts',(28.2375186613009,-4.9415051357895,1.19550342842609));
#73445=CARTESIAN_POINT('Ctrl Pts',(28.2664112878558,-4.95200672834798,-0.00447880390354169));
#73446=CARTESIAN_POINT('Origin',(10.45,0.,0.));
#73447=CARTESIAN_POINT('',(29.1217887121441,-4.9620979667096,-0.000568056217270518));
#73448=CARTESIAN_POINT('',(29.0164112878558,-4.96212320436852,0.000469511818217842));
#73449=CARTESIAN_POINT('',(10.45,-4.954,-6.06690024297599E-16));
#73450=CARTESIAN_POINT('Ctrl Pts',(29.1217887121441,-4.9620979667096,-0.000568056217270518));
#73451=CARTESIAN_POINT('Ctrl Pts',(29.0827665436384,-4.95948881461475,1.61158375926093));
#73452=CARTESIAN_POINT('Ctrl Pts',(29.0437443751326,-4.10050759025402,3.2261208355131));
#73453=CARTESIAN_POINT('Ctrl Pts',(29.0047222066268,-2.76101916288883,4.12310366992494));
#73454=CARTESIAN_POINT('Ctrl Pts',(28.9649668824878,-1.39636418215534,5.03693918175563));
#73455=CARTESIAN_POINT('Ctrl Pts',(28.9252115583487,0.467023332900544,5.20600407764322));
#73456=CARTESIAN_POINT('Ctrl Pts',(28.8854562342097,1.9738647621892,4.55269904467401));
#73457=CARTESIAN_POINT('Ctrl Pts',(28.8457009100706,3.48070619147776,3.89939401170483));
#73458=CARTESIAN_POINT('Ctrl Pts',(28.8059455859316,4.63100153499924,2.42371904987888));
#73459=CARTESIAN_POINT('Ctrl Pts',(28.7661902617925,4.89677526101191,0.802996098327756));
#73460=CARTESIAN_POINT('Ctrl Pts',(28.7264349376535,5.1625489870246,-0.817726853223465));
#73461=CARTESIAN_POINT('Ctrl Pts',(28.6866796135144,4.54380109552853,-2.58349779449976));
#73462=CARTESIAN_POINT('Ctrl Pts',(28.6469242893753,3.32453147304543,-3.68384326152976));
#73463=CARTESIAN_POINT('Ctrl Pts',(28.6071689652363,2.10526185056232,-4.78418872855976));
#73464=CARTESIAN_POINT('Ctrl Pts',(28.5674136410972,0.285470497092144,-5.21910872134327));
#73465=CARTESIAN_POINT('Ctrl Pts',(28.5276583169582,-1.29957422527118,-4.7889787558308));
#73466=CARTESIAN_POINT('Ctrl Pts',(28.4879029928191,-2.88461894763441,-4.35884879031834));
#73467=CARTESIAN_POINT('Ctrl Pts',(28.4481476686801,-4.23491703889091,-3.06366886650999));
#73468=CARTESIAN_POINT('Ctrl Pts',(28.408392344541,-4.73069345017502,-1.49791527506032));
#73469=CARTESIAN_POINT('Ctrl Pts',(28.396191133742,-4.88285099471092,-1.0173736107117));
#73470=CARTESIAN_POINT('Ctrl Pts',(28.3839899229431,-4.9545192024457,-0.511345998405597));
#73471=CARTESIAN_POINT('Ctrl Pts',(28.3717887121441,-4.95045814526779,-0.00419805499302928));
#73472=CARTESIAN_POINT('Ctrl Pts',(28.2664112878558,-4.95200672834798,-0.00447880390354169));
#73473=CARTESIAN_POINT('Ctrl Pts',(28.27727398544,-4.95595498912304,-0.455633498040154));
#73474=CARTESIAN_POINT('Ctrl Pts',(28.2881366830242,-4.89939725962342,-0.905816018007978));
#73475=CARTESIAN_POINT('Ctrl Pts',(28.2989993806083,-4.77839806799436,-1.33795488241193));
#73476=CARTESIAN_POINT('Ctrl Pts',(28.3387547047474,-4.33556496447621,-2.9194976340483));
#73477=CARTESIAN_POINT('Ctrl Pts',(28.3785100288864,-3.02959312925948,-4.25936092243318));
#73478=CARTESIAN_POINT('Ctrl Pts',(28.4182653530255,-1.4599122462263,-4.74255918222436));
#73479=CARTESIAN_POINT('Ctrl Pts',(28.4580206771646,0.109768636807045,-5.22575744201559));
#73480=CARTESIAN_POINT('Ctrl Pts',(28.4977760013036,1.94315856765701,-4.85229067321291));
#73481=CARTESIAN_POINT('Ctrl Pts',(28.5375313254427,3.19874755579615,-3.7935768659499));
#73482=CARTESIAN_POINT('Ctrl Pts',(28.5772866495817,4.4543365439353,-2.7348630586869));
#73483=CARTESIAN_POINT('Ctrl Pts',(28.6170419737208,5.13212458936373,-0.990902212963525));
#73484=CARTESIAN_POINT('Ctrl Pts',(28.6567972978598,4.92101288975318,0.637842850916404));
#73485=CARTESIAN_POINT('Ctrl Pts',(28.6965526219989,4.70990119014265,2.26658791479624));
#73486=CARTESIAN_POINT('Ctrl Pts',(28.7363079461379,3.60988974549346,3.78011719683246));
#73487=CARTESIAN_POINT('Ctrl Pts',(28.776063270277,2.12587421645596,4.48373395501895));
#73488=CARTESIAN_POINT('Ctrl Pts',(28.815818594416,0.641858687418374,5.18735071320548));
#73489=CARTESIAN_POINT('Ctrl Pts',(28.8555739185551,-1.22616092600755,5.08105494754191));
#73490=CARTESIAN_POINT('Ctrl Pts',(28.8953292426942,-2.62077991097366,4.21363548753556));
#73491=CARTESIAN_POINT('Ctrl Pts',(28.9350845668332,-4.0153988959397,3.34621602752926));
#73492=CARTESIAN_POINT('Ctrl Pts',(28.9748398909723,-4.93661725244607,1.71767287318022));
#73493=CARTESIAN_POINT('Ctrl Pts',(29.0145952151113,-4.96160378816815,0.0754931309297103));
#73494=CARTESIAN_POINT('Ctrl Pts',(29.0152005726928,-4.96198426019705,0.0504875252986975));
#73495=CARTESIAN_POINT('Ctrl Pts',(29.0158059302743,-4.96215692830693,0.0254787578334992));
#73496=CARTESIAN_POINT('Ctrl Pts',(29.0164112878558,-4.96212320436852,0.000469511818217842));
#73497=CARTESIAN_POINT('Origin',(10.45,0.,0.));
#73498=CARTESIAN_POINT('',(29.8717887121441,-4.95216086653923,0.0044958085145208));
#73499=CARTESIAN_POINT('',(29.7664112878558,-4.95060002325747,0.00423272256442855));
#73500=CARTESIAN_POINT('',(10.45,-4.954,-6.06690024297599E-16));
#73501=CARTESIAN_POINT('Ctrl Pts',(29.8717887121441,-4.95216086653923,0.0044958085145208));
#73502=CARTESIAN_POINT('Ctrl Pts',(29.8610538126118,-4.95608712658793,0.450307475266639));
#73503=CARTESIAN_POINT('Ctrl Pts',(29.8503189130794,-4.90087411902633,0.895163507848311));
#73504=CARTESIAN_POINT('Ctrl Pts',(29.839584013547,-4.78267074519706,1.32260017912596));
#73505=CARTESIAN_POINT('Ctrl Pts',(29.7998286894079,-4.34491970460876,2.90555709123284));
#73506=CARTESIAN_POINT('Ctrl Pts',(29.7600733652689,-3.04325814371637,4.24960811376942));
#73507=CARTESIAN_POINT('Ctrl Pts',(29.7203180411298,-1.47513736807399,4.73784554793628));
#73508=CARTESIAN_POINT('Ctrl Pts',(29.6805627169907,0.0929834075686548,
5.22608298210322));
#73509=CARTESIAN_POINT('Ctrl Pts',(29.6408073928517,1.9275633979613,4.85850682790008));
#73510=CARTESIAN_POINT('Ctrl Pts',(29.6010520687127,3.18654638562424,3.80383133472726));
#73511=CARTESIAN_POINT('Ctrl Pts',(29.5612967445736,4.44552937328696,2.74915584155461));
#73512=CARTESIAN_POINT('Ctrl Pts',(29.5215414204345,5.12891535822014,1.0073810094123));
#73513=CARTESIAN_POINT('Ctrl Pts',(29.4817860962955,4.92303613267859,-0.622033702566684));
#73514=CARTESIAN_POINT('Ctrl Pts',(29.4420307721564,4.71715690713703,-2.25144841454585));
#73515=CARTESIAN_POINT('Ctrl Pts',(29.4022754480174,3.62201247112069,-3.76850300636179));
#73516=CARTESIAN_POINT('Ctrl Pts',(29.3625201238783,2.1402645707595,-4.47688264956091));
#73517=CARTESIAN_POINT('Ctrl Pts',(29.3227647997393,0.658516670398306,-5.18526229276003));
#73518=CARTESIAN_POINT('Ctrl Pts',(29.2830094756002,-1.20983469430763,-5.08496698734232));
#73519=CARTESIAN_POINT('Ctrl Pts',(29.2432541514611,-2.60723253956581,-4.22203140388807));
#73520=CARTESIAN_POINT('Ctrl Pts',(29.2034988273221,-4.00463038482382,-3.35909582043393));
#73521=CARTESIAN_POINT('Ctrl Pts',(29.163743503183,-4.93107471063413,-1.73351995894351));
#73522=CARTESIAN_POINT('Ctrl Pts',(29.123988179044,-4.96133565033377,-0.0914289643114814));
#73523=CARTESIAN_POINT('Ctrl Pts',(29.1232550234107,-4.96189371340808,-0.0611460200982296));
#73524=CARTESIAN_POINT('Ctrl Pts',(29.1225218677774,-4.96214698793598,-0.0308574591512815));
#73525=CARTESIAN_POINT('Ctrl Pts',(29.1217887121441,-4.9620979667096,-0.000568056217270518));
#73526=CARTESIAN_POINT('Ctrl Pts',(29.0164112878558,-4.96212320436852,0.000469511818217842));
#73527=CARTESIAN_POINT('Ctrl Pts',(29.0555612544134,-4.95994219416689,-1.61694005742288));
#73528=CARTESIAN_POINT('Ctrl Pts',(29.0947112209709,-4.09452073852457,-3.2363511756137));
#73529=CARTESIAN_POINT('Ctrl Pts',(29.1338611875285,-2.7477619212938,-4.13195060322239));
#73530=CARTESIAN_POINT('Ctrl Pts',(29.1736165116676,-1.38017880375977,-5.04139826497171));
#73531=CARTESIAN_POINT('Ctrl Pts',(29.2133718358066,0.483742146245983,-5.20447725831835));
#73532=CARTESIAN_POINT('Ctrl Pts',(29.2531271599456,1.98847746664373,-4.54633574741596));
#73533=CARTESIAN_POINT('Ctrl Pts',(29.2928824840847,3.49321278704156,-3.88819423651354));
#73534=CARTESIAN_POINT('Ctrl Pts',(29.3326378082238,4.63876247783135,-2.408832221362));
#73535=CARTESIAN_POINT('Ctrl Pts',(29.3723931323628,4.89932922049166,-0.787263966417092));
#73536=CARTESIAN_POINT('Ctrl Pts',(29.4121484565019,5.15989596315194,0.834304288527634));
#73537=CARTESIAN_POINT('Ctrl Pts',(29.4519037806409,4.53547975768294,2.5980787832657));
#73538=CARTESIAN_POINT('Ctrl Pts',(29.49165910478,3.31268219729058,3.69450240537696));
#73539=CARTESIAN_POINT('Ctrl Pts',(29.531414428919,2.08988463689801,4.79092602748841));
#73540=CARTESIAN_POINT('Ctrl Pts',(29.5711697530581,0.268705721581839,5.21999877697279));
#73541=CARTESIAN_POINT('Ctrl Pts',(29.6109250771972,-1.31494930777667,4.78478000346513));
#73542=CARTESIAN_POINT('Ctrl Pts',(29.6506804013362,-2.89860433713499,4.34956122995753));
#73543=CARTESIAN_POINT('Ctrl Pts',(29.6904357254753,-4.24473548053571,3.05005093345812));
#73544=CARTESIAN_POINT('Ctrl Pts',(29.7301910496143,-4.73548028184195,1.48271300792442));
#73545=CARTESIAN_POINT('Ctrl Pts',(29.7422644623615,-4.88451603159391,1.00672348704749));
#73546=CARTESIAN_POINT('Ctrl Pts',(29.7543378751087,-4.95465999137664,0.506032378106856));
#73547=CARTESIAN_POINT('Ctrl Pts',(29.7664112878558,-4.95060002325747,0.00423272256442855));
#73548=CARTESIAN_POINT('Origin',(10.45,0.,0.));
#73549=CARTESIAN_POINT('',(30.6217887121441,-4.94627182265837,-0.00156944476627563));
#73550=CARTESIAN_POINT('',(30.5164112878558,-4.94694225394907,-0.00239988756266602));
#73551=CARTESIAN_POINT('',(10.45,-4.954,-6.06690024297599E-16));
#73552=CARTESIAN_POINT('Ctrl Pts',(30.6217887121441,-4.94627182265837,-0.00156944476627563));
#73553=CARTESIAN_POINT('Ctrl Pts',(30.5995857574461,-4.94365246685677,0.923267018668746));
#73554=CARTESIAN_POINT('Ctrl Pts',(30.577382802748,-4.69512873603121,1.84941055057953));
#73555=CARTESIAN_POINT('Ctrl Pts',(30.55517984805,-4.20943847831249,2.62751563041785));
#73556=CARTESIAN_POINT('Ctrl Pts',(30.5154245239109,-3.33978964601186,4.02074549932014));
#73557=CARTESIAN_POINT('Ctrl Pts',(30.4756691997719,-1.70977523980265,4.93935804323487));
#73558=CARTESIAN_POINT('Ctrl Pts',(30.4359138756328,-0.0675576579001141,
4.96171811509349));
#73559=CARTESIAN_POINT('Ctrl Pts',(30.3961585514937,1.57465992400252,4.98407818695211));
#73560=CARTESIAN_POINT('Ctrl Pts',(30.3564032273547,3.22908068159848,4.11018578675453));
#73561=CARTESIAN_POINT('Ctrl Pts',(30.3166479032156,4.13633991421696,2.74114990557676));
#73562=CARTESIAN_POINT('Ctrl Pts',(30.2768925790766,5.04359914683538,1.37211402439907));
#73563=CARTESIAN_POINT('Ctrl Pts',(30.2371372549375,5.2036968544764,-0.492065337758739));
#73564=CARTESIAN_POINT('Ctrl Pts',(30.1973819307985,4.54314958543481,-1.99574610989259));
#73565=CARTESIAN_POINT('Ctrl Pts',(30.1576266066594,3.88260231639321,-3.49942688202644));
#73566=CARTESIAN_POINT('Ctrl Pts',(30.1178712825204,2.40141007066901,-4.64260906413632));
#73567=CARTESIAN_POINT('Ctrl Pts',(30.0781159583813,0.779427172590541,-4.90058200353951));
#73568=CARTESIAN_POINT('Ctrl Pts',(30.0383606342423,-0.842555725488016,
-5.15855494294273));
#73569=CARTESIAN_POINT('Ctrl Pts',(29.9986053101032,-2.60532927592085,-4.53131863963915));
#73570=CARTESIAN_POINT('Ctrl Pts',(29.9588499859641,-3.6997957909952,-3.30676908714867));
#73571=CARTESIAN_POINT('Ctrl Pts',(29.9298295613575,-4.49872986267182,-2.41287754595835));
#73572=CARTESIAN_POINT('Ctrl Pts',(29.9008091367508,-4.9415467258679,-1.20069887679431));
#73573=CARTESIAN_POINT('Ctrl Pts',(29.8717887121441,-4.95216086653923,0.0044958085145208));
#73574=CARTESIAN_POINT('Ctrl Pts',(29.7664112878558,-4.95060002325747,0.00423272256442855));
#73575=CARTESIAN_POINT('Ctrl Pts',(29.7940931992477,-4.94129133149963,-1.14629313885498));
#73576=CARTESIAN_POINT('Ctrl Pts',(29.8217751106396,-4.54189791215148,-2.30264655026279));
#73577=CARTESIAN_POINT('Ctrl Pts',(29.8494570220315,-3.80892294691085,-3.18045866944975));
#73578=CARTESIAN_POINT('Ctrl Pts',(29.8892123461705,-2.75626235146179,-4.44112686672221));
#73579=CARTESIAN_POINT('Ctrl Pts',(29.9289676703096,-1.01558270135191,-5.12729770669915));
#73580=CARTESIAN_POINT('Ctrl Pts',(29.9687229944486,0.614159223288633,-4.92402475745519));
#73581=CARTESIAN_POINT('Ctrl Pts',(30.0084783185877,2.24390114792926,-4.72075180821122));
#73582=CARTESIAN_POINT('Ctrl Pts',(30.0482336427267,3.76270534710054,-3.62803506974627));
#73583=CARTESIAN_POINT('Ctrl Pts',(30.0879889668658,4.47345393782982,-2.1474219961845));
#73584=CARTESIAN_POINT('Ctrl Pts',(30.1277442910049,5.18420252855906,-0.666808922622812));
#73585=CARTESIAN_POINT('Ctrl Pts',(30.1674996151439,5.0868955108464,1.20170048603564));
#73586=CARTESIAN_POINT('Ctrl Pts',(30.207254939283,4.22619595727435,2.60047670520234));
#73587=CARTESIAN_POINT('Ctrl Pts',(30.247010263422,3.36549640370231,3.99925292436904));
#73588=CARTESIAN_POINT('Ctrl Pts',(30.2867655875611,1.74140431427089,4.92829595404398));
#73589=CARTESIAN_POINT('Ctrl Pts',(30.3265209117001,0.0993637954387848,
4.96118314515178));
#73590=CARTESIAN_POINT('Ctrl Pts',(30.3662762358392,-1.54267672339342,4.99407033625959));
#73591=CARTESIAN_POINT('Ctrl Pts',(30.4060315599783,-3.20266567162631,4.13080168880015));
#73592=CARTESIAN_POINT('Ctrl Pts',(30.4457868841173,-4.11868259764308,2.76760998398513));
#73593=CARTESIAN_POINT('Ctrl Pts',(30.4693283520301,-4.66111014762382,1.96038392123949));
#73594=CARTESIAN_POINT('Ctrl Pts',(30.492869819943,-4.94266232326109,0.97785877353352));
#73595=CARTESIAN_POINT('Ctrl Pts',(30.5164112878558,-4.94694225394907,-0.00239988756266602));
#73596=CARTESIAN_POINT('Origin',(10.45,0.,0.));
#73597=CARTESIAN_POINT('',(31.3717887121441,-4.95793233061953,-0.00387638962322745));
#73598=CARTESIAN_POINT('',(31.2664112878558,-4.9594059793847,-0.00326224302469192));
#73599=CARTESIAN_POINT('',(10.45,-4.954,-6.06690024297599E-16));
#73600=CARTESIAN_POINT('Ctrl Pts',(31.3717887121441,-4.95793233061953,-0.00387638962322745));
#73601=CARTESIAN_POINT('Ctrl Pts',(31.3381177022804,-4.94594313351065,1.39027847680682));
#73602=CARTESIAN_POINT('Ctrl Pts',(31.3044466924167,-4.33051759246278,2.7936983782844));
#73603=CARTESIAN_POINT('Ctrl Pts',(31.270775682553,-3.28893015515837,3.71566267646537));
#73604=CARTESIAN_POINT('Ctrl Pts',(31.2310203584139,-2.05912901890516,4.80422490454117));
#73605=CARTESIAN_POINT('Ctrl Pts',(31.1912650342748,-0.2352369420535,5.22161400632066));
#73606=CARTESIAN_POINT('Ctrl Pts',(31.1515097101358,1.34559551703039,4.77625202385045));
#73607=CARTESIAN_POINT('Ctrl Pts',(31.1117543859967,2.92642797611456,4.33089004138017));
#73608=CARTESIAN_POINT('Ctrl Pts',(31.0719990618577,4.26420081743087,3.02277697465984));
#73609=CARTESIAN_POINT('Ctrl Pts',(31.0322437377186,4.74488797261209,1.45232531415967));
#73610=CARTESIAN_POINT('Ctrl Pts',(30.9924884135796,5.22557512779325,-0.118126346340324));
#73611=CARTESIAN_POINT('Ctrl Pts',(30.9527330894405,4.84917659683952,-1.9509166006201));
#73612=CARTESIAN_POINT('Ctrl Pts',(30.9129777653015,3.78845602314589,-3.20481070446875));
#73613=CARTESIAN_POINT('Ctrl Pts',(30.8732224411624,2.72773544945226,-4.4587048083174));
#73614=CARTESIAN_POINT('Ctrl Pts',(30.8334671170233,0.982692833018733,-5.13370276173493));
#73615=CARTESIAN_POINT('Ctrl Pts',(30.7937117928843,-0.645712482528409,
-4.91998639029569));
#73616=CARTESIAN_POINT('Ctrl Pts',(30.7539564687452,-2.27411779807564,-4.70627001885644));
#73617=CARTESIAN_POINT('Ctrl Pts',(30.7142011446062,-3.78588581273648,-3.60383932256033));
#73618=CARTESIAN_POINT('Ctrl Pts',(30.6744458204671,-4.48712819087084,-2.11870037746728));
#73619=CARTESIAN_POINT('Ctrl Pts',(30.6568934510261,-4.79673364763043,-1.46299682077366));
#73620=CARTESIAN_POINT('Ctrl Pts',(30.6393410815851,-4.94834253357735,-0.73269156339755));
#73621=CARTESIAN_POINT('Ctrl Pts',(30.6217887121441,-4.94627182265837,-0.00156944476627563));
#73622=CARTESIAN_POINT('Ctrl Pts',(30.5164112878558,-4.94694225394907,-0.00239988756266602));
#73623=CARTESIAN_POINT('Ctrl Pts',(30.532625144082,-4.94988999625171,-0.67753930768575));
#73624=CARTESIAN_POINT('Ctrl Pts',(30.5488390003082,-4.82131163479957,-1.35160360341962));
#73625=CARTESIAN_POINT('Ctrl Pts',(30.5650528565345,-4.55585019848591,-1.96658087363273));
#73626=CARTESIAN_POINT('Ctrl Pts',(30.6048081806735,-3.90495596951134,-3.47446526426518));
#73627=CARTESIAN_POINT('Ctrl Pts',(30.6445635048126,-2.43112260776153,-4.62711928335961));
#73628=CARTESIAN_POINT('Ctrl Pts',(30.6843188289516,-0.810826773992338,
-4.89548478765477));
#73629=CARTESIAN_POINT('Ctrl Pts',(30.7240741530907,0.809469059776941,-5.16385029194995));
#73630=CARTESIAN_POINT('Ctrl Pts',(30.7638294772297,2.57622736556561,-4.54792728144577));
#73631=CARTESIAN_POINT('Ctrl Pts',(30.8035848013688,3.6785214877009,-3.33041904692261));
#73632=CARTESIAN_POINT('Ctrl Pts',(30.8433401255079,4.78081560983612,-2.11291081239953));
#73633=CARTESIAN_POINT('Ctrl Pts',(30.8830954496469,5.21864554831803,-0.29381735385755));
#73634=CARTESIAN_POINT('Ctrl Pts',(30.9228507737859,4.79105117939728,1.29191329429574));
#73635=CARTESIAN_POINT('Ctrl Pts',(30.962606097925,4.36345681047652,2.87764394244903));
#73636=CARTESIAN_POINT('Ctrl Pts',(31.0023614220641,3.07043813415308,4.23001178021363));
#73637=CARTESIAN_POINT('Ctrl Pts',(31.0421167462031,1.50547944733267,4.72829176312557));
#73638=CARTESIAN_POINT('Ctrl Pts',(31.0818720703422,-0.0594792394878271,
5.22657174603753));
#73639=CARTESIAN_POINT('Ctrl Pts',(31.1216273944812,-1.89637793680533,4.87076387409672));
#73640=CARTESIAN_POINT('Ctrl Pts',(31.1613827186203,-3.16209616088146,3.82418085776822));
#73641=CARTESIAN_POINT('Ctrl Pts',(31.1963922416988,-4.27671897773194,2.90253393230071));
#73642=CARTESIAN_POINT('Ctrl Pts',(31.2314017647773,-4.94839134831731,1.44519089534153));
#73643=CARTESIAN_POINT('Ctrl Pts',(31.2664112878558,-4.9594059793847,-0.00326224302469192));
#73644=CARTESIAN_POINT('Origin',(10.45,0.,0.));
#73645=CARTESIAN_POINT('',(32.1217887121441,-4.95872700410626,0.0035772032441482));
#73646=CARTESIAN_POINT('',(32.0164112878558,-4.95717366314325,0.00410403508777372));
#73647=CARTESIAN_POINT('',(10.45,-4.954,-6.06690024297599E-16));
#73648=CARTESIAN_POINT('Ctrl Pts',(32.1217887121441,-4.95872700410626,0.0035772032441482));
#73649=CARTESIAN_POINT('Ctrl Pts',(32.1164049712538,-4.96054007908593,0.226399070643231));
#73650=CARTESIAN_POINT('Ctrl Pts',(32.1110212303634,-4.94682528332486,0.448996398812498));
#73651=CARTESIAN_POINT('Ctrl Pts',(32.1056374894731,-4.9168227585756,0.669376315342024));
#73652=CARTESIAN_POINT('Ctrl Pts',(32.065882165334,-4.69527418840998,2.29673453963713));
#73653=CARTESIAN_POINT('Ctrl Pts',(32.026126841195,-3.58558275123426,3.80318098227819));
#73654=CARTESIAN_POINT('Ctrl Pts',(31.986371517056,-2.09708713985614,4.49726986277651));
#73655=CARTESIAN_POINT('Ctrl Pts',(31.9466161929169,-0.608591528478095,
5.19135874327479));
#73656=CARTESIAN_POINT('Ctrl Pts',(31.9068608687778,1.25870825710231,5.07309006163041));
#73657=CARTESIAN_POINT('Ctrl Pts',(31.8671055446388,2.64773789874118,4.19674811137832));
#73658=CARTESIAN_POINT('Ctrl Pts',(31.8273502204997,4.03676754038028,3.32040616112608));
#73659=CARTESIAN_POINT('Ctrl Pts',(31.7875948963607,4.94752703807765,1.68599094226582));
#73660=CARTESIAN_POINT('Ctrl Pts',(31.7478395722216,4.96198572449744,0.0436847876433137));
#73661=CARTESIAN_POINT('Ctrl Pts',(31.7080842480826,4.97644441091723,-1.59862136697901));
#73662=CARTESIAN_POINT('Ctrl Pts',(31.6683289239435,4.09460228605965,-3.24881845736358));
#73663=CARTESIAN_POINT('Ctrl Pts',(31.6285735998044,2.72121719529554,-4.14948040925797));
#73664=CARTESIAN_POINT('Ctrl Pts',(31.5888182756654,1.34783210453152,-5.05014236115231));
#73665=CARTESIAN_POINT('Ctrl Pts',(31.5490629515264,-0.517095952138985,
-5.20126917455656));
#73666=CARTESIAN_POINT('Ctrl Pts',(31.5093076273873,-2.01758125945948,-4.53349495999121));
#73667=CARTESIAN_POINT('Ctrl Pts',(31.4695523032482,-3.51806656678022,-3.86572074542575));
#73668=CARTESIAN_POINT('Ctrl Pts',(31.4297969791092,-4.65410912475082,-2.37904550289038));
#73669=CARTESIAN_POINT('Ctrl Pts',(31.3900416549701,-4.90427530590864,-0.755840204436467));
#73670=CARTESIAN_POINT('Ctrl Pts',(31.3839573406948,-4.94256174175555,-0.507418354456599));
#73671=CARTESIAN_POINT('Ctrl Pts',(31.3778730264194,-4.96009876528884,-0.255798633422028));
#73672=CARTESIAN_POINT('Ctrl Pts',(31.3717887121441,-4.95793233061953,-0.00387638962322745));
#73673=CARTESIAN_POINT('Ctrl Pts',(31.2664112878558,-4.9594059793847,-0.00326224302469192));
#73674=CARTESIAN_POINT('Ctrl Pts',(31.2711570889163,-4.96089909449181,-0.199610831515726));
#73675=CARTESIAN_POINT('Ctrl Pts',(31.2759028899769,-4.95025208354887,-0.395796060852635));
#73676=CARTESIAN_POINT('Ctrl Pts',(31.2806486910374,-4.92692264233869,-0.590461378916891));
#73677=CARTESIAN_POINT('Ctrl Pts',(31.3204040151765,-4.7314931488852,-2.22116243855789));
#73678=CARTESIAN_POINT('Ctrl Pts',(31.3601593393156,-3.64609641114327,-3.74520639712367));
#73679=CARTESIAN_POINT('Ctrl Pts',(31.3999146634546,-2.16892006673788,-4.46307036777193));
#73680=CARTESIAN_POINT('Ctrl Pts',(31.4396699875937,-0.691743722332493,
-5.18093433842019));
#73681=CARTESIAN_POINT('Ctrl Pts',(31.4794253117327,1.17721222873627,-5.09261832115089));
#73682=CARTESIAN_POINT('Ctrl Pts',(31.5191806358718,2.58011330280755,-4.23865859774737));
#73683=CARTESIAN_POINT('Ctrl Pts',(31.5589359600108,3.98301437687875,-3.38469887434389));
#73684=CARTESIAN_POINT('Ctrl Pts',(31.5986912841499,4.91986057395253,-1.76509544480606));
#73685=CARTESIAN_POINT('Ctrl Pts',(31.638446608289,4.96064765916329,-0.123232159844304));
#73686=CARTESIAN_POINT('Ctrl Pts',(31.678201932428,5.00143474437405,1.51863112511736));
#73687=CARTESIAN_POINT('Ctrl Pts',(31.717957256567,4.14616271772212,3.18275426550314));
#73688=CARTESIAN_POINT('Ctrl Pts',(31.7577125807061,2.7873939812014,4.10531925154967));
#73689=CARTESIAN_POINT('Ctrl Pts',(31.7974679048452,1.42862524468052,5.02788423759631));
#73690=CARTESIAN_POINT('Ctrl Pts',(31.8372232289842,-0.433640201709166,
5.20889106930347));
#73691=CARTESIAN_POINT('Ctrl Pts',(31.8769785531233,-1.94463875761121,4.56525918935371));
#73692=CARTESIAN_POINT('Ctrl Pts',(31.9167338772624,-3.45563731351326,3.92162730940394));
#73693=CARTESIAN_POINT('Ctrl Pts',(31.9564892014014,-4.61536897892758,2.45335671779726));
#73694=CARTESIAN_POINT('Ctrl Pts',(31.9962445255404,-4.89152703265136,0.834370812302948));
#73695=CARTESIAN_POINT('Ctrl Pts',(32.0029667796456,-4.93822278096961,0.560615412616595));
#73696=CARTESIAN_POINT('Ctrl Pts',(32.0096890337507,-4.95965569987392,0.282550813091737));
#73697=CARTESIAN_POINT('Ctrl Pts',(32.0164112878558,-4.95717366314325,0.00410403508777372));
#73698=CARTESIAN_POINT('Origin',(10.45,0.,0.));
#73699=CARTESIAN_POINT('',(32.8717887121441,-4.94658723177794,0.00201400887214764));
#73700=CARTESIAN_POINT('',(32.7664112878558,-4.94605458361617,0.00114969562655201));
#73701=CARTESIAN_POINT('',(10.45,-4.954,-6.06690024297599E-16));
#73702=CARTESIAN_POINT('Ctrl Pts',(32.8717887121441,-4.94658723177794,0.00201400887214764));
#73703=CARTESIAN_POINT('Ctrl Pts',(32.8549369160881,-4.94914770039353,0.70384286307377));
#73704=CARTESIAN_POINT('Ctrl Pts',(32.8380851200321,-4.80985358206998,1.4047015626472));
#73705=CARTESIAN_POINT('Ctrl Pts',(32.8212333239761,-4.52373539183098,2.03936970544422));
#73706=CARTESIAN_POINT('Ctrl Pts',(32.7814779998371,-3.84874968958156,3.53662481426251));
#73707=CARTESIAN_POINT('Ctrl Pts',(32.741722675698,-2.35662586424462,4.66550145063581));
#73708=CARTESIAN_POINT('Ctrl Pts',(32.7019673515589,-0.732235739864097,
4.90785508262556));
#73709=CARTESIAN_POINT('Ctrl Pts',(32.6622120274199,0.892154384516242,5.15020871461528));
#73710=CARTESIAN_POINT('Ctrl Pts',(32.6224567032808,2.64881080794023,4.5060393422217));
#73711=CARTESIAN_POINT('Ctrl Pts',(32.5827013791418,3.73144355064897,3.27101509001533));
#73712=CARTESIAN_POINT('Ctrl Pts',(32.5429460550027,4.81407629335783,2.03599083780882));
#73713=CARTESIAN_POINT('Ctrl Pts',(32.5031907308637,5.22268535535135,0.210111705789586));
#73714=CARTESIAN_POINT('Ctrl Pts',(32.4634354067246,4.76972274037325,-1.36855970668223));
#73715=CARTESIAN_POINT('Ctrl Pts',(32.4236800825855,4.31676012539514,-2.94723111915404));
#73716=CARTESIAN_POINT('Ctrl Pts',(32.3839247584465,3.00222583344523,-4.27869481207827));
#73717=CARTESIAN_POINT('Ctrl Pts',(32.3441694343074,1.42947964137902,-4.75182056118187));
#73718=CARTESIAN_POINT('Ctrl Pts',(32.3044141101684,-0.143266550687003,
-5.22494631028541));
#73719=CARTESIAN_POINT('Ctrl Pts',(32.2646587860293,-1.97422464286937,-4.83973411556855));
#73720=CARTESIAN_POINT('Ctrl Pts',(32.2249034618903,-3.22300083738286,-3.77299301523568));
#73721=CARTESIAN_POINT('Ctrl Pts',(32.1905318786416,-4.3026654070543,-2.85071200435332));
#73722=CARTESIAN_POINT('Ctrl Pts',(32.1561602953928,-4.9471517335148,-1.41899132688034));
#73723=CARTESIAN_POINT('Ctrl Pts',(32.1217887121441,-4.95872700410626,0.0035772032441482));
#73724=CARTESIAN_POINT('Ctrl Pts',(32.0164112878558,-4.95717366314325,0.00410403508777372));
#73725=CARTESIAN_POINT('Ctrl Pts',(32.0494443578897,-4.944976966638,-1.36417984330865));
#73726=CARTESIAN_POINT('Ctrl Pts',(32.0824774279237,-4.35529939531296,-2.74169228837345));
#73727=CARTESIAN_POINT('Ctrl Pts',(32.1155104979576,-3.34807880300487,-3.66245541849339));
#73728=CARTESIAN_POINT('Ctrl Pts',(32.1552658220967,-2.13588807760102,-4.77059452441411));
#73729=CARTESIAN_POINT('Ctrl Pts',(32.1950211462357,-0.31892218476007,-5.21717151687348));
#73730=CARTESIAN_POINT('Ctrl Pts',(32.2347764703748,1.26884737521433,-4.79721145062356));
#73731=CARTESIAN_POINT('Ctrl Pts',(32.2745317945138,2.85661693518855,-4.3772513843737));
#73732=CARTESIAN_POINT('Ctrl Pts',(32.3142871186529,4.2151901622961,-3.09075425941461));
#73733=CARTESIAN_POINT('Ctrl Pts',(32.3540424427919,4.72099379247748,-1.52821103744581));
#73734=CARTESIAN_POINT('Ctrl Pts',(32.393797766931,5.22679742265886,0.0343321845229944));
#73735=CARTESIAN_POINT('Ctrl Pts',(32.43355309107,4.87983145591409,1.87292150350164));
#73736=CARTESIAN_POINT('Ctrl Pts',(32.4733084152091,3.83935024532743,3.14366045515198));
#73737=CARTESIAN_POINT('Ctrl Pts',(32.5130637393482,2.79886903474065,4.41439940680247));
#73738=CARTESIAN_POINT('Ctrl Pts',(32.5528190634872,1.06487258031201,5.11728799112456));
#73739=CARTESIAN_POINT('Ctrl Pts',(32.5925743876263,-0.566749866366629,
4.92970647732251));
#73740=CARTESIAN_POINT('Ctrl Pts',(32.6323297117653,-2.198372313045,4.7421249635205));
#73741=CARTESIAN_POINT('Ctrl Pts',(32.6720850359044,-3.72762075197333,3.66407335159448));
#73742=CARTESIAN_POINT('Ctrl Pts',(32.7118403600434,-4.45258348520756,2.19036793047174));
#73743=CARTESIAN_POINT('Ctrl Pts',(32.7300306693142,-4.78429493802344,1.51606435064163));
#73744=CARTESIAN_POINT('Ctrl Pts',(32.748220978585,-4.94762274111771,0.758927479174985));
#73745=CARTESIAN_POINT('Ctrl Pts',(32.7664112878558,-4.94605458361617,0.00114969562655201));
#73746=CARTESIAN_POINT('Origin',(10.45,0.,0.));
#73747=CARTESIAN_POINT('',(33.6217887121441,-4.9513279518383,-0.00438127959876189));
#73748=CARTESIAN_POINT('',(33.5164112878558,-4.95294315282494,-0.00455417533769269));
#73749=CARTESIAN_POINT('',(10.45,-4.954,-6.06690024297599E-16));
#73750=CARTESIAN_POINT('Ctrl Pts',(33.6217887121441,-4.9513279518383,-0.00438127959876189));
#73751=CARTESIAN_POINT('Ctrl Pts',(33.5934688609224,-4.94136392358352,1.17222104474813));
#73752=CARTESIAN_POINT('Ctrl Pts',(33.5651490097007,-4.5216107651878,2.35521240637459));
#73753=CARTESIAN_POINT('Ctrl Pts',(33.5368291584791,-3.75744266893846,3.24111636329651));
#73754=CARTESIAN_POINT('Ctrl Pts',(33.49707383434,-2.6847057352125,4.48474574142488));
#73755=CARTESIAN_POINT('Ctrl Pts',(33.457318510201,-0.933248809232052,5.14292095116953));
#73756=CARTESIAN_POINT('Ctrl Pts',(33.4175631860619,0.693024653229394,4.9135453107511));
#73757=CARTESIAN_POINT('Ctrl Pts',(33.3778078619229,2.31929811569066,4.68416967033269));
#73758=CARTESIAN_POINT('Ctrl Pts',(33.3380525377838,3.82038811463306,3.56724317975119));
#73759=CARTESIAN_POINT('Ctrl Pts',(33.2982972136447,4.50730743051541,2.07542535823586));
#73760=CARTESIAN_POINT('Ctrl Pts',(33.2585418895057,5.19422674639788,0.583607536720267));
#73761=CARTESIAN_POINT('Ctrl Pts',(33.2187865653666,5.06697537922034,-1.28310161572913));
#73762=CARTESIAN_POINT('Ctrl Pts',(33.1790312412276,4.18396059684558,-2.6678988764253));
#73763=CARTESIAN_POINT('Ctrl Pts',(33.1392759170885,3.30094581447098,-4.05269613712124));
#73764=CARTESIAN_POINT('Ctrl Pts',(33.0995205929495,1.66216761689915,-4.95558150606392));
#73765=CARTESIAN_POINT('Ctrl Pts',(33.0597652688104,0.0198109061580776,
-4.96213847235091));
#73766=CARTESIAN_POINT('Ctrl Pts',(33.0200099446714,-1.62254580458299,-4.9686954386379));
#73767=CARTESIAN_POINT('Ctrl Pts',(32.9802546205323,-3.26848102849344,-4.07892400226939));
#73768=CARTESIAN_POINT('Ctrl Pts',(32.9404992963932,-4.16252485086781,-2.70122149345361));
#73769=CARTESIAN_POINT('Ctrl Pts',(32.9175957683102,-4.67759442297352,-1.90751024133607));
#73770=CARTESIAN_POINT('Ctrl Pts',(32.8946922402272,-4.94310726058389,-0.951852084585827));
#73771=CARTESIAN_POINT('Ctrl Pts',(32.8717887121441,-4.94658723177794,0.00201400887214764));
#73772=CARTESIAN_POINT('Ctrl Pts',(32.7664112878558,-4.94605458361617,0.00114969562655201));
#73773=CARTESIAN_POINT('Ctrl Pts',(32.7879763027241,-4.94419549813648,-0.897212664561465));
#73774=CARTESIAN_POINT('Ctrl Pts',(32.8095413175923,-4.71058127270834,-1.7964758028442));
#73775=CARTESIAN_POINT('Ctrl Pts',(32.8311063324606,-4.25102312046575,-2.55969017516725));
#73776=CARTESIAN_POINT('Ctrl Pts',(32.8708616565997,-3.40382299494956,-3.96668362936352));
#73777=CARTESIAN_POINT('Ctrl Pts',(32.9106169807387,-1.78874571637721,-4.91131130743615));
#73778=CARTESIAN_POINT('Ctrl Pts',(32.9503723048778,-0.147097671634971,
-4.95999734259825));
#73779=CARTESIAN_POINT('Ctrl Pts',(32.9901276290168,1.49455037310708,-5.00868337776036));
#73780=CARTESIAN_POINT('Ctrl Pts',(33.0298829531559,3.16276918401907,-4.16142777001195));
#73781=CARTESIAN_POINT('Ctrl Pts',(33.0696382772949,4.09186087428128,-2.80711345497616));
#73782=CARTESIAN_POINT('Ctrl Pts',(33.109393601434,5.02095256454354,-1.45279913994028));
#73783=CARTESIAN_POINT('Ctrl Pts',(33.149148925573,5.21091713415614,0.408573882383032));
#73784=CARTESIAN_POINT('Ctrl Pts',(33.1889042497121,4.57456250221729,1.92265162650169));
#73785=CARTESIAN_POINT('Ctrl Pts',(33.2286595738511,3.93820787027841,3.43672937062043));
#73786=CARTESIAN_POINT('Ctrl Pts',(33.2684148979902,2.47553403678802,4.60351183653435));
#73787=CARTESIAN_POINT('Ctrl Pts',(33.3081702221293,0.857895536345488,4.88745604709655));
#73788=CARTESIAN_POINT('Ctrl Pts',(33.3479255462683,-0.759742964096859,
5.17140025765872));
#73789=CARTESIAN_POINT('Ctrl Pts',(33.3876808704074,-2.53234613149147,4.57250621286921));
#73790=CARTESIAN_POINT('Ctrl Pts',(33.4274361945464,-3.64630456965725,3.36566105674335));
#73791=CARTESIAN_POINT('Ctrl Pts',(33.4570945589829,-4.47734257630615,2.46532747290505));
#73792=CARTESIAN_POINT('Ctrl Pts',(33.4867529234193,-4.94181218791447,1.22663900174132));
#73793=CARTESIAN_POINT('Ctrl Pts',(33.5164112878558,-4.95294315282494,-0.00455417533769269));
#73794=CARTESIAN_POINT('Origin',(10.45,0.,0.));
#73795=CARTESIAN_POINT('',(34.3717887121441,-4.96217785588676,2.53259700289598E-5));
#73796=CARTESIAN_POINT('',(34.2664112878558,-4.96190593350399,0.00105408447129014));
#73797=CARTESIAN_POINT('',(10.45,-4.954,-6.06690024297599E-16));
#73798=CARTESIAN_POINT('Ctrl Pts',(34.3717887121441,-4.96217785588676,2.53259700289598E-5));
#73799=CARTESIAN_POINT('Ctrl Pts',(34.3320008057567,-4.96230199391906,1.64374130780069));
#73800=CARTESIAN_POINT('Ctrl Pts',(34.2922128993694,-4.06428393345358,3.287340649827));
#73801=CARTESIAN_POINT('Ctrl Pts',(34.2524249929821,-2.68116326291599,4.17547293709044));
#73802=CARTESIAN_POINT('Ctrl Pts',(34.212669668843,-1.29917522752317,5.06287793434716));
#73803=CARTESIAN_POINT('Ctrl Pts',(34.172914344704,0.567120692079285,5.19605267203163));
#73804=CARTESIAN_POINT('Ctrl Pts',(34.1331590205649,2.06111094347969,4.5138711068721));
#73805=CARTESIAN_POINT('Ctrl Pts',(34.0934036964258,3.55510119487992,3.83168954171264));
#73806=CARTESIAN_POINT('Ctrl Pts',(34.0536483722868,4.67678577807796,2.33415167370907));
#73807=CARTESIAN_POINT('Ctrl Pts',(34.0138930481477,4.91132125082459,0.708614325277302));
#73808=CARTESIAN_POINT('Ctrl Pts',(33.9741377240087,5.14585672357124,-0.916923023154561));
#73809=CARTESIAN_POINT('Ctrl Pts',(33.9343823998696,4.49324308586658,-2.67045985201484));
#73810=CARTESIAN_POINT('Ctrl Pts',(33.8946270757306,3.25302430642285,-3.74713804824555));
#73811=CARTESIAN_POINT('Ctrl Pts',(33.8548717515915,2.01280552697904,-4.82381624447632));
#73812=CARTESIAN_POINT('Ctrl Pts',(33.8151164274525,0.184981605796054,-5.22363580807742));
#73813=CARTESIAN_POINT('Ctrl Pts',(33.7753611033134,-1.39149221649886,-4.76308304590743));
#73814=CARTESIAN_POINT('Ctrl Pts',(33.7356057791743,-2.96796603879368,-4.30253028373747));
#73815=CARTESIAN_POINT('Ctrl Pts',(33.6958504550353,-4.29308976220046,-2.98160519579652));
#73816=CARTESIAN_POINT('Ctrl Pts',(33.6560951308962,-4.75864315316813,-1.4066008785701));
#73817=CARTESIAN_POINT('Ctrl Pts',(33.6446596579789,-4.89255787551782,-0.953556673688374));
#73818=CARTESIAN_POINT('Ctrl Pts',(33.6332241850615,-4.95535139724285,-0.479489849529769));
#73819=CARTESIAN_POINT('Ctrl Pts',(33.6217887121441,-4.9513279518383,-0.00438127959876189));
#73820=CARTESIAN_POINT('Ctrl Pts',(33.5164112878558,-4.95294315282494,-0.00455417533769269));
#73821=CARTESIAN_POINT('Ctrl Pts',(33.5265082475584,-4.95673260333198,-0.42370432509382));
#73822=CARTESIAN_POINT('Ctrl Pts',(33.536605207261,-4.90797969150976,-0.84198576343423));
#73823=CARTESIAN_POINT('Ctrl Pts',(33.5467021669636,-4.80326067454432,-1.24575208446876));
#73824=CARTESIAN_POINT('Ctrl Pts',(33.5864574911026,-4.39094463232837,-2.83552380209275));
#73825=CARTESIAN_POINT('Ctrl Pts',(33.6262128152417,-3.11099883895928,-4.20027096987823));
#73826=CARTESIAN_POINT('Ctrl Pts',(33.6659681393807,-1.55090725206635,-4.71358653883326));
#73827=CARTESIAN_POINT('Ctrl Pts',(33.7057234635198,0.00918433482640424,
-5.22690210778824));
#73828=CARTESIAN_POINT('Ctrl Pts',(33.7454787876589,1.84942171524284,-4.88878607791293));
#73829=CARTESIAN_POINT('Ctrl Pts',(33.7852341117979,3.12515197901683,-3.85443075844271));
#73830=CARTESIAN_POINT('Ctrl Pts',(33.824989435937,4.40088224279089,-2.82007543897243));
#73831=CARTESIAN_POINT('Ctrl Pts',(33.864744760076,5.11210538992238,-1.0894808299069));
#73832=CARTESIAN_POINT('Ctrl Pts',(33.9045000842151,4.93237619796575,0.543025234518007));
#73833=CARTESIAN_POINT('Ctrl Pts',(33.9442554083541,4.7526470060091,2.17553129894301));
#73834=CARTESIAN_POINT('Ctrl Pts',(33.9840107324932,3.68196547496439,3.7099488187275));
#73835=CARTESIAN_POINT('Ctrl Pts',(34.0237660566323,2.21176509090388,4.44199353289049));
#73836=CARTESIAN_POINT('Ctrl Pts',(34.0635213807713,0.741564706843371,5.17403824705348));
#73837=CARTESIAN_POINT('Ctrl Pts',(34.1032767049103,-1.12815453023284,5.1037101555949));
#73838=CARTESIAN_POINT('Ctrl Pts',(34.1430320290494,-2.53920779504284,4.26328923921134));
#73839=CARTESIAN_POINT('Ctrl Pts',(34.1827873531884,-3.95026105985269,3.42286832282788));
#73840=CARTESIAN_POINT('Ctrl Pts',(34.2225426773275,-4.90264835239638,1.8123545815197));
#73841=CARTESIAN_POINT('Ctrl Pts',(34.2622980014666,-4.95923221051056,0.170959778364143));
#73842=CARTESIAN_POINT('Ctrl Pts',(34.2636690969297,-4.96118369431365,0.114350782802527));
#73843=CARTESIAN_POINT('Ctrl Pts',(34.2650401923928,-4.96206966815802,0.0577050558803606));
#73844=CARTESIAN_POINT('Ctrl Pts',(34.2664112878558,-4.96190593350399,0.00105408447129014));
#73845=CARTESIAN_POINT('Origin',(10.45,0.,0.));
#73846=CARTESIAN_POINT('',(35.1217887121441,-4.95125214780166,0.00436800828097772));
#73847=CARTESIAN_POINT('',(35.0164112878558,-4.94977286428982,0.00400141439014362));
#73848=CARTESIAN_POINT('',(10.45,-4.954,-6.06690024297599E-16));
#73849=CARTESIAN_POINT('Ctrl Pts',(35.1217887121441,-4.95125214780166,0.00436800828097772));
#73850=CARTESIAN_POINT('Ctrl Pts',(35.1102880747301,-4.95528165247632,0.482202489736174));
#73851=CARTESIAN_POINT('Ctrl Pts',(35.0987874373162,-4.89175694914764,0.958987841215879));
#73852=CARTESIAN_POINT('Ctrl Pts',(35.0872867999022,-4.75633309420263,1.41439251562917));
#73853=CARTESIAN_POINT('Ctrl Pts',(35.0475314757632,-4.28820084590116,2.98863225505063));
#73854=CARTESIAN_POINT('Ctrl Pts',(35.0077761516241,-2.9609155390429,4.30738533457894));
#73855=CARTESIAN_POINT('Ctrl Pts',(34.9680208274851,-1.38368955531006,4.76535559064072));
#73856=CARTESIAN_POINT('Ctrl Pts',(34.928265503346,0.193536428422955,5.22332584670255));
#73857=CARTESIAN_POINT('Ctrl Pts',(34.8885101792069,2.02070308903071,4.82051327929763));
#73858=CARTESIAN_POINT('Ctrl Pts',(34.8487548550679,3.25915686285117,3.74180534421805));
#73859=CARTESIAN_POINT('Ctrl Pts',(34.8089995309288,4.49761063667156,2.66309740913853));
#73860=CARTESIAN_POINT('Ctrl Pts',(34.7692442067898,5.14735152370474,0.908494106384621));
#73861=CARTESIAN_POINT('Ctrl Pts',(34.7294888826507,4.91015412269713,-0.716656948771265));
#73862=CARTESIAN_POINT('Ctrl Pts',(34.6897335585117,4.67295672168951,-2.34180800392724));
#73863=CARTESIAN_POINT('Ctrl Pts',(34.6499782343726,3.54882103264079,-3.83750681148506));
#73864=CARTESIAN_POINT('Ctrl Pts',(34.6102229102336,2.05371553403593,-4.51724066173508));
#73865=CARTESIAN_POINT('Ctrl Pts',(34.5704675860945,0.558610035431147,-5.19697451198506));
#73866=CARTESIAN_POINT('Ctrl Pts',(34.5307122619555,-1.30746527272985,-5.06074340492735));
#73867=CARTESIAN_POINT('Ctrl Pts',(34.4909569378164,-2.68799809677426,-4.17107623072434));
#73868=CARTESIAN_POINT('Ctrl Pts',(34.4512341959257,-4.06739947832071,-3.28213820053907));
#73869=CARTESIAN_POINT('Ctrl Pts',(34.4115114540349,-4.9620539211673,-1.64099858346418));
#73870=CARTESIAN_POINT('Ctrl Pts',(34.3717887121441,-4.96217785588676,2.53259700289598E-5));
#73871=CARTESIAN_POINT('Ctrl Pts',(34.2664112878558,-4.96190593350399,0.00105408447129014));
#73872=CARTESIAN_POINT('Ctrl Pts',(34.3047955165318,-4.95732213276104,-1.58490684956072));
#73873=CARTESIAN_POINT('Ctrl Pts',(34.3431797452078,-4.13004313544497,-3.17497808106077));
#73874=CARTESIAN_POINT('Ctrl Pts',(34.3815639738838,-2.82676794883698,-4.07830777737638));
#73875=CARTESIAN_POINT('Ctrl Pts',(34.4213192980228,-1.4769394053648,-5.01390466495807));
#73876=CARTESIAN_POINT('Ctrl Pts',(34.4610746221618,0.383498105263837,-5.21282257511845));
#73877=CARTESIAN_POINT('Ctrl Pts',(34.5008299463009,1.90061998926887,-4.58375992172047));
#73878=CARTESIAN_POINT('Ctrl Pts',(34.5405852704399,3.41774187327381,-3.95469726832253));
#73879=CARTESIAN_POINT('Ctrl Pts',(34.580340594579,4.59154813065502,-2.49765405136622));
#73880=CARTESIAN_POINT('Ctrl Pts',(34.6200959187181,4.88327192522793,-0.881400401562105));
#73881=CARTESIAN_POINT('Ctrl Pts',(34.6598512428571,5.17499571980086,0.7348532482421));
#73882=CARTESIAN_POINT('Ctrl Pts',(34.6996065669962,4.58463705156541,2.51031733089426));
#73883=CARTESIAN_POINT('Ctrl Pts',(34.7393618911352,3.38316540113682,3.63006931505732));
#73884=CARTESIAN_POINT('Ctrl Pts',(34.7791172152743,2.18169375070823,4.74982129922038));
#73885=CARTESIAN_POINT('Ctrl Pts',(34.8188725394133,0.369109118086691,5.2138611848944));
#73886=CARTESIAN_POINT('Ctrl Pts',(34.8586278635524,-1.22262795667244,4.80919871112959));
#73887=CARTESIAN_POINT('Ctrl Pts',(34.8983831876914,-2.81436503143139,4.40453623736482));
#73888=CARTESIAN_POINT('Ctrl Pts',(34.9381385118305,-4.18525454832788,3.13117140416126));
#73889=CARTESIAN_POINT('Ctrl Pts',(34.9778938359695,-4.70607017366559,1.57356756581696));
#73890=CARTESIAN_POINT('Ctrl Pts',(34.9907329865983,-4.87426978990138,1.07053279667574));
#73891=CARTESIAN_POINT('Ctrl Pts',(35.003572137227,-4.95380717245401,0.537852057524207));
#73892=CARTESIAN_POINT('Ctrl Pts',(35.0164112878558,-4.94977286428982,0.00400141439014362));
#73893=CARTESIAN_POINT('Origin',(10.45,0.,0.));
#73894=CARTESIAN_POINT('',(35.8717887121441,-4.94662056565563,-0.00205432018779872));
#73895=CARTESIAN_POINT('',(35.7664112878558,-4.94744996620173,-0.002834044534147));
#73896=CARTESIAN_POINT('',(10.45,-4.954,-6.06690024297599E-16));
#73897=CARTESIAN_POINT('Ctrl Pts',(35.8717887121441,-4.94662056565563,-0.00205432018779872));
#73898=CARTESIAN_POINT('Ctrl Pts',(35.8488200195645,-4.94305946801648,0.954509582032164));
#73899=CARTESIAN_POINT('Ctrl Pts',(35.8258513269848,-4.67593326216678,1.91291262543561));
#73900=CARTESIAN_POINT('Ctrl Pts',(35.8028826344052,-4.15809531370436,2.70803509441322));
#73901=CARTESIAN_POINT('Ctrl Pts',(35.7631273102661,-3.26179634408548,4.08427152471256));
#73902=CARTESIAN_POINT('Ctrl Pts',(35.7233719861271,-1.6144060892818,4.97134611834161));
#73903=CARTESIAN_POINT('Ctrl Pts',(35.6836166619881,0.0279376812127906,
4.96209937198498));
#73904=CARTESIAN_POINT('Ctrl Pts',(35.643861337849,1.67028145170757,4.95285262562834));
#73905=CARTESIAN_POINT('Ctrl Pts',(35.6041060137099,3.30757873789314,4.0472845392858));
#73906=CARTESIAN_POINT('Ctrl Pts',(35.5643506895709,4.18832436752257,2.66104296796643));
#73907=CARTESIAN_POINT('Ctrl Pts',(35.5245953654318,5.06906999715185,1.2748013966473));
#73908=CARTESIAN_POINT('Ctrl Pts',(35.4848400412928,5.19326397022515,-0.592113659648685));
#73909=CARTESIAN_POINT('Ctrl Pts',(35.4450847171537,4.50390233381199,-2.0828044702768));
#73910=CARTESIAN_POINT('Ctrl Pts',(35.4053293930147,3.81454069739863,-3.57349528090534));
#73911=CARTESIAN_POINT('Ctrl Pts',(35.3655740688756,2.31162345149843,-4.68796184586595));
#73912=CARTESIAN_POINT('Ctrl Pts',(35.3258187447365,0.684976507282884,-4.91467373027875));
#73913=CARTESIAN_POINT('Ctrl Pts',(35.2860634205975,-0.941670436932289,
-5.1413856146915));
#73914=CARTESIAN_POINT('Ctrl Pts',(35.2463080964584,-2.69204707946263,-4.48034281855686));
#73915=CARTESIAN_POINT('Ctrl Pts',(35.2065527723194,-3.76274580585559,-3.2349582208322));
#73916=CARTESIAN_POINT('Ctrl Pts',(35.1782980855943,-4.52370695373544,-2.34984528506821));
#73917=CARTESIAN_POINT('Ctrl Pts',(35.1500433988692,-4.9413524884922,-1.16957245205999));
#73918=CARTESIAN_POINT('Ctrl Pts',(35.1217887121441,-4.95125214780166,0.00436800828097772));
#73919=CARTESIAN_POINT('Ctrl Pts',(35.0164112878558,-4.94977286428982,0.00400141439014362));
#73920=CARTESIAN_POINT('Ctrl Pts',(35.0433274613661,-4.94131528468185,-1.11517048059559));
#73921=CARTESIAN_POINT('Ctrl Pts',(35.0702436348764,-4.56556420838047,-2.23948404641346));
#73922=CARTESIAN_POINT('Ctrl Pts',(35.0971598083867,-3.86942204801114,-3.10657116091815));
#73923=CARTESIAN_POINT('Ctrl Pts',(35.1369151325258,-2.84121656324018,-4.38726320582311));
#73924=CARTESIAN_POINT('Ctrl Pts',(35.1766704566648,-1.11406385991951,-5.10680445214766));
#73925=CARTESIAN_POINT('Ctrl Pts',(35.2164257808039,0.519288032529988,-4.93493174246518));
#73926=CARTESIAN_POINT('Ctrl Pts',(35.2561811049429,2.1526399249793,-4.76305903278271));
#73927=CARTESIAN_POINT('Ctrl Pts',(35.295936429082,3.69219100655747,-3.69977236709346));
#73928=CARTESIAN_POINT('Ctrl Pts',(35.335691753221,4.43130075601119,-2.23311105273416));
#73929=CARTESIAN_POINT('Ctrl Pts',(35.3754470773601,5.17041050546498,-0.76644973837468));
#73930=CARTESIAN_POINT('Ctrl Pts',(35.4152024014992,5.10907892279414,1.10358622465495));
#73931=CARTESIAN_POINT('Ctrl Pts',(35.4549577256382,4.27545666994702,2.51866663657865));
#73932=CARTESIAN_POINT('Ctrl Pts',(35.4947130497773,3.44183441710001,3.93374704850219));
#73933=CARTESIAN_POINT('Ctrl Pts',(35.5344683739163,1.83592149407689,4.8938719093199));
#73934=CARTESIAN_POINT('Ctrl Pts',(35.5742236980554,0.194817927850411,4.95835228058715));
#73935=CARTESIAN_POINT('Ctrl Pts',(35.6139790221944,-1.44628563837616,5.0228326518544));
#73936=CARTESIAN_POINT('Ctrl Pts',(35.6537343463335,-3.12257984780612,4.19166853357104));
#73937=CARTESIAN_POINT('Ctrl Pts',(35.6934896704725,-4.0646602749189,2.84635700786281));
#73938=CARTESIAN_POINT('Ctrl Pts',(35.717796876267,-4.64066722021841,2.02380644838001));
#73939=CARTESIAN_POINT('Ctrl Pts',(35.7421040820614,-4.94219966027112,1.00904980577044));
#73940=CARTESIAN_POINT('Ctrl Pts',(35.7664112878558,-4.94744996620173,-0.002834044534147));
#73941=CARTESIAN_POINT('Origin',(10.45,0.,0.));
#73942=CARTESIAN_POINT('',(36.6217887121441,-4.95879821043464,-0.00354683266310052));
#73943=CARTESIAN_POINT('',(36.5164112878558,-4.960151313927,-0.00283453072728394));
#73944=CARTESIAN_POINT('',(10.45,-4.954,-6.06690024297599E-16));
#73945=CARTESIAN_POINT('Ctrl Pts',(36.6217887121441,-4.95879821043464,-0.00354683266310052));
#73946=CARTESIAN_POINT('Ctrl Pts',(36.5873519643988,-4.94727189684655,1.42166512058158));
#73947=CARTESIAN_POINT('Ctrl Pts',(36.5529152166535,-4.30004065620608,2.85600973832634));
#73948=CARTESIAN_POINT('Ctrl Pts',(36.5184784689082,-3.21681736593896,3.77826645686206));
#73949=CARTESIAN_POINT('Ctrl Pts',(36.4787231447691,-1.96629587831048,4.8429609238304));
#73950=CARTESIAN_POINT('Ctrl Pts',(36.4389678206301,-0.134709133881325,
5.22517393978799));
#73951=CARTESIAN_POINT('Ctrl Pts',(36.399212496491,1.43726013425452,4.74947304431184));
#73952=CARTESIAN_POINT('Ctrl Pts',(36.359457172352,3.00922940239028,4.27377214883571));
#73953=CARTESIAN_POINT('Ctrl Pts',(36.3197018482129,4.32158119423285,2.94015734192591));
#73954=CARTESIAN_POINT('Ctrl Pts',(36.2799465240739,4.77195768647691,1.36074620048107));
#73955=CARTESIAN_POINT('Ctrl Pts',(36.2401911999348,5.222334178721,-0.218664940963859));
#73956=CARTESIAN_POINT('Ctrl Pts',(36.2004358757957,4.81073537136662,-2.04387241694371));
#73957=CARTESIAN_POINT('Ctrl Pts',(36.1606805516567,3.72608141976468,-3.27712191766261));
#73958=CARTESIAN_POINT('Ctrl Pts',(36.1209252275176,2.6414274681628,-4.51037141838145));
#73959=CARTESIAN_POINT('Ctrl Pts',(36.0811699033786,0.883718372313122,-5.15166294383926));
#73960=CARTESIAN_POINT('Ctrl Pts',(36.0414145792395,-0.740272663720714,
-4.90664927332293));
#73961=CARTESIAN_POINT('Ctrl Pts',(36.0016592551005,-2.36426369975464,-4.66163560280659));
#73962=CARTESIAN_POINT('Ctrl Pts',(35.9619039309614,-3.85453667597279,-3.53031673631638));
#73963=CARTESIAN_POINT('Ctrl Pts',(35.9221486068224,-4.52706932186502,-2.03195816958627));
#73964=CARTESIAN_POINT('Ctrl Pts',(35.905361975263,-4.81104531709985,-1.39927830221521));
#73965=CARTESIAN_POINT('Ctrl Pts',(35.8885753437035,-4.94922318806473,-0.701157490031947));
#73966=CARTESIAN_POINT('Ctrl Pts',(35.8717887121441,-4.94662056565563,-0.00205432018779872));
#73967=CARTESIAN_POINT('Ctrl Pts',(35.7664112878558,-4.94744996620173,-0.002834044534147));
#73968=CARTESIAN_POINT('Ctrl Pts',(35.7818594062004,-4.95078672765623,-0.64592324214638));
#73969=CARTESIAN_POINT('Ctrl Pts',(35.7973075245451,-4.83445313833523,-1.28785209958534));
#73970=CARTESIAN_POINT('Ctrl Pts',(35.8127556428897,-4.59285123428814,-1.87854435599614));
#73971=CARTESIAN_POINT('Ctrl Pts',(35.8525109670288,-3.97109512174899,-3.39867526101325));
#73972=CARTESIAN_POINT('Ctrl Pts',(35.8922662911678,-2.51971625187527,-4.57947813791414));
#73973=CARTESIAN_POINT('Ctrl Pts',(35.9320216153069,-0.904884865128097,
-4.8789747637326));
#73974=CARTESIAN_POINT('Ctrl Pts',(35.9717769394459,0.709946521618895,-5.17847138955102));
#73975=CARTESIAN_POINT('Ctrl Pts',(36.011532263585,2.4882304252392,-4.59666176428724));
#73976=CARTESIAN_POINT('Ctrl Pts',(36.051287587724,3.61375003293099,-3.40059143130933));
#73977=CARTESIAN_POINT('Ctrl Pts',(36.0910429118631,4.73926964062285,-2.20452109833136));
#73978=CARTESIAN_POINT('Ctrl Pts',(36.1307982360022,5.21202495238608,-0.39419005763898));
#73979=CARTESIAN_POINT('Ctrl Pts',(36.1705535601412,4.81502541832947,1.19947552771663));
#73980=CARTESIAN_POINT('Ctrl Pts',(36.2103088842803,4.41802588427284,2.79314111307233));
#73981=CARTESIAN_POINT('Ctrl Pts',(36.2500642084193,3.15127150439663,4.17014124309119));
#73982=CARTESIAN_POINT('Ctrl Pts',(36.2898195325584,1.59619146287508,4.69844486981268));
#73983=CARTESIAN_POINT('Ctrl Pts',(36.3295748566974,0.0411114213536087,
5.22674849653414));
#73984=CARTESIAN_POINT('Ctrl Pts',(36.3693301808365,-1.80229428181327,4.90635561995797));
#73985=CARTESIAN_POINT('Ctrl Pts',(36.4090855049756,-3.08791844754446,3.88432376920091));
#73986=CARTESIAN_POINT('Ctrl Pts',(36.4448607659356,-4.24483367894236,2.96461158065307));
#73987=CARTESIAN_POINT('Ctrl Pts',(36.4806360268957,-4.95006028065536,1.4767157475938));
#73988=CARTESIAN_POINT('Ctrl Pts',(36.5164112878558,-4.960151313927,-0.00283453072728394));
#73989=CARTESIAN_POINT('Origin',(10.45,0.,0.));
#73990=CARTESIAN_POINT('',(37.3717887121441,-4.95785187747778,0.00390184669589733));
#73991=CARTESIAN_POINT('',(37.2664112878558,-4.95623082790828,0.00431859730377795));
#73992=CARTESIAN_POINT('',(10.45,-4.954,-6.06690024297599E-16));
#73993=CARTESIAN_POINT('Ctrl Pts',(37.3717887121441,-4.95785187747778,0.00390184669589733));
#73994=CARTESIAN_POINT('Ctrl Pts',(37.3656392333722,-4.96004850919265,0.258532516263073));
#73995=CARTESIAN_POINT('Ctrl Pts',(37.3594897546003,-4.94212966831781,0.512852861899553));
#73996=CARTESIAN_POINT('Ctrl Pts',(37.3533402758283,-4.90302063743832,0.763871725959299));
#73997=CARTESIAN_POINT('Ctrl Pts',(37.3135849516893,-4.65018746945052,2.38666557172065));
#73998=CARTESIAN_POINT('Ctrl Pts',(37.2738296275502,-3.51173140695091,3.87147728190302));
#73999=CARTESIAN_POINT('Ctrl Pts',(37.2340743034112,-2.01015914239786,4.5367929335275));
#74000=CARTESIAN_POINT('Ctrl Pts',(37.1943189792721,-0.508586877844729,
5.20210858515201));
#74001=CARTESIAN_POINT('Ctrl Pts',(37.1545636551331,1.3561015887619,5.04792817821849));
#74002=CARTESIAN_POINT('Ctrl Pts',(37.114808330994,2.72801223498102,4.14501827783009));
#74003=CARTESIAN_POINT('Ctrl Pts',(37.075053006855,4.09992288120007,3.24210837744174));
#74004=CARTESIAN_POINT('Ctrl Pts',(37.0352976827159,4.97905570703167,1.59046898359859));
#74005=CARTESIAN_POINT('Ctrl Pts',(36.9955423585768,4.9619060349538,-0.0518113523523847));
#74006=CARTESIAN_POINT('Ctrl Pts',(36.9557870344378,4.94475636287593,-1.69409168830335));
#74007=CARTESIAN_POINT('Ctrl Pts',(36.9160317102987,4.0313241928886,-3.32701296636214));
#74008=CARTESIAN_POINT('Ctrl Pts',(36.8762763861597,2.6408618587565,-4.2010788082045));
#74009=CARTESIAN_POINT('Ctrl Pts',(36.8365210620206,1.25039952462425,-5.07514465004697));
#74010=CARTESIAN_POINT('Ctrl Pts',(36.7967657378816,-0.617092973652882,
-5.19035505567283));
#74011=CARTESIAN_POINT('Ctrl Pts',(36.7570104137425,-2.10445019667369,-4.49382932261318));
#74012=CARTESIAN_POINT('Ctrl Pts',(36.7172550896035,-3.59180741969424,-3.79730358955364));
#74013=CARTESIAN_POINT('Ctrl Pts',(36.6774997654644,-4.69902936745862,-2.28904171780891));
#74014=CARTESIAN_POINT('Ctrl Pts',(36.6377444413253,-4.91791222592692,-0.661322822947106));
#74015=CARTESIAN_POINT('Ctrl Pts',(36.6324258649316,-4.94719497557761,-0.443562121019674));
#74016=CARTESIAN_POINT('Ctrl Pts',(36.6271072885378,-4.96057838955638,-0.223663398451484));
#74017=CARTESIAN_POINT('Ctrl Pts',(36.6217887121441,-4.95879821043464,-0.00354683266310052));
#74018=CARTESIAN_POINT('Ctrl Pts',(36.5164112878558,-4.960151313927,-0.00283453072728394));
#74019=CARTESIAN_POINT('Ctrl Pts',(36.5203913510348,-4.96127395982487,-0.167437203807423));
#74020=CARTESIAN_POINT('Ctrl Pts',(36.5243714142137,-4.95379293417925,-0.331936584213332));
#74021=CARTESIAN_POINT('Ctrl Pts',(36.5283514773927,-4.93737302018323,-0.495538814038059));
#74022=CARTESIAN_POINT('Ctrl Pts',(36.5681068015317,-4.77336079879503,-2.12969872158212));
#74023=CARTESIAN_POINT('Ctrl Pts',(36.6078621256708,-3.71749372772285,-3.67434771173236));
#74024=CARTESIAN_POINT('Ctrl Pts',(36.6476174498099,-2.2544053816326,-4.42050539418716));
#74025=CARTESIAN_POINT('Ctrl Pts',(36.6873727739489,-0.791317035542348,
-5.16666307664196));
#74026=CARTESIAN_POINT('Ctrl Pts',(36.727128098088,1.07899258556597,-5.11432945140131));
#74027=CARTESIAN_POINT('Ctrl Pts',(36.766883422227,2.4980672888367,-4.28752514602669));
#74028=CARTESIAN_POINT('Ctrl Pts',(36.8066387463661,3.91714199210752,-3.46072084065203));
#74029=CARTESIAN_POINT('Ctrl Pts',(36.8463940705051,4.8849817775407,-1.8594458551433));
#74030=CARTESIAN_POINT('Ctrl Pts',(36.8861493946442,4.95735735749111,-0.218671539309196));
#74031=CARTESIAN_POINT('Ctrl Pts',(36.9259047187833,5.02973293744153,1.42210277652491));
#74032=CARTESIAN_POINT('Ctrl Pts',(36.9656600429223,4.20664431190917,3.1023764226844));
#74033=CARTESIAN_POINT('Ctrl Pts',(37.0054153670614,2.86588058829837,4.05091862867918));
#74034=CARTESIAN_POINT('Ctrl Pts',(37.0451706912004,1.52511686468772,4.99946083467385));
#74035=CARTESIAN_POINT('Ctrl Pts',(37.0849260153394,-0.333321957001219,
5.216271600504));
#74036=CARTESIAN_POINT('Ctrl Pts',(37.1246813394785,-1.85642601585715,4.601836332316));
#74037=CARTESIAN_POINT('Ctrl Pts',(37.1644366636176,-3.37953007471326,3.98740106412792));
#74038=CARTESIAN_POINT('Ctrl Pts',(37.2041919877566,-4.56729937073627,2.54171976192149));
#74039=CARTESIAN_POINT('Ctrl Pts',(37.2439473118957,-4.87456318408798,0.928348188082862));
#74040=CARTESIAN_POINT('Ctrl Pts',(37.2514353038824,-4.9324369160222,0.62446654007456));
#74041=CARTESIAN_POINT('Ctrl Pts',(37.2589232958691,-4.95907343999133,0.314635836675023));
#74042=CARTESIAN_POINT('Ctrl Pts',(37.2664112878558,-4.95623082790828,0.00431859730377795));
#74043=CARTESIAN_POINT('Origin',(10.45,0.,0.));
#74044=CARTESIAN_POINT('',(38.1217887121441,-4.94678507297176,0.00149831882859774));
#74045=CARTESIAN_POINT('',(38.0164112878558,-4.94597286168509,0.000644103793583921));
#74046=CARTESIAN_POINT('',(10.45,-4.954,-6.06690024297599E-16));
#74047=CARTESIAN_POINT('Ctrl Pts',(38.1217887121441,-4.94678507297176,0.00149831882859774));
#74048=CARTESIAN_POINT('Ctrl Pts',(38.1041711782065,-4.94843324508386,0.735362320538199));
#74049=CARTESIAN_POINT('Ctrl Pts',(38.0865536442689,-4.79519616293353,1.46843094882367));
#74050=CARTESIAN_POINT('Ctrl Pts',(38.0689361103313,-4.48317629555338,2.12606890820242));
#74051=CARTESIAN_POINT('Ctrl Pts',(38.0291807861923,-3.77907939927567,3.6100796859804));
#74052=CARTESIAN_POINT('Ctrl Pts',(37.9894254620532,-2.26643827773527,4.70998691207959));
#74053=CARTESIAN_POINT('Ctrl Pts',(37.9496701379142,-0.637905686603803,
4.92102505154708));
#74054=CARTESIAN_POINT('Ctrl Pts',(37.9099148137751,0.990626904527571,5.13206319101456));
#74055=CARTESIAN_POINT('Ctrl Pts',(37.8701594896361,2.73505096525,4.45423224385044));
#74056=CARTESIAN_POINT('Ctrl Pts',(37.830404165497,3.79383240100999,3.19860832268579));
#74057=CARTESIAN_POINT('Ctrl Pts',(37.7906488413579,4.85261383676997,1.94298440152115));
#74058=CARTESIAN_POINT('Ctrl Pts',(37.7508935172189,5.2257526475675,0.109567506355982));
#74059=CARTESIAN_POINT('Ctrl Pts',(37.7111381930798,4.74243313727792,-1.46009779252003));
#74060=CARTESIAN_POINT('Ctrl Pts',(37.6713828689408,4.25911362698833,-3.02976309139605));
#74061=CARTESIAN_POINT('Ctrl Pts',(37.6316275448017,2.91933579561142,-4.33567679398308));
#74062=CARTESIAN_POINT('Ctrl Pts',(37.5918722206627,1.33780816048755,-4.77844757626196));
#74063=CARTESIAN_POINT('Ctrl Pts',(37.5521168965236,-0.243719474636306,
-5.22121835854084));
#74064=CARTESIAN_POINT('Ctrl Pts',(37.5123615723846,-2.06699691350693,-4.80084622051189));
#74065=CARTESIAN_POINT('Ctrl Pts',(37.4726062482455,-3.29503049620446,-3.71027216082727));
#74066=CARTESIAN_POINT('Ctrl Pts',(37.4390004028784,-4.33310797587571,-2.78839153213513));
#74067=CARTESIAN_POINT('Ctrl Pts',(37.4053945575112,-4.94584766240908,-1.3876110318066));
#74068=CARTESIAN_POINT('Ctrl Pts',(37.3717887121441,-4.95785187747778,0.00390184669589733));
#74069=CARTESIAN_POINT('Ctrl Pts',(37.2664112878558,-4.95623082790828,0.00431859730377795));
#74070=CARTESIAN_POINT('Ctrl Pts',(37.2986786200082,-4.94398141465747,-1.33290364507722));
#74071=CARTESIAN_POINT('Ctrl Pts',(37.3309459521605,-4.38432527605305,-2.67916051664711));
#74072=CARTESIAN_POINT('Ctrl Pts',(37.3632132843128,-3.41794155109712,-3.59734673003167));
#74073=CARTESIAN_POINT('Ctrl Pts',(37.4029686084519,-2.22729777407411,-4.72860822883691));
#74074=CARTESIAN_POINT('Ctrl Pts',(37.4427239325909,-0.419251889347554,
-5.2100693809767));
#74075=CARTESIAN_POINT('Ctrl Pts',(37.48247925673,1.17630066541565,-4.82074136594268));
#74076=CARTESIAN_POINT('Ctrl Pts',(37.5222345808691,2.77185322017895,-4.43141335090864));
#74077=CARTESIAN_POINT('Ctrl Pts',(37.5619899050081,4.15491244497898,-3.17129616870065));
#74078=CARTESIAN_POINT('Ctrl Pts',(37.6017452291472,4.69070067672837,-1.61877708111193));
#74079=CARTESIAN_POINT('Ctrl Pts',(37.6415005532862,5.22648890847773,-0.066257993523289));
#74080=CARTESIAN_POINT('Ctrl Pts',(37.6812558774253,4.91500614717662,1.77866299944616));
#74081=CARTESIAN_POINT('Ctrl Pts',(37.7210112015643,3.89915481177568,3.06919172853735));
#74082=CARTESIAN_POINT('Ctrl Pts',(37.7607665257034,2.88330347637469,4.35972045762861));
#74083=CARTESIAN_POINT('Ctrl Pts',(37.8005218498425,1.16308356687407,5.0958569228415));
#74084=CARTESIAN_POINT('Ctrl Pts',(37.8402771739815,-0.471814661666735,
4.93970480306567));
#74085=CARTESIAN_POINT('Ctrl Pts',(37.8800324981206,-2.10671289020754,4.78355268328984));
#74086=CARTESIAN_POINT('Ctrl Pts',(37.9197878222596,-3.65628943778838,3.73511197852511));
#74087=CARTESIAN_POINT('Ctrl Pts',(37.9595431463987,-4.40953831280109,2.27563841322242));
#74088=CARTESIAN_POINT('Ctrl Pts',(37.9784991935511,-4.76870080239037,1.57973540348341));
#74089=CARTESIAN_POINT('Ctrl Pts',(37.9974552407034,-4.94681402495116,0.790381920166041));
#74090=CARTESIAN_POINT('Ctrl Pts',(38.0164112878558,-4.94597286168509,0.000644103793583921));
#74091=CARTESIAN_POINT('Origin',(-19.0048063345371,0.,0.));
#74092=CARTESIAN_POINT('',(38.3701936654629,-4.51716168224788,0.0013681913210258));
#74093=CARTESIAN_POINT('',(38.5180063345368,-4.52176644287018,-0.00146738152635217));
#74094=CARTESIAN_POINT('',(-19.0048063345371,-4.52375,5.14627461305311E-12));
#74095=CARTESIAN_POINT('',(38.546,-0.439158351705441,-4.50835702469513));
#74096=CARTESIAN_POINT('Ctrl Pts',(38.3701936654629,-4.51716168224788,0.00136819132102561));
#74097=CARTESIAN_POINT('Ctrl Pts',(38.3923314556644,-4.5152704959798,-0.84070012943849));
#74098=CARTESIAN_POINT('Ctrl Pts',(38.4509335671768,-3.91909753352112,-3.072819358561));
#74099=CARTESIAN_POINT('Ctrl Pts',(38.5095356786891,-1.80749920607627,-4.36540260482715));
#74100=CARTESIAN_POINT('Ctrl Pts',(38.546,-0.439158351705441,-4.50835702469513));
#74101=CARTESIAN_POINT('',(38.546,-4.39991769847472,-1.05120802372743));
#74102=CARTESIAN_POINT('Origin',(38.546,0.,0.));
#74103=CARTESIAN_POINT('Ctrl Pts',(38.5180063345368,-4.52176644287018,-0.00146738152635186));
#74104=CARTESIAN_POINT('Ctrl Pts',(38.5273375563579,-4.52240870358347,-0.354396659090419));
#74105=CARTESIAN_POINT('Ctrl Pts',(38.5366687781789,-4.48209384756912,-0.707252988537638));
#74106=CARTESIAN_POINT('Ctrl Pts',(38.546,-4.39991769847472,-1.05120802372743));
#74107=CARTESIAN_POINT('Origin',(-19.0048063345371,0.,0.));
#74108=CARTESIAN_POINT('',(37.6201936654629,-4.52726734572873,0.00356297517063345));
#74109=CARTESIAN_POINT('',(37.7680063345368,-4.5164200107081,0.000588164021544935));
#74110=CARTESIAN_POINT('',(-19.0048063345371,-4.52375,5.14627461305311E-12));
#74111=CARTESIAN_POINT('Ctrl Pts',(37.6201936654629,-4.52726734572873,0.0035629751706337));
#74112=CARTESIAN_POINT('Ctrl Pts',(37.6537995108301,-4.51630568486565,-1.267098386179));
#74113=CARTESIAN_POINT('Ctrl Pts',(37.7271606803363,-3.29487162736131,-4.05941141533821));
#74114=CARTESIAN_POINT('Ctrl Pts',(37.8402771739814,1.44237491738078,-5.15162394203852));
#74115=CARTESIAN_POINT('Ctrl Pts',(37.9595431463987,5.11263327306786,-1.57413477445065));
#74116=CARTESIAN_POINT('Ctrl Pts',(38.0788091188158,4.09043705061455,3.44842457930616));
#74117=CARTESIAN_POINT('Ctrl Pts',(38.198075091233,-0.688330618759455,5.30531057884261));
#74118=CARTESIAN_POINT('Ctrl Pts',(38.2952032734487,-4.0629784562643,2.8514571901215));
#74119=CARTESIAN_POINT('Ctrl Pts',(38.3525761315253,-4.51866671224215,0.671496830346738));
#74120=CARTESIAN_POINT('Ctrl Pts',(38.3701936654629,-4.51716168224788,0.00136819132102561));
#74121=CARTESIAN_POINT('Ctrl Pts',(37.7680063345368,-4.5164200107081,0.000588164021545212));
#74122=CARTESIAN_POINT('Ctrl Pts',(37.7888056115235,-4.51557721299165,-0.790684179628111));
#74123=CARTESIAN_POINT('Ctrl Pts',(37.8493602126493,-3.94034756933214,-3.09560886266219));
#74124=CARTESIAN_POINT('Ctrl Pts',(37.9496701379142,-0.260588162173769,
-5.34342727819689));
#74125=CARTESIAN_POINT('Ctrl Pts',(38.0689361103313,4.35070685430609,-3.11045822607375));
#74126=CARTESIAN_POINT('Ctrl Pts',(38.1882020827485,4.97397191480465,1.9771100447851));
#74127=CARTESIAN_POINT('Ctrl Pts',(38.3074680551657,1.01988032406546,5.25111166397229));
#74128=CARTESIAN_POINT('Ctrl Pts',(38.4068563655133,-3.03575591970712,3.96049046164289));
#74129=CARTESIAN_POINT('Ctrl Pts',(38.4770357919704,-4.36801631736721,1.54840600921283));
#74130=CARTESIAN_POINT('Ctrl Pts',(38.5074598942884,-4.52104053962122,0.397424383040628));
#74131=CARTESIAN_POINT('Ctrl Pts',(38.5180063345368,-4.52176644287018,-0.00146738152635186));
#74132=CARTESIAN_POINT('Origin',(-19.0048063345371,0.,0.));
#74133=CARTESIAN_POINT('',(36.8701936654629,-4.5281314906043,-0.00323879375352202));
#74134=CARTESIAN_POINT('',(37.0180063345368,-4.525787082711,0.00394353140479434));
#74135=CARTESIAN_POINT('',(-19.0048063345371,-4.52375,5.14627461305311E-12));
#74136=CARTESIAN_POINT('Ctrl Pts',(36.8701936654629,-4.5281314906043,-0.00323879375352231));
#74137=CARTESIAN_POINT('Ctrl Pts',(36.8755122418567,-4.52975706293013,-0.204238453520589));
#74138=CARTESIAN_POINT('Ctrl Pts',(36.9205861423895,-4.4261858061835,-1.90598563772707));
#74139=CARTESIAN_POINT('Ctrl Pts',(37.0054153670614,-2.26880168119574,-4.84478234871799));
#74140=CARTESIAN_POINT('Ctrl Pts',(37.1246813394785,2.84710618461792,-4.5291688611629));
#74141=CARTESIAN_POINT('Ctrl Pts',(37.2439473118957,5.34941065311671,-0.0558578206189876));
#74142=CARTESIAN_POINT('Ctrl Pts',(37.3632132843128,2.9410676247427,4.46873061775304));
#74143=CARTESIAN_POINT('Ctrl Pts',(37.48247925673,-2.16715872819103,4.89110059102707));
#74144=CARTESIAN_POINT('Ctrl Pts',(37.56813938378,-4.40712914903362,1.96965775200708));
#74145=CARTESIAN_POINT('Ctrl Pts',(37.614044186691,-4.5292732021518,0.236079222940852));
#74146=CARTESIAN_POINT('Ctrl Pts',(37.6201936654629,-4.52726734572873,0.0035629751706337));
#74147=CARTESIAN_POINT('Ctrl Pts',(37.0180063345368,-4.525787082711,0.0039435314047942));
#74148=CARTESIAN_POINT('Ctrl Pts',(37.0502736666892,-4.51460151888657,-1.21714228187317));
#74149=CARTESIAN_POINT('Ctrl Pts',(37.1222963229807,-3.37390546114829,-3.96109486306854));
#74150=CARTESIAN_POINT('Ctrl Pts',(37.2340743034112,1.26817861053563,-5.1972267358067));
#74151=CARTESIAN_POINT('Ctrl Pts',(37.3533402758283,5.05700430786462,-1.745194981863));
#74152=CARTESIAN_POINT('Ctrl Pts',(37.4726062482455,4.20371193315622,3.30887930675979));
#74153=CARTESIAN_POINT('Ctrl Pts',(37.5918722206627,-0.508749602332581,
5.32549053072501));
#74154=CARTESIAN_POINT('Ctrl Pts',(37.6903389160931,-4.01344027747341,2.95422312405012));
#74155=CARTESIAN_POINT('Ctrl Pts',(37.7490502873845,-4.51718811977569,0.721738032169875));
#74156=CARTESIAN_POINT('Ctrl Pts',(37.7680063345368,-4.5164200107081,0.000588164021545212));
#74157=CARTESIAN_POINT('Origin',(-19.0048063345371,0.,0.));
#74158=CARTESIAN_POINT('',(36.1201936654629,-4.51701146222944,-0.00187590450993699));
#74159=CARTESIAN_POINT('',(36.2680063345368,-4.52936707839667,-0.0025883545316796));
#74160=CARTESIAN_POINT('',(-19.0048063345371,-4.52375,5.14627461305311E-12));
#74161=CARTESIAN_POINT('Ctrl Pts',(36.1201936654629,-4.51701146222944,-0.0018759045099373));
#74162=CARTESIAN_POINT('Ctrl Pts',(36.1369802970224,-4.51938804945676,-0.64026265553622));
#74163=CARTESIAN_POINT('Ctrl Pts',(36.1935222527209,-4.09438860903943,-2.78750195261098));
#74164=CARTESIAN_POINT('Ctrl Pts',(36.2898195325583,-0.79808549366158,-5.28984210344808));
#74165=CARTESIAN_POINT('Ctrl Pts',(36.4090855049755,4.01707590461207,-3.53305413112963));
#74166=CARTESIAN_POINT('Ctrl Pts',(36.5283514773927,5.14463147875642,1.46701590488028));
#74167=CARTESIAN_POINT('Ctrl Pts',(36.6476174498098,1.54950546845328,5.12039094490375));
#74168=CARTESIAN_POINT('Ctrl Pts',(36.7615648458333,-3.24428659251404,4.12002897620758));
#74169=CARTESIAN_POINT('Ctrl Pts',(36.8357569177176,-4.51760622595037,1.29819491102844));
#74170=CARTESIAN_POINT('Ctrl Pts',(36.8701936654629,-4.5281314906043,-0.00323879375352231));
#74171=CARTESIAN_POINT('Ctrl Pts',(36.2680063345368,-4.52936707839667,-0.00258835453167952));
#74172=CARTESIAN_POINT('Ctrl Pts',(36.2719863977159,-4.53039222360893,-0.152895448264976));
#74173=CARTESIAN_POINT('Ctrl Pts',(36.3157217850339,-4.45532562316811,-1.80352596964413));
#74174=CARTESIAN_POINT('Ctrl Pts',(36.399212496491,-2.4304670141352,-4.76573200043202));
#74175=CARTESIAN_POINT('Ctrl Pts',(36.5184784689082,2.69315822717824,-4.62236649547752));
#74176=CARTESIAN_POINT('Ctrl Pts',(36.6377444413254,5.34450979925368,-0.235748984964162));
#74177=CARTESIAN_POINT('Ctrl Pts',(36.7570104137425,3.08969722168957,4.36728164088206));
#74178=CARTESIAN_POINT('Ctrl Pts',(36.8762763861597,-2.00140852293053,4.96122453667856));
#74179=CARTESIAN_POINT('Ctrl Pts',(36.9632750264245,-4.3749228334945,2.07232576585655));
#74180=CARTESIAN_POINT('Ctrl Pts',(37.0105183425502,-4.52838281674591,0.28731002546971));
#74181=CARTESIAN_POINT('Ctrl Pts',(37.0180063345368,-4.525787082711,0.0039435314047942));
#74182=CARTESIAN_POINT('Origin',(-19.0048063345371,0.,0.));
#74183=CARTESIAN_POINT('',(35.3701936654629,-4.52124079604718,0.00398865108261888));
#74184=CARTESIAN_POINT('',(35.5180063345368,-4.51776883015844,-0.00258791056364449));
#74185=CARTESIAN_POINT('',(-19.0048063345371,-4.52375,5.14627461305311E-12));
#74186=CARTESIAN_POINT('Ctrl Pts',(35.3701936654629,-4.52124079604718,0.0039886510826187));
#74187=CARTESIAN_POINT('Ctrl Pts',(35.398448352188,-4.5122009123571,-1.06799624142191));
#74188=CARTESIAN_POINT('Ctrl Pts',(35.4664583630522,-3.59422183212154,-3.66221952290216));
#74189=CARTESIAN_POINT('Ctrl Pts',(35.5742236980554,0.738470871532858,-5.29849324252636));
#74190=CARTESIAN_POINT('Ctrl Pts',(35.6934896704726,4.85564198041892,-2.24546450419021));
#74191=CARTESIAN_POINT('Ctrl Pts',(35.8127556428897,4.5154184323632,2.86886148647546));
#74192=CARTESIAN_POINT('Ctrl Pts',(35.9320216153069,0.0301195233717248,
5.34962266769844));
#74193=CARTESIAN_POINT('Ctrl Pts',(36.0345009561646,-3.84763319583539,3.2615588907316));
#74194=CARTESIAN_POINT('Ctrl Pts',(36.0972249728833,-4.51375964239769,0.87161136893887));
#74195=CARTESIAN_POINT('Ctrl Pts',(36.1201936654629,-4.51701146222944,-0.0018759045099373));
#74196=CARTESIAN_POINT('Ctrl Pts',(35.5180063345368,-4.51776883015844,-0.00258791056364442));
#74197=CARTESIAN_POINT('Ctrl Pts',(35.5334544528815,-4.52081579718175,-0.589825447444406));
#74198=CARTESIAN_POINT('Ctrl Pts',(35.5886578953653,-4.14120522846699,-2.68451692967342));
#74199=CARTESIAN_POINT('Ctrl Pts',(35.6836166619881,-0.975553337067666,
-5.26000630617043));
#74200=CARTESIAN_POINT('Ctrl Pts',(35.8028826344052,3.89597177940602,-3.66616620183877));
#74201=CARTESIAN_POINT('Ctrl Pts',(35.9221486068224,5.19106272102259,1.29315053937908));
#74202=CARTESIAN_POINT('Ctrl Pts',(36.0414145792395,1.72084867623149,5.06537763153141));
#74203=CARTESIAN_POINT('Ctrl Pts',(36.1567004884777,-3.16055193286242,4.21696646507988));
#74204=CARTESIAN_POINT('Ctrl Pts',(36.2322310735768,-4.52015244138191,1.34846444553836));
#74205=CARTESIAN_POINT('Ctrl Pts',(36.2680063345368,-4.52936707839667,-0.00258835453167952));
#74206=CARTESIAN_POINT('Origin',(-19.0048063345371,0.,0.));
#74207=CARTESIAN_POINT('',(34.620193665463,-4.53121761719171,2.31264352865476E-5));
#74208=CARTESIAN_POINT('',(34.7680063345368,-4.51988998684523,0.00365389551349821));
#74209=CARTESIAN_POINT('',(-19.0048063345371,-4.52375,5.14627461305311E-12));
#74210=CARTESIAN_POINT('Ctrl Pts',(34.620193665463,-4.53121761719171,2.31264352862156E-5));
#74211=CARTESIAN_POINT('Ctrl Pts',(34.6599164073537,-4.53110444608029,-1.49847947960086));
#74212=CARTESIAN_POINT('Ctrl Pts',(34.7393944733835,-2.89652516710536,-4.49692522971762));
#74213=CARTESIAN_POINT('Ctrl Pts',(34.8586278635524,2.21410381975605,-4.8700219861014));
#74214=CARTESIAN_POINT('Ctrl Pts',(34.9778938359695,5.29362066876786,-0.772625449552068));
#74215=CARTESIAN_POINT('Ctrl Pts',(35.0971598083868,3.51368606780953,4.03402777461097));
#74216=CARTESIAN_POINT('Ctrl Pts',(35.2164257808038,-1.49175106234197,5.13751385765428));
#74217=CARTESIAN_POINT('Ctrl Pts',(35.307437066496,-4.26639226681861,2.38070896116213));
#74218=CARTESIAN_POINT('Ctrl Pts',(35.358693028049,-4.52492034222639,0.440323680449301));
#74219=CARTESIAN_POINT('Ctrl Pts',(35.3701936654629,-4.52124079604718,0.0039886510826187));
#74220=CARTESIAN_POINT('Ctrl Pts',(34.7680063345368,-4.51988998684523,0.00365389551349841));
#74221=CARTESIAN_POINT('Ctrl Pts',(34.7949225080472,-4.51216693966198,-1.01831902736694));
#74222=CARTESIAN_POINT('Ctrl Pts',(34.8615940056966,-3.66226324200522,-3.56138095634942));
#74223=CARTESIAN_POINT('Ctrl Pts',(34.968020827485,0.559842683756944,-5.32033333739675));
#74224=CARTESIAN_POINT('Ctrl Pts',(35.0872867999022,4.7773704624956,-2.40750952598498));
#74225=CARTESIAN_POINT('Ctrl Pts',(35.2065527723194,4.60935547635934,2.71536604189249));
#74226=CARTESIAN_POINT('Ctrl Pts',(35.3258187447365,0.210032554159402,5.34558294083782));
#74227=CARTESIAN_POINT('Ctrl Pts',(35.429636598809,-3.78729362285914,3.36357162759583));
#74228=CARTESIAN_POINT('Ctrl Pts',(35.4936991287425,-4.5129745081037,0.921414828194142));
#74229=CARTESIAN_POINT('Ctrl Pts',(35.5180063345368,-4.51776883015844,-0.00258791056364442));
#74230=CARTESIAN_POINT('Origin',(-19.0048063345371,0.,0.));
#74231=CARTESIAN_POINT('',(33.8701936654629,-4.52131001657821,-0.00400076979791308));
#74232=CARTESIAN_POINT('',(34.0180063345368,-4.53096931099894,0.000962538283377275));
#74233=CARTESIAN_POINT('',(-19.0048063345371,-4.52375,5.14627461305311E-12));
#74234=CARTESIAN_POINT('Ctrl Pts',(33.8701936654629,-4.52131001657821,-0.00400076979791265));
#74235=CARTESIAN_POINT('Ctrl Pts',(33.8816291383803,-4.52498402972909,-0.437846630360423));
#74236=CARTESIAN_POINT('Ctrl Pts',(33.9328199354367,-4.26830215849308,-2.37569557039852));
#74237=CARTESIAN_POINT('Ctrl Pts',(34.0237660566323,-1.50016308523093,-5.13506383480611));
#74238=CARTESIAN_POINT('Ctrl Pts',(34.1430320290494,3.50707457935405,-4.03977694491552));
#74239=CARTESIAN_POINT('Ctrl Pts',(34.2622980014666,5.29487894566462,0.763954724174054));
#74240=CARTESIAN_POINT('Ctrl Pts',(34.3815639738838,2.22207678584961,4.86638928031932));
#74241=CARTESIAN_POINT('Ctrl Pts',(34.5008299463009,-2.89055310896428,4.5015633500008));
#74242=CARTESIAN_POINT('Ctrl Pts',(34.5803731768273,-4.53065996027806,1.50221304852085));
#74243=CARTESIAN_POINT('Ctrl Pts',(34.6201610832147,-4.53121771001937,0.00125226072096765));
#74244=CARTESIAN_POINT('Ctrl Pts',(34.620193665463,-4.53121761719171,2.31264352862156E-5));
#74245=CARTESIAN_POINT('Ctrl Pts',(34.0180063345368,-4.53096931099894,0.000962538283377154));
#74246=CARTESIAN_POINT('Ctrl Pts',(34.0563905632129,-4.52678360881868,-1.44725925730328));
#74247=CARTESIAN_POINT('Ctrl Pts',(34.134530116028,-2.98893814438493,-4.40307445317525));
#74248=CARTESIAN_POINT('Ctrl Pts',(34.252424992982,2.04905202712797,-4.94173617688352));
#74249=CARTESIAN_POINT('Ctrl Pts',(34.3716909653993,5.26463906194561,-0.95023481270979));
#74250=CARTESIAN_POINT('Ctrl Pts',(34.4909569378164,3.64737925647783,3.91356553684459));
#74251=CARTESIAN_POINT('Ctrl Pts',(34.6102229102336,-1.31811109383836,5.18478097860004));
#74252=CARTESIAN_POINT('Ctrl Pts',(34.7025727091403,-4.22605285621444,2.4837093520579));
#74253=CARTESIAN_POINT('Ctrl Pts',(34.7551671839081,-4.52357391933511,0.491140138321174));
#74254=CARTESIAN_POINT('Ctrl Pts',(34.7680063345368,-4.51988998684523,0.00365389551349841));
#74255=CARTESIAN_POINT('Origin',(-19.0048063345371,0.,0.));
#74256=CARTESIAN_POINT('',(33.1201936654629,-4.51698102336606,0.00183909419487934));
#74257=CARTESIAN_POINT('',(33.2680063345368,-4.52278493895671,-0.00415864970829849));
#74258=CARTESIAN_POINT('',(-19.0048063345371,-4.52375,5.14627461305311E-12));
#74259=CARTESIAN_POINT('Ctrl Pts',(33.1201936654629,-4.51698102336606,0.00183909419487933));
#74260=CARTESIAN_POINT('Ctrl Pts',(33.143097193546,-4.51380328422841,-0.869184672515116));
#74261=CARTESIAN_POINT('Ctrl Pts',(33.2057560457681,-3.85050608020546,-3.25658480382206));
#74262=CARTESIAN_POINT('Ctrl Pts',(33.3081702221293,0.0213580713928514,
-5.34966482152014));
#74263=CARTESIAN_POINT('Ctrl Pts',(33.4274361945464,4.51071386747616,-2.87625281843973));
#74264=CARTESIAN_POINT('Ctrl Pts',(33.5467021669636,4.85931300288409,2.23750910832247));
#74265=CARTESIAN_POINT('Ctrl Pts',(33.6659681393807,0.747147551098779,5.29727669720119));
#74266=CARTESIAN_POINT('Ctrl Pts',(33.7737986388806,-3.59084071708882,3.66711594592562));
#74267=CARTESIAN_POINT('Ctrl Pts',(33.8418738142413,-4.51221135432166,1.0704148064563));
#74268=CARTESIAN_POINT('Ctrl Pts',(33.8701936654629,-4.52131001657821,-0.00400076979791265));
#74269=CARTESIAN_POINT('Ctrl Pts',(33.2680063345368,-4.52278493895671,-0.00415864970829852));
#74270=CARTESIAN_POINT('Ctrl Pts',(33.2781032942395,-4.52624527943587,-0.386906023541205));
#74271=CARTESIAN_POINT('Ctrl Pts',(33.3279555780812,-4.3064402681918,-2.27274940851596));
#74272=CARTESIAN_POINT('Ctrl Pts',(33.417563186062,-1.67202789967526,-5.08170181676528));
#74273=CARTESIAN_POINT('Ctrl Pts',(33.536829158479,3.36921585264198,-4.15544885543223));
#74274=CARTESIAN_POINT('Ctrl Pts',(33.6560951308963,5.31757821346333,0.585433681563546));
#74275=CARTESIAN_POINT('Ctrl Pts',(33.7753611033134,2.38449651621095,4.78889830921323));
#74276=CARTESIAN_POINT('Ctrl Pts',(33.8946270757306,-2.73751139581363,4.59623781038317));
#74277=CARTESIAN_POINT('Ctrl Pts',(33.9755088194717,-4.50685179120484,1.60423335784827));
#74278=CARTESIAN_POINT('Ctrl Pts',(34.0166352390738,-4.53111882546014,0.0526934288572369));
#74279=CARTESIAN_POINT('Ctrl Pts',(34.0180063345368,-4.53096931099894,0.000962538283377154));
#74280=CARTESIAN_POINT('Origin',(-19.0048063345371,0.,0.));
#74281=CARTESIAN_POINT('',(32.3701936654629,-4.52806646847511,0.00326652668130843));
#74282=CARTESIAN_POINT('',(32.5180063345368,-4.51649463517031,0.0010498457038996));
#74283=CARTESIAN_POINT('',(-19.0048063345371,-4.52375,5.14627461305311E-12));
#74284=CARTESIAN_POINT('Ctrl Pts',(32.3701936654629,-4.52806646847511,0.00326652668130825));
#74285=CARTESIAN_POINT('Ctrl Pts',(32.4045652487117,-4.51749649868563,-1.29575333366401));
#74286=CARTESIAN_POINT('Ctrl Pts',(32.4786921560994,-3.24828895209341,-4.11528667960992));
#74287=CARTESIAN_POINT('Ctrl Pts',(32.5925743876263,1.54111720041119,-5.12292178784925));
#74288=CARTESIAN_POINT('Ctrl Pts',(32.7118403600434,5.14222206711005,-1.47543962341761));
#74289=CARTESIAN_POINT('Ctrl Pts',(32.8311063324606,4.02285675976709,3.52647038272272));
#74290=CARTESIAN_POINT('Ctrl Pts',(32.9503723048777,-0.789420891907063,
5.29114208137));
#74291=CARTESIAN_POINT('Ctrl Pts',(33.0467347492119,-4.09205124409713,2.79251416600766));
#74292=CARTESIAN_POINT('Ctrl Pts',(33.1033418694069,-4.51931911781478,0.642714806587559));
#74293=CARTESIAN_POINT('Ctrl Pts',(33.1201936654629,-4.51698102336606,0.00183909419487933));
#74294=CARTESIAN_POINT('Ctrl Pts',(32.5180063345368,-4.51649463517031,0.00104984570389918));
#74295=CARTESIAN_POINT('Ctrl Pts',(32.5395713494051,-4.51479700942663,-0.819290632073363));
#74296=CARTESIAN_POINT('Ctrl Pts',(32.6008916884125,-3.90820502976704,-3.15427603926576));
#74297=CARTESIAN_POINT('Ctrl Pts',(32.701967351559,-0.15858550575743,-5.34735647672489));
#74298=CARTESIAN_POINT('Ctrl Pts',(32.821233323976,4.41142146589973,-3.02633958801825));
#74299=CARTESIAN_POINT('Ctrl Pts',(32.9404992963933,4.93182046980722,2.07280426123612));
#74300=CARTESIAN_POINT('Ctrl Pts',(33.0597652688104,0.924894296461516,5.26914994967698));
#74301=CARTESIAN_POINT('Ctrl Pts',(33.168934281525,-3.51996685280539,3.76740329753486));
#74302=CARTESIAN_POINT('Ctrl Pts',(33.2383479701004,-4.51262068733767,1.12010661771242));
#74303=CARTESIAN_POINT('Ctrl Pts',(33.2680063345368,-4.52278493895671,-0.00415864970829852));
#74304=CARTESIAN_POINT('Origin',(-19.0048063345371,0.,0.));
#74305=CARTESIAN_POINT('',(31.6201936654629,-4.52734081159469,-0.00353972901762604));
#74306=CARTESIAN_POINT('',(31.7680063345368,-4.52664803363837,0.00374760370527943));
#74307=CARTESIAN_POINT('',(-19.0048063345371,-4.52375,5.14627461305311E-12));
#74308=CARTESIAN_POINT('Ctrl Pts',(31.6201936654629,-4.52734081159469,-0.00353972901762627));
#74309=CARTESIAN_POINT('Ctrl Pts',(31.6262779797383,-4.52931909355584,-0.233582775118892));
#74310=CARTESIAN_POINT('Ctrl Pts',(31.6721176181527,-4.40866889995517,-1.96466148405792));
#74311=CARTESIAN_POINT('Ctrl Pts',(31.7577125807061,-2.17514757970455,-4.88754569045954));
#74312=CARTESIAN_POINT('Ctrl Pts',(31.8769785531233,2.9337351189414,-4.47354089304141));
#74313=CARTESIAN_POINT('Ctrl Pts',(31.9962445255404,5.34950014457238,0.047096422840884));
#74314=CARTESIAN_POINT('Ctrl Pts',(32.1155104979576,2.85451733611025,4.52450004394633));
#74315=CARTESIAN_POINT('Ctrl Pts',(32.2347764703748,-2.26086260233548,4.84849153481623));
#74316=CARTESIAN_POINT('Ctrl Pts',(32.3196708595432,-4.42471940840208,1.91097730457275));
#74317=CARTESIAN_POINT('Ctrl Pts',(32.3648099245726,-4.52972207968608,0.206736535289742));
#74318=CARTESIAN_POINT('Ctrl Pts',(32.3701936654629,-4.52806646847511,0.00326652668130825));
#74319=CARTESIAN_POINT('Ctrl Pts',(31.7680063345368,-4.52664803363837,0.00374760370527919));
#74320=CARTESIAN_POINT('Ctrl Pts',(31.8010394045708,-4.51551060816241,-1.24570217322333));
#74321=CARTESIAN_POINT('Ctrl Pts',(31.8738277987439,-3.32900333837359,-4.01743474331935));
#74322=CARTESIAN_POINT('Ctrl Pts',(31.986371517056,1.36794009374822,-5.17185755330946));
#74323=CARTESIAN_POINT('Ctrl Pts',(32.1056374894731,5.08968755204155,-1.64755918691883));
#74324=CARTESIAN_POINT('Ctrl Pts',(32.2249034618903,4.13919060489128,3.3891697786018));
#74325=CARTESIAN_POINT('Ctrl Pts',(32.3441694343074,-0.611011127479355,
5.31469999660417));
#74326=CARTESIAN_POINT('Ctrl Pts',(32.4418703918563,-4.04282844254874,2.89542259591036));
#74327=CARTESIAN_POINT('Ctrl Pts',(32.4998160252661,-4.51792659974311,0.693015378267232));
#74328=CARTESIAN_POINT('Ctrl Pts',(32.5180063345368,-4.51649463517031,0.00104984570389918));
#74329=CARTESIAN_POINT('Origin',(-19.0048063345371,0.,0.));
#74330=CARTESIAN_POINT('',(30.8701936654629,-4.51669300721655,-0.00143314003944115));
#74331=CARTESIAN_POINT('',(31.0180063345369,-4.52868647542216,-0.00297892043936654));
#74332=CARTESIAN_POINT('',(-19.0048063345371,-4.52375,5.14627461305311E-12));
#74333=CARTESIAN_POINT('Ctrl Pts',(30.870193665463,-4.51669300721655,-0.00143314003944142));
#74334=CARTESIAN_POINT('Ctrl Pts',(30.887746034904,-4.51858387894054,-0.669058025820529));
#74335=CARTESIAN_POINT('Ctrl Pts',(30.945053728484,-4.06657764023515,-2.84638774123857));
#74336=CARTESIAN_POINT('Ctrl Pts',(31.0421167462031,-0.696140458765788,
-5.30422080342567));
#74337=CARTESIAN_POINT('Ctrl Pts',(31.1613827186203,4.08432171488679,-3.45509565701559));
#74338=CARTESIAN_POINT('Ctrl Pts',(31.2806486910375,5.11544778739555,1.56574704350808));
#74339=CARTESIAN_POINT('Ctrl Pts',(31.3999146634546,1.45068200768019,5.14926126569795));
#74340=CARTESIAN_POINT('Ctrl Pts',(31.5130963215965,-3.29089145935549,4.06417453521408));
#74341=CARTESIAN_POINT('Ctrl Pts',(31.5865226555992,-4.51639286439593,1.26953416622099));
#74342=CARTESIAN_POINT('Ctrl Pts',(31.6201936654629,-4.52734081159469,-0.00353972901762627));
#74343=CARTESIAN_POINT('Ctrl Pts',(31.0180063345369,-4.52868647542216,-0.00297892043936619));
#74344=CARTESIAN_POINT('Ctrl Pts',(31.0227521355974,-4.53004991495928,-0.182274828229998));
#74345=CARTESIAN_POINT('Ctrl Pts',(31.0672532607971,-4.43888415483644,-1.86212428583227));
#74346=CARTESIAN_POINT('Ctrl Pts',(31.1515097101358,-2.33830543955411,-4.81162117411165));
#74347=CARTESIAN_POINT('Ctrl Pts',(31.270775682553,2.78161148635255,-4.56968359854373));
#74348=CARTESIAN_POINT('Ctrl Pts',(31.3900416549701,5.34805758082949,-0.132856177649306));
#74349=CARTESIAN_POINT('Ctrl Pts',(31.5093076273873,3.00508008957021,4.42593089723243));
#74350=CARTESIAN_POINT('Ctrl Pts',(31.6285735998045,-2.09650851344057,4.92179059945456));
#74351=CARTESIAN_POINT('Ctrl Pts',(31.7148065021876,-4.39359747073332,2.01357634362355));
#74352=CARTESIAN_POINT('Ctrl Pts',(31.7612840804318,-4.52891450793364,0.258011554449596));
#74353=CARTESIAN_POINT('Ctrl Pts',(31.7680063345368,-4.52664803363837,0.00374760370527919));
#74354=CARTESIAN_POINT('Origin',(-19.0048063345371,0.,0.));
#74355=CARTESIAN_POINT('',(30.1201936654629,-4.52207059346122,0.00410535199279809));
#74356=CARTESIAN_POINT('',(30.2680063345368,-4.51730521221276,-0.00219145969648615));
#74357=CARTESIAN_POINT('',(-19.0048063345371,-4.52375,5.14627461305311E-12));
#74358=CARTESIAN_POINT('Ctrl Pts',(30.1201936654629,-4.52207059346122,0.00410535199279808));
#74359=CARTESIAN_POINT('Ctrl Pts',(30.1492140900696,-4.51237828040898,-1.09641936695486));
#74360=CARTESIAN_POINT('Ctrl Pts',(30.2179898388154,-3.55408529374172,-3.71967609856161));
#74361=CARTESIAN_POINT('Ctrl Pts',(30.3265209117001,0.840297817034937,-5.28330099923434));
#74362=CARTESIAN_POINT('Ctrl Pts',(30.4457868841173,4.89795430972499,-2.15160717829025));
#74363=CARTESIAN_POINT('Ctrl Pts',(30.5650528565345,4.45937416947051,2.95522450695096));
#74364=CARTESIAN_POINT('Ctrl Pts',(30.6843188289516,-0.0728336840866598,
5.34921163577276));
#74365=CARTESIAN_POINT('Ctrl Pts',(30.7860324319278,-3.88101638918563,3.2030683936662));
#74366=CARTESIAN_POINT('Ctrl Pts',(30.8479907107649,-4.5143011398753,0.843082191301476));
#74367=CARTESIAN_POINT('Ctrl Pts',(30.870193665463,-4.51669300721655,-0.00143314003944142));
#74368=CARTESIAN_POINT('Ctrl Pts',(30.2680063345368,-4.51730521221276,-0.00219145969648581));
#74369=CARTESIAN_POINT('Ctrl Pts',(30.2842201907631,-4.5199969460127,-0.618695688963642));
#74370=CARTESIAN_POINT('Ctrl Pts',(30.3401893711284,-4.11470020632812,-2.74343937300367));
#74371=CARTESIAN_POINT('Ctrl Pts',(30.4359138756328,-0.874149621850558,
-5.27780570790802));
#74372=CARTESIAN_POINT('Ctrl Pts',(30.55517984805,3.96580166144261,-3.59051358915504));
#74373=CARTESIAN_POINT('Ctrl Pts',(30.6744458204671,5.16521618558982,1.39280738364225));
#74374=CARTESIAN_POINT('Ctrl Pts',(30.7937117928843,1.62305233596266,5.09755546968683));
#74375=CARTESIAN_POINT('Ctrl Pts',(30.9082319642409,-3.20880931129668,4.16162230541739));
#74376=CARTESIAN_POINT('Ctrl Pts',(30.9829968114584,-4.5186284541668,1.31967749552273));
#74377=CARTESIAN_POINT('Ctrl Pts',(31.0180063345369,-4.52868647542216,-0.00297892043936619));
#74378=CARTESIAN_POINT('Origin',(-19.0048063345371,0.,0.));
#74379=CARTESIAN_POINT('',(29.3701936654629,-4.53114466631056,-0.000518721095705797));
#74380=CARTESIAN_POINT('',(29.5180063345369,-4.52064530787469,0.00386511480189006));
#74381=CARTESIAN_POINT('',(-19.0048063345371,-4.52375,5.14627461305311E-12));
#74382=CARTESIAN_POINT('Ctrl Pts',(29.3701936654629,-4.53114466631056,-0.000518721095705719));
#74383=CARTESIAN_POINT('Ctrl Pts',(29.3709268210962,-4.53118943009193,-0.0281775193443082));
#74384=CARTESIAN_POINT('Ctrl Pts',(29.4114153008686,-4.51841712149835,-1.55559068039991));
#74385=CARTESIAN_POINT('Ctrl Pts',(29.49165910478,-2.81084864442134,-4.55175787668666));
#74386=CARTESIAN_POINT('Ctrl Pts',(29.6109250771972,2.30741204557965,-4.82651214871964));
#74387=CARTESIAN_POINT('Ctrl Pts',(29.7301910496143,5.30750872044597,-0.670612445614996));
#74388=CARTESIAN_POINT('Ctrl Pts',(29.8494570220315,3.43540495621067,4.10089778666421));
#74389=CARTESIAN_POINT('Ctrl Pts',(29.9687229944486,-1.59034064221755,5.10785537300494));
#74390=CARTESIAN_POINT('Ctrl Pts',(30.0589685422591,-4.28852214464261,2.32180582197069));
#74391=CARTESIAN_POINT('Ctrl Pts',(30.1094587659306,-4.52565586170806,0.411198716439513));
#74392=CARTESIAN_POINT('Ctrl Pts',(30.1201936654629,-4.52207059346122,0.00410535199279808));
#74393=CARTESIAN_POINT('Ctrl Pts',(29.5180063345369,-4.52064530787469,0.0038651148018904));
#74394=CARTESIAN_POINT('Ctrl Pts',(29.5456882459288,-4.51214506679005,-1.04673871353975));
#74395=CARTESIAN_POINT('Ctrl Pts',(29.6131254814597,-3.62366603379782,-3.61912902093094));
#74396=CARTESIAN_POINT('Ctrl Pts',(29.7203180411298,0.662122995951101,-5.30857455349746));
#74397=CARTESIAN_POINT('Ctrl Pts',(29.839584013547,4.8228156661174,-2.31512844189271));
#74398=CARTESIAN_POINT('Ctrl Pts',(29.9588499859641,4.55624766770592,2.8035652020832));
#74399=CARTESIAN_POINT('Ctrl Pts',(30.0781159583813,0.107123774146093,5.34863488647531));
#74400=CARTESIAN_POINT('Ctrl Pts',(30.1811680745722,-3.822123913385,3.3052499950529));
#74401=CARTESIAN_POINT('Ctrl Pts',(30.2444648666241,-4.51339698927079,0.89293270625552));
#74402=CARTESIAN_POINT('Ctrl Pts',(30.2680063345368,-4.51730521221276,-0.00219145969648581));
#74403=CARTESIAN_POINT('Origin',(-19.0048063345371,0.,0.));
#74404=CARTESIAN_POINT('',(28.6201936654629,-4.52051575184804,-0.0038334580682193));
#74405=CARTESIAN_POINT('',(28.7680063345369,-4.53116771210378,0.000428735186510879));
#74406=CARTESIAN_POINT('',(-19.0048063345371,-4.52375,5.14627461305311E-12));
#74407=CARTESIAN_POINT('Ctrl Pts',(28.6201936654629,-4.52051575184804,-0.00383345806821922));
#74408=CARTESIAN_POINT('Ctrl Pts',(28.6323948762619,-4.52422411022693,-0.466936104215469));
#74409=CARTESIAN_POINT('Ctrl Pts',(28.6843514111999,-4.24554373484115,-2.43461423389684));
#74410=CARTESIAN_POINT('Ctrl Pts',(28.7760632702771,-1.4010666075983,-5.1629819127029));
#74411=CARTESIAN_POINT('Ctrl Pts',(28.8953292426941,3.58416621553077,-3.97153904793497));
#74412=CARTESIAN_POINT('Ctrl Pts',(29.0145952151114,5.27919696290035,0.865707396715219));
#74413=CARTESIAN_POINT('Ctrl Pts',(29.1338611875285,2.12801697082046,4.90824954965865));
#74414=CARTESIAN_POINT('Ctrl Pts',(29.2523940043124,-2.94526594078766,4.44795128087226));
#74415=CARTESIAN_POINT('Ctrl Pts',(29.3311714969572,-4.52876211649412,1.47161930378696));
#74416=CARTESIAN_POINT('Ctrl Pts',(29.3701936654629,-4.53114466631056,-0.000518721095705719));
#74417=CARTESIAN_POINT('Ctrl Pts',(28.7680063345369,-4.53116771210378,0.000428735186511165));
#74418=CARTESIAN_POINT('Ctrl Pts',(28.8071563010945,-4.5291761204828,-1.47651041274696));
#74419=CARTESIAN_POINT('Ctrl Pts',(28.8860615917911,-2.93643577703342,-4.45690962027768));
#74420=CARTESIAN_POINT('Ctrl Pts',(29.0047222066268,2.14377087841479,-4.90138930025648));
#74421=CARTESIAN_POINT('Ctrl Pts',(29.123988179044,5.28195037803777,-0.848746638140402));
#74422=CARTESIAN_POINT('Ctrl Pts',(29.2432541514612,3.57139155113628,3.98303063511691));
#74423=CARTESIAN_POINT('Ctrl Pts',(29.3625201238783,-1.41764243240855,5.15845525187946));
#74424=CARTESIAN_POINT('Ctrl Pts',(29.4541041849036,-4.24939018309867,2.42478002480354));
#74425=CARTESIAN_POINT('Ctrl Pts',(29.5059329217897,-4.52435267177785,0.462083966588632));
#74426=CARTESIAN_POINT('Ctrl Pts',(29.5180063345369,-4.52064530787469,0.0038651148018904));
#74427=CARTESIAN_POINT('Origin',(-19.0048063345371,0.,0.));
#74428=CARTESIAN_POINT('',(27.870193665463,-4.51737697201026,0.00225976351037011));
#74429=CARTESIAN_POINT('',(28.0180063345369,-4.52192984201937,-0.00408982420865234));
#74430=CARTESIAN_POINT('',(-19.0048063345371,-4.52375,5.14627461305311E-12));
#74431=CARTESIAN_POINT('Ctrl Pts',(27.870193665463,-4.51737697201026,0.00225976351037008));
#74432=CARTESIAN_POINT('Ctrl Pts',(27.8938629314276,-4.51332129582812,-0.8976879117203));
#74433=CARTESIAN_POINT('Ctrl Pts',(27.9572875215313,-3.81636887415937,-3.31499081853051));
#74434=CARTESIAN_POINT('Ctrl Pts',(28.060467435774,0.124302552914632,-5.34826315219841));
#74435=CARTESIAN_POINT('Ctrl Pts',(28.1797334081912,4.56522890198429,-2.78891644591795));
#74436=CARTESIAN_POINT('Ctrl Pts',(28.2989993806083,4.81535473947628,2.33060691727008));
#74437=CARTESIAN_POINT('Ctrl Pts',(28.4182653530255,0.645068908923938,5.31067377764479));
#74438=CARTESIAN_POINT('Ctrl Pts',(28.5253301146437,-3.6301684636346,3.60950202170377));
#74439=CARTESIAN_POINT('Ctrl Pts',(28.5926395521229,-4.51214112995506,1.04199576415337));
#74440=CARTESIAN_POINT('Ctrl Pts',(28.6201936654629,-4.52051575184804,-0.00383345806821922));
#74441=CARTESIAN_POINT('Ctrl Pts',(28.0180063345369,-4.52192984201937,-0.0040898242086522));
#74442=CARTESIAN_POINT('Ctrl Pts',(28.0288690321211,-4.52553520025187,-0.416062179398293));
#74443=CARTESIAN_POINT('Ctrl Pts',(28.0794870538443,-4.28487623826261,-2.3316351509503));
#74444=CARTESIAN_POINT('Ctrl Pts',(28.1698603997067,-1.57392648948877,-5.11293712629961));
#74445=CARTESIAN_POINT('Ctrl Pts',(28.2891263721238,3.44855899679427,-4.08984247831593));
#74446=CARTESIAN_POINT('Ctrl Pts',(28.408392344541,5.30532746904341,0.687656235354114));
#74447=CARTESIAN_POINT('Ctrl Pts',(28.5276583169582,2.291897852936,4.83389851812331));
#74448=CARTESIAN_POINT('Ctrl Pts',(28.6469242893753,-2.82545402003632,4.54270626746531));
#74449=CARTESIAN_POINT('Ctrl Pts',(28.7270402952349,-4.52068612267638,1.54585040122244));
#74450=CARTESIAN_POINT('Ctrl Pts',(28.7674009769554,-4.53119850715146,0.0232659529202972));
#74451=CARTESIAN_POINT('Ctrl Pts',(28.7680063345369,-4.53116771210378,0.000428735186511165));
#74452=CARTESIAN_POINT('Origin',(-19.0048063345371,0.,0.));
#74453=CARTESIAN_POINT('',(27.120193665463,-4.52880516386923,0.00291706699860573));
#74454=CARTESIAN_POINT('',(27.2680063345369,-4.51674019473067,0.00150848591183417));
#74455=CARTESIAN_POINT('',(-19.0048063345371,-4.52375,5.14627461305311E-12));
#74456=CARTESIAN_POINT('Ctrl Pts',(27.120193665463,-4.52880516386923,0.0029170669986057));
#74457=CARTESIAN_POINT('Ctrl Pts',(27.1553309865932,-4.51887004847389,-1.32447633190377));
#74458=CARTESIAN_POINT('Ctrl Pts',(27.2302236318626,-3.2008213721839,-4.17088006383837));
#74459=CARTESIAN_POINT('Ctrl Pts',(27.344871601271,1.63941683012594,-5.09231600815622));
#74460=CARTESIAN_POINT('Ctrl Pts',(27.4641375736882,5.16966304351028,-1.37620997176607));
#74461=CARTESIAN_POINT('Ctrl Pts',(27.5834035461054,3.95424874510512,3.60323281674365));
#74462=CARTESIAN_POINT('Ctrl Pts',(27.7026695185225,-0.891096936738138,
5.27497072211403));
#74463=CARTESIAN_POINT('Ctrl Pts',(27.7982662249751,-4.11917516279323,2.73360655033951));
#74464=CARTESIAN_POINT('Ctrl Pts',(27.8541076072885,-4.52013328237071,0.61388036379995));
#74465=CARTESIAN_POINT('Ctrl Pts',(27.870193665463,-4.51737697201026,0.00225976351037008));
#74466=CARTESIAN_POINT('Ctrl Pts',(27.2680063345368,-4.51674019473067,0.00150848591183396));
#74467=CARTESIAN_POINT('Ctrl Pts',(27.2903370872867,-4.51420659348407,-0.847845685554157));
#74468=CARTESIAN_POINT('Ctrl Pts',(27.3524231641757,-3.8755018834822,-3.21283625088979));
#74469=CARTESIAN_POINT('Ctrl Pts',(27.4542645652037,-0.0556521236575815,
-5.34941805180156));
#74470=CARTESIAN_POINT('Ctrl Pts',(27.5735305376208,4.46884314287686,-2.94088619571898));
#74471=CARTESIAN_POINT('Ctrl Pts',(27.692796510038,4.89101834366639,2.16732789714115));
#74472=CARTESIAN_POINT('Ctrl Pts',(27.8120624824552,0.823324007385604,5.2859727799782));
#74473=CARTESIAN_POINT('Ctrl Pts',(27.9204657572881,-3.5608457184922,3.71009937882906));
#74474=CARTESIAN_POINT('Ctrl Pts',(27.989113707982,-4.51234030238609,1.09167513814337));
#74475=CARTESIAN_POINT('Ctrl Pts',(28.0180063345369,-4.52192984201937,-0.0040898242086522));
#74476=CARTESIAN_POINT('Origin',(-19.0048063345371,0.,0.));
#74477=CARTESIAN_POINT('',(26.370193665463,-4.52650623014407,-0.00378441848545811));
#74478=CARTESIAN_POINT('',(26.5180063345369,-4.52747628307774,0.00349333724076611));
#74479=CARTESIAN_POINT('',(-19.0048063345371,-4.52375,5.14627461305311E-12));
#74480=CARTESIAN_POINT('Ctrl Pts',(26.370193665463,-4.52650623014407,-0.00378441848545744));
#74481=CARTESIAN_POINT('Ctrl Pts',(26.3770437176199,-4.52882920222418,-0.262903224669573));
#74482=CARTESIAN_POINT('Ctrl Pts',(26.4236490939158,-4.39052545737866,-2.02337872152482));
#74483=CARTESIAN_POINT('Ctrl Pts',(26.5100097943509,-2.08068932314761,-4.92849894089096));
#74484=CARTESIAN_POINT('Ctrl Pts',(26.629275766768,3.01928023853817,-4.41625596076554));
#74485=CARTESIAN_POINT('Ctrl Pts',(26.7485417391852,5.34760319937945,0.1500329690799));
#74486=CARTESIAN_POINT('Ctrl Pts',(26.8678077116024,2.76691968873083,4.57859424997864));
#74487=CARTESIAN_POINT('Ctrl Pts',(26.9870736840195,-2.35374783936478,4.80408586294104));
#74488=CARTESIAN_POINT('Ctrl Pts',(27.0712023353064,-4.4416704537898,1.85234129232427));
#74489=CARTESIAN_POINT('Ctrl Pts',(27.1155756624542,-4.53011090919392,0.177372788514735));
#74490=CARTESIAN_POINT('Ctrl Pts',(27.120193665463,-4.52880516386923,0.0029170669986057));
#74491=CARTESIAN_POINT('Ctrl Pts',(26.5180063345369,-4.52747628307774,0.00349333724076601));
#74492=CARTESIAN_POINT('Ctrl Pts',(26.5518051424524,-4.51658359282757,-1.27431317611325));
#74493=CARTESIAN_POINT('Ctrl Pts',(26.625359274507,-3.28317857968101,-4.07351566037758));
#74494=CARTESIAN_POINT('Ctrl Pts',(26.7386687307007,1.4672135077607,-5.14457531526681));
#74495=CARTESIAN_POINT('Ctrl Pts',(26.8579347031179,5.12045050920806,-1.54930863115098));
#74496=CARTESIAN_POINT('Ctrl Pts',(26.977200675535,4.073203247058,3.46819635545099));
#74497=CARTESIAN_POINT('Ctrl Pts',(27.0964666479522,-0.713173556682066,
5.30195757526005));
#74498=CARTESIAN_POINT('Ctrl Pts',(27.1934018676195,-4.0712717902843,2.83656196042909));
#74499=CARTESIAN_POINT('Ctrl Pts',(27.2505817631477,-4.51871715073782,0.664255172562189));
#74500=CARTESIAN_POINT('Ctrl Pts',(27.2680063345368,-4.51674019473067,0.00150848591183396));
#74501=CARTESIAN_POINT('Origin',(-19.0048063345371,0.,0.));
#74502=CARTESIAN_POINT('',(25.620193665463,-4.51646227191973,-0.000971816212263622));
#74503=CARTESIAN_POINT('',(25.7680063345369,-4.52793736187105,-0.0033197696265741));
#74504=CARTESIAN_POINT('',(-19.0048063345371,-4.52375,5.14627461305311E-12));
#74505=CARTESIAN_POINT('Ctrl Pts',(25.620193665463,-4.51646227191973,-0.000971816212263291));
#74506=CARTESIAN_POINT('Ctrl Pts',(25.6385117727855,-4.51779658626017,-0.697811251222172));
#74507=CARTESIAN_POINT('Ctrl Pts',(25.6965852042472,-4.038006838103,-2.90524271252507));
#74508=CARTESIAN_POINT('Ctrl Pts',(25.7944139598479,-0.593937630424711,
-5.31663502236041));
#74509=CARTESIAN_POINT('Ctrl Pts',(25.9136799322651,4.15005490520629,-3.37585754343952));
#74510=CARTESIAN_POINT('Ctrl Pts',(26.0329459046822,5.08436941740803,1.66389828329445));
#74511=CARTESIAN_POINT('Ctrl Pts',(26.1522118770994,1.35132147900805,5.17622450538955));
#74512=CARTESIAN_POINT('Ctrl Pts',(26.2646277973596,-3.3365604235817,4.00804952635544));
#74513=CARTESIAN_POINT('Ctrl Pts',(26.3372883934808,-4.51534747888903,1.24093235123574));
#74514=CARTESIAN_POINT('Ctrl Pts',(26.370193665463,-4.52650623014407,-0.00378441848545744));
#74515=CARTESIAN_POINT('Ctrl Pts',(25.7680063345369,-4.52793736187105,-0.00331976962657424));
#74516=CARTESIAN_POINT('Ctrl Pts',(25.773517873479,-4.5296519411211,-0.211635204411083));
#74517=CARTESIAN_POINT('Ctrl Pts',(25.8187847365603,-4.42183036494298,-1.92076769273718));
#74518=CARTESIAN_POINT('Ctrl Pts',(25.9038069237805,-2.24527805335948,-4.85572827852936));
#74519=CARTESIAN_POINT('Ctrl Pts',(26.0230728961977,2.86903493736783,-4.51530831505123));
#74520=CARTESIAN_POINT('Ctrl Pts',(26.1423388686148,5.34962389335311,-0.0299140681537413));
#74521=CARTESIAN_POINT('Ctrl Pts',(26.2616048410321,2.91935141602282,4.48294077158877));
#74522=CARTESIAN_POINT('Ctrl Pts',(26.3808708134492,-2.19083474590394,4.88053416830044));
#74523=CARTESIAN_POINT('Ctrl Pts',(26.4663379779508,-4.4116357972034,1.95486584720251));
#74524=CARTESIAN_POINT('Ctrl Pts',(26.5120498183134,-4.52939595096529,0.22868693715409));
#74525=CARTESIAN_POINT('Ctrl Pts',(26.5180063345369,-4.52747628307774,0.00349333724076601));
#74526=CARTESIAN_POINT('Origin',(-19.0048063345371,0.,0.));
#74527=CARTESIAN_POINT('',(24.870193665463,-4.52292991114911,0.00416441657176817));
#74528=CARTESIAN_POINT('',(25.0180063345369,-4.51692316959201,-0.00176640309098947));
#74529=CARTESIAN_POINT('',(-19.0048063345371,-4.52375,5.14627461305311E-12));
#74530=CARTESIAN_POINT('Ctrl Pts',(24.870193665463,-4.52292991114911,0.00416441657176813));
#74531=CARTESIAN_POINT('Ctrl Pts',(24.8999798279512,-4.51267992564295,-1.12485307430951));
#74532=CARTESIAN_POINT('Ctrl Pts',(24.9695213145785,-3.51305705825671,-3.77694834013157));
#74533=CARTESIAN_POINT('Ctrl Pts',(25.0788181253449,0.941813547390232,-5.2661520213317));
#74534=CARTESIAN_POINT('Ctrl Pts',(25.1980840977621,4.93845262345068,-2.05695297849937));
#74535=CARTESIAN_POINT('Ctrl Pts',(25.3173500701792,4.40167832088221,3.04049302405052));
#74536=CARTESIAN_POINT('Ctrl Pts',(25.4366160425964,-0.175759912236459,
5.34681945861972));
#74537=CARTESIAN_POINT('Ctrl Pts',(25.537563907691,-3.91358405387219,3.14449502406534));
#74538=CARTESIAN_POINT('Ctrl Pts',(25.5987564486465,-4.51490075765882,0.814521716580516));
#74539=CARTESIAN_POINT('Ctrl Pts',(25.620193665463,-4.51646227191973,-0.000971816212263291));
#74540=CARTESIAN_POINT('Ctrl Pts',(25.0180063345369,-4.51692316959201,-0.00176640309098988));
#74541=CARTESIAN_POINT('Ctrl Pts',(25.0349859286447,-4.51918422158869,-0.647522979345086));
#74542=CARTESIAN_POINT('Ctrl Pts',(25.0917208468916,-4.08745153246059,-2.80234344813435));
#74543=CARTESIAN_POINT('Ctrl Pts',(25.1882110892776,-0.772422159146575,
-5.29365040967637));
#74544=CARTESIAN_POINT('Ctrl Pts',(25.3074770616947,4.03416276912766,-3.51353118728043));
#74545=CARTESIAN_POINT('Ctrl Pts',(25.4267430341119,5.13745663366157,1.49194838686019));
#74546=CARTESIAN_POINT('Ctrl Pts',(25.546009006529,1.52465490894722,5.12784536237498));
#74547=CARTESIAN_POINT('Ctrl Pts',(25.659763440004,-3.25611918384849,4.10598031695728));
#74548=CARTESIAN_POINT('Ctrl Pts',(25.73376254934,-4.51728449628163,1.2909664681739));
#74549=CARTESIAN_POINT('Ctrl Pts',(25.7680063345369,-4.52793736187105,-0.00331976962657424));
#74550=CARTESIAN_POINT('Origin',(-19.0048063345371,0.,0.));
#74551=CARTESIAN_POINT('',(24.120193665463,-4.53092246829786,-0.00105004667653403));
#74552=CARTESIAN_POINT('',(24.2680063345369,-4.52144663499091,0.00402336840721218));
#74553=CARTESIAN_POINT('',(-19.0048063345371,-4.52375,5.14627461305311E-12));
#74554=CARTESIAN_POINT('Ctrl Pts',(24.120193665463,-4.53092246829786,-0.00105004667653446));
#74555=CARTESIAN_POINT('Ctrl Pts',(24.1216925589779,-4.53109947999406,-0.0576042696761754));
#74556=CARTESIAN_POINT('Ctrl Pts',(24.1629467766318,-4.50448666451256,-1.61398211810567));
#74557=CARTESIAN_POINT('Ctrl Pts',(24.2439563184247,-2.72273453653836,-4.60500667897073));
#74558=CARTESIAN_POINT('Ctrl Pts',(24.3632222908419,2.39986569333583,-4.78121475399025));
#74559=CARTESIAN_POINT('Ctrl Pts',(24.4824882632591,5.31943107188467,-0.568351072218813));
#74560=CARTESIAN_POINT('Ctrl Pts',(24.6017542356763,3.35585150064429,4.16624898145168));
#74561=CARTESIAN_POINT('Ctrl Pts',(24.7210202080934,-1.6883412200409,5.0763051321345));
#74562=CARTESIAN_POINT('Ctrl Pts',(24.8105000180223,-4.30997355915991,2.2629239214585));
#74563=CARTESIAN_POINT('Ctrl Pts',(24.8602245038122,-4.52636048944094,0.38203645287768));
#74564=CARTESIAN_POINT('Ctrl Pts',(24.870193665463,-4.52292991114911,0.00416441657176813));
#74565=CARTESIAN_POINT('Ctrl Pts',(24.2680063345369,-4.52144663499091,0.00402336840721242));
#74566=CARTESIAN_POINT('Ctrl Pts',(24.2964539838104,-4.51223436788339,-1.07515811813252));
#74567=CARTESIAN_POINT('Ctrl Pts',(24.364656957223,-3.58419125381158,-3.67671503401053));
#74568=CARTESIAN_POINT('Ctrl Pts',(24.4726152547746,0.764158082763927,-5.29484967457566));
#74569=CARTESIAN_POINT('Ctrl Pts',(24.5918812271917,4.86647468160752,-2.22188992190905));
#74570=CARTESIAN_POINT('Ctrl Pts',(24.7111471996089,4.50145239709396,2.89072602792189));
#74571=CARTESIAN_POINT('Ctrl Pts',(24.8304131720261,0.00417532019002488,
5.34970590018823));
#74572=CARTESIAN_POINT('Ctrl Pts',(24.9326995503354,-3.85612301657671,3.24682793721983));
#74573=CARTESIAN_POINT('Ctrl Pts',(24.9952306045057,-4.51389028732547,0.864424941250599));
#74574=CARTESIAN_POINT('Ctrl Pts',(25.0180063345369,-4.51692316959201,-0.00176640309098988));
#74575=CARTESIAN_POINT('Origin',(-19.0048063345371,0.,0.));
#74576=CARTESIAN_POINT('',(23.370193665463,-4.51976894652972,-0.00361372362653868));
#74577=CARTESIAN_POINT('',(23.5180063345369,-4.53121424191125,-0.000113818667257792));
#74578=CARTESIAN_POINT('',(-19.0048063345371,-4.52375,5.14627461305311E-12));
#74579=CARTESIAN_POINT('Ctrl Pts',(23.370193665463,-4.51976894652972,-0.00361372362653871));
#74580=CARTESIAN_POINT('Ctrl Pts',(23.3831606141435,-4.52344198664446,-0.495985503601568));
#74581=CARTESIAN_POINT('Ctrl Pts',(23.4358828869631,-4.22208968250827,-2.49354528016135));
#74582=CARTESIAN_POINT('Ctrl Pts',(23.5283604839218,-1.30145122794406,-5.1889878175909));
#74583=CARTESIAN_POINT('Ctrl Pts',(23.6476264563389,3.65993041225227,-3.90183024326985));
#74584=CARTESIAN_POINT('Ctrl Pts',(23.7668924287561,5.26155976547379,0.967139444016044));
#74585=CARTESIAN_POINT('Ctrl Pts',(23.8861584011732,2.03316901887958,4.94829198921123));
#74586=CARTESIAN_POINT('Ctrl Pts',(24.0039254800755,-2.99760568614095,4.39405292852535));
#74587=CARTESIAN_POINT('Ctrl Pts',(24.0819372348388,-4.52640457852891,1.44238985563963));
#74588=CARTESIAN_POINT('Ctrl Pts',(24.120193665463,-4.53092246829786,-0.00105004667653446));
#74589=CARTESIAN_POINT('Ctrl Pts',(23.5180063345369,-4.53121424191125,-0.000113818667257794));
#74590=CARTESIAN_POINT('Ctrl Pts',(23.518166714837,-4.53121647143214,-0.00616402523120993));
#74591=CARTESIAN_POINT('Ctrl Pts',(23.5580824192762,-4.52846221956104,-1.51194697710339));
#74592=CARTESIAN_POINT('Ctrl Pts',(23.6377534478544,-2.87607962259252,-4.51082438766087));
#74593=CARTESIAN_POINT('Ctrl Pts',(23.7570194202716,2.2376957581383,-4.85922713461897));
#74594=CARTESIAN_POINT('Ctrl Pts',(23.8762853926887,5.2973054597101,-0.746944119953741));
#74595=CARTESIAN_POINT('Ctrl Pts',(23.9955513651059,3.49408113758448,4.05102056965703));
#74596=CARTESIAN_POINT('Ctrl Pts',(24.1148173375231,-1.51664872988588,5.13021902865199));
#74597=CARTESIAN_POINT('Ctrl Pts',(24.2056356606667,-4.27203338814583,2.3658639017595));
#74598=CARTESIAN_POINT('Ctrl Pts',(24.2566986596713,-4.52510842511722,0.432987929006955));
#74599=CARTESIAN_POINT('Ctrl Pts',(24.2680063345369,-4.52144663499091,0.00402336840721242));
#74600=CARTESIAN_POINT('Origin',(-19.0048063345371,0.,0.));
#74601=CARTESIAN_POINT('',(22.620193665463,-4.51785376865908,0.00265090740345769));
#74602=CARTESIAN_POINT('',(22.7680063345369,-4.52110593686914,-0.00396372416147706));
#74603=CARTESIAN_POINT('',(-19.0048063345371,-4.52375,5.14627461305311E-12));
#74604=CARTESIAN_POINT('Ctrl Pts',(22.620193665463,-4.51785376865908,0.0026509074034578));
#74605=CARTESIAN_POINT('Ctrl Pts',(22.6446286693092,-4.51291135001306,-0.926166110723544));
#74606=CARTESIAN_POINT('Ctrl Pts',(22.7088189972944,-3.78139899895146,-3.37329467135839));
#74607=CARTESIAN_POINT('Ctrl Pts',(22.8127646494188,0.227200997477541,-5.34488068871223));
#74608=CARTESIAN_POINT('Ctrl Pts',(22.9320306218359,4.61805314856548,-2.70054716434442));
#74609=CARTESIAN_POINT('Ctrl Pts',(23.0512965942531,4.76961305100215,2.42284155766206));
#74610=CARTESIAN_POINT('Ctrl Pts',(23.1705625666702,0.542751357650036,5.32210398560502));
#74611=CARTESIAN_POINT('Ctrl Pts',(23.2768615904069,-3.6686200124915,3.55172811343481));
#74612=CARTESIAN_POINT('Ctrl Pts',(23.3434052900045,-4.51218082536938,1.01357547269836));
#74613=CARTESIAN_POINT('Ctrl Pts',(23.370193665463,-4.51976894652972,-0.00361372362653871));
#74614=CARTESIAN_POINT('Ctrl Pts',(22.7680063345369,-4.52110593686913,-0.00396372416147671));
#74615=CARTESIAN_POINT('Ctrl Pts',(22.7796347700027,-4.52479494802337,-0.445180761673963));
#74616=CARTESIAN_POINT('Ctrl Pts',(22.8310185296075,-4.26263226036918,-2.39054140945846));
#74617=CARTESIAN_POINT('Ctrl Pts',(22.9221576133515,-1.47524215652576,-5.14227879751937));
#74618=CARTESIAN_POINT('Ctrl Pts',(23.0414235857686,3.52662492527076,-4.02272137840373));
#74619=CARTESIAN_POINT('Ctrl Pts',(23.1606895581858,5.29111183221057,0.789624107312617));
#74620=CARTESIAN_POINT('Ctrl Pts',(23.2799555306029,2.19845035747676,4.87710843405375));
#74621=CARTESIAN_POINT('Ctrl Pts',(23.39906112272,-2.90547756613246,4.48801620593015));
#74622=CARTESIAN_POINT('Ctrl Pts',(23.4784113906979,-4.53066381424317,1.49357081045434));
#74623=CARTESIAN_POINT('Ctrl Pts',(23.5180063345369,-4.53121424191125,-0.000113818667257794));
#74624=CARTESIAN_POINT('Origin',(-19.0048063345371,0.,0.));
#74625=CARTESIAN_POINT('',(21.870193665463,-4.52947294422145,0.00251866946226621));
#74626=CARTESIAN_POINT('',(22.0180063345369,-4.51707300815329,0.00194757944713214));
#74627=CARTESIAN_POINT('',(-19.0048063345371,-4.52375,5.14627461305311E-12));
#74628=CARTESIAN_POINT('Ctrl Pts',(21.870193665463,-4.52947294422145,0.00251866946226618));
#74629=CARTESIAN_POINT('Ctrl Pts',(21.9060967244749,-4.52042477226542,-1.35327695553929));
#74630=CARTESIAN_POINT('Ctrl Pts',(21.9817551076258,-3.15240519488923,-4.22617295064406));
#74631=CARTESIAN_POINT('Ctrl Pts',(22.0971688149158,1.73710928192197,-5.05982422742967));
#74632=CARTESIAN_POINT('Ctrl Pts',(22.2164347873329,5.19518937246391,-1.27647062404992));
#74633=CARTESIAN_POINT('Ctrl Pts',(22.3357007597501,3.88417622643207,3.67866074976264));
#74634=CARTESIAN_POINT('Ctrl Pts',(22.4549667321673,-0.992442953004545,
5.25684571343457));
#74635=CARTESIAN_POINT('Ctrl Pts',(22.5497977007382,-4.14555697384072,2.6746816967096));
#74636=CARTESIAN_POINT('Ctrl Pts',(22.6048733451701,-4.52095257875769,0.585002942242804));
#74637=CARTESIAN_POINT('Ctrl Pts',(22.620193665463,-4.51785376865908,0.0026509074034578));
#74638=CARTESIAN_POINT('Ctrl Pts',(22.0180063345369,-4.51707300815329,0.00194757944713159));
#74639=CARTESIAN_POINT('Ctrl Pts',(22.0411028251683,-4.51367549994054,-0.87636993032822));
#74640=CARTESIAN_POINT('Ctrl Pts',(22.1039546399389,-3.84198169693815,-3.27131196429832));
#74641=CARTESIAN_POINT('Ctrl Pts',(22.2065617788485,0.0473018698816033,
-5.34949840498282));
#74642=CARTESIAN_POINT('Ctrl Pts',(22.3258277512656,4.5246097295625,-2.85434361052691));
#74643=CARTESIAN_POINT('Ctrl Pts',(22.4450937236827,4.84840476952531,2.26104883685696));
#74644=CARTESIAN_POINT('Ctrl Pts',(22.5643596961,0.72144879027182,5.30083788611039));
#74645=CARTESIAN_POINT('Ctrl Pts',(22.6719972330513,-3.60083421408175,3.65261330297864));
#74646=CARTESIAN_POINT('Ctrl Pts',(22.7398794458636,-4.51218294749925,1.0632531453274));
#74647=CARTESIAN_POINT('Ctrl Pts',(22.7680063345369,-4.52110593686913,-0.00396372416147671));
#74648=CARTESIAN_POINT('Origin',(-19.0048063345371,0.,0.));
#74649=CARTESIAN_POINT('',(21.120193665463,-4.5256415251865,-0.00397048047999635));
#74650=CARTESIAN_POINT('',(21.2680063345369,-4.52825856173475,0.00318332847191585));
#74651=CARTESIAN_POINT('',(-19.0048063345371,-4.52375,5.14627461305311E-12));
#74652=CARTESIAN_POINT('Ctrl Pts',(21.120193665463,-4.5256415251865,-0.0039704804799966));
#74653=CARTESIAN_POINT('Ctrl Pts',(21.1278094555015,-4.52829030282037,-0.292197201058006));
#74654=CARTESIAN_POINT('Ctrl Pts',(21.175180569679,-4.37174733578044,-2.08213483401641));
#74655=CARTESIAN_POINT('Ctrl Pts',(21.2623070079956,-1.98546045804875,-4.96762686192806));
#74656=CARTESIAN_POINT('Ctrl Pts',(21.3815729804128,3.10370713105701,-4.35733541449928));
#74657=CARTESIAN_POINT('Ctrl Pts',(21.50083895283,5.34372570444373,0.252913948788086));
#74658=CARTESIAN_POINT('Ctrl Pts',(21.6201049252471,2.67829727906562,4.63099271806533));
#74659=CARTESIAN_POINT('Ctrl Pts',(21.7393708976643,-2.44576133731702,4.75790093956452));
#74660=CARTESIAN_POINT('Ctrl Pts',(21.8227338110696,-4.45801051457141,1.79375067470569));
#74661=CARTESIAN_POINT('Ctrl Pts',(21.8663414003358,-4.53044377952769,0.147990513631471));
#74662=CARTESIAN_POINT('Ctrl Pts',(21.870193665463,-4.52947294422145,0.00251866946226618));
#74663=CARTESIAN_POINT('Ctrl Pts',(21.2680063345369,-4.52825856173475,0.00318332847191599));
#74664=CARTESIAN_POINT('Ctrl Pts',(21.302570880334,-4.5178259772815,-1.30298465945109));
#74665=CARTESIAN_POINT('Ctrl Pts',(21.3768907502702,-3.23641643652308,-4.12932346936464));
#74666=CARTESIAN_POINT('Ctrl Pts',(21.4909659443455,1.56594352144461,-5.11538772132217));
#74667=CARTESIAN_POINT('Ctrl Pts',(21.6102319167626,5.14931704538713,-1.45048427012945));
#74668=CARTESIAN_POINT('Ctrl Pts',(21.7294978891798,4.00570732897041,3.54593844369029));
#74669=CARTESIAN_POINT('Ctrl Pts',(21.848763861597,-0.81507185340302,5.28725150958398));
#74670=CARTESIAN_POINT('Ctrl Pts',(21.9449333433827,-4.09895685643359,2.77767174480397));
#74671=CARTESIAN_POINT('Ctrl Pts',(22.0013475010293,-4.51952353297804,0.635452703477159));
#74672=CARTESIAN_POINT('Ctrl Pts',(22.0180063345369,-4.51707300815329,0.00194757944713159));
#74673=CARTESIAN_POINT('Origin',(-19.0048063345371,0.,0.));
#74674=CARTESIAN_POINT('',(20.370193665463,-4.51632155205853,-0.000497944189619361));
#74675=CARTESIAN_POINT('',(20.5180063345369,-4.52713413638993,-0.00360679990569157));
#74676=CARTESIAN_POINT('',(-19.0048063345371,-4.52375,5.14627461305311E-12));
#74677=CARTESIAN_POINT('Ctrl Pts',(20.370193665463,-4.51632155205854,-0.000497944189619404));
#74678=CARTESIAN_POINT('Ctrl Pts',(20.3892775106672,-4.51703258266485,-0.726523234129351));
#74679=CARTESIAN_POINT('Ctrl Pts',(20.4481166800104,-4.00866695933645,-2.96405924100118));
#74680=CARTESIAN_POINT('Ctrl Pts',(20.5467111734927,-0.491514830074133,
-5.32708016099266));
#74681=CARTESIAN_POINT('Ctrl Pts',(20.6659771459098,4.21425107232707,-3.29536914005304));
#74682=CARTESIAN_POINT('Ctrl Pts',(20.785243118327,5.05140798950344,1.76143327815877));
#74683=CARTESIAN_POINT('Ctrl Pts',(20.9045090907442,1.25146047202657,5.20127066751764));
#74684=CARTESIAN_POINT('Ctrl Pts',(21.0161592731228,-3.38129990730632,3.95166908847989));
#74685=CARTESIAN_POINT('Ctrl Pts',(21.0880541313624,-4.51446337050284,1.21238034693031));
#74686=CARTESIAN_POINT('Ctrl Pts',(21.120193665463,-4.5256415251865,-0.0039704804799966));
#74687=CARTESIAN_POINT('Ctrl Pts',(20.5180063345369,-4.52713413638994,-0.00360679990569227));
#74688=CARTESIAN_POINT('Ctrl Pts',(20.5242836113606,-4.52920047619369,-0.240973755364537));
#74689=CARTESIAN_POINT('Ctrl Pts',(20.5703162123234,-4.40415625335664,-1.97945418684146));
#74690=CARTESIAN_POINT('Ctrl Pts',(20.6561041374253,-2.1514191011895,-4.89803700505059));
#74691=CARTESIAN_POINT('Ctrl Pts',(20.7753701098425,2.95539580647574,-4.45926073232701));
#74692=CARTESIAN_POINT('Ctrl Pts',(20.8946360822597,5.34920890774529,0.0730391203798664));
#74693=CARTESIAN_POINT('Ctrl Pts',(21.0139020546768,2.83254152524977,4.53829033442592));
#74694=CARTESIAN_POINT('Ctrl Pts',(21.133168027094,-2.28434957613141,4.83747017208749));
#74695=CARTESIAN_POINT('Ctrl Pts',(21.217869453714,-4.42904907663949,1.89619713950708));
#74696=CARTESIAN_POINT('Ctrl Pts',(21.262815556195,-4.52982528949528,0.199338907729788));
#74697=CARTESIAN_POINT('Ctrl Pts',(21.2680063345369,-4.52825856173475,0.00318332847191599));
#74698=CARTESIAN_POINT('Origin',(-19.0048063345371,0.,0.));
#74699=CARTESIAN_POINT('',(19.620193665463,-4.52380831897895,0.00416407692592279));
#74700=CARTESIAN_POINT('',(19.7680063345369,-4.51662655140182,-0.00131840381877635));
#74701=CARTESIAN_POINT('',(-19.0048063345371,-4.52375,5.14627461305311E-12));
#74702=CARTESIAN_POINT('Ctrl Pts',(19.620193665463,-4.52380831897895,0.00416407692592272));
#74703=CARTESIAN_POINT('Ctrl Pts',(19.6507455658328,-4.51311329478492,-1.15330418304886));
#74704=CARTESIAN_POINT('Ctrl Pts',(19.7210527903417,-3.47112927897302,-3.83402298617469));
#74705=CARTESIAN_POINT('Ctrl Pts',(19.8311153389897,1.04298046566866,-5.24705266011862));
#74706=CARTESIAN_POINT('Ctrl Pts',(19.9503813114068,4.97712192131473,-1.9615369612098));
#74707=CARTESIAN_POINT('Ctrl Pts',(20.069647283824,4.34235225730947,3.12463545765959));
#74708=CARTESIAN_POINT('Ctrl Pts',(20.1889132562412,-0.278621045569882,
5.34244702199188));
#74709=CARTESIAN_POINT('Ctrl Pts',(20.2890953834541,-3.94534524041323,3.08584830453267));
#74710=CARTESIAN_POINT('Ctrl Pts',(20.3495221865281,-4.51555136900353,0.785927240390639));
#74711=CARTESIAN_POINT('Ctrl Pts',(20.370193665463,-4.51632155205854,-0.000497944189619404));
#74712=CARTESIAN_POINT('Ctrl Pts',(19.7680063345369,-4.51662655140182,-0.00131840381877607));
#74713=CARTESIAN_POINT('Ctrl Pts',(19.7857516665263,-4.51838370628948,-0.676307662444315));
#74714=CARTESIAN_POINT('Ctrl Pts',(19.8432523226548,-4.0594499556041,-2.86122216995006));
#74715=CARTESIAN_POINT('Ctrl Pts',(19.9405083029223,-0.670408620522066,
-5.30753454377244));
#74716=CARTESIAN_POINT('Ctrl Pts',(20.0597742753395,4.10102977567299,-3.43524750649084));
#74717=CARTESIAN_POINT('Ctrl Pts',(20.1790402477567,5.10779436232139,1.59053682888681));
#74718=CARTESIAN_POINT('Ctrl Pts',(20.2983062201738,1.42569280748336,5.15623609530228));
#74719=CARTESIAN_POINT('Ctrl Pts',(20.4112949157672,-3.30248785860587,4.05005623492106));
#74720=CARTESIAN_POINT('Ctrl Pts',(20.4845282872216,-4.51611390840542,1.26232146629252));
#74721=CARTESIAN_POINT('Ctrl Pts',(20.5180063345369,-4.52713413638994,-0.00360679990569227));
#74722=CARTESIAN_POINT('Origin',(-19.0048063345371,0.,0.));
#74723=CARTESIAN_POINT('',(18.870193665463,-4.53056695484048,-0.00156093939472719));
#74724=CARTESIAN_POINT('',(19.0180063345369,-4.52228481540387,0.00412574957127501));
#74725=CARTESIAN_POINT('',(-19.0048063345371,-4.52375,5.14627461305311E-12));
#74726=CARTESIAN_POINT('Ctrl Pts',(18.870193665463,-4.53056695484048,-0.00156093939472799));
#74727=CARTESIAN_POINT('Ctrl Pts',(18.8724582968594,-4.53094833149528,-0.0870248407490605));
#74728=CARTESIAN_POINT('Ctrl Pts',(18.9144782523949,-4.48997606208692,-1.67242400599934));
#74729=CARTESIAN_POINT('Ctrl Pts',(18.9962535320695,-2.63361203087714,-4.65654996114543));
#74730=CARTESIAN_POINT('Ctrl Pts',(19.1155195044867,2.49143052170795,-4.73414657835247));
#74731=CARTESIAN_POINT('Ctrl Pts',(19.2347854769038,5.32938330746976,-0.465879203105705));
#74732=CARTESIAN_POINT('Ctrl Pts',(19.354051449321,3.27505516474859,4.23005715536775));
#74733=CARTESIAN_POINT('Ctrl Pts',(19.4733174217382,-1.78571650020385,5.04287482005294));
#74734=CARTESIAN_POINT('Ctrl Pts',(19.5620314937855,-4.3307553536982,2.20406739515846));
#74735=CARTESIAN_POINT('Ctrl Pts',(19.6109902416938,-4.52703007732092,0.352838652550256));
#74736=CARTESIAN_POINT('Ctrl Pts',(19.620193665463,-4.52380831897895,0.00416407692592272));
#74737=CARTESIAN_POINT('Ctrl Pts',(19.0180063345369,-4.52228481540387,0.00412574957127487));
#74738=CARTESIAN_POINT('Ctrl Pts',(19.047219721692,-4.51244234885314,-1.10358329220441));
#74739=CARTESIAN_POINT('Ctrl Pts',(19.1161884329861,-3.5438307602279,-3.73412638843344));
#74740=CARTESIAN_POINT('Ctrl Pts',(19.2249124684193,0.865910154356953,-5.27916378381931));
#74741=CARTESIAN_POINT('Ctrl Pts',(19.3441784408365,4.9083313391403,-2.12782849802824));
#74742=CARTESIAN_POINT('Ctrl Pts',(19.4634444132536,4.4449899589576,2.97681623829445));
#74743=CARTESIAN_POINT('Ctrl Pts',(19.5827103856708,-0.0987746801464204,
5.3487955853977));
#74744=CARTESIAN_POINT('Ctrl Pts',(19.6842310260986,-3.88929985589648,3.18831563741184));
#74745=CARTESIAN_POINT('Ctrl Pts',(19.7459963423872,-4.51444710695377,0.835888152378177));
#74746=CARTESIAN_POINT('Ctrl Pts',(19.7680063345369,-4.51662655140182,-0.00131840381877607));
#74747=CARTESIAN_POINT('Origin',(-19.0048063345371,0.,0.));
#74748=CARTESIAN_POINT('',(18.120193665463,-4.51907785273017,-0.00334514387128823));
#74749=CARTESIAN_POINT('',(18.2680063345369,-4.53110217211561,-0.000654014894287402));
#74750=CARTESIAN_POINT('',(-19.0048063345371,-4.52375,5.14627461305311E-12));
#74751=CARTESIAN_POINT('Ctrl Pts',(18.120193665463,-4.51907785273017,-0.00334514387128795));
#74752=CARTESIAN_POINT('Ctrl Pts',(18.1339263520251,-4.52264256910505,-0.524993719082137));
#74753=CARTESIAN_POINT('Ctrl Pts',(18.1874143627263,-4.19793093531997,-2.55248358637957));
#74754=CARTESIAN_POINT('Ctrl Pts',(18.2806576975665,-1.20135384003343,-5.21307191786773));
#74755=CARTESIAN_POINT('Ctrl Pts',(18.3999236699837,3.73433910932905,-3.83067634842202));
#74756=CARTESIAN_POINT('Ctrl Pts',(18.5191896424009,5.24197388553433,1.06821329948656));
#74757=CARTESIAN_POINT('Ctrl Pts',(18.638455614818,1.9375680581184,4.98650176877373));
#74758=CARTESIAN_POINT('Ctrl Pts',(18.7554569558387,-3.04897393187464,4.33978615214932));
#74759=CARTESIAN_POINT('Ctrl Pts',(18.8327029727204,-4.52425331147807,1.41328337976522));
#74760=CARTESIAN_POINT('Ctrl Pts',(18.870193665463,-4.53056695484048,-0.00156093939472799));
#74761=CARTESIAN_POINT('Ctrl Pts',(18.2680063345369,-4.53110217211561,-0.000654014894286977));
#74762=CARTESIAN_POINT('Ctrl Pts',(18.2689324527186,-4.53117262419495,-0.0355933401423199));
#74763=CARTESIAN_POINT('Ctrl Pts',(18.3096138950394,-4.51496105281763,-1.57030029484246));
#74764=CARTESIAN_POINT('Ctrl Pts',(18.3900506614992,-2.78874115530351,-4.5653360687384));
#74765=CARTESIAN_POINT('Ctrl Pts',(18.5093166339163,2.33079188008128,-4.81526529524129));
#74766=CARTESIAN_POINT('Ctrl Pts',(18.6285826063335,5.31069862001794,-0.644864961947463));
#74767=CARTESIAN_POINT('Ctrl Pts',(18.7478485787507,3.41547664867964,4.11751015956628));
#74768=CARTESIAN_POINT('Ctrl Pts',(18.8671145511678,-1.61509331810011,5.10008276654765));
#74769=CARTESIAN_POINT('Ctrl Pts',(18.9571671364299,-4.29399145827576,2.30696570578231));
#74770=CARTESIAN_POINT('Ctrl Pts',(19.0074643975529,-4.52583656589393,0.403853410488209));
#74771=CARTESIAN_POINT('Ctrl Pts',(19.0180063345369,-4.52228481540387,0.00412574957127487));
#74772=CARTESIAN_POINT('Origin',(-19.0048063345371,0.,0.));
#74773=CARTESIAN_POINT('',(17.370193665463,-4.51840654405581,0.00300719303878977));
#74774=CARTESIAN_POINT('',(17.5180063345369,-4.5203228109947,-0.00378289537507237));
#74775=CARTESIAN_POINT('',(-19.0048063345371,-4.52375,5.14627461305311E-12));
#74776=CARTESIAN_POINT('Ctrl Pts',(17.370193665463,-4.51840654405581,0.00300719303878934));
#74777=CARTESIAN_POINT('Ctrl Pts',(17.3953944071908,-4.51258082867698,-0.954623115859167));
#74778=CARTESIAN_POINT('Ctrl Pts',(17.4603504730576,-3.74558763789832,-3.43148573659885));
#74779=CARTESIAN_POINT('Ctrl Pts',(17.5650618630635,0.330015295393627,-5.33951868379825));
#74780=CARTESIAN_POINT('Ctrl Pts',(17.6843278354807,4.66916704311892,-2.61117770235508));
#74781=CARTESIAN_POINT('Ctrl Pts',(17.8035938078979,4.72210487845107,2.51417886927967));
#74782=CARTESIAN_POINT('Ctrl Pts',(17.922859780315,0.440232791824194,5.33156308776582));
#74783=CARTESIAN_POINT('Ctrl Pts',(18.0283930661701,-3.70620368291918,3.49380638893738));
#74784=CARTESIAN_POINT('Ctrl Pts',(18.0941710278861,-4.51232292376063,0.985148386060359));
#74785=CARTESIAN_POINT('Ctrl Pts',(18.120193665463,-4.51907785273017,-0.00334514387128795));
#74786=CARTESIAN_POINT('Ctrl Pts',(17.5180063345369,-4.5203228109947,-0.00378289537507182));
#74787=CARTESIAN_POINT('Ctrl Pts',(17.5304005078843,-4.52402898419069,-0.474260255155535));
#74788=CARTESIAN_POINT('Ctrl Pts',(17.5825500053707,-4.23969939200739,-2.44946365805436));
#74789=CARTESIAN_POINT('Ctrl Pts',(17.6744548269962,-1.37601144972682,-5.1697159633802));
#74790=CARTESIAN_POINT('Ctrl Pts',(17.7937207994134,3.60338472540743,-3.95411041480993));
#74791=CARTESIAN_POINT('Ctrl Pts',(17.9129867718305,5.27493656789836,0.891299532400152));
#74792=CARTESIAN_POINT('Ctrl Pts',(18.0322527442477,2.10418863924757,4.91851205368746));
#74793=CARTESIAN_POINT('Ctrl Pts',(18.1505925984831,-2.95854719837581,4.43440487545489));
#74794=CARTESIAN_POINT('Ctrl Pts',(18.2291771285795,-4.52814833927571,1.46424137628141));
#74795=CARTESIAN_POINT('Ctrl Pts',(18.2680063345369,-4.53110217211561,-0.000654014894286977));
#74796=CARTESIAN_POINT('Origin',(-19.0048063345371,0.,0.));
#74797=CARTESIAN_POINT('',(16.620193665463,-4.53005497334718,0.00207663933256817));
#74798=CARTESIAN_POINT('',(16.7680063345369,-4.51748974129652,0.00236132788964866));
#74799=CARTESIAN_POINT('',(-19.0048063345371,-4.52375,5.14627461305311E-12));
#74800=CARTESIAN_POINT('Ctrl Pts',(16.620193665463,-4.53005497334718,0.00207663933256816));
#74801=CARTESIAN_POINT('Ctrl Pts',(16.6568624623565,-4.52216716072903,-1.3821656394565));
#74802=CARTESIAN_POINT('Ctrl Pts',(16.733286583389,-3.10303436385726,-4.28114918944539));
#74803=CARTESIAN_POINT('Ctrl Pts',(16.8494660285605,1.83415837421399,-5.02545847939519));
#74804=CARTESIAN_POINT('Ctrl Pts',(16.9687320009777,5.21879159998521,-1.17625851994709));
#74805=CARTESIAN_POINT('Ctrl Pts',(17.0879979733949,3.81266515595566,3.75272624612899));
#74806=CARTESIAN_POINT('Ctrl Pts',(17.2072639458121,-1.09342140597902,5.23677376814878));
#74807=CARTESIAN_POINT('Ctrl Pts',(17.3013291765014,-4.17120591260208,2.61574616717072));
#74808=CARTESIAN_POINT('Ctrl Pts',(17.3556390830517,-4.52177116147468,0.556082550935958));
#74809=CARTESIAN_POINT('Ctrl Pts',(17.370193665463,-4.51840654405581,0.00300719303878934));
#74810=CARTESIAN_POINT('Ctrl Pts',(16.7680063345369,-4.51748974129652,0.00236132788964886));
#74811=CARTESIAN_POINT('Ctrl Pts',(16.79186856305,-4.51321097395483,-0.904866519473273));
#74812=CARTESIAN_POINT('Ctrl Pts',(16.855486115702,-3.80763549775125,-3.32969321608406));
#74813=CARTESIAN_POINT('Ctrl Pts',(16.9588589924932,0.150238344599186,-5.34759750650883));
#74814=CARTESIAN_POINT('Ctrl Pts',(17.0781249649104,4.57870057212474,-2.76674388453876));
#74815=CARTESIAN_POINT('Ctrl Pts',(17.1973909373275,4.80399552983808,2.35393236969624));
#74816=CARTESIAN_POINT('Ctrl Pts',(17.3166569097447,0.619306375843183,5.31373976260104));
#74817=CARTESIAN_POINT('Ctrl Pts',(17.4235287088145,-3.6399403872671,3.59495789521742));
#74818=CARTESIAN_POINT('Ctrl Pts',(17.4906451837452,-4.51214113071371,1.03483433420766));
#74819=CARTESIAN_POINT('Ctrl Pts',(17.5180063345369,-4.5203228109947,-0.00378289537507182));
#74820=CARTESIAN_POINT('Origin',(-19.0048063345371,0.,0.));
#74821=CARTESIAN_POINT('',(15.870193665463,-4.5247597024484,-0.0040964371096966));
#74822=CARTESIAN_POINT('',(16.0180063345369,-4.52898076399324,0.00282109434503318));
#74823=CARTESIAN_POINT('',(-19.0048063345371,-4.52375,5.14627461305311E-12));
#74824=CARTESIAN_POINT('Ctrl Pts',(15.870193665463,-4.5247597024484,-0.00409643710969645));
#74825=CARTESIAN_POINT('Ctrl Pts',(15.8785751933831,-4.52770537576116,-0.321462229303889));
#74826=CARTESIAN_POINT('Ctrl Pts',(15.9267120454422,-4.35232613711668,-2.14092699303294));
#74827=CARTESIAN_POINT('Ctrl Pts',(16.0146042216404,-1.88949625357401,-5.00491496207014));
#74828=CARTESIAN_POINT('Ctrl Pts',(16.1338701940576,3.18698452797358,-4.2968010761823));
#74829=CARTESIAN_POINT('Ctrl Pts',(16.2531361664747,5.33786909584254,0.355701258745961));
#74830=CARTESIAN_POINT('Ctrl Pts',(16.3724021388919,2.58868292949964,4.68167604179753));
#74831=CARTESIAN_POINT('Ctrl Pts',(16.4916681113091,-2.53686901787644,4.70995386983385));
#74832=CARTESIAN_POINT('Ctrl Pts',(16.5742652868328,-4.47374742312347,1.73520711701237));
#74833=CARTESIAN_POINT('Ctrl Pts',(16.6171071382174,-4.5307189151892,0.118592638491145));
#74834=CARTESIAN_POINT('Ctrl Pts',(16.620193665463,-4.53005497334718,0.00207663933256816));
#74835=CARTESIAN_POINT('Ctrl Pts',(16.0180063345369,-4.52898076399324,0.0028210943450329));
#74836=CARTESIAN_POINT('Ctrl Pts',(16.0533366182156,-4.51924456004213,-1.33172626091404));
#74837=CARTESIAN_POINT('Ctrl Pts',(16.1284222260334,-3.18871039908969,-4.18484263335493));
#74838=CARTESIAN_POINT('Ctrl Pts',(16.2432631579902,1.66409356894118,-5.08430558145515));
#74839=CARTESIAN_POINT('Ctrl Pts',(16.3625291304074,5.17627646950703,-1.35112270465559));
#74840=CARTESIAN_POINT('Ctrl Pts',(16.4817951028246,3.93672784856066,3.62236725059386));
#74841=CARTESIAN_POINT('Ctrl Pts',(16.6010610752417,-0.916668278371397,
5.27058724614582));
#74842=CARTESIAN_POINT('Ctrl Pts',(16.6964648191458,-4.12589289623653,2.71875914615102));
#74843=CARTESIAN_POINT('Ctrl Pts',(16.7521132389109,-4.52033955301825,0.606607445339812));
#74844=CARTESIAN_POINT('Ctrl Pts',(16.7680063345369,-4.51748974129652,0.00236132788964886));
#74845=CARTESIAN_POINT('Origin',(-19.0048063345371,0.,0.));
#74846=CARTESIAN_POINT('',(15.120193665463,-4.51627216358632,-1.76542077389561E-5));
#74847=CARTESIAN_POINT('',(15.2680063345369,-4.52629070818003,-0.00383690431508932));
#74848=CARTESIAN_POINT('',(-19.0048063345371,-4.52375,5.14627461305311E-12));
#74849=CARTESIAN_POINT('Ctrl Pts',(15.120193665463,-4.51627223874174,-1.76540303067213E-5));
#74850=CARTESIAN_POINT('Ctrl Pts',(15.1400432485488,-4.51629844318397,-0.755195211199893));
#74851=CARTESIAN_POINT('Ctrl Pts',(15.1996481557736,-3.97854876929622,-3.02282933081675));
#74852=CARTESIAN_POINT('Ctrl Pts',(15.2990083871374,-0.388909991241378,
-5.33555235083833));
#74853=CARTESIAN_POINT('Ctrl Pts',(15.4182743595546,4.27688644041953,-3.21366025671349));
#74854=CARTESIAN_POINT('Ctrl Pts',(15.5375403319717,5.01657571134664,1.85831590483193));
#74855=CARTESIAN_POINT('Ctrl Pts',(15.6568063043889,1.15113597147179,5.22439047593186));
#74856=CARTESIAN_POINT('Ctrl Pts',(15.767690748886,-3.42511693477894,3.8950479816348));
#74857=CARTESIAN_POINT('Ctrl Pts',(15.838819869244,-4.51373343669785,1.18386950252823));
#74858=CARTESIAN_POINT('Ctrl Pts',(15.870193665463,-4.5247597024484,-0.00409643710969645));
#74859=CARTESIAN_POINT('Ctrl Pts',(15.2680063345369,-4.52629070818003,-0.0038369043150898));
#74860=CARTESIAN_POINT('Ctrl Pts',(15.2750493492422,-4.52869797060996,-0.270287775271952));
#74861=CARTESIAN_POINT('Ctrl Pts',(15.3218476880866,-4.38585365861661,-2.03818147109467));
#74862=CARTESIAN_POINT('Ctrl Pts',(15.4084013510701,-2.05676334484598,-4.93853168412494));
#74863=CARTESIAN_POINT('Ctrl Pts',(15.5276673234872,3.0406621088803,-4.40156160827348));
#74864=CARTESIAN_POINT('Ctrl Pts',(15.6469332959044,5.34681277770121,0.175965257988861));
#74865=CARTESIAN_POINT('Ctrl Pts',(15.7661992683216,2.74468256834738,4.5919590863615));
#74866=CARTESIAN_POINT('Ctrl Pts',(15.8854652407387,-2.3770183697707,4.79261456008932));
#74867=CARTESIAN_POINT('Ctrl Pts',(15.9694009294772,-4.44584540992525,1.83757239306991));
#74868=CARTESIAN_POINT('Ctrl Pts',(16.0135812940766,-4.53020020216151,0.169970220487411));
#74869=CARTESIAN_POINT('Ctrl Pts',(16.0180063345369,-4.52898076399324,0.0028210943450329));
#74870=CARTESIAN_POINT('Origin',(-19.0048063345371,0.,0.));
#74871=CARTESIAN_POINT('',(14.370193665463,-4.52469469919503,0.00410328708299658));
#74872=CARTESIAN_POINT('',(14.5180063345369,-4.51641831892787,-0.00085334569348311));
#74873=CARTESIAN_POINT('',(-19.0048063345371,-4.52375,5.14627461305311E-12));
#74874=CARTESIAN_POINT('Ctrl Pts',(14.370193665463,-4.52469469919503,0.0041032870829967));
#74875=CARTESIAN_POINT('Ctrl Pts',(14.4015113037144,-4.51368577701503,-1.18177995784863));
#74876=CARTESIAN_POINT('Ctrl Pts',(14.4725842661049,-3.4282942933837,-3.89088640352849));
#74877=CARTESIAN_POINT('Ctrl Pts',(14.5834125526344,1.14376110347399,-5.22600998927515));
#74878=CARTESIAN_POINT('Ctrl Pts',(14.7026785250516,5.01394788167348,-1.86539446490182));
#74879=CARTESIAN_POINT('Ctrl Pts',(14.8219444974688,4.28141795087999,3.20762064460667));
#74880=CARTESIAN_POINT('Ctrl Pts',(14.9412104698859,-0.381378988217642,
5.33609594527402));
#74881=CARTESIAN_POINT('Ctrl Pts',(15.0406268592173,-3.97630906655061,3.02713738035306));
#74882=CARTESIAN_POINT('Ctrl Pts',(15.1002879244097,-4.51624596016253,0.757296433492399));
#74883=CARTESIAN_POINT('Ctrl Pts',(15.120193665463,-4.51627223874174,-1.76540303067213E-5));
#74884=CARTESIAN_POINT('Ctrl Pts',(14.5180063345369,-4.51641831892787,-0.000853345693483179));
#74885=CARTESIAN_POINT('Ctrl Pts',(14.5365174044079,-4.5176016717366,-0.705050397317584));
#74886=CARTESIAN_POINT('Ctrl Pts',(14.594783798418,-4.03068622056879,-2.9200681878472));
#74887=CARTESIAN_POINT('Ctrl Pts',(14.6928055165671,-0.568146787928893,
-5.31945296803855));
#74888=CARTESIAN_POINT('Ctrl Pts',(14.8120714889842,4.16637791607122,-3.35569154009744));
#74889=CARTESIAN_POINT('Ctrl Pts',(14.9313374614014,5.07624035735161,1.68853619629629));
#74890=CARTESIAN_POINT('Ctrl Pts',(15.0506034338186,1.32620268338616,5.18271715361618));
#74891=CARTESIAN_POINT('Ctrl Pts',(15.1628263915304,-3.3479219489578,3.99386544736847));
#74892=CARTESIAN_POINT('Ctrl Pts',(15.2352940251032,-4.51510982658446,1.23373304325699));
#74893=CARTESIAN_POINT('Ctrl Pts',(15.2680063345369,-4.52629070818003,-0.0038369043150898));
#74894=CARTESIAN_POINT('Origin',(-19.0048063345371,0.,0.));
#74895=CARTESIAN_POINT('',(13.620193665463,-4.53009387229811,-0.00204267091282001));
#74896=CARTESIAN_POINT('',(13.7680063345369,-4.52314995435732,0.00416998364050888));
#74897=CARTESIAN_POINT('',(-19.0048063345371,-4.52375,5.14627461305311E-12));
#74898=CARTESIAN_POINT('Ctrl Pts',(13.620193665463,-4.53009387229811,-0.00204267091282042));
#74899=CARTESIAN_POINT('Ctrl Pts',(13.623224034741,-4.53073677915691,-0.116436113594865));
#74900=CARTESIAN_POINT('Ctrl Pts',(13.6660097281581,-4.47487801284166,-1.73091551955723));
#74901=CARTESIAN_POINT('Ctrl Pts',(13.7485507457143,-2.54351413503901,-4.70636863353064));
#74902=CARTESIAN_POINT('Ctrl Pts',(13.8678167181314,2.58207261855057,-4.68532505407631));
#74903=CARTESIAN_POINT('Ctrl Pts',(13.9870826905486,5.33736174127025,-0.363234789975878));
#74904=CARTESIAN_POINT('Ctrl Pts',(14.1063486629658,3.19304587242686,4.29229867628082));
#74905=CARTESIAN_POINT('Ctrl Pts',(14.2256146353829,-1.88243041858965,5.00757681808199));
#74906=CARTESIAN_POINT('Ctrl Pts',(14.3135629695487,-4.35087627651381,2.14524004940141));
#74907=CARTESIAN_POINT('Ctrl Pts',(14.3617559795754,-4.52766075386909,0.323607275213117));
#74908=CARTESIAN_POINT('Ctrl Pts',(14.370193665463,-4.52469469919503,0.0041032870829967));
#74909=CARTESIAN_POINT('Ctrl Pts',(13.7680063345369,-4.52314995435732,0.00416998364050923));
#74910=CARTESIAN_POINT('Ctrl Pts',(13.7979854595736,-4.5127764880711,-1.1320207248508));
#74911=CARTESIAN_POINT('Ctrl Pts',(13.8677199087493,-3.502576575626,-3.79135010209604));
#74912=CARTESIAN_POINT('Ctrl Pts',(13.9772096820641,0.96734152561576,-5.26152269068825));
#74913=CARTESIAN_POINT('Ctrl Pts',(14.0964756544813,4.94837013659463,-2.03297900704013));
#74914=CARTESIAN_POINT('Ctrl Pts',(14.2157416268984,4.38688126484615,3.06180394864691));
#74915=CARTESIAN_POINT('Ctrl Pts',(14.3350075993156,-0.201688098081399,
5.3459042792497));
#74916=CARTESIAN_POINT('Ctrl Pts',(14.4357625018617,-3.92166343592592,3.12972290055515));
#74917=CARTESIAN_POINT('Ctrl Pts',(14.4967620802688,-4.5150602424832,0.807319349011126));
#74918=CARTESIAN_POINT('Ctrl Pts',(14.5180063345369,-4.51641831892787,-0.000853345693483179));
#74919=CARTESIAN_POINT('Origin',(-19.0048063345371,0.,0.));
#74920=CARTESIAN_POINT('',(12.870193665463,-4.51844992363578,-0.00303181240373236));
#74921=CARTESIAN_POINT('',(13.0180063345369,-4.53084488398297,-0.00118107851521998));
#74922=CARTESIAN_POINT('',(-19.0048063345371,-4.52375,5.14627461305311E-12));
#74923=CARTESIAN_POINT('Ctrl Pts',(12.870193665463,-4.51844992363578,-0.00303181240373214));
#74924=CARTESIAN_POINT('Ctrl Pts',(12.8846920899067,-4.52183101233865,-0.553959891712047));
#74925=CARTESIAN_POINT('Ctrl Pts',(12.9389458384895,-4.1730583699505,-2.61142368232673));
#74926=CARTESIAN_POINT('Ctrl Pts',(13.0329549112113,-1.10081151614861,-5.23522529369453));
#74927=CARTESIAN_POINT('Ctrl Pts',(13.1522208836285,3.80736474859714,-3.75810371609987));
#74928=CARTESIAN_POINT('Ctrl Pts',(13.2714868560456,5.22044657695045,1.16889152919789));
#74929=CARTESIAN_POINT('Ctrl Pts',(13.3907528284628,1.84124949551275,5.02286473689053));
#74930=CARTESIAN_POINT('Ctrl Pts',(13.5069884316019,-3.09937585488682,4.28516814783659));
#74931=CARTESIAN_POINT('Ctrl Pts',(13.583468710602,-4.52230250325925,1.38428804770569));
#74932=CARTESIAN_POINT('Ctrl Pts',(13.620193665463,-4.53009387229811,-0.00204267091282042));
#74933=CARTESIAN_POINT('Ctrl Pts',(13.0180063345369,-4.53084488398297,-0.00118107851522056));
#74934=CARTESIAN_POINT('Ctrl Pts',(13.0196981906002,-4.53106719519265,-0.0650188296293057));
#74935=CARTESIAN_POINT('Ctrl Pts',(13.0611453708025,-4.5008850794886,-1.62870450993968));
#74936=CARTESIAN_POINT('Ctrl Pts',(13.1423478751439,-2.70036984388385,-4.61815692219858));
#74937=CARTESIAN_POINT('Ctrl Pts',(13.2616138475611,2.42302476496527,-4.76952006392394));
#74938=CARTESIAN_POINT('Ctrl Pts',(13.3808798199783,5.32212489864176,-0.542546970376561));
#74939=CARTESIAN_POINT('Ctrl Pts',(13.5001457923954,3.33560719654819,4.18247477961839));
#74940=CARTESIAN_POINT('Ctrl Pts',(13.6194117648126,-1.71293973690343,5.06805762689664));
#74941=CARTESIAN_POINT('Ctrl Pts',(13.7086986121931,-4.31527330193496,2.2480898219303));
#74942=CARTESIAN_POINT('Ctrl Pts',(13.7582301354345,-4.52653274393746,0.374682017293747));
#74943=CARTESIAN_POINT('Ctrl Pts',(13.7680063345369,-4.52314995435732,0.00416998364050923));
#74944=CARTESIAN_POINT('Origin',(-19.0048063345371,0.,0.));
#74945=CARTESIAN_POINT('',(12.120193665463,-4.51902956961554,0.00332363250920302));
#74946=CARTESIAN_POINT('',(12.2680063345369,-4.51958929800233,-0.00355049372932015));
#74947=CARTESIAN_POINT('',(-19.0048063345371,-4.52375,5.14627461305311E-12));
#74948=CARTESIAN_POINT('Ctrl Pts',(12.120193665463,-4.51902956961554,0.00332363250920252));
#74949=CARTESIAN_POINT('Ctrl Pts',(12.1461601450724,-4.51233717109749,-0.983063180516055));
#74950=CARTESIAN_POINT('Ctrl Pts',(12.2118819488208,-3.7089260789378,-3.48955300938175));
#74951=CARTESIAN_POINT('Ctrl Pts',(12.3173590767083,0.432707368140066,-5.33217912333988));
#74952=CARTESIAN_POINT('Ctrl Pts',(12.4366250491255,4.71855165499341,-2.52084115901474));
#74953=CARTESIAN_POINT('Ctrl Pts',(12.5558910215426,4.67284781705142,2.6045850242413));
#74954=CARTESIAN_POINT('Ctrl Pts',(12.6751569939598,0.337551180441248,5.33904758083378));
#74955=CARTESIAN_POINT('Ctrl Pts',(12.7799245419332,-3.74292793381757,3.43574863833749));
#74956=CARTESIAN_POINT('Ctrl Pts',(12.8449367657677,-4.51255991685876,0.95670938516384));
#74957=CARTESIAN_POINT('Ctrl Pts',(12.870193665463,-4.51844992363578,-0.00303181240373214));
#74958=CARTESIAN_POINT('Ctrl Pts',(12.2680063345369,-4.51958929800233,-0.00355049372931973));
#74959=CARTESIAN_POINT('Ctrl Pts',(12.2811662457659,-4.52324203005514,-0.503299371711655));
#74960=CARTESIAN_POINT('Ctrl Pts',(12.3340814811339,-4.21606861625357,-2.50839703100191));
#74961=CARTESIAN_POINT('Ctrl Pts',(12.4267520406409,-1.27627112038846,-5.19523846219496));
#74962=CARTESIAN_POINT('Ctrl Pts',(12.5460180130581,3.67880996828069,-3.88403499843739));
#74963=CARTESIAN_POINT('Ctrl Pts',(12.6652839854753,5.25680766681221,0.992644853889018));
#74964=CARTESIAN_POINT('Ctrl Pts',(12.7845499578925,2.00914760921968,4.95809404269169));
#74965=CARTESIAN_POINT('Ctrl Pts',(12.9021240742463,-3.01064165969237,4.38041204226545));
#74966=CARTESIAN_POINT('Ctrl Pts',(12.9799428664611,-4.52584331451383,1.43504405569548));
#74967=CARTESIAN_POINT('Ctrl Pts',(13.0180063345369,-4.53084488398297,-0.00118107851522056));
#74968=CARTESIAN_POINT('Origin',(-19.0048063345371,0.,0.));
#74969=CARTESIAN_POINT('',(11.370193665463,-4.53053606468118,0.00159735848326331));
#74970=CARTESIAN_POINT('',(11.5180063345369,-4.5179861772387,0.00274417767465035));
#74971=CARTESIAN_POINT('',(-19.0048063345371,-4.52375,5.14627461305311E-12));
#74972=CARTESIAN_POINT('Ctrl Pts',(11.370193665463,-4.53053606468118,0.00159735848326391));
#74973=CARTESIAN_POINT('Ctrl Pts',(11.4076282002381,-4.52410350302755,-1.41115327369312));
#74974=CARTESIAN_POINT('Ctrl Pts',(11.4848180591522,-3.05270309746021,-4.3357922845143));
#74975=CARTESIAN_POINT('Ctrl Pts',(11.6017632422053,1.93052816369304,-4.98923149182437));
#74976=CARTESIAN_POINT('Ctrl Pts',(11.7210292146225,5.24046098470274,-1.07561077422649));
#74977=CARTESIAN_POINT('Ctrl Pts',(11.8402951870396,3.73974201866875,3.8254018747875));
#74978=CARTESIAN_POINT('Ctrl Pts',(11.9595611594568,-1.1939948970662,5.21476232014501));
#74979=CARTESIAN_POINT('Ctrl Pts',(12.0528606522646,-4.19613118865777,2.55680616480241));
#74980=CARTESIAN_POINT('Ctrl Pts',(12.1064048209333,-4.52258339917136,0.52711948837973));
#74981=CARTESIAN_POINT('Ctrl Pts',(12.120193665463,-4.51902956961554,0.00332363250920252));
#74982=CARTESIAN_POINT('Ctrl Pts',(11.5180063345369,-4.5179861772387,0.00274417767465021));
#74983=CARTESIAN_POINT('Ctrl Pts',(11.5426343009315,-4.51282034450835,-0.933338999714355));
#74984=CARTESIAN_POINT('Ctrl Pts',(11.6070175914652,-3.77245439838875,-3.38796966408972));
#74985=CARTESIAN_POINT('Ctrl Pts',(11.711156206138,0.25311917672245,-5.34371606040058));
#74986=CARTESIAN_POINT('Ctrl Pts',(11.8304221785551,4.63109563736341,-2.67811946137613));
#74987=CARTESIAN_POINT('Ctrl Pts',(11.9496881509723,4.7578070721057,2.44594409511522));
#74988=CARTESIAN_POINT('Ctrl Pts',(12.0689541233894,0.51693459378251,5.32467363108372));
#74989=CARTESIAN_POINT('Ctrl Pts',(12.1750601845777,-3.67817244537976,3.53714560518498));
#74990=CARTESIAN_POINT('Ctrl Pts',(12.2414109216268,-4.5122073396058,1.00641283581426));
#74991=CARTESIAN_POINT('Ctrl Pts',(12.2680063345369,-4.51958929800233,-0.00355049372931973));
#74992=CARTESIAN_POINT('Origin',(-19.0048063345371,0.,0.));
#74993=CARTESIAN_POINT('',(10.620193665463,-4.52387319312239,-0.00416168075873038));
#74994=CARTESIAN_POINT('',(10.7680063345369,-4.52962834834061,0.00241115988119614));
#74995=CARTESIAN_POINT('',(-19.0048063345371,-4.52375,5.14627461305311E-12));
#74996=CARTESIAN_POINT('Ctrl Pts',(10.620193665463,-4.52387319312239,-0.00416168075873042));
#74997=CARTESIAN_POINT('Ctrl Pts',(10.6293409312647,-4.52707769761145,-0.350695986930693));
#74998=CARTESIAN_POINT('Ctrl Pts',(10.6782435212054,-4.33225334002266,-2.19975205777105));
#74999=CARTESIAN_POINT('Ctrl Pts',(10.7669014352852,-1.79283225123103,-5.04034943121707));
#75000=CARTESIAN_POINT('Ctrl Pts',(10.8861674077023,3.26908158649335,-4.23467536544114));
#75001=CARTESIAN_POINT('Ctrl Pts',(11.0054333801195,5.3300355426419,0.458356830425908));
#75002=CARTESIAN_POINT('Ctrl Pts',(11.1246993525366,2.49810982979476,4.73062544999149));
#75003=CARTESIAN_POINT('Ctrl Pts',(11.2439653249538,-2.62703713820798,4.66026241152792));
#75004=CARTESIAN_POINT('Ctrl Pts',(11.3257967625959,-4.48888884709553,1.6767120036351));
#75005=CARTESIAN_POINT('Ctrl Pts',(11.367872876099,-4.53093485742053,0.0891821691630021));
#75006=CARTESIAN_POINT('Ctrl Pts',(11.370193665463,-4.53053606468118,0.00159735848326391));
#75007=CARTESIAN_POINT('Ctrl Pts',(10.7680063345369,-4.52962834834061,0.00241115988119607));
#75008=CARTESIAN_POINT('Ctrl Pts',(10.8041023560972,-4.5208459704019,-1.36054807436645));
#75009=CARTESIAN_POINT('Ctrl Pts',(10.8799537017966,-3.14005421280247,-4.24005726281787));
#75010=CARTESIAN_POINT('Ctrl Pts',(10.995560371635,1.76162729918915,-5.05134040731361));
#75011=CARTESIAN_POINT('Ctrl Pts',(11.1148263440521,5.20131879681764,-1.2512607344911));
#75012=CARTESIAN_POINT('Ctrl Pts',(11.2340923164693,3.86629035321667,3.69745446982539));
#75013=CARTESIAN_POINT('Ctrl Pts',(11.3533582888864,-1.01792520411819,5.25197095675792));
#75014=CARTESIAN_POINT('Ctrl Pts',(11.447996294909,-4.15208915750858,2.65983099715797));
#75015=CARTESIAN_POINT('Ctrl Pts',(11.5028789767925,-4.52115921225539,0.577719182756343));
#75016=CARTESIAN_POINT('Ctrl Pts',(11.5180063345369,-4.5179861772387,0.00274417767465021));
#75017=CARTESIAN_POINT('Origin',(-19.0048063345371,0.,0.));
#75018=CARTESIAN_POINT('',(9.87019366546302,-4.51631481829542,0.000462863536248687));
#75019=CARTESIAN_POINT('',(10.0180063345369,-4.52542048575924,-0.0040079242928287));
#75020=CARTESIAN_POINT('',(-19.0048063345371,-4.52375,5.14627461305311E-12));
#75021=CARTESIAN_POINT('Ctrl Pts',(9.87019366546302,-4.51631481829542,0.000462863536248928));
#75022=CARTESIAN_POINT('Ctrl Pts',(9.89080898643035,-4.51560089924546,-0.783828764199309));
#75023=CARTESIAN_POINT('Ctrl Pts',(9.95117963153673,-3.94764305999575,-3.08154461394558));
#75024=CARTESIAN_POINT('Ctrl Pts',(10.0513056007822,-0.286161114873556,
-5.34204845411932));
#75025=CARTESIAN_POINT('Ctrl Pts',(10.1705715731993,4.33793781171498,-3.13076115529714));
#75026=CARTESIAN_POINT('Ctrl Pts',(10.2898375456165,4.97988548349452,1.95451028165742));
#75027=CARTESIAN_POINT('Ctrl Pts',(10.4091035180337,1.05038513373988,5.24557536793082));
#75028=CARTESIAN_POINT('Ctrl Pts',(10.5192222246492,-3.46801874972811,3.83820060209342));
#75029=CARTESIAN_POINT('Ctrl Pts',(10.5895856071256,-4.51315046324109,1.15539162065489));
#75030=CARTESIAN_POINT('Ctrl Pts',(10.620193665463,-4.52387319312239,-0.00416168075873042));
#75031=CARTESIAN_POINT('Ctrl Pts',(10.0180063345369,-4.52542048575924,-0.00400792429282804));
#75032=CARTESIAN_POINT('Ctrl Pts',(10.0258150871238,-4.52814717979581,-0.299574684771682));
#75033=CARTESIAN_POINT('Ctrl Pts',(10.0733791638498,-4.3669142806853,-2.09694694671342));
#75034=CARTESIAN_POINT('Ctrl Pts',(10.1606985647148,-1.96134584123722,-4.97719731805657));
#75035=CARTESIAN_POINT('Ctrl Pts',(10.279964537132,3.12480226517166,-4.34223231246161));
#75036=CARTESIAN_POINT('Ctrl Pts',(10.3992305095491,5.34243639065652,0.278826224728918));
#75037=CARTESIAN_POINT('Ctrl Pts',(10.5184964819663,2.65580708494681,4.64392715052188));
#75038=CARTESIAN_POINT('Ctrl Pts',(10.6377624543835,-2.46880680580944,4.74598394512631));
#75039=CARTESIAN_POINT('Ctrl Pts',(10.7209324052403,-4.46203274740751,1.77899348776185));
#75040=CARTESIAN_POINT('Ctrl Pts',(10.7643470319582,-4.53051867854459,0.140583734725522));
#75041=CARTESIAN_POINT('Ctrl Pts',(10.7680063345369,-4.52962834834061,0.00241115988119607));
#75042=CARTESIAN_POINT('Origin',(-19.0048063345371,0.,0.));
#75043=CARTESIAN_POINT('',(9.12019366546302,-4.52557728081363,0.00398177268663652));
#75044=CARTESIAN_POINT('',(9.26800633453692,-4.5163005375385,-0.000377275191646986));
#75045=CARTESIAN_POINT('',(-19.0048063345371,-4.52375,5.14627461305311E-12));
#75046=CARTESIAN_POINT('Ctrl Pts',(9.12019366546302,-4.52557728081363,0.00398177268663646));
#75047=CARTESIAN_POINT('Ctrl Pts',(9.15227704159602,-4.5144046866037,-1.21028811178658));
#75048=CARTESIAN_POINT('Ctrl Pts',(9.22411574186808,-3.38454463484326,-3.94752458958706));
#75049=CARTESIAN_POINT('Ctrl Pts',(9.33570976627918,1.24411813547422,-5.20303180220995));
#75050=CARTESIAN_POINT('Ctrl Pts',(9.45497573869635,5.04891686558556,-1.76856109711541));
#75051=CARTESIAN_POINT('Ctrl Pts',(9.57424171111352,4.21889796935353,3.28941785032073));
#75052=CARTESIAN_POINT('Ctrl Pts',(9.69350768353068,-0.483995682528848,
5.32776858066465));
#75053=CARTESIAN_POINT('Ctrl Pts',(9.79215833498051,-4.00648469947538,2.96837102108853));
#75054=CARTESIAN_POINT('Ctrl Pts',(9.85105366229129,-4.51697764633978,0.728627332389643));
#75055=CARTESIAN_POINT('Ctrl Pts',(9.87019366546302,-4.51631481829542,0.000462863536248928));
#75056=CARTESIAN_POINT('Ctrl Pts',(9.26800633453692,-4.5163005375385,-0.000377275191646917));
#75057=CARTESIAN_POINT('Ctrl Pts',(9.2872831422895,-4.51684456770769,-0.733752169377256));
#75058=CARTESIAN_POINT('Ctrl Pts',(9.34631527418114,-4.0011510798866,-2.97887378297804));
#75059=CARTESIAN_POINT('Ctrl Pts',(9.44510273021184,-0.46567453527804,-5.32940126834165));
#75060=CARTESIAN_POINT('Ctrl Pts',(9.56436870262899,4.23018298784551,-3.27489275261803));
#75061=CARTESIAN_POINT('Ctrl Pts',(9.68363467504617,5.04280630516079,1.78591019383345));
#75062=CARTESIAN_POINT('Ctrl Pts',(9.80290064746333,1.2262213840307,5.20727872973531));
#75063=CARTESIAN_POINT('Ctrl Pts',(9.91435786729357,-3.39242830756635,3.93742298437625));
#75064=CARTESIAN_POINT('Ctrl Pts',(9.98605976298477,-4.51426524359083,1.20519220811969));
#75065=CARTESIAN_POINT('Ctrl Pts',(10.0180063345369,-4.52542048575924,-0.00400792429282804));
#75066=CARTESIAN_POINT('Origin',(-19.0048063345371,0.,0.));
#75067=CARTESIAN_POINT('',(8.37019366546303,-4.52951872580807,-0.00248766312977575));
#75068=CARTESIAN_POINT('',(8.51800633453692,-4.52403144532135,0.00415447988692308));
#75069=CARTESIAN_POINT('',(-19.0048063345371,-4.52375,5.14627461305311E-12));
#75070=CARTESIAN_POINT('Ctrl Pts',(8.37019366546303,-4.52951872580807,-0.00248766312977579));
#75071=CARTESIAN_POINT('Ctrl Pts',(8.37398977262264,-4.53046593894472,-0.14583501537258));
#75072=CARTESIAN_POINT('Ctrl Pts',(8.41754120392131,-4.45918503465124,-1.78945556809376));
#75073=CARTESIAN_POINT('Ctrl Pts',(8.50084795935902,-2.4524742178731,-4.75444424517648));
#75074=CARTESIAN_POINT('Ctrl Pts',(8.6201139317762,2.67175841346331,-4.63476826280582));
#75075=CARTESIAN_POINT('Ctrl Pts',(8.73937990419336,5.34336341837622,-0.260455848433275));
#75076=CARTESIAN_POINT('Ctrl Pts',(8.85864587661052,3.10985399681577,4.35295049228831));
#75077=CARTESIAN_POINT('Ctrl Pts',(8.97791184902769,-1.97844715602509,4.97042419926512));
#75078=CARTESIAN_POINT('Ctrl Pts',(9.06509444531185,-4.37034497134543,2.08644536657521));
#75079=CARTESIAN_POINT('Ctrl Pts',(9.11252171745696,-4.52824893112611,0.294344463332979));
#75080=CARTESIAN_POINT('Ctrl Pts',(9.12019366546302,-4.52557728081363,0.00398177268663646));
#75081=CARTESIAN_POINT('Ctrl Pts',(8.51800633453692,-4.52403144532135,0.00415447988692291));
#75082=CARTESIAN_POINT('Ctrl Pts',(8.54875119745517,-4.51324421933796,-1.1604773474593));
#75083=CARTESIAN_POINT('Ctrl Pts',(8.61925138451249,-3.46042089846282,-3.84837281968134));
#75084=CARTESIAN_POINT('Ctrl Pts',(8.72950689570885,1.06841463020081,-5.2419329287755));
#75085=CARTESIAN_POINT('Ctrl Pts',(8.848772868126,4.98657624511604,-1.93737657760491));
#75086=CARTESIAN_POINT('Ctrl Pts',(8.96803884054318,4.32714783601959,3.14565768274914));
#75087=CARTESIAN_POINT('Ctrl Pts',(9.08730481296034,-0.304526818381393,
5.34103305257461));
#75088=CARTESIAN_POINT('Ctrl Pts',(9.18729397762492,-3.95322283016004,3.07105915382242));
#75089=CARTESIAN_POINT('Ctrl Pts',(9.24752781815045,-4.51572259274196,0.778715922228201));
#75090=CARTESIAN_POINT('Ctrl Pts',(9.26800633453692,-4.5163005375385,-0.000377275191646917));
#75091=CARTESIAN_POINT('Origin',(-19.0048063345371,0.,0.));
#75092=CARTESIAN_POINT('',(7.62019366546304,-4.51789179120342,-0.00267828408389951));
#75093=CARTESIAN_POINT('',(7.76800633453693,-4.53045826813502,-0.00168539955221481));
#75094=CARTESIAN_POINT('',(-19.0048063345371,-4.52375,5.14627461305311E-12));
#75095=CARTESIAN_POINT('Ctrl Pts',(7.62019366546304,-4.51789179120342,-0.00267828408389924));
#75096=CARTESIAN_POINT('Ctrl Pts',(7.63545782778832,-4.52101270627242,-0.582883426044371));
#75097=CARTESIAN_POINT('Ctrl Pts',(7.69047731425265,-4.14746281599376,-2.67035974633324));
#75098=CARTESIAN_POINT('Ctrl Pts',(7.78525212485605,-0.999861493359396,
-5.25543974029968));
#75099=CARTESIAN_POINT('Ctrl Pts',(7.90451809727322,3.87898028412496,-3.68413922445854));
#75100=CARTESIAN_POINT('Ctrl Pts',(8.02378406969037,5.19698581262198,1.26913684574598));
#75101=CARTESIAN_POINT('Ctrl Pts',(8.14305004210754,1.74424900381116,5.05736742609511));
#75102=CARTESIAN_POINT('Ctrl Pts',(8.25851990736508,-3.14881692963313,4.23021577656234));
#75103=CARTESIAN_POINT('Ctrl Pts',(8.33423444848359,-4.52054610167646,1.35539248250157));
#75104=CARTESIAN_POINT('Ctrl Pts',(8.37019366546303,-4.52951872580807,-0.00248766312977579));
#75105=CARTESIAN_POINT('Ctrl Pts',(7.76800633453693,-4.53045826813502,-0.00168539955221455));
#75106=CARTESIAN_POINT('Ctrl Pts',(7.77046392848179,-4.53090073763734,-0.0944373503981022));
#75107=CARTESIAN_POINT('Ctrl Pts',(7.81267684656572,-4.48622713824118,-1.68715899213078));
#75108=CARTESIAN_POINT('Ctrl Pts',(7.89464508878868,-2.6109984177212,-4.66926738519707));
#75109=CARTESIAN_POINT('Ctrl Pts',(8.01391106120587,2.51436025322183,-4.72200838296865));
#75110=CARTESIAN_POINT('Ctrl Pts',(8.13317703362301,5.33158006372075,-0.440028039951035));
#75111=CARTESIAN_POINT('Ctrl Pts',(8.25244300604019,3.25450236181101,4.2458903693777));
#75112=CARTESIAN_POINT('Ctrl Pts',(8.37170897845735,-1.81015174768696,5.0341554705982));
#75113=CARTESIAN_POINT('Ctrl Pts',(8.46023008795626,-4.33588773946907,2.18924030229226));
#75114=CARTESIAN_POINT('Ctrl Pts',(8.50899587331612,-4.5271928801816,0.345475563175432));
#75115=CARTESIAN_POINT('Ctrl Pts',(8.51800633453692,-4.52403144532135,0.00415447988692291));
#75116=CARTESIAN_POINT('Origin',(-19.0048063345371,0.,0.));
#75117=CARTESIAN_POINT('',(6.87019366546302,-4.51971627441788,0.00359563931439616));
#75118=CARTESIAN_POINT('',(7.01800633453693,-4.51891345091625,-0.00327023183485431));
#75119=CARTESIAN_POINT('',(-19.0048063345371,-4.52375,5.14627461305311E-12));
#75120=CARTESIAN_POINT('Ctrl Pts',(6.87019366546302,-4.51971627441788,0.0035956393143962));
#75121=CARTESIAN_POINT('Ctrl Pts',(6.89692588295397,-4.51218785835947,-1.01149097213452));
#75122=CARTESIAN_POINT('Ctrl Pts',(6.96341342458398,-3.67140572599566,-3.54748510584191));
#75123=CARTESIAN_POINT('Ctrl Pts',(7.06965629035308,0.535239182461503,-5.32286472563243));
#75124=CARTESIAN_POINT('Ctrl Pts',(7.18892226277021,4.76618869399877,-2.42957099155845));
#75125=CARTESIAN_POINT('Ctrl Pts',(7.3081882351874,4.62186010975348,2.69402653953035));
#75126=CARTESIAN_POINT('Ctrl Pts',(7.42745420760454,0.234744552882073,5.34455469283609));
#75127=CARTESIAN_POINT('Ctrl Pts',(7.53145601769645,-3.7788013523074,3.37756627327991));
#75128=CARTESIAN_POINT('Ctrl Pts',(7.59570250364927,-4.51288432113509,0.928253771938683));
#75129=CARTESIAN_POINT('Ctrl Pts',(7.62019366546304,-4.51789179120342,-0.00267828408389924));
#75130=CARTESIAN_POINT('Ctrl Pts',(7.01800633453693,-4.51891345091625,-0.00327023183485403));
#75131=CARTESIAN_POINT('Ctrl Pts',(7.03193198364747,-4.52243905823974,-0.53229706378677));
#75132=CARTESIAN_POINT('Ctrl Pts',(7.08561295689706,-4.19173085158956,-2.56733631833659));
#75133=CARTESIAN_POINT('Ctrl Pts',(7.1790492542857,-1.17605810855195,-5.21883684139645));
#75134=CARTESIAN_POINT('Ctrl Pts',(7.29831522670288,3.75287271923664,-3.81252108256694));
#75135=CARTESIAN_POINT('Ctrl Pts',(7.41758119912002,5.23673184321061,1.09362253730968));
#75136=CARTESIAN_POINT('Ctrl Pts',(7.53684717153721,1.91336246699203,4.99583974139622));
#75137=CARTESIAN_POINT('Ctrl Pts',(7.65365555000949,-3.06176589728834,4.32605514967914));
#75138=CARTESIAN_POINT('Ctrl Pts',(7.73070860434274,-4.52374311970654,1.40596668425102));
#75139=CARTESIAN_POINT('Ctrl Pts',(7.76800633453693,-4.53045826813502,-0.00168539955221455));
#75140=CARTESIAN_POINT('Origin',(-19.0048063345371,0.,0.));
#75141=CARTESIAN_POINT('',(6.12019366546304,-4.53090073291162,0.00108832199009027));
#75142=CARTESIAN_POINT('',(6.26800633453693,-4.51855722871701,0.00309087752998455));
#75143=CARTESIAN_POINT('',(-19.0048063345371,-4.52375,5.14627461305311E-12));
#75144=CARTESIAN_POINT('Ctrl Pts',(6.12019366546304,-4.53090073291162,0.00108832199009022));
#75145=CARTESIAN_POINT('Ctrl Pts',(6.15839393811966,-4.52623986823191,-1.4402512020058));
#75146=CARTESIAN_POINT('Ctrl Pts',(6.23634953491534,-3.00140589985132,-4.39008539965263));
#75147=CARTESIAN_POINT('Ctrl Pts',(6.35406045585007,2.02618295863798,-4.95115668182184));
#75148=CARTESIAN_POINT('Ctrl Pts',(6.47332642826723,5.26018950109706,-0.974564663002068));
#75149=CARTESIAN_POINT('Ctrl Pts',(6.59259240068441,3.66543382254001,3.89666071943709));
#75150=CARTESIAN_POINT('Ctrl Pts',(6.71185837310155,-1.29412617765311,5.19081952163018));
#75151=CARTESIAN_POINT('Ctrl Pts',(6.80439212802777,-4.22034197546579,2.49786753720102));
#75152=CARTESIAN_POINT('Ctrl Pts',(6.85717055881492,-4.52338388505486,0.498114330194732));
#75153=CARTESIAN_POINT('Ctrl Pts',(6.87019366546302,-4.51971627441788,0.0035956393143962));
#75154=CARTESIAN_POINT('Ctrl Pts',(6.26800633453693,-4.51855722871701,0.00309087752998441));
#75155=CARTESIAN_POINT('Ctrl Pts',(6.29340003881314,-4.51251100940576,-0.961791319275635));
#75156=CARTESIAN_POINT('Ctrl Pts',(6.35854906722839,-3.73642960746153,-3.44613058706164));
#75157=CARTESIAN_POINT('Ctrl Pts',(6.46345341978273,0.355906263086912,-5.33785550419859));
#75158=CARTESIAN_POINT('Ctrl Pts',(6.58271939219988,4.68177552013038,-2.58850316416958));
#75159=CARTESIAN_POINT('Ctrl Pts',(6.70198536461705,4.70985650278392,2.5370499354549));
#75160=CARTESIAN_POINT('Ctrl Pts',(6.8212513370342,0.41437135872153,5.33363544206753));
#75161=CARTESIAN_POINT('Ctrl Pts',(6.92659166034084,-3.71553874394547,3.47918850561399));
#75162=CARTESIAN_POINT('Ctrl Pts',(6.99217665950841,-4.51237405797874,0.977983212239285));
#75163=CARTESIAN_POINT('Ctrl Pts',(7.01800633453693,-4.51891345091625,-0.00327023183485403));
#75164=CARTESIAN_POINT('Origin',(-19.0048063345371,0.,0.));
#75165=CARTESIAN_POINT('',(5.37019366546304,-4.52299381468164,-0.00416642727447685));
#75166=CARTESIAN_POINT('',(5.51800633453693,-4.53018638553777,0.00195909808577518));
#75167=CARTESIAN_POINT('',(-19.0048063345371,-4.52375,5.14627461305311E-12));
#75168=CARTESIAN_POINT('Ctrl Pts',(5.37019366546304,-4.52299381468164,-0.00416642727447635));
#75169=CARTESIAN_POINT('Ctrl Pts',(5.38010666914628,-4.52641083528021,-0.379896318639062));
#75170=CARTESIAN_POINT('Ctrl Pts',(5.42977499696857,-4.31152030878754,-2.25860656938695));
#75171=CARTESIAN_POINT('Ctrl Pts',(5.51919864892993,-1.69550425170618,-5.07391714578299));
#75172=CARTESIAN_POINT('Ctrl Pts',(5.63846462134707,3.34996790097437,-4.17098129128691));
#75173=CARTESIAN_POINT('Ctrl Pts',(5.75773059376426,5.32022794609337,0.560842644091171));
#75174=CARTESIAN_POINT('Ctrl Pts',(5.8769965661814,2.40661152479762,4.77782281363966));
#75175=CARTESIAN_POINT('Ctrl Pts',(5.99626253859857,-2.71623230345395,4.6088449684815));
#75176=CARTESIAN_POINT('Ctrl Pts',(6.07732823835912,-4.50344228157147,1.61826644506594));
#75177=CARTESIAN_POINT('Ctrl Pts',(6.1186386139806,-4.53109046675448,0.0597621744943599));
#75178=CARTESIAN_POINT('Ctrl Pts',(6.12019366546304,-4.53090073291162,0.00108832199009022));
#75179=CARTESIAN_POINT('Ctrl Pts',(5.51800633453693,-4.53018638553777,0.00195909808577534));
#75180=CARTESIAN_POINT('Ctrl Pts',(5.55486809397881,-4.52263664999813,-1.38946064949308));
#75181=CARTESIAN_POINT('Ctrl Pts',(5.63148517755975,-3.09044188949161,-4.29495111977223));
#75182=CARTESIAN_POINT('Ctrl Pts',(5.74785758527973,1.85850858938807,-5.01650440794967));
#75183=CARTESIAN_POINT('Ctrl Pts',(5.86712355769689,5.22443475258933,-1.1509353447283));
#75184=CARTESIAN_POINT('Ctrl Pts',(5.98638953011406,3.79442093031935,3.77117229192225));
#75185=CARTESIAN_POINT('Ctrl Pts',(6.10565550253122,-1.11880512891234,5.2314095361888));
#75186=CARTESIAN_POINT('Ctrl Pts',(6.19952777067219,-4.17755487009671,2.60089376910365));
#75187=CARTESIAN_POINT('Ctrl Pts',(6.25364471467408,-4.52197671814679,0.548787998841091));
#75188=CARTESIAN_POINT('Ctrl Pts',(6.26800633453693,-4.51855722871701,0.00309087752998441));
#75189=CARTESIAN_POINT('Origin',(-19.0048063345371,0.,0.));
#75190=CARTESIAN_POINT('',(4.62019366546303,-4.5164488708372,0.000937415633822161));
#75191=CARTESIAN_POINT('',(4.76800633453694,-4.52453633389133,-0.00411860558352517));
#75192=CARTESIAN_POINT('',(-19.0048063345371,-4.52375,5.14627461305311E-12));
#75193=CARTESIAN_POINT('Ctrl Pts',(4.62019366546303,-4.5164488708372,0.000937415633822658));
#75194=CARTESIAN_POINT('Ctrl Pts',(4.64157472431194,-4.51494682565391,-0.81242583017847));
#75195=CARTESIAN_POINT('Ctrl Pts',(4.70271110729991,-3.91594066105292,-3.14019634832245));
#75196=CARTESIAN_POINT('Ctrl Pts',(4.80360281442692,-0.183306255264012,
-5.34656606492479));
#75197=CARTESIAN_POINT('Ctrl Pts',(4.9228687868441,4.39738257509714,-3.04670253849241));
#75198=CARTESIAN_POINT('Ctrl Pts',(5.04213475926125,4.94135089461829,2.04998078188042));
#75199=CARTESIAN_POINT('Ctrl Pts',(5.16140073167843,0.949245273126337,5.26481749743252));
#75200=CARTESIAN_POINT('Ctrl Pts',(5.27075370041235,-3.5100128039859,3.78114097945864));
#75201=CARTESIAN_POINT('Ctrl Pts',(5.34035134500722,-4.51270714204787,1.12693895523339));
#75202=CARTESIAN_POINT('Ctrl Pts',(5.37019366546304,-4.52299381468164,-0.00416642727447635));
#75203=CARTESIAN_POINT('Ctrl Pts',(4.76800633453694,-4.52453633389133,-0.00411860558352531));
#75204=CARTESIAN_POINT('Ctrl Pts',(4.77658082500543,-4.52755115931345,-0.328832045921557));
#75205=CARTESIAN_POINT('Ctrl Pts',(4.82491063961298,-4.34732968960615,-2.1557477070525));
#75206=CARTESIAN_POINT('Ctrl Pts',(4.91299577835959,-1.86520192939329,-5.01401958655883));
#75207=CARTESIAN_POINT('Ctrl Pts',(5.03226175077674,3.20778511302202,-4.28129481821586));
#75208=CARTESIAN_POINT('Ctrl Pts',(5.15152772319392,5.33608136745939,0.381583924793045));
#75209=CARTESIAN_POINT('Ctrl Pts',(5.27079369561107,2.56594799116161,4.69417527990397));
#75210=CARTESIAN_POINT('Ctrl Pts',(5.39005966802824,-2.5596808892866,4.69759559741243));
#75211=CARTESIAN_POINT('Ctrl Pts',(5.47246388100352,-4.47761888070279,1.72046201744189));
#75212=CARTESIAN_POINT('Ctrl Pts',(5.51511276983976,-4.53077902269241,0.111182399455819));
#75213=CARTESIAN_POINT('Ctrl Pts',(5.51800633453693,-4.53018638553777,0.00195909808577534));
#75214=CARTESIAN_POINT('Origin',(-19.0048063345371,0.,0.));
#75215=CARTESIAN_POINT('',(3.87019366546304,-4.52644367634736,0.00380007935178159));
#75216=CARTESIAN_POINT('',(4.01800633453694,-4.5162743706215,0.000103656827587228));
#75217=CARTESIAN_POINT('',(-19.0048063345371,-4.52375,5.14627461305311E-12));
#75218=CARTESIAN_POINT('Ctrl Pts',(3.87019366546304,-4.52644367634736,0.00380007935178173));
#75219=CARTESIAN_POINT('Ctrl Pts',(3.90304277947762,-4.51527724527072,-1.2388368090617));
#75220=CARTESIAN_POINT('Ctrl Pts',(3.97564721763126,-3.33987304397421,-4.00392317487317));
#75221=CARTESIAN_POINT('Ctrl Pts',(4.08800697992394,1.34401439322441,-5.17812660917343));
#75222=CARTESIAN_POINT('Ctrl Pts',(4.2072729523411,5.08201592186332,-1.67107272126372));
#75223=CARTESIAN_POINT('Ctrl Pts',(4.32653892475827,4.15481546776415,3.36999678021387));
#75224=CARTESIAN_POINT('Ctrl Pts',(4.44580489717544,-0.586433123165232,
5.31746801230425));
#75225=CARTESIAN_POINT('Ctrl Pts',(4.54368981074369,-4.03588134478939,2.90955762213697));
#75226=CARTESIAN_POINT('Ctrl Pts',(4.60181940017289,-4.51773968514488,0.699918329601546));
#75227=CARTESIAN_POINT('Ctrl Pts',(4.62019366546303,-4.5164488708372,0.000937415633822658));
#75228=CARTESIAN_POINT('Ctrl Pts',(4.01800633453694,-4.5162743706215,0.000103656827587367));
#75229=CARTESIAN_POINT('Ctrl Pts',(4.0380488801711,-4.51611900984864,-0.762414301265039));
#75230=CARTESIAN_POINT('Ctrl Pts',(4.09784674994431,-3.97083530460699,-3.03763086589696));
#75231=CARTESIAN_POINT('Ctrl Pts',(4.1973999438566,-0.363029814411452,-5.33737576020804));
#75232=CARTESIAN_POINT('Ctrl Pts',(4.31666591627375,4.29242136001334,-3.19288106886381));
#75233=CARTESIAN_POINT('Ctrl Pts',(4.43593188869093,5.0075045884559,1.88262275785692));
#75234=CARTESIAN_POINT('Ctrl Pts',(4.55519786110808,1.12578593870418,5.22991172698201));
#75235=CARTESIAN_POINT('Ctrl Pts',(4.66588934305676,-3.43601401505965,3.88074351461167));
#75236=CARTESIAN_POINT('Ctrl Pts',(4.73682550086638,-4.51357302704782,1.17669042452511));
#75237=CARTESIAN_POINT('Ctrl Pts',(4.76800633453694,-4.52453633389133,-0.00411860558352531));
#75238=CARTESIAN_POINT('Origin',(-19.0048063345371,0.,0.));
#75239=CARTESIAN_POINT('',(3.12019366546304,-4.5288567256231,-0.00288945374903278));
#75240=CARTESIAN_POINT('',(3.26800633453694,-4.52491800259618,0.00407838215102319));
#75241=CARTESIAN_POINT('',(-19.0048063345371,-4.52375,5.14627461305311E-12));
#75242=CARTESIAN_POINT('Ctrl Pts',(3.12019366546304,-4.5288567256231,-0.00288945374903232));
#75243=CARTESIAN_POINT('Ctrl Pts',(3.12475551050424,-4.53013724628028,-0.175218534882211));
#75244=CARTESIAN_POINT('Ctrl Pts',(3.16907267968449,-4.44288947225829,-1.84804278754527));
#75245=CARTESIAN_POINT('Ctrl Pts',(3.25314517300379,-2.3605259971177,-4.80075899069673));
#75246=CARTESIAN_POINT('Ctrl Pts',(3.37241114542096,2.76045469022341,-4.58249492886218));
#75247=CARTESIAN_POINT('Ctrl Pts',(3.49167711783813,5.34738611599374,-0.157580443906409));
#75248=CARTESIAN_POINT('Ctrl Pts',(3.61094309025528,3.02551034903617,4.41199014025406));
#75249=CARTESIAN_POINT('Ctrl Pts',(3.73020906267246,-2.07373115154603,4.93143072352554));
#75250=CARTESIAN_POINT('Ctrl Pts',(3.81662592107503,-4.38916996825105,2.02768651061558));
#75251=CARTESIAN_POINT('Ctrl Pts',(3.86328745533856,-4.52879131103003,0.265052527621712));
#75252=CARTESIAN_POINT('Ctrl Pts',(3.87019366546304,-4.52644367634736,0.00380007935178173));
#75253=CARTESIAN_POINT('Ctrl Pts',(3.26800633453694,-4.52491800259618,0.00407838215102287));
#75254=CARTESIAN_POINT('Ctrl Pts',(3.29951693533677,-4.51385291460914,-1.1889605374125));
#75255=CARTESIAN_POINT('Ctrl Pts',(3.37078286027565,-3.41735611451173,-3.90518081470287));
#75256=CARTESIAN_POINT('Ctrl Pts',(3.48180410935361,1.16909203446164,-5.22040175338702));
#75257=CARTESIAN_POINT('Ctrl Pts',(3.60107008177076,5.0229355146086,-1.84105661724222));
#75258=CARTESIAN_POINT('Ctrl Pts',(3.72033605418794,4.2658117954781,3.2283463843534));
#75259=CARTESIAN_POINT('Ctrl Pts',(3.83960202660509,-0.407252753478724,
5.33418370949033));
#75260=CARTESIAN_POINT('Ctrl Pts',(3.9388254533881,-3.98398716984629,3.01233344768666));
#75261=CARTESIAN_POINT('Ctrl Pts',(3.99829355603205,-4.51642717518832,0.750075635849043));
#75262=CARTESIAN_POINT('Ctrl Pts',(4.01800633453694,-4.5162743706215,0.000103656827587367));
#75263=CARTESIAN_POINT('Origin',(-19.0048063345371,0.,0.));
#75264=CARTESIAN_POINT('',(2.37019366546305,-4.5174092464024,-0.00228951928982141));
#75265=CARTESIAN_POINT('',(2.51800633453694,-4.52995801530325,-0.00215854265389115));
#75266=CARTESIAN_POINT('',(-19.0048063345371,-4.52375,5.14627461305311E-12));
#75267=CARTESIAN_POINT('Ctrl Pts',(2.37019366546305,-4.5174092464024,-0.00228951928982118));
#75268=CARTESIAN_POINT('Ctrl Pts',(2.38622356566991,-4.52019326613613,-0.611764002830002));
#75269=CARTESIAN_POINT('Ctrl Pts',(2.44200879001584,-4.12113506616917,-2.72928560151133));
#75270=CARTESIAN_POINT('Ctrl Pts',(2.5375493385008,-0.898541159731936,-5.27370777101761));
#75271=CARTESIAN_POINT('Ctrl Pts',(2.65681531091797,3.94915919222963,-3.60881026714515));
#75272=CARTESIAN_POINT('Ctrl Pts',(2.77608128333514,5.17160028152781,1.36891212206108));
#75273=CARTESIAN_POINT('Ctrl Pts',(2.8953472557523,1.64660250832305,5.0899970578978));
#75274=CARTESIAN_POINT('Ctrl Pts',(3.01005138312827,-3.19730291715651,4.1749455591871));
#75275=CARTESIAN_POINT('Ctrl Pts',(3.08500018636519,-4.51897783307502,1.3265857607853));
#75276=CARTESIAN_POINT('Ctrl Pts',(3.12019366546304,-4.5288567256231,-0.00288945374903232));
#75277=CARTESIAN_POINT('Ctrl Pts',(2.51800633453694,-4.52995801530325,-0.00215854265389051));
#75278=CARTESIAN_POINT('Ctrl Pts',(2.52122966636339,-4.53067412723567,-0.123845793639021));
#75279=CARTESIAN_POINT('Ctrl Pts',(2.56420832232889,-4.47097988144249,-1.745662850511));
#75280=CARTESIAN_POINT('Ctrl Pts',(2.64694230243346,-2.52065997660762,-4.71864852835388));
#75281=CARTESIAN_POINT('Ctrl Pts',(2.76620827485062,2.60476451764482,-4.67274784890289));
#75282=CARTESIAN_POINT('Ctrl Pts',(2.88547424726778,5.33906061341968,-0.337346139800582));
#75283=CARTESIAN_POINT('Ctrl Pts',(3.00474021968495,3.17219218262773,4.3077334421112));
#75284=CARTESIAN_POINT('Ctrl Pts',(3.1240061921021,-1.90669334680315,4.99838885372723));
#75285=CARTESIAN_POINT('Ctrl Pts',(3.21176156371945,-4.35584349366905,2.13042087106249));
#75286=CARTESIAN_POINT('Ctrl Pts',(3.25976161119772,-4.52781317396269,0.316236055284816));
#75287=CARTESIAN_POINT('Ctrl Pts',(3.26800633453694,-4.52491800259618,0.00407838215102287));
#75288=CARTESIAN_POINT('Origin',(-19.0048063345371,0.,0.));
#75289=CARTESIAN_POINT('',(1.62019366546304,-4.52045926477682,0.00381908414570068));
#75290=CARTESIAN_POINT('',(1.76800633453694,-4.51830251797945,-0.00294632473948842));
#75291=CARTESIAN_POINT('',(-19.0048063345371,-4.52375,5.14627461305311E-12));
#75292=CARTESIAN_POINT('Ctrl Pts',(1.62019366546304,-4.52045926477682,0.00381908414570031));
#75293=CARTESIAN_POINT('Ctrl Pts',(1.64769162083558,-4.51214039746521,-1.03991157870731));
#75294=CARTESIAN_POINT('Ctrl Pts',(1.71494490034717,-3.63301811037992,-3.6052702635876));
#75295=CARTESIAN_POINT('Ctrl Pts',(1.82195350399781,0.637572764456073,-5.31157894037619));
#75296=CARTESIAN_POINT('Ctrl Pts',(1.94121947641498,4.81206051717935,-2.33740100300047));
#75297=CARTESIAN_POINT('Ctrl Pts',(2.06048544883214,4.56916064047356,2.78247028939603));
#75298=CARTESIAN_POINT('Ctrl Pts',(2.17975142124932,0.13185098482894,5.34808238414702));
#75299=CARTESIAN_POINT('Ctrl Pts',(2.2829874934596,-3.81383264233026,3.31927032643957));
#75300=CARTESIAN_POINT('Ctrl Pts',(2.34646824153085,-4.51328869371237,0.899777262863328));
#75301=CARTESIAN_POINT('Ctrl Pts',(2.37019366546305,-4.5174092464024,-0.00228951928982118));
#75302=CARTESIAN_POINT('Ctrl Pts',(1.76800633453694,-4.51830251797944,-0.00294632473948821));
#75303=CARTESIAN_POINT('Ctrl Pts',(1.78269772152906,-4.52162528364921,-0.561252537622042));
#75304=CARTESIAN_POINT('Ctrl Pts',(1.83714443266024,-4.1666769618709,-2.62627596164084));
#75305=CARTESIAN_POINT('Ctrl Pts',(1.93134646793046,-1.07540952932231,-5.24050236103854));
#75306=CARTESIAN_POINT('Ctrl Pts',(2.05061244034763,3.82554554823664,-3.73959515324518));
#75307=CARTESIAN_POINT('Ctrl Pts',(2.16987841276479,5.21471653241851,1.19419518435166));
#75308=CARTESIAN_POINT('Ctrl Pts',(2.28914438518196,1.81686868775421,5.03173517022369));
#75309=CARTESIAN_POINT('Ctrl Pts',(2.40518702577268,-3.11192516407456,4.27135130982762));
#75310=CARTESIAN_POINT('Ctrl Pts',(2.48147434222434,-4.52184188050285,1.37699754703399));
#75311=CARTESIAN_POINT('Ctrl Pts',(2.51800633453694,-4.52995801530325,-0.00215854265389051));
#75312=CARTESIAN_POINT('Origin',(-19.0048063345371,0.,0.));
#75313=CARTESIAN_POINT('',(0.870193665463051,-4.53113324750611,0.000558172709172654));
#75314=CARTESIAN_POINT('',(1.01800633453695,-4.51919695317837,0.00339653540470913));
#75315=CARTESIAN_POINT('',(-19.0048063345371,-4.52375,5.14627461305311E-12));
#75316=CARTESIAN_POINT('Ctrl Pts',(0.870193665463051,-4.53113324750611,
0.000558172709172731));
#75317=CARTESIAN_POINT('Ctrl Pts',(0.909159676001256,-4.52858208666899,
-1.46947121982517));
#75318=CARTESIAN_POINT('Ctrl Pts',(0.987881010678515,-2.94913757193914,
-4.44401136316868));
#75319=CARTESIAN_POINT('Ctrl Pts',(1.10635766949483,2.12108733213468,-4.91124815085553));
#75320=CARTESIAN_POINT('Ctrl Pts',(1.22562364191199,5.27796984247255,-0.873157609927544));
#75321=CARTESIAN_POINT('Ctrl Pts',(1.34488961432916,3.58976808851186,3.96647638849978));
#75322=CARTESIAN_POINT('Ctrl Pts',(1.46415558674632,-1.39377816290472,5.16495424011036));
#75323=CARTESIAN_POINT('Ctrl Pts',(1.55592360379095,-4.24384740014909,2.43893578023149));
#75324=CARTESIAN_POINT('Ctrl Pts',(1.60793629669652,-4.52416744682079,0.469067916438565));
#75325=CARTESIAN_POINT('Ctrl Pts',(1.62019366546304,-4.52045926477682,0.00381908414570031));
#75326=CARTESIAN_POINT('Ctrl Pts',(1.01800633453695,-4.51919695317837,0.00339653540470948));
#75327=CARTESIAN_POINT('Ctrl Pts',(1.04416577669474,-4.51229041994084,-0.990227835244301));
#75328=CARTESIAN_POINT('Ctrl Pts',(1.11008054299158,-3.69955244106376,-3.50416488459642));
#75329=CARTESIAN_POINT('Ctrl Pts',(1.21575063342748,0.458561535247667,-5.33001800843103));
#75330=CARTESIAN_POINT('Ctrl Pts',(1.33501660584464,4.73072145051602,-2.49792818340231));
#75331=CARTESIAN_POINT('Ctrl Pts',(1.4542825782618,4.66016158094803,2.62721614856175));
#75332=CARTESIAN_POINT('Ctrl Pts',(1.57354855067898,0.311654656198974,5.34062187643698));
#75333=CARTESIAN_POINT('Ctrl Pts',(1.67812313610401,-3.75204777525101,3.42109829131755));
#75334=CARTESIAN_POINT('Ctrl Pts',(1.74294239739001,-4.51263378228107,0.94954045107943));
#75335=CARTESIAN_POINT('Ctrl Pts',(1.76800633453694,-4.51830251797944,-0.00294632473948821));
#75336=CARTESIAN_POINT('Origin',(-19.0048063345371,0.,0.));
#75337=CARTESIAN_POINT('',(0.120193665463054,-4.5221327339856,-0.00411166771258635));
#75338=CARTESIAN_POINT('',(0.268006334536952,-4.53063960879454,0.00147156798560651));
#75339=CARTESIAN_POINT('',(-19.0048063345371,-4.52375,5.14627461305311E-12));
#75340=CARTESIAN_POINT('Ctrl Pts',(0.120193665463054,-4.5221327339856,-0.00411166771258617));
#75341=CARTESIAN_POINT('Ctrl Pts',(0.130872407027874,-4.52570863968184,
-0.409061250785844));
#75342=CARTESIAN_POINT('Ctrl Pts',(0.181306472731748,-4.29011830250525,
-2.31748674548857));
#75343=CARTESIAN_POINT('Ctrl Pts',(0.271495862574679,-1.59754830160526,
-5.10560567355749));
#75344=CARTESIAN_POINT('Ctrl Pts',(0.390761834991842,3.42961351418844,-4.10574244359289));
#75345=CARTESIAN_POINT('Ctrl Pts',(0.510027807409007,5.30844993855932,0.663120742876867));
#75346=CARTESIAN_POINT('Ctrl Pts',(0.629293779826171,2.3142219020159,4.82325065262569));
#75347=CARTESIAN_POINT('Ctrl Pts',(0.748559752243337,-2.80442147910245,
4.55572058376859));
#75348=CARTESIAN_POINT('Ctrl Pts',(0.828859714122298,-4.51741504144067,
1.5598712850993));
#75349=CARTESIAN_POINT('Ctrl Pts',(0.869404351862201,-4.53118492500449,
0.0303357705989649));
#75350=CARTESIAN_POINT('Ctrl Pts',(0.870193665463051,-4.53113324750611,
0.000558172709172731));
#75351=CARTESIAN_POINT('Ctrl Pts',(0.268006334536952,-4.53063960879454,
0.00147156798560636));
#75352=CARTESIAN_POINT('Ctrl Pts',(0.30563383186041,-4.52462283428668,-1.41847499082472));
#75353=CARTESIAN_POINT('Ctrl Pts',(0.383016653322921,-3.03986771850672,
-4.34950762223985));
#75354=CARTESIAN_POINT('Ctrl Pts',(0.500154798924492,1.95470155837633,-4.9798104852985));
#75355=CARTESIAN_POINT('Ctrl Pts',(0.619420771341654,5.24561577554724,-1.05018369209291));
#75356=CARTESIAN_POINT('Ctrl Pts',(0.738686743758821,3.72114619758183,3.84349341459433));
#75357=CARTESIAN_POINT('Ctrl Pts',(0.857952716175984,-1.21927069064937,
5.20891059961017));
#75358=CARTESIAN_POINT('Ctrl Pts',(0.951059246435361,-4.20229923544821,
2.54195357514844));
#75359=CARTESIAN_POINT('Ctrl Pts',(1.00441045255568,-4.52278649496717,0.51981426310584));
#75360=CARTESIAN_POINT('Ctrl Pts',(1.01800633453695,-4.51919695317837,0.00339653540470948));
#75361=CARTESIAN_POINT('Origin',(-19.0048063345371,0.,0.));
#75362=CARTESIAN_POINT('',(-0.629806334536947,-4.51667307150718,0.00139986576683541));
#75363=CARTESIAN_POINT('',(-0.481993665463047,-4.52365053271834,-0.00416855255043758));
#75364=CARTESIAN_POINT('',(-19.0048063345371,-4.52375,5.14627461305311E-12));
#75365=CARTESIAN_POINT('Ctrl Pts',(-0.629806334536947,-4.51667307150718,
0.00139986576683564));
#75366=CARTESIAN_POINT('Ctrl Pts',(-0.607659537806456,-4.51434322716492,
-0.840988711232888));
#75367=CARTESIAN_POINT('Ctrl Pts',(-0.545757416936911,-3.88343245072244,
-3.19877541626441));
#75368=CARTESIAN_POINT('Ctrl Pts',(-0.444099971928309,-0.0803835059582494,
-5.3491035101028));
#75369=CARTESIAN_POINT('Ctrl Pts',(-0.324833999511145,4.45519871447649,
-2.9615155384281));
#75370=CARTESIAN_POINT('Ctrl Pts',(-0.205568027093979,4.90098621647057,
2.14469204684251));
#75371=CARTESIAN_POINT('Ctrl Pts',(-0.0863020546768169,0.847753848005954,
5.28210973788082));
#75372=CARTESIAN_POINT('Ctrl Pts',(0.0222851761755296,-3.55110674608297,
3.72388277406811));
#75373=CARTESIAN_POINT('Ctrl Pts',(0.0911170828888195,-4.51239608883662,
1.09850420880814));
#75374=CARTESIAN_POINT('Ctrl Pts',(0.120193665463054,-4.5221327339856,-0.00411166771258617));
#75375=CARTESIAN_POINT('Ctrl Pts',(-0.481993665463047,-4.52365053271834,
-0.00416855255043813));
#75376=CARTESIAN_POINT('Ctrl Pts',(-0.472653437112973,-4.52691325946138,
-0.358057576997311));
#75377=CARTESIAN_POINT('Ctrl Pts',(-0.423557884623844,-4.32709133434675,
-2.21458053169529));
#75378=CARTESIAN_POINT('Ctrl Pts',(-0.33470700799566,-1.76836721737897,
-5.04898485205759));
#75379=CARTESIAN_POINT('Ctrl Pts',(-0.215441035578497,3.2895799187264,-4.21877169447693));
#75380=CARTESIAN_POINT('Ctrl Pts',(-0.0961750631613321,5.32775006176976,
0.484200300619735));
#75381=CARTESIAN_POINT('Ctrl Pts',(0.0230909092558323,2.4751385673978,4.74268486450319));
#75382=CARTESIAN_POINT('Ctrl Pts',(0.142356881672996,-2.64960696388247,
4.64746743815955));
#75383=CARTESIAN_POINT('Ctrl Pts',(0.223995356766704,-4.49261143470523,
1.66197929681203));
#75384=CARTESIAN_POINT('Ctrl Pts',(0.265878507721356,-4.53097985608846,
0.0817692380266874));
#75385=CARTESIAN_POINT('Ctrl Pts',(0.268006334536952,-4.53063960879454,
0.00147156798560636));
#75386=CARTESIAN_POINT('Origin',(-19.0048063345371,0.,0.));
#75387=CARTESIAN_POINT('',(-1.37980633453694,-4.52728092082441,0.00355961958845701));
#75388=CARTESIAN_POINT('',(-1.23199366546305,-4.51634007617231,0.000583253576266762));
#75389=CARTESIAN_POINT('',(-19.0048063345371,-4.52375,5.14627461305311E-12));
#75390=CARTESIAN_POINT('Ctrl Pts',(-1.37980633453694,-4.52728092082441,
0.00355961958845723));
#75391=CARTESIAN_POINT('Ctrl Pts',(-1.34619148264078,-4.51631056435734,
-1.26743466713941));
#75392=CARTESIAN_POINT('Ctrl Pts',(-1.27282130660557,-3.29427248004508,
-4.06006742591324));
#75393=CARTESIAN_POINT('Ctrl Pts',(-1.1596958064313,1.4434128789333,-5.15130363410601));
#75394=CARTESIAN_POINT('Ctrl Pts',(-1.04042983401413,5.1132327918697,-1.57296544334973));
#75395=CARTESIAN_POINT('Ctrl Pts',(-0.921163861596969,4.08919417984387,
3.4493275909016));
#75396=CARTESIAN_POINT('Ctrl Pts',(-0.801897889179802,-0.688653371177603,
5.30519805513329));
#75397=CARTESIAN_POINT('Ctrl Pts',(-0.704778713493129,-4.06450823554763,
2.8507052065737));
#75398=CARTESIAN_POINT('Ctrl Pts',(-0.64741486194551,-4.51852548964501,
0.671168163515238));
#75399=CARTESIAN_POINT('Ctrl Pts',(-0.629806334536947,-4.51667307150718,
0.00139986576683564));
#75400=CARTESIAN_POINT('Ctrl Pts',(-1.23199366546305,-4.51634007617231,
0.00058325357626697));
#75401=CARTESIAN_POINT('Ctrl Pts',(-1.2111853819473,-4.51543176696114,-0.791038463333831));
#75402=CARTESIAN_POINT('Ctrl Pts',(-1.1506217742925,-3.93972969518399,-3.09633097448578));
#75403=CARTESIAN_POINT('Ctrl Pts',(-1.05030284249865,-0.260250641047462,
-5.34337349018783));
#75404=CARTESIAN_POINT('Ctrl Pts',(-0.931036870081484,4.35306998183813,
-3.10968686285734));
#75405=CARTESIAN_POINT('Ctrl Pts',(-0.811770897664319,4.97034828165621,
1.97863806969469));
#75406=CARTESIAN_POINT('Ctrl Pts',(-0.692504925247154,1.02493354489289,
5.25060776295097));
#75407=CARTESIAN_POINT('Ctrl Pts',(-0.582579181180064,-3.47868636868056,
3.82384134221039));
#75408=CARTESIAN_POINT('Ctrl Pts',(-0.512408761252028,-4.51302593739761,
1.14821960904481));
#75409=CARTESIAN_POINT('Ctrl Pts',(-0.481993665463047,-4.52365053271834,
-0.00416855255043813));
#75410=CARTESIAN_POINT('Origin',(-19.0048063345371,0.,0.));
#75411=CARTESIAN_POINT('',(-2.12980633453694,-4.5281227353363,-0.00324265984058113));
#75412=CARTESIAN_POINT('',(-1.98199366546304,-4.5257976962895,0.00394161820304176));
#75413=CARTESIAN_POINT('',(-19.0048063345371,-4.52375,5.14627461305311E-12));
#75414=CARTESIAN_POINT('Ctrl Pts',(-2.12980633453694,-4.5281227353363,-0.00324265984058134));
#75415=CARTESIAN_POINT('Ctrl Pts',(-2.12447875161416,-4.52975245353138,
-0.204583738014264));
#75416=CARTESIAN_POINT('Ctrl Pts',(-2.07939584455233,-4.42598350509595,
-1.90667553345163));
#75417=CARTESIAN_POINT('Ctrl Pts',(-1.99455761335145,-2.26770352691226,
-4.84529571686329));
#75418=CARTESIAN_POINT('Ctrl Pts',(-1.87529164093429,2.84812859908841,-4.52852441230905));
#75419=CARTESIAN_POINT('Ctrl Pts',(-1.75602566851712,5.3494283442679,-0.0546466775498073));
#75420=CARTESIAN_POINT('Ctrl Pts',(-1.63675969609995,2.94004616678162,4.46939575412793));
#75421=CARTESIAN_POINT('Ctrl Pts',(-1.51749372368279,-2.1682471155684,4.89061083257026));
#75422=CARTESIAN_POINT('Ctrl Pts',(-1.43184260316178,-4.40735967461942,
1.96896633272643));
#75423=CARTESIAN_POINT('Ctrl Pts',(-1.38594680677984,-4.52928489125952,
0.235733932378456));
#75424=CARTESIAN_POINT('Ctrl Pts',(-1.37980633453694,-4.52728092082441,
0.00355961958845723));
#75425=CARTESIAN_POINT('Ctrl Pts',(-1.98199366546304,-4.5257976962895,0.00394161820304197));
#75426=CARTESIAN_POINT('Ctrl Pts',(-1.94971732678163,-4.51460986650304,
-1.21747812123507));
#75427=CARTESIAN_POINT('Ctrl Pts',(-1.87768566396116,-3.37337480828373,
-3.96175999185013));
#75428=CARTESIAN_POINT('Ctrl Pts',(-1.76589867700163,1.26933645129948,-5.19693713885497));
#75429=CARTESIAN_POINT('Ctrl Pts',(-1.64663270458447,5.05743447897554,-1.74405479921852));
#75430=CARTESIAN_POINT('Ctrl Pts',(-1.52736673216731,4.20289585976879,3.30983942869535));
#75431=CARTESIAN_POINT('Ctrl Pts',(-1.40810075975014,-0.509827857576372,
5.32535878673416));
#75432=CARTESIAN_POINT('Ctrl Pts',(-1.30964307084872,-4.01396563289227,
2.95355445726466));
#75433=CARTESIAN_POINT('Ctrl Pts',(-1.25094070608636,-4.51716713965928,
0.721396617025564));
#75434=CARTESIAN_POINT('Ctrl Pts',(-1.23199366546305,-4.51634007617231,
0.00058325357626697));
#75435=CARTESIAN_POINT('Origin',(-19.0048063345371,0.,0.));
#75436=CARTESIAN_POINT('',(-2.87980633453694,-4.51700722203196,-0.00187082749320296));
#75437=CARTESIAN_POINT('',(-2.73199366546304,-4.52935956130001,-0.002593214221287));
#75438=CARTESIAN_POINT('',(-19.0048063345371,-4.52375,5.14627461305311E-12));
#75439=CARTESIAN_POINT('Ctrl Pts',(-2.87980633453694,-4.51700722203196,
-0.00187082749320257));
#75440=CARTESIAN_POINT('Ctrl Pts',(-2.86301069644849,-4.51937852208916,
-0.640601591406374));
#75441=CARTESIAN_POINT('Ctrl Pts',(-2.80645973422099,-4.09406588665098,
-2.7881947122476));
#75442=CARTESIAN_POINT('Ctrl Pts',(-2.71015344785444,-0.796888040481462,
-5.29002262006144));
#75443=CARTESIAN_POINT('Ctrl Pts',(-2.59088747543727,4.01787548130092,-3.53214474315326));
#75444=CARTESIAN_POINT('Ctrl Pts',(-2.4716215030201,5.1442993855074,1.46818040515877));
#75445=CARTESIAN_POINT('Ctrl Pts',(-2.35235553060294,1.54834617361307,5.12074154751847));
#75446=CARTESIAN_POINT('Ctrl Pts',(-2.23841714110855,-3.24483985403934,
4.11937367175704));
#75447=CARTESIAN_POINT('Ctrl Pts',(-2.16423407575322,-4.51759122093492,
1.2978574142544));
#75448=CARTESIAN_POINT('Ctrl Pts',(-2.12980633453694,-4.5281227353363,-0.00324265984058134));
#75449=CARTESIAN_POINT('Ctrl Pts',(-2.73199366546304,-4.52935956130001,
-0.00259321422128662));
#75450=CARTESIAN_POINT('Ctrl Pts',(-2.72800459575501,-4.53038856066062,
-0.153241100583692));
#75451=CARTESIAN_POINT('Ctrl Pts',(-2.68426020190793,-4.4551357826128,-1.8042149261768));
#75452=CARTESIAN_POINT('Ctrl Pts',(-2.60076048392179,-2.42938797848125,
-4.76628206276323));
#75453=CARTESIAN_POINT('Ctrl Pts',(-2.48149451150462,2.69420407591751,-4.62175670596335));
#75454=CARTESIAN_POINT('Ctrl Pts',(-2.36222853908746,5.34456377722621,-0.234539299413323));
#75455=CARTESIAN_POINT('Ctrl Pts',(-2.2429625666703,3.0887071435723,4.36798109348626));
#75456=CARTESIAN_POINT('Ctrl Pts',(-2.12369659425313,-2.00252877889888,
4.96077102288439));
#75457=CARTESIAN_POINT('Ctrl Pts',(-2.03670696051738,-4.37514918048342,
2.07163492985408));
#75458=CARTESIAN_POINT('Ctrl Pts',(-1.98947265092069,-4.52839010979406,
0.286965679856997));
#75459=CARTESIAN_POINT('Ctrl Pts',(-1.98199366546304,-4.5257976962895,0.00394161820304197));
#75460=CARTESIAN_POINT('Origin',(-19.0048063345371,0.,0.));
#75461=CARTESIAN_POINT('',(-3.62980633453693,-4.52125034636371,0.00399034990006141));
#75462=CARTESIAN_POINT('',(-3.48199366546304,-4.51776292098496,-0.00258343477365697));
#75463=CARTESIAN_POINT('',(-19.0048063345371,-4.52375,5.14627461305311E-12));
#75464=CARTESIAN_POINT('Ctrl Pts',(-3.62980633453693,-4.52125034636371,
0.00399034990006115));
#75465=CARTESIAN_POINT('Ctrl Pts',(-3.60154264128282,-4.51220230515001,
-1.06833051476153));
#75466=CARTESIAN_POINT('Ctrl Pts',(-3.53352362388965,-3.59375490220193,
-3.66289634246604));
#75467=CARTESIAN_POINT('Ctrl Pts',(-3.42574928235742,0.73967021363975,-5.29832594739868));
#75468=CARTESIAN_POINT('Ctrl Pts',(-3.30648330994026,4.85615013534878,-2.24436532961465));
#75469=CARTESIAN_POINT('Ctrl Pts',(-3.18721733752309,4.51476892709962,2.86988351762224));
#75470=CARTESIAN_POINT('Ctrl Pts',(-3.06795136510593,0.0289085841635225,
5.34962934824326));
#75471=CARTESIAN_POINT('Ctrl Pts',(-2.96548103077721,-3.84803061328253,
3.2608714513295));
#75472=CARTESIAN_POINT('Ctrl Pts',(-2.90276602058755,-4.51376564796621,
0.871275981998934));
#75473=CARTESIAN_POINT('Ctrl Pts',(-2.87980633453694,-4.51700722203196,
-0.00187082749320257));
#75474=CARTESIAN_POINT('Ctrl Pts',(-3.48199366546304,-4.51776292098496,
-0.00258343477365669));
#75475=CARTESIAN_POINT('Ctrl Pts',(-3.46653654058934,-4.52080615393757,
-0.59016526618593));
#75476=CARTESIAN_POINT('Ctrl Pts',(-3.41132409157659,-4.14089776643248,
-2.6852100500767));
#75477=CARTESIAN_POINT('Ctrl Pts',(-3.31635631842477,-0.97436265912244,
-5.26022699703307));
#75478=CARTESIAN_POINT('Ctrl Pts',(-3.19709034600761,3.89680154001646,-3.66528421947511));
#75479=CARTESIAN_POINT('Ctrl Pts',(-3.07782437359044,5.19076988807344,1.29432554671451));
#75480=CARTESIAN_POINT('Ctrl Pts',(-2.95855840117328,1.71970200914856,5.0657670348663));
#75481=CARTESIAN_POINT('Ctrl Pts',(-2.84328149846415,-3.16112500776204,
4.21631729843839));
#75482=CARTESIAN_POINT('Ctrl Pts',(-2.76775991989407,-4.52013348714372,
1.34812538121587));
#75483=CARTESIAN_POINT('Ctrl Pts',(-2.73199366546304,-4.52935956130001,
-0.00259321422128662));
#75484=CARTESIAN_POINT('Origin',(-19.0048063345371,0.,0.));
#75485=CARTESIAN_POINT('',(-4.37980633453694,-4.53121768806138,1.67337722143111E-5));
#75486=CARTESIAN_POINT('',(-4.23199366546304,-4.51989857042376,0.00365667477888132));
#75487=CARTESIAN_POINT('',(-19.0048063345371,-4.52375,5.14627461305311E-12));
#75488=CARTESIAN_POINT('Ctrl Pts',(-4.37980633453694,-4.53121768806138,
1.6733772214251E-5));
#75489=CARTESIAN_POINT('Ctrl Pts',(-4.34007458611715,-4.53113573122214,
-1.49882557159262));
#75490=CARTESIAN_POINT('Ctrl Pts',(-4.2605875135583,-2.8958932222745,-4.49755267314905));
#75491=CARTESIAN_POINT('Ctrl Pts',(-4.14134511686041,2.21520613519663,-4.86952067953422));
#75492=CARTESIAN_POINT('Ctrl Pts',(-4.02207914444325,5.29379542366406,-0.771427172335632));
#75493=CARTESIAN_POINT('Ctrl Pts',(-3.90281317202608,3.51277284030709,4.03482302489525));
#75494=CARTESIAN_POINT('Ctrl Pts',(-3.78354719960892,-1.49291394549895,
5.13717605510642));
#75495=CARTESIAN_POINT('Ctrl Pts',(-3.69254492044586,-4.2666565334125,2.38001604204234));
#75496=CARTESIAN_POINT('Ctrl Pts',(-3.64129796542187,-4.52492915609762,
0.439981338626065));
#75497=CARTESIAN_POINT('Ctrl Pts',(-3.62980633453693,-4.52125034636371,
0.00399034990006115));
#75498=CARTESIAN_POINT('Ctrl Pts',(-4.23199366546304,-4.51989857042376,
0.00365667477888139));
#75499=CARTESIAN_POINT('Ctrl Pts',(-4.20506848542367,-4.51216606523885,
-1.01865332044624));
#75500=CARTESIAN_POINT('Ctrl Pts',(-4.13838798124524,-3.66181433414549,
-3.5620610773861));
#75501=CARTESIAN_POINT('Ctrl Pts',(-4.03195215292777,0.561046973578825,
-5.32020647580954));
#75502=CARTESIAN_POINT('Ctrl Pts',(-3.91268618051059,4.77791530080097,-2.40642806461773));
#75503=CARTESIAN_POINT('Ctrl Pts',(-3.79342020809343,4.60874071171544,2.71640934028442));
#75504=CARTESIAN_POINT('Ctrl Pts',(-3.67415423567627,0.208822528592261,
5.3456303466813));
#75505=CARTESIAN_POINT('Ctrl Pts',(-3.5703453881328,-3.78770815692856,3.36288627847629));
#75506=CARTESIAN_POINT('Ctrl Pts',(-3.50629186472839,-4.51297903774032,
0.921079959357981));
#75507=CARTESIAN_POINT('Ctrl Pts',(-3.48199366546304,-4.51776292098496,
-0.00258343477365669));
#75508=CARTESIAN_POINT('Origin',(-19.0048063345371,0.,0.));
#75509=CARTESIAN_POINT('',(-5.12980633453694,-4.5213004327236,-0.00399911873852178));
#75510=CARTESIAN_POINT('',(-4.98199366546304,-4.5309724658868,0.000956350713833126));
#75511=CARTESIAN_POINT('',(-19.0048063345371,-4.52375,5.14627461305311E-12));
#75512=CARTESIAN_POINT('Ctrl Pts',(-5.12980633453694,-4.5213004327236,-0.00399911873852177));
#75513=CARTESIAN_POINT('Ctrl Pts',(-5.11836185509054,-4.52497523886784,
-0.438189005660487));
#75514=CARTESIAN_POINT('Ctrl Pts',(-5.06716205150508,-4.26803848439264,
-2.37638847486489));
#75515=CARTESIAN_POINT('Ctrl Pts',(-4.97620692378056,-1.49900068010318,
-5.13540327830972));
#75516=CARTESIAN_POINT('Ctrl Pts',(-4.8569409513634,3.50798892841612,-4.03898298435808));
#75517=CARTESIAN_POINT('Ctrl Pts',(-4.73767497894623,5.29470588216781,0.765153246847895));
#75518=CARTESIAN_POINT('Ctrl Pts',(-4.61840900652908,2.22097517906763,4.86689214219808));
#75519=CARTESIAN_POINT('Ctrl Pts',(-4.4991430341119,-2.89157200322203,4.50090893264979));
#75520=CARTESIAN_POINT('Ctrl Pts',(-4.41960881011453,-4.53081425398383,
1.50152710822327));
#75521=CARTESIAN_POINT('Ctrl Pts',(-4.37982991025621,-4.53121773669229,
0.000906105290546244));
#75522=CARTESIAN_POINT('Ctrl Pts',(-4.37980633453694,-4.53121768806138,
1.6733772214251E-5));
#75523=CARTESIAN_POINT('Ctrl Pts',(-4.98199366546304,-4.5309724658868,0.000956350713833048));
#75524=CARTESIAN_POINT('Ctrl Pts',(-4.943600430258,-4.5268105339362,-1.44760255615506));
#75525=CARTESIAN_POINT('Ctrl Pts',(-4.8654518709139,-2.98832627775091,-4.40370984899896));
#75526=CARTESIAN_POINT('Ctrl Pts',(-4.74754798743075,2.05017057992043,-4.94127222939968));
#75527=CARTESIAN_POINT('Ctrl Pts',(-4.62828201501358,5.26485402104248,-0.949043091182221));
#75528=CARTESIAN_POINT('Ctrl Pts',(-4.50901604259642,3.64649329319062,3.91439105283614));
#75529=CARTESIAN_POINT('Ctrl Pts',(-4.38975007017925,-1.31928468068921,
5.18448247977621));
#75530=CARTESIAN_POINT('Ctrl Pts',(-4.29740927780146,-4.22633141630272,
2.48301617388978));
#75531=CARTESIAN_POINT('Ctrl Pts',(-4.24482380956272,-4.52358319409679,
0.490798619014908));
#75532=CARTESIAN_POINT('Ctrl Pts',(-4.23199366546304,-4.51989857042376,
0.00365667477888139));
#75533=CARTESIAN_POINT('Origin',(-19.0048063345371,0.,0.));
#75534=CARTESIAN_POINT('',(-5.87980633453694,-4.51698519435381,0.00184419225129259));
#75535=CARTESIAN_POINT('',(-5.73199366546304,-4.52277473914781,-0.00415818099157916));
#75536=CARTESIAN_POINT('',(-19.0048063345371,-4.52375,5.14627461305311E-12));
#75537=CARTESIAN_POINT('Ctrl Pts',(-5.87980633453694,-4.51698519435381,
0.00184419225129261));
#75538=CARTESIAN_POINT('Ctrl Pts',(-5.85689379992486,-4.51379722466762,
-0.869520083832802));
#75539=CARTESIAN_POINT('Ctrl Pts',(-5.79422594117374,-3.85010936700085,
-3.25727232317951));
#75540=CARTESIAN_POINT('Ctrl Pts',(-5.69180275828355,0.0225690143544715,
-5.34965984987971));
#75541=CARTESIAN_POINT('Ctrl Pts',(-5.57253678586638,4.51136481694416,-2.87523170514354));
#75542=CARTESIAN_POINT('Ctrl Pts',(-5.45327081344922,4.85880639859978,2.23860899907733));
#75543=CARTESIAN_POINT('Ctrl Pts',(-5.33400484103205,0.745948446959714,
5.29744568488459));
#75544=CARTESIAN_POINT('Ctrl Pts',(-5.22618334806129,-3.59130840982308,
3.66643927470266));
#75545=CARTESIAN_POINT('Ctrl Pts',(-5.15811717922959,-4.51220986058247,
1.07008052929913));
#75546=CARTESIAN_POINT('Ctrl Pts',(-5.12980633453694,-4.5213004327236,-0.00399911873852177));
#75547=CARTESIAN_POINT('Ctrl Pts',(-5.73199366546304,-4.52277473914781,
-0.00415818099157958));
#75548=CARTESIAN_POINT('Ctrl Pts',(-5.72188769923138,-4.52623711933511,
-0.387249167118643));
#75549=CARTESIAN_POINT('Ctrl Pts',(-5.67202640886067,-4.30619055181852,
-2.27344188077484));
#75550=CARTESIAN_POINT('Ctrl Pts',(-5.5824097943509,-1.67087756910494,-5.08208016474257));
#75551=CARTESIAN_POINT('Ctrl Pts',(-5.46314382193374,3.37015638858599,-4.15468609744235));
#75552=CARTESIAN_POINT('Ctrl Pts',(-5.34387784951657,5.31744555918776,0.586637346988937));
#75553=CARTESIAN_POINT('Ctrl Pts',(-5.22461187709941,2.38341244602753,4.7894379382062));
#75554=CARTESIAN_POINT('Ctrl Pts',(-5.10534590468224,-2.73855172438397,
4.59561803293978));
#75555=CARTESIAN_POINT('Ctrl Pts',(-5.02447316747012,-4.50701785980123,
1.60354636847148));
#75556=CARTESIAN_POINT('Ctrl Pts',(-4.98335575439705,-4.53112012006139,
0.0523473326608906));
#75557=CARTESIAN_POINT('Ctrl Pts',(-4.98199366546304,-4.5309724658868,0.000956350713833048));
#75558=CARTESIAN_POINT('Origin',(-19.0048063345371,0.,0.));
#75559=CARTESIAN_POINT('',(-6.62980633453694,-4.52807551305362,0.00326271820855672));
#75560=CARTESIAN_POINT('',(-6.48199366546304,-4.51649700603775,0.0010553308724473));
#75561=CARTESIAN_POINT('',(-19.0048063345371,-4.52375,5.14627461305311E-12));
#75562=CARTESIAN_POINT('Ctrl Pts',(-6.62980633453694,-4.52807551305362,
0.00326271820855709));
#75563=CARTESIAN_POINT('Ctrl Pts',(-6.59542574475919,-4.51751162682835,
-1.29609075831453));
#75564=CARTESIAN_POINT('Ctrl Pts',(-6.52128983084239,-3.24773613231329,
-4.11594224841461));
#75565=CARTESIAN_POINT('Ctrl Pts',(-6.40739859278654,1.54227677916538,-5.12257281122204));
#75566=CARTESIAN_POINT('Ctrl Pts',(-6.28813262036938,5.14255591405802,-1.47427559859448));
#75567=CARTESIAN_POINT('Ctrl Pts',(-6.16886664795221,4.0220584092331,3.52738090125541));
#75568=CARTESIAN_POINT('Ctrl Pts',(-6.04960067553505,-0.790618568056538,
5.2909632534793));
#75569=CARTESIAN_POINT('Ctrl Pts',(-5.95324723772995,-4.09237462138663,
2.79182142727619));
#75570=CARTESIAN_POINT('Ctrl Pts',(-5.89664912406392,-4.5193286410022,0.64237590783374));
#75571=CARTESIAN_POINT('Ctrl Pts',(-5.87980633453694,-4.51698519435381,
0.00184419225129261));
#75572=CARTESIAN_POINT('Ctrl Pts',(-6.48199366546304,-4.51649700603775,
0.00105533087244723));
#75573=CARTESIAN_POINT('Ctrl Pts',(-6.46041964406571,-4.514789747878,-0.819626683720531));
#75574=CARTESIAN_POINT('Ctrl Pts',(-6.39909029852933,-3.90782509244913,
-3.15496527216252));
#75575=CARTESIAN_POINT('Ctrl Pts',(-6.29800562885389,-0.157375080700092,
-5.34739223694899));
#75576=CARTESIAN_POINT('Ctrl Pts',(-6.17873965643672,4.41210639136683,-3.02534094658233));
#75577=CARTESIAN_POINT('Ctrl Pts',(-6.05947368401956,4.93135114605077,2.07392056891087));
#75578=CARTESIAN_POINT('Ctrl Pts',(-5.94020771160239,0.923701554504711,
5.2693591726142));
#75579=CARTESIAN_POINT('Ctrl Pts',(-5.83104770541689,-3.5204528709042,3.76673040395475));
#75580=CARTESIAN_POINT('Ctrl Pts',(-5.76164302337044,-4.51261664569771,
1.11977212892738));
#75581=CARTESIAN_POINT('Ctrl Pts',(-5.73199366546304,-4.52277473914781,
-0.00415818099157958));
#75582=CARTESIAN_POINT('Origin',(-19.0048063345371,0.,0.));
#75583=CARTESIAN_POINT('',(-7.37980633453694,-4.52733122205943,-0.00354293946284749));
#75584=CARTESIAN_POINT('',(-7.23199366546304,-4.5266579896236,0.00374494774771153));
#75585=CARTESIAN_POINT('',(-19.0048063345371,-4.52375,5.14627461305311E-12));
#75586=CARTESIAN_POINT('Ctrl Pts',(-7.37980633453694,-4.52733122205943,
-0.00354293946284695));
#75587=CARTESIAN_POINT('Ctrl Pts',(-7.37371301373258,-4.52931362694418,
-0.233927783108747));
#75588=CARTESIAN_POINT('Ctrl Pts',(-7.32786436878916,-4.40845915531641,
-1.96535187413747));
#75589=CARTESIAN_POINT('Ctrl Pts',(-7.24226039970668,-2.17404118518495,
-4.88803792895919));
#75590=CARTESIAN_POINT('Ctrl Pts',(-7.12299442728953,2.93474766896221,-4.4728767017821));
#75591=CARTESIAN_POINT('Ctrl Pts',(-7.00372845487236,5.34948934683475,0.0483073278670784));
#75592=CARTESIAN_POINT('Ctrl Pts',(-6.8844624824552,2.85349310274905,4.52514607304423));
#75593=CARTESIAN_POINT('Ctrl Pts',(-6.76519651003803,-2.26196004295795,
4.84797964454119));
#75594=CARTESIAN_POINT('Ctrl Pts',(-6.68031112739861,-4.42492236636027,
1.91028737732804));
#75595=CARTESIAN_POINT('Ctrl Pts',(-6.63518106889825,-4.52972697053736,
0.206391280659083));
#75596=CARTESIAN_POINT('Ctrl Pts',(-6.62980633453694,-4.52807551305362,
0.00326271820855709));
#75597=CARTESIAN_POINT('Ctrl Pts',(-7.23199366546304,-4.5266579896236,0.00374494774771174));
#75598=CARTESIAN_POINT('Ctrl Pts',(-7.19895158890004,-4.51552227061198,
-1.2460383771676));
#75599=CARTESIAN_POINT('Ctrl Pts',(-7.12615418819799,-3.32846977442805,
-4.01809588963737));
#75600=CARTESIAN_POINT('Ctrl Pts',(-7.01360146335687,1.36911075397815,-5.17154777558412));
#75601=CARTESIAN_POINT('Ctrl Pts',(-6.89433549093971,5.09006036110679,-1.64640704933419));
#75602=CARTESIAN_POINT('Ctrl Pts',(-6.77506951852255,4.13842333057186,3.3901066338371));
#75603=CARTESIAN_POINT('Ctrl Pts',(-6.65580354610538,-0.612214140739847,
5.31456155272341));
#75604=CARTESIAN_POINT('Ctrl Pts',(-6.55811159508555,-4.04316743284744,
2.89473048394592));
#75605=CARTESIAN_POINT('Ctrl Pts',(-6.50017496820477,-4.51793578172491,
0.692677346406831));
#75606=CARTESIAN_POINT('Ctrl Pts',(-6.48199366546304,-4.51649700603775,
0.00105533087244723));
#75607=CARTESIAN_POINT('Origin',(-19.0048063345371,0.,0.));
#75608=CARTESIAN_POINT('',(-8.12980633453695,-4.51668977813578,-0.00142781023108144));
#75609=CARTESIAN_POINT('',(-7.98199366546304,-4.52867803382547,-0.00298322746560442));
#75610=CARTESIAN_POINT('',(-19.0048063345371,-4.52375,5.14627461305311E-12));
#75611=CARTESIAN_POINT('Ctrl Pts',(-8.12980633453695,-4.51668977813578,
-0.00142781023108107));
#75612=CARTESIAN_POINT('Ctrl Pts',(-8.11224495856691,-4.51857450838071,
-0.669396461747199));
#75613=CARTESIAN_POINT('Ctrl Pts',(-8.05492825845782,-4.06624602752072,
-2.84708018096034));
#75614=CARTESIAN_POINT('Ctrl Pts',(-7.95785623420967,-0.694939784074152,
-5.30437824502882));
#75615=CARTESIAN_POINT('Ctrl Pts',(-7.83859026179251,4.08510370142725,-3.45417104648997));
#75616=CARTESIAN_POINT('Ctrl Pts',(-7.71932428937535,5.11509323577896,1.56690492982581));
#75617=CARTESIAN_POINT('Ctrl Pts',(-7.60005831695818,1.44951639010705,5.1495895083623));
#75618=CARTESIAN_POINT('Ctrl Pts',(-7.48688566534538,-3.29143404128054,
4.06351594110314));
#75619=CARTESIAN_POINT('Ctrl Pts',(-7.41346833787163,-4.51637960438101,
1.26919743053686));
#75620=CARTESIAN_POINT('Ctrl Pts',(-7.37980633453694,-4.52733122205943,
-0.00354293946284695));
#75621=CARTESIAN_POINT('Ctrl Pts',(-7.98199366546304,-4.52867803382547,
-0.00298322746560407));
#75622=CARTESIAN_POINT('Ctrl Pts',(-7.97723885787343,-4.53004555346133,
-0.182620278006116));
#75623=CARTESIAN_POINT('Ctrl Pts',(-7.93272872614476,-4.43868714409182,
-1.86281378505977));
#75624=CARTESIAN_POINT('Ctrl Pts',(-7.84846327027703,-2.33721622703428,
-4.8121503467676));
#75625=CARTESIAN_POINT('Ctrl Pts',(-7.72919729785987,2.78264580301424,-4.56905383933861));
#75626=CARTESIAN_POINT('Ctrl Pts',(-7.60993132544269,5.34808751697683,-0.131645594550073));
#75627=CARTESIAN_POINT('Ctrl Pts',(-7.49066535302554,3.00407816434195,4.42661101005405));
#75628=CARTESIAN_POINT('Ctrl Pts',(-7.37139938060837,-2.09762255015898,
4.92131591028987));
#75629=CARTESIAN_POINT('Ctrl Pts',(-7.28517548475421,-4.39381329989842,
2.01288556324745));
#75630=CARTESIAN_POINT('Ctrl Pts',(-7.2387069130391,-4.52892046360946,0.257666787695734));
#75631=CARTESIAN_POINT('Ctrl Pts',(-7.23199366546304,-4.5266579896236,0.00374494774771174));
#75632=CARTESIAN_POINT('Origin',(-19.0048063345371,0.,0.));
#75633=CARTESIAN_POINT('',(-8.87980633453694,-4.52208054885539,0.00410638580840894));
#75634=CARTESIAN_POINT('',(-8.73199366546304,-4.51730023616471,-0.0021866156284378));
#75635=CARTESIAN_POINT('',(-19.0048063345371,-4.52375,5.14627461305311E-12));
#75636=CARTESIAN_POINT('Ctrl Pts',(-8.87980633453694,-4.52208054885539,
0.00410638580840929));
#75637=CARTESIAN_POINT('Ctrl Pts',(-8.85077690340124,-4.51238109141432,
-1.0967537268227));
#75638=CARTESIAN_POINT('Ctrl Pts',(-8.78199214812648,-3.55360792181159,
-3.72035082563007));
#75639=CARTESIAN_POINT('Ctrl Pts',(-8.67345206871266,0.841493716983345,
-5.28311065510666));
#75640=CARTESIAN_POINT('Ctrl Pts',(-8.55418609629549,4.8984412193819,-2.15049842829157));
#75641=CARTESIAN_POINT('Ctrl Pts',(-8.43492012387834,4.45870511426281,2.9562338496592));
#75642=CARTESIAN_POINT('Ctrl Pts',(-8.31565415146116,-0.0740445231469701,
5.3491950121879));
#75643=CARTESIAN_POINT('Ctrl Pts',(-8.21394955501404,-3.88140416868336,
3.20237992240633));
#75644=CARTESIAN_POINT('Ctrl Pts',(-8.15200028270597,-4.51430786880021,
0.842746453538187));
#75645=CARTESIAN_POINT('Ctrl Pts',(-8.12980633453695,-4.51668977813578,
-0.00142781023108107));
#75646=CARTESIAN_POINT('Ctrl Pts',(-8.73199366546304,-4.51730023616471,
-0.0021866156284378));
#75647=CARTESIAN_POINT('Ctrl Pts',(-8.71577080270775,-4.51998733949217,
-0.619035001797185));
#75648=CARTESIAN_POINT('Ctrl Pts',(-8.65979261581342,-4.1143840503259,-2.74413231667926));
#75649=CARTESIAN_POINT('Ctrl Pts',(-8.56405910478001,-0.872954921887009,
-5.27800344412176));
#75650=CARTESIAN_POINT('Ctrl Pts',(-8.44479313236285,3.96661430405479,-3.58961580321287));
#75651=CARTESIAN_POINT('Ctrl Pts',(-8.32552715994568,5.16490077910572,1.39397653990334));
#75652=CARTESIAN_POINT('Ctrl Pts',(-8.20626118752853,1.62189841803372,5.09792273121));
#75653=CARTESIAN_POINT('Ctrl Pts',(-8.09175002270096,-3.20937125987305,
4.16096954991165));
#75654=CARTESIAN_POINT('Ctrl Pts',(-8.01699418201248,-4.51861161310398,
1.31933937798815));
#75655=CARTESIAN_POINT('Ctrl Pts',(-7.98199366546304,-4.52867803382547,
-0.00298322746560407));
#75656=CARTESIAN_POINT('Origin',(-19.0048063345371,0.,0.));
#75657=CARTESIAN_POINT('',(-9.62980633453695,-4.53114288885854,-0.00052505224322001));
#75658=CARTESIAN_POINT('',(-9.48199366546304,-4.52065448282384,0.00386729026705834));
#75659=CARTESIAN_POINT('',(-19.0048063345371,-4.52375,5.14627461305311E-12));
#75660=CARTESIAN_POINT('Ctrl Pts',(-9.62980633453694,-4.53114288885854,
-0.000525052243220102));
#75661=CARTESIAN_POINT('Ctrl Pts',(-9.62906417237462,-4.53118872991189,
-0.0285236575162823));
#75662=CARTESIAN_POINT('Ctrl Pts',(-9.58856668607325,-4.51825661700592,
-1.55627717876711));
#75663=CARTESIAN_POINT('Ctrl Pts',(-9.50831387563282,-2.80981824212958,
-4.55239402029525));
#75664=CARTESIAN_POINT('Ctrl Pts',(-9.38904790321564,2.30850450978291,-4.82598972213328));
#75665=CARTESIAN_POINT('Ctrl Pts',(-9.26978193079849,5.30766038347549,-0.669411027328533));
#75666=CARTESIAN_POINT('Ctrl Pts',(-9.15051595838132,3.43447659405036,4.10167531561732));
#75667=CARTESIAN_POINT('Ctrl Pts',(-9.03124998596416,-1.59149680929566,
5.10749525460629));
#75668=CARTESIAN_POINT('Ctrl Pts',(-8.9410134446827,-4.28877837960027,2.3211131273353));
#75669=CARTESIAN_POINT('Ctrl Pts',(-8.89053222754029,-4.52566433739803,
0.410855926456967));
#75670=CARTESIAN_POINT('Ctrl Pts',(-8.87980633453694,-4.52208054885539,
0.00410638580840929));
#75671=CARTESIAN_POINT('Ctrl Pts',(-9.48199366546304,-4.52065448282384,
0.003867290267058));
#75672=CARTESIAN_POINT('Ctrl Pts',(-9.45430274754209,-4.51214545629191,
-1.04707296981455));
#75673=CARTESIAN_POINT('Ctrl Pts',(-9.38685650548208,-3.62320685191578,
-3.61980730776049));
#75674=CARTESIAN_POINT('Ctrl Pts',(-9.279654939283,0.663324621354469,-5.30842454015434));
#75675=CARTESIAN_POINT('Ctrl Pts',(-9.16038896686585,4.82333959217,-2.31403669599532));
#75676=CARTESIAN_POINT('Ctrl Pts',(-9.04112299444865,4.55561293942915,2.80459647684182));
#75677=CARTESIAN_POINT('Ctrl Pts',(-8.92185702203153,0.105913061027885,
5.34865899785279));
#75678=CARTESIAN_POINT('Ctrl Pts',(-8.81881391236962,-3.82252862056392,
3.30456340422465));
#75679=CARTESIAN_POINT('Ctrl Pts',(-8.7555261268468,-4.51340239419676,0.892597556938324));
#75680=CARTESIAN_POINT('Ctrl Pts',(-8.73199366546304,-4.51730023616471,
-0.0021866156284378));
#75681=CARTESIAN_POINT('Origin',(-19.0048063345371,0.,0.));
#75682=CARTESIAN_POINT('',(-10.3798063345369,-4.52050667523945,-0.00383117177063042));
#75683=CARTESIAN_POINT('',(-10.231993665463,-4.53116917314862,0.000422383571537207));
#75684=CARTESIAN_POINT('',(-19.0048063345371,-4.52375,5.14627461305311E-12));
#75685=CARTESIAN_POINT('Ctrl Pts',(-10.3798063345369,-4.52050667523944,
-0.00383117177062971));
#75686=CARTESIAN_POINT('Ctrl Pts',(-10.367596117209,-4.52421503063526,-0.467278015537651));
#75687=CARTESIAN_POINT('Ctrl Pts',(-10.3156305757419,-4.24527193127081,
-2.43530731245446));
#75688=CARTESIAN_POINT('Ctrl Pts',(-10.2239097101358,-1.39989788550755,
-5.1632989241352));
#75689=CARTESIAN_POINT('Ctrl Pts',(-10.1046437377186,3.5850651163716,-3.97072763875836));
#75690=CARTESIAN_POINT('Ctrl Pts',(-9.98537776530147,5.27900086719687,0.866902367028086));
#75691=CARTESIAN_POINT('Ctrl Pts',(-9.86611179288431,2.12690589100833,4.90873111920161));
#75692=CARTESIAN_POINT('Ctrl Pts',(-9.74758798262946,-2.9458872206108,4.4473195424606));
#75693=CARTESIAN_POINT('Ctrl Pts',(-9.66881949651368,-4.52873316692682,
1.4712747485241));
#75694=CARTESIAN_POINT('Ctrl Pts',(-9.62980633453694,-4.53114288885854,
-0.000525052243220102));
#75695=CARTESIAN_POINT('Ctrl Pts',(-10.231993665463,-4.53116917314862,0.000422383571537441));
#75696=CARTESIAN_POINT('Ctrl Pts',(-10.1928346923764,-4.52920551616272,
-1.47685525433921));
#75697=CARTESIAN_POINT('Ctrl Pts',(-10.1139203951507,-2.93581244463462,
-4.4575405446346));
#75698=CARTESIAN_POINT('Ctrl Pts',(-9.995250773786,2.14488029590958,-4.90090391336402));
#75699=CARTESIAN_POINT('Ctrl Pts',(-9.87598480136882,5.28214236395734,-0.847551000645274));
#75700=CARTESIAN_POINT('Ctrl Pts',(-9.75671882895166,3.57048986575489,3.98383894884689));
#75701=CARTESIAN_POINT('Ctrl Pts',(-9.6374528565345,-1.41881005763682,5.15813422393762));
#75702=CARTESIAN_POINT('Ctrl Pts',(-9.54587780203829,-4.2496605265107,2.42408697318163));
#75703=CARTESIAN_POINT('Ctrl Pts',(-9.49405807168114,-4.52436170383019,
0.461741971228011));
#75704=CARTESIAN_POINT('Ctrl Pts',(-9.48199366546304,-4.52065448282384,
0.003867290267058));
#75705=CARTESIAN_POINT('Origin',(-19.0048063345371,0.,0.));
#75706=CARTESIAN_POINT('',(-11.1298063345369,-4.51738211886999,0.00226454645098684));
#75707=CARTESIAN_POINT('',(-10.981993665463,-4.52191995054341,-0.00408866953903741));
#75708=CARTESIAN_POINT('',(-19.0048063345371,-4.52375,5.14627461305311E-12));
#75709=CARTESIAN_POINT('Ctrl Pts',(-11.1298063345369,-4.51738211886999,
0.00226454645098691));
#75710=CARTESIAN_POINT('Ctrl Pts',(-11.1061280620433,-4.51331604098809,
-0.89802300770951));
#75711=CARTESIAN_POINT('Ctrl Pts',(-11.0426944654106,-3.81596241879828,
-3.3156771965644));
#75712=CARTESIAN_POINT('Ctrl Pts',(-10.9395055446388,0.125513175958816,
-5.3482348782084));
#75713=CARTESIAN_POINT('Ctrl Pts',(-10.8202395722216,4.56586008070243,-2.78788299490349));
#75714=CARTESIAN_POINT('Ctrl Pts',(-10.7009735998044,4.81482706281336,2.3316968553018));
#75715=CARTESIAN_POINT('Ctrl Pts',(-10.5817076273873,0.643866774853417,
5.31081965858981));
#75716=CARTESIAN_POINT('Ctrl Pts',(-10.4746518722981,-3.63062580284369,
3.60882339659679));
#75717=CARTESIAN_POINT('Ctrl Pts',(-10.407351441348,-4.51214097275215,1.04166150619729));
#75718=CARTESIAN_POINT('Ctrl Pts',(-10.3798063345369,-4.52050667523944,
-0.00383117177062971));
#75719=CARTESIAN_POINT('Ctrl Pts',(-10.981993665463,-4.52191995054341,-0.00408866953903672));
#75720=CARTESIAN_POINT('Ctrl Pts',(-10.9711219613498,-4.52552666035439,
-0.416404890679838));
#75721=CARTESIAN_POINT('Ctrl Pts',(-10.9204949330975,-4.28461857606984,
-2.33232788952565));
#75722=CARTESIAN_POINT('Ctrl Pts',(-10.8301125807061,-1.57276909104567,
-5.11329326736293));
#75723=CARTESIAN_POINT('Ctrl Pts',(-10.710846608289,3.44948468012718,-4.08906176199085));
#75724=CARTESIAN_POINT('Ctrl Pts',(-10.5915806358718,5.30517167611101,0.688857125097259));
#75725=CARTESIAN_POINT('Ctrl Pts',(-10.4723146634547,2.29080359893313,4.83441718544467));
#75726=CARTESIAN_POINT('Ctrl Pts',(-10.3530486910375,-2.82648222901952,
4.54206658480968));
#75727=CARTESIAN_POINT('Ctrl Pts',(-10.272941691707,-4.52084542429402,1.54516401016659));
#75728=CARTESIAN_POINT('Ctrl Pts',(-10.2325900165155,-4.53119907763328,
0.0229198089290014));
#75729=CARTESIAN_POINT('Ctrl Pts',(-10.231993665463,-4.53116917314862,0.000422383571537441));
#75730=CARTESIAN_POINT('Origin',(-19.0048063345371,0.,0.));
#75731=CARTESIAN_POINT('',(-11.8798063345369,-4.52881345908333,0.00291265612866996));
#75732=CARTESIAN_POINT('',(-11.731993665463,-4.51674360781622,0.00151377565128424));
#75733=CARTESIAN_POINT('',(-19.0048063345371,-4.52375,5.14627461305311E-12));
#75734=CARTESIAN_POINT('Ctrl Pts',(-11.8798063345369,-4.52881345908333,
0.00291265612866994));
#75735=CARTESIAN_POINT('Ctrl Pts',(-11.8446600068776,-4.51888726912132,
-1.32481461068629));
#75736=CARTESIAN_POINT('Ctrl Pts',(-11.7697583550792,-3.20025743132486,
-4.17153219074509));
#75737=CARTESIAN_POINT('Ctrl Pts',(-11.6551013791418,1.64056947847539,-5.09194478133052));
#75738=CARTESIAN_POINT('Ctrl Pts',(-11.5358354067246,5.16997442825406,-1.37503973797965));
#75739=CARTESIAN_POINT('Ctrl Pts',(-11.4165694343074,3.95343302047925,3.60412780328452));
#75740=CARTESIAN_POINT('Ctrl Pts',(-11.2973034618903,-0.892290949753927,
5.2747688793739));
#75741=CARTESIAN_POINT('Ctrl Pts',(-11.2017157619668,-4.11948975774644,
2.73291356932791));
#75742=CARTESIAN_POINT('Ctrl Pts',(-11.1458833861823,-4.52014290068459,
0.613540960632567));
#75743=CARTESIAN_POINT('Ctrl Pts',(-11.1298063345369,-4.51738211886999,
0.00226454645098691));
#75744=CARTESIAN_POINT('Ctrl Pts',(-11.731993665463,-4.51674360781622,0.00151377565128417));
#75745=CARTESIAN_POINT('Ctrl Pts',(-11.7096539061841,-4.51419998793741,
-0.848181357999456));
#75746=CARTESIAN_POINT('Ctrl Pts',(-11.6475588227661,-3.87511238866226,
-3.21352454637504));
#75747=CARTESIAN_POINT('Ctrl Pts',(-11.5457084152091,-0.0544412345818395,
-5.34943051209986));
#75748=CARTESIAN_POINT('Ctrl Pts',(-11.4264424427919,4.46950872374863,-2.93987455857264));
#75749=CARTESIAN_POINT('Ctrl Pts',(-11.3071764703748,4.89052762470212,2.16843496647541));
#75750=CARTESIAN_POINT('Ctrl Pts',(-11.1879104979576,0.822127460035971,
5.28615901115948));
#75751=CARTESIAN_POINT('Ctrl Pts',(-11.0795162296537,-3.56132121802685,
3.70942426675612));
#75752=CARTESIAN_POINT('Ctrl Pts',(-11.0108772854889,-4.51233775122686,
1.0913407992777));
#75753=CARTESIAN_POINT('Ctrl Pts',(-10.981993665463,-4.52191995054341,-0.00408866953903672));
#75754=CARTESIAN_POINT('Origin',(-19.0048063345371,0.,0.));
#75755=CARTESIAN_POINT('',(-12.6298063345369,-4.52649620861785,-0.00378695143178565));
#75756=CARTESIAN_POINT('',(-12.4819936654631,-4.52748577852528,0.00349000897288482));
#75757=CARTESIAN_POINT('',(-19.0048063345371,-4.52375,5.14627461305311E-12));
#75758=CARTESIAN_POINT('Ctrl Pts',(-12.6298063345369,-4.52649620861785,
-0.0037869514317854));
#75759=CARTESIAN_POINT('Ctrl Pts',(-12.622947275851,-4.52882314301935,-0.263247936212846));
#75760=CARTESIAN_POINT('Ctrl Pts',(-12.576332893026,-4.39030829601886,-2.02406958410072));
#75761=CARTESIAN_POINT('Ctrl Pts',(-12.4899631860619,-2.07957366092086,
-4.92896979688741));
#75762=CARTESIAN_POINT('Ctrl Pts',(-12.3706972136447,3.02027981942101,-4.41557240708635));
#75763=CARTESIAN_POINT('Ctrl Pts',(-12.2514312412276,5.34756910110119,0.151243442078761));
#75764=CARTESIAN_POINT('Ctrl Pts',(-12.1321652688104,2.76588321291629,4.57922044919569));
#75765=CARTESIAN_POINT('Ctrl Pts',(-12.0128992963933,-2.35483522599469,
4.80355294841628));
#75766=CARTESIAN_POINT('Ctrl Pts',(-11.9287796516354,-4.44186617927913,
1.85165188822665));
#75767=CARTESIAN_POINT('Ctrl Pts',(-11.8844153310167,-4.53011515338936,
0.177027299288359));
#75768=CARTESIAN_POINT('Ctrl Pts',(-11.8798063345369,-4.52881345908333,
0.00291265612866994));
#75769=CARTESIAN_POINT('Ctrl Pts',(-12.481993665463,-4.52748577852528,0.00349000897288478));
#75770=CARTESIAN_POINT('Ctrl Pts',(-12.4481858510185,-4.51659720762945,
-1.27465003716645));
#75771=CARTESIAN_POINT('Ctrl Pts',(-12.3746227124348,-3.28263402910187,
-4.07417368335456));
#75772=CARTESIAN_POINT('Ctrl Pts',(-12.2613042497121,1.4683779898736,-5.14424306683332));
#75773=CARTESIAN_POINT('Ctrl Pts',(-12.142038277295,5.12080107761086,-1.54814953261863));
#75774=CARTESIAN_POINT('Ctrl Pts',(-12.0227723048778,4.07241808607112,3.46911827184497));
#75775=CARTESIAN_POINT('Ctrl Pts',(-11.9035063324606,-0.714373682966412,
5.30179600634471));
#75776=CARTESIAN_POINT('Ctrl Pts',(-11.8065801193224,-4.07160180796638,
2.83586945730652));
#75777=CARTESIAN_POINT('Ctrl Pts',(-11.7494092303232,-4.51872655563701,
0.663916647888202));
#75778=CARTESIAN_POINT('Ctrl Pts',(-11.731993665463,-4.51674360781622,0.00151377565128417));
#75779=CARTESIAN_POINT('Origin',(-19.0048063345371,0.,0.));
#75780=CARTESIAN_POINT('',(-13.3798063345369,-4.51646009003207,-0.000966303587493708));
#75781=CARTESIAN_POINT('',(-13.2319936654631,-4.52792820117867,-0.00332346547265827));
#75782=CARTESIAN_POINT('',(-19.0048063345371,-4.52375,5.14627461305311E-12));
#75783=CARTESIAN_POINT('Ctrl Pts',(-13.3798063345369,-4.51646009003207,
-0.000966303587493431));
#75784=CARTESIAN_POINT('Ctrl Pts',(-13.3614792206853,-4.51778745205074,
-0.69814919617005));
#75785=CARTESIAN_POINT('Ctrl Pts',(-13.3033967826947,-4.0376662333295,-2.90593474512968));
#75786=CARTESIAN_POINT('Ctrl Pts',(-13.2055590205649,-0.592734148285034,
-5.31676932913924));
#75787=CARTESIAN_POINT('Ctrl Pts',(-13.0862930481478,4.15081895382183,-3.37491805566053));
#75788=CARTESIAN_POINT('Ctrl Pts',(-12.9670270757306,5.08399264919423,1.66504913223642));
#75789=CARTESIAN_POINT('Ctrl Pts',(-12.8477611033134,1.35014976061496,5.17653025623679));
#75790=CARTESIAN_POINT('Ctrl Pts',(-12.7353541895822,-3.3370920331084,4.00738784074087));
#75791=CARTESIAN_POINT('Ctrl Pts',(-12.66270259999,-4.51533615659485,1.24059625344786));
#75792=CARTESIAN_POINT('Ctrl Pts',(-12.6298063345369,-4.52649620861785,
-0.0037869514317854));
#75793=CARTESIAN_POINT('Ctrl Pts',(-13.2319936654631,-4.52792820117867,
-0.00332346547265792));
#75794=CARTESIAN_POINT('Ctrl Pts',(-13.2264731199919,-4.52964693741261,
-0.211980413649894));
#75795=CARTESIAN_POINT('Ctrl Pts',(-13.1811972503816,-4.42162610491374,
-1.92145771095745));
#75796=CARTESIAN_POINT('Ctrl Pts',(-13.0961660566323,-2.24417885919362,
-4.85623639249116));
#75797=CARTESIAN_POINT('Ctrl Pts',(-12.9769000842151,2.8700569434679,-4.51465876817511));
#75798=CARTESIAN_POINT('Ctrl Pts',(-12.8576341117979,5.34963052761172,-0.0287031331433309));
#75799=CARTESIAN_POINT('Ctrl Pts',(-12.7383681393808,2.91833658830642,4.48360147751333));
#75800=CARTESIAN_POINT('Ctrl Pts',(-12.6191021669636,-2.19193944145102,
4.88003812862352));
#75801=CARTESIAN_POINT('Ctrl Pts',(-12.533644008991,-4.41184422699395,1.95417554456908));
#75802=CARTESIAN_POINT('Ctrl Pts',(-12.4879411751575,-4.52940130847082,
0.228341879470367));
#75803=CARTESIAN_POINT('Ctrl Pts',(-12.481993665463,-4.52748577852528,0.00349000897288478));
#75804=CARTESIAN_POINT('Origin',(-19.0048063345371,0.,0.));
#75805=CARTESIAN_POINT('',(-14.1298063345369,-4.52294015312425,0.00416476062241385));
#75806=CARTESIAN_POINT('',(-13.9819936654631,-4.51691917766224,-0.00176125576838326));
#75807=CARTESIAN_POINT('',(-19.0048063345371,-4.52375,5.14627461305311E-12));
#75808=CARTESIAN_POINT('Ctrl Pts',(-14.1298063345369,-4.52294015312425,
0.00416476062241395));
#75809=CARTESIAN_POINT('Ctrl Pts',(-14.1000111655197,-4.51268424282815,
-1.12518759832097));
#75810=CARTESIAN_POINT('Ctrl Pts',(-14.0304606723633,-3.51256915117181,
-3.77762082095125));
#75811=CARTESIAN_POINT('Ctrl Pts',(-13.9211548550679,0.943005562874773,
-5.26593869864046));
#75812=CARTESIAN_POINT('Ctrl Pts',(-13.8018888826508,4.93891810628447,-2.05583506379208));
#75813=CARTESIAN_POINT('Ctrl Pts',(-13.6826229102336,4.40098996586505,3.04148930462108));
#75814=CARTESIAN_POINT('Ctrl Pts',(-13.5633569378164,-0.176970207163579,
5.34677953683851));
#75815=CARTESIAN_POINT('Ctrl Pts',(-13.4624180792509,-3.91396229489176,
3.1438056354711));
#75816=CARTESIAN_POINT('Ctrl Pts',(-13.4012345448244,-4.51490812758485,
0.814185593869427));
#75817=CARTESIAN_POINT('Ctrl Pts',(-13.3798063345369,-4.51646009003207,
-0.000966303587493431));
#75818=CARTESIAN_POINT('Ctrl Pts',(-13.9819936654631,-4.51691917766224,
-0.00176125576838361));
#75819=CARTESIAN_POINT('Ctrl Pts',(-13.9650050648262,-4.51917472294271,
-0.647861788429469));
#75820=CARTESIAN_POINT('Ctrl Pts',(-13.9082611400502,-4.08712657467319,
-2.80303613492246));
#75821=CARTESIAN_POINT('Ctrl Pts',(-13.8117618911353,-0.771223875207531,
-5.29382511857655));
#75822=CARTESIAN_POINT('Ctrl Pts',(-13.6924959187181,4.03495798434998,-3.51261792917751));
#75823=CARTESIAN_POINT('Ctrl Pts',(-13.5732299463009,5.13711878645237,1.49311125696483));
#75824=CARTESIAN_POINT('Ctrl Pts',(-13.4539639738838,1.52349413715743,5.12819035000159));
#75825=CARTESIAN_POINT('Ctrl Pts',(-13.3402185469378,-3.25667002467314,
4.1053241526965));
#75826=CARTESIAN_POINT('Ctrl Pts',(-13.2662284441309,-4.51726973366597,
1.29062918388309));
#75827=CARTESIAN_POINT('Ctrl Pts',(-13.2319936654631,-4.52792820117867,
-0.00332346547265792));
#75828=CARTESIAN_POINT('Origin',(-19.0048063345371,0.,0.));
#75829=CARTESIAN_POINT('',(-14.879806334537,-4.53091903216787,-0.00105619164529906));
#75830=CARTESIAN_POINT('',(-14.7319936654631,-4.521456298353,0.00402490267532751));
#75831=CARTESIAN_POINT('',(-19.0048063345371,-4.52375,5.14627461305311E-12));
#75832=CARTESIAN_POINT('Ctrl Pts',(-14.8798063345369,-4.53091903216787,
-0.00105619164529849));
#75833=CARTESIAN_POINT('Ctrl Pts',(-14.878298434493,-4.53109805835402,-0.0579503522764566));
#75834=CARTESIAN_POINT('Ctrl Pts',(-14.8370352103101,-4.50431938173549,
-1.61466921124215));
#75835=CARTESIAN_POINT('Ctrl Pts',(-14.7560166619881,-2.72169207944861,
-4.60562287829862));
#75836=CARTESIAN_POINT('Ctrl Pts',(-14.6367506895709,2.40094789974828,-4.78067139956327));
#75837=CARTESIAN_POINT('Ctrl Pts',(-14.5174847171537,5.31955958788271,-0.56714695851215));
#75838=CARTESIAN_POINT('Ctrl Pts',(-14.3982187447365,3.35490834716323,4.16700850147134));
#75839=CARTESIAN_POINT('Ctrl Pts',(-14.2789527723194,-1.68949024264872,
5.07592283106375));
#75840=CARTESIAN_POINT('Ctrl Pts',(-14.1894819689195,-4.31022186693971,
2.26223150191539));
#75841=CARTESIAN_POINT('Ctrl Pts',(-14.1397664896587,-4.52636857661816,
0.38169323430466));
#75842=CARTESIAN_POINT('Ctrl Pts',(-14.1298063345369,-4.52294015312425,
0.00416476062241395));
#75843=CARTESIAN_POINT('Ctrl Pts',(-14.7319936654631,-4.521456298353,0.00402490267532758));
#75844=CARTESIAN_POINT('Ctrl Pts',(-14.7035370096605,-4.51223610990917,
-1.07549240604431));
#75845=CARTESIAN_POINT('Ctrl Pts',(-14.6353250297189,-3.58372170086442,
-3.67739134091624));
#75846=CARTESIAN_POINT('Ctrl Pts',(-14.5273577256382,0.765356598558913,
-5.29467656481004));
#75847=CARTESIAN_POINT('Ctrl Pts',(-14.4080917532211,4.86697750131595,-2.22078829592513));
#75848=CARTESIAN_POINT('Ctrl Pts',(-14.2888257808039,4.50079794053571,2.89174489712377));
#75849=CARTESIAN_POINT('Ctrl Pts',(-14.1695598083868,0.00296436731219236,
5.34970670821892));
#75850=CARTESIAN_POINT('Ctrl Pts',(-14.0672824366065,-3.85651800034967,
3.24614022654441));
#75851=CARTESIAN_POINT('Ctrl Pts',(-14.0047603889652,-4.51389648162949,
0.864089469439338));
#75852=CARTESIAN_POINT('Ctrl Pts',(-13.9819936654631,-4.51691917766224,
-0.00176125576838361));
#75853=CARTESIAN_POINT('Origin',(-19.0048063345371,0.,0.));
#75854=CARTESIAN_POINT('',(-15.6298063345369,-4.51976043794902,-0.00361086820214561));
#75855=CARTESIAN_POINT('',(-15.4819936654631,-4.5312138402642,-0.000120197794654664));
#75856=CARTESIAN_POINT('',(-19.0048063345371,-4.52375,5.14627461305311E-12));
#75857=CARTESIAN_POINT('Ctrl Pts',(-15.6298063345369,-4.51976043794902,
-0.00361086820214504));
#75858=CARTESIAN_POINT('Ctrl Pts',(-15.6168303793274,-4.52343268604556,
-0.496326928866944));
#75859=CARTESIAN_POINT('Ctrl Pts',(-15.5640990999787,-4.22180986129563,
-2.49423832903335));
#75860=CARTESIAN_POINT('Ctrl Pts',(-15.4716124964911,-1.30027644702517,
-5.18928239612476));
#75861=CARTESIAN_POINT('Ctrl Pts',(-15.3523465240739,3.66081343996144,-3.90100162460633));
#75862=CARTESIAN_POINT('Ctrl Pts',(-15.2330805516567,5.26134075862523,0.968330387076498));
#75863=CARTESIAN_POINT('Ctrl Pts',(-15.1138145792395,2.03204885203783,4.94875210508029));
#75864=CARTESIAN_POINT('Ctrl Pts',(-14.9960565068663,-2.99821549744162,
4.39341674690176));
#75865=CARTESIAN_POINT('Ctrl Pts',(-14.9180537586321,-4.52637808763146,
1.44204681706245));
#75866=CARTESIAN_POINT('Ctrl Pts',(-14.8798063345369,-4.53091903216787,
-0.00105619164529849));
#75867=CARTESIAN_POINT('Ctrl Pts',(-15.4819936654631,-4.5312138402642,-0.000120197794654437));
#75868=CARTESIAN_POINT('Ctrl Pts',(-15.4818242786339,-4.53121632572514,
-0.00651016932136081));
#75869=CARTESIAN_POINT('Ctrl Pts',(-15.4418995676657,-4.52830675455073,
-1.51263300533729));
#75870=CARTESIAN_POINT('Ctrl Pts',(-15.3622195325584,-2.87505846220515,
-4.51147531916218));
#75871=CARTESIAN_POINT('Ctrl Pts',(-15.2429535601412,2.2387956178267,-4.85872047690402));
#75872=CARTESIAN_POINT('Ctrl Pts',(-15.1236875877241,5.29747440746447,-0.745745015197441));
#75873=CARTESIAN_POINT('Ctrl Pts',(-15.0044216153069,3.49316406084406,4.05181138485548));
#75874=CARTESIAN_POINT('Ctrl Pts',(-14.8851556428897,-1.51780995936451,
5.1298755888585));
#75875=CARTESIAN_POINT('Ctrl Pts',(-14.7943463262751,-4.27229562126168,
2.36517103447762));
#75876=CARTESIAN_POINT('Ctrl Pts',(-14.7432923337996,-4.52511715899487,
0.43264547282851));
#75877=CARTESIAN_POINT('Ctrl Pts',(-14.7319936654631,-4.521456298353,0.00402490267532758));
#75878=CARTESIAN_POINT('Origin',(-19.0048063345371,0.,0.));
#75879=CARTESIAN_POINT('',(-16.379806334537,-4.51785206555557,0.00265012365101876));
#75880=CARTESIAN_POINT('',(-16.2319936654631,-4.52109632398741,-0.0039620509408117));
#75881=CARTESIAN_POINT('',(-19.0048063345371,-4.52375,5.14627461305311E-12));
#75882=CARTESIAN_POINT('Ctrl Pts',(-16.379806334537,-4.51785206555557,0.00265012365101888));
#75883=CARTESIAN_POINT('Ctrl Pts',(-16.3553623241617,-4.51290234764468,
-0.926504029521305));
#75884=CARTESIAN_POINT('Ctrl Pts',(-16.2911629896474,-3.78099521940542,
-3.37397142963533));
#75885=CARTESIAN_POINT('Ctrl Pts',(-16.187208330994,0.228419052524531,-5.34483459461538));
#75886=CARTESIAN_POINT('Ctrl Pts',(-16.0679423585769,4.61866000512981,-2.69949887735067));
#75887=CARTESIAN_POINT('Ctrl Pts',(-15.9486763861597,4.76906677072755,2.42391962238011));
#75888=CARTESIAN_POINT('Ctrl Pts',(-15.8294104137425,0.541545441910157,
5.32222750447519));
#75889=CARTESIAN_POINT('Ctrl Pts',(-15.723120396535,-3.66906666373755,3.55104739187141));
#75890=CARTESIAN_POINT('Ctrl Pts',(-15.6565857034664,-4.51218176763232,
1.01324106700467));
#75891=CARTESIAN_POINT('Ctrl Pts',(-15.6298063345369,-4.51976043794902,
-0.00361086820214504));
#75892=CARTESIAN_POINT('Ctrl Pts',(-16.2319936654631,-4.52109632398741,
-0.00396205094081122));
#75893=CARTESIAN_POINT('Ctrl Pts',(-16.2203562234682,-4.52478620761938,
-0.445522898085508));
#75894=CARTESIAN_POINT('Ctrl Pts',(-16.1689634573343,-4.26236780789856,
-2.39123315065092));
#75895=CARTESIAN_POINT('Ctrl Pts',(-16.0778153670614,-1.47407708230512,
-5.14261359698791));
#75896=CARTESIAN_POINT('Ctrl Pts',(-15.9585493946442,3.52753486740744,-4.02192246785722));
#75897=CARTESIAN_POINT('Ctrl Pts',(-15.839283422227,5.29093324565558,0.790821500180201));
#75898=CARTESIAN_POINT('Ctrl Pts',(-15.7200174498099,2.197346173644,4.87760609314791));
#75899=CARTESIAN_POINT('Ctrl Pts',(-15.6009208642219,-2.90610737191627,
4.48738784408032));
#75900=CARTESIAN_POINT('Ctrl Pts',(-15.5215796027729,-4.53063298458979,
1.49322502577473));
#75901=CARTESIAN_POINT('Ctrl Pts',(-15.4819936654631,-4.5312138402642,-0.000120197794654437));
#75902=CARTESIAN_POINT('Origin',(-19.0048063345371,0.,0.));
#75903=CARTESIAN_POINT('',(-17.129806334537,-4.52905226269683,0.00222857838524445));
#75904=CARTESIAN_POINT('',(-16.9819936654631,-4.51703452062264,0.00191132365274405));
#75905=CARTESIAN_POINT('',(-19.0048063345371,-4.52375,5.14627461305311E-12));
#75906=CARTESIAN_POINT('Ctrl Pts',(-17.129806334537,-4.52905226269683,0.0022285783852446));
#75907=CARTESIAN_POINT('Ctrl Pts',(-17.093894268996,-4.51989244089427,-1.35398501844981));
#75908=CARTESIAN_POINT('Ctrl Pts',(-17.018226879316,-3.1525253686288,-4.22635735705538));
#75909=CARTESIAN_POINT('Ctrl Pts',(-16.902804165497,1.73863948785637,-5.05968774485838));
#75910=CARTESIAN_POINT('Ctrl Pts',(-16.7835381930798,5.19527552722027,-1.27515938975536));
#75911=CARTESIAN_POINT('Ctrl Pts',(-16.6642722206627,3.88345012932081,3.67946867571279));
#75912=CARTESIAN_POINT('Ctrl Pts',(-16.5450062482455,-0.993689040191803,
5.25665841728971));
#75913=CARTESIAN_POINT('Ctrl Pts',(-16.4501842862036,-4.14585089210754,
2.67398054345583));
#75914=CARTESIAN_POINT('Ctrl Pts',(-16.3951176483008,-4.52095248495535,
0.584656535682572));
#75915=CARTESIAN_POINT('Ctrl Pts',(-16.379806334537,-4.51785206555557,0.00265012365101888));
#75916=CARTESIAN_POINT('Ctrl Pts',(-16.9819936654631,-4.51703452062264,
0.00191132365274384));
#75917=CARTESIAN_POINT('Ctrl Pts',(-16.9588881683026,-4.51364627034173,
-0.876727737145359));
#75918=CARTESIAN_POINT('Ctrl Pts',(-16.896027347003,-3.84165527310814,-3.27192923320261));
#75919=CARTESIAN_POINT('Ctrl Pts',(-16.7934112015644,0.0485614395649859,
-5.3495343788269));
#75920=CARTESIAN_POINT('Ctrl Pts',(-16.6741452291472,4.52523009731703,-2.85329470276329));
#75921=CARTESIAN_POINT('Ctrl Pts',(-16.5548792567301,4.84790632702384,2.26213327989446));
#75922=CARTESIAN_POINT('Ctrl Pts',(-16.4356132843129,0.720241778271576,
5.30100788941611));
#75923=CARTESIAN_POINT('Ctrl Pts',(-16.3279847538905,-3.60129660722932,
3.65193354570378));
#75924=CARTESIAN_POINT('Ctrl Pts',(-16.2601115476073,-4.51218098734078,
1.06291809892601));
#75925=CARTESIAN_POINT('Ctrl Pts',(-16.2319936654631,-4.52109632398741,
-0.00396205094081122));
#75926=CARTESIAN_POINT('Origin',(38.546,1.12989188470299E-15,0.));
#75927=CARTESIAN_POINT('',(38.546,4.53891924175741,1.9850259738362));
#75928=CARTESIAN_POINT('Ctrl Pts',(38.546,-0.439158351705697,-4.5083570246951));
#75929=CARTESIAN_POINT('Ctrl Pts',(38.546,-0.315853056119089,-4.52699458320461));
#75930=CARTESIAN_POINT('Ctrl Pts',(38.546,-0.192031275270563,-4.54020498535423));
#75931=CARTESIAN_POINT('Ctrl Pts',(38.546,-0.0679863494789869,-4.54781023322234));
#75932=CARTESIAN_POINT('Ctrl Pts',(38.546,0.0658300049648387,-4.55601457159295));
#75933=CARTESIAN_POINT('Ctrl Pts',(38.546,0.199906495945809,-4.55769712636147));
#75934=CARTESIAN_POINT('Ctrl Pts',(38.546,0.333895251847595,-4.55311715047026));
#75935=CARTESIAN_POINT('Ctrl Pts',(38.546,0.421702187996495,-4.55011575197278));
#75936=CARTESIAN_POINT('Ctrl Pts',(38.546,0.509471668919712,-4.54442374836765));
#75937=CARTESIAN_POINT('Ctrl Pts',(38.546,0.597106546689854,-4.53610218299441));
#75938=CARTESIAN_POINT('Ctrl Pts',(38.546,0.633311340086029,-4.53266427604758));
#75939=CARTESIAN_POINT('Ctrl Pts',(38.546,0.669493157857147,-4.52877745241455));
#75940=CARTESIAN_POINT('Ctrl Pts',(38.546,0.705645122236047,-4.52444556954959));
#75941=CARTESIAN_POINT('Ctrl Pts',(38.546,0.735430140612607,-4.52087660136336));
#75942=CARTESIAN_POINT('Ctrl Pts',(38.546,0.765199499756815,-4.51700477895578));
#75943=CARTESIAN_POINT('Ctrl Pts',(38.546,0.794920189293162,-4.5128365307021));
#75944=CARTESIAN_POINT('Ctrl Pts',(38.546,0.929985258158801,-4.49389401132535));
#75945=CARTESIAN_POINT('Ctrl Pts',(38.546,1.06415017772404,-4.46882312852544));
#75946=CARTESIAN_POINT('Ctrl Pts',(38.546,1.19705809126121,-4.43789314039624));
#75947=CARTESIAN_POINT('Ctrl Pts',(38.546,1.33345806832171,-4.4061504882168));
#75948=CARTESIAN_POINT('Ctrl Pts',(38.546,1.46853485839017,-4.3682367144278));
#75949=CARTESIAN_POINT('Ctrl Pts',(38.546,1.60190114888884,-4.32438793860729));
#75950=CARTESIAN_POINT('Ctrl Pts',(38.546,1.66024890098201,-4.30520409918582));
#75951=CARTESIAN_POINT('Ctrl Pts',(38.546,1.71826916481067,-4.28488357481551));
#75952=CARTESIAN_POINT('Ctrl Pts',(38.546,1.77592884056993,-4.26344303157349));
#75953=CARTESIAN_POINT('Ctrl Pts',(38.546,1.8222598517875,-4.24621501153391));
#75954=CARTESIAN_POINT('Ctrl Pts',(38.546,1.8683580417243,-4.22826381145395));
#75955=CARTESIAN_POINT('Ctrl Pts',(38.546,1.91420593282979,-4.20959724038542));
#75956=CARTESIAN_POINT('Ctrl Pts',(38.546,1.93303706195004,-4.2019303095507));
#75957=CARTESIAN_POINT('Ctrl Pts',(38.546,1.95181787751382,-4.19414596487753));
#75958=CARTESIAN_POINT('Ctrl Pts',(38.546,1.97054439427792,-4.18624627462939));
#75959=CARTESIAN_POINT('Ctrl Pts',(38.546,2.10072143930887,-4.1313317197169));
#75960=CARTESIAN_POINT('Ctrl Pts',(38.546,2.22831997826692,-4.07082932523913));
#75961=CARTESIAN_POINT('Ctrl Pts',(38.546,2.35296605824652,-4.00501001895691));
#75962=CARTESIAN_POINT('Ctrl Pts',(38.546,2.47876377876209,-3.9385825894094));
#75963=CARTESIAN_POINT('Ctrl Pts',(38.546,2.60155501516022,-3.86673927649386));
#75964=CARTESIAN_POINT('Ctrl Pts',(38.546,2.72094480205364,-3.78970660262367));
#75965=CARTESIAN_POINT('Ctrl Pts',(38.546,2.84027235032137,-3.71271408635724));
#75966=CARTESIAN_POINT('Ctrl Pts',(38.546,2.95620277917153,-3.63053727474296));
#75967=CARTESIAN_POINT('Ctrl Pts',(38.546,3.06831947638516,-3.54335537619024));
#75968=CARTESIAN_POINT('Ctrl Pts',(38.546,3.15240699929538,-3.47796895227571));
#75969=CARTESIAN_POINT('Ctrl Pts',(38.546,3.2343489187559,-3.40976617475385));
#75970=CARTESIAN_POINT('Ctrl Pts',(38.546,3.31395719113316,-3.33880703264479));
#75971=CARTESIAN_POINT('Ctrl Pts',(38.546,3.34819221866253,-3.30829150817704));
#75972=CARTESIAN_POINT('Ctrl Pts',(38.546,3.38199551452986,-3.27726606885898));
#75973=CARTESIAN_POINT('Ctrl Pts',(38.546,3.41535137166061,-3.24573478649975));
#75974=CARTESIAN_POINT('Ctrl Pts',(38.546,3.43218348133969,-3.22982339795673));
#75975=CARTESIAN_POINT('Ctrl Pts',(38.546,3.44890367494083,-3.21378110636634));
#75976=CARTESIAN_POINT('Ctrl Pts',(38.546,3.46549235688335,-3.19762579924582));
#75977=CARTESIAN_POINT('Ctrl Pts',(38.546,3.56835841884713,-3.09744708528517));
#75978=CARTESIAN_POINT('Ctrl Pts',(38.546,3.66631150069133,-2.99279463917215));
#75979=CARTESIAN_POINT('Ctrl Pts',(38.546,3.75896065749294,-2.88389381695821));
#75980=CARTESIAN_POINT('Ctrl Pts',(38.546,3.82831127839855,-2.80237834613921));
#75981=CARTESIAN_POINT('Ctrl Pts',(38.546,3.89468982964041,-2.71848149692477));
#75982=CARTESIAN_POINT('Ctrl Pts',(38.546,3.95792179330259,-2.63228181070258));
#75983=CARTESIAN_POINT('Ctrl Pts',(38.546,4.04051693559048,-2.51968566570969));
#75984=CARTESIAN_POINT('Ctrl Pts',(38.546,4.11774512193109,-2.40316146256433));
#75985=CARTESIAN_POINT('Ctrl Pts',(38.546,4.18956529902346,-2.28317878216882));
#75986=CARTESIAN_POINT('Ctrl Pts',(38.546,4.2623473162119,-2.1615892531479));
#75987=CARTESIAN_POINT('Ctrl Pts',(38.546,4.32957582585562,-2.03644727806392));
#75988=CARTESIAN_POINT('Ctrl Pts',(38.546,4.39116358165225,-1.9082119883273));
#75989=CARTESIAN_POINT('Ctrl Pts',(38.546,4.40867475231375,-1.87175100652405));
#75990=CARTESIAN_POINT('Ctrl Pts',(38.546,4.42572961893407,-1.83503980875703));
#75991=CARTESIAN_POINT('Ctrl Pts',(38.546,4.44232547369155,-1.79808864718056));
#75992=CARTESIAN_POINT('Ctrl Pts',(38.546,4.45192170739655,-1.77672234894881));
#75993=CARTESIAN_POINT('Ctrl Pts',(38.546,4.46136446421361,-1.75527581657772));
#75994=CARTESIAN_POINT('Ctrl Pts',(38.546,4.4706531714735,-1.73375101734231));
#75995=CARTESIAN_POINT('Ctrl Pts',(38.546,4.47839968625891,-1.71579995366198));
#75996=CARTESIAN_POINT('Ctrl Pts',(38.546,4.48603931914584,-1.69779368007736));
#75997=CARTESIAN_POINT('Ctrl Pts',(38.546,4.49356556988639,-1.67974851790699));
#75998=CARTESIAN_POINT('Ctrl Pts',(38.546,4.54834464674398,-1.54840857727591));
#75999=CARTESIAN_POINT('Ctrl Pts',(38.546,4.59720230371699,-1.41482472346982));
#76000=CARTESIAN_POINT('Ctrl Pts',(38.546,4.64012638128586,-1.27949345669834));
#76001=CARTESIAN_POINT('Ctrl Pts',(38.546,4.68454708660772,-1.13944361375309));
#76002=CARTESIAN_POINT('Ctrl Pts',(38.546,4.72261371185113,-0.997521695858663));
#76003=CARTESIAN_POINT('Ctrl Pts',(38.546,4.75426513105171,-0.854245649721898));
#76004=CARTESIAN_POINT('Ctrl Pts',(38.546,4.78591655025229,-0.710969603585134));
#76005=CARTESIAN_POINT('Ctrl Pts',(38.546,4.81115300645672,-0.566338522023502));
#76006=CARTESIAN_POINT('Ctrl Pts',(38.546,4.82986142094086,-0.420850963889773));
#76007=CARTESIAN_POINT('Ctrl Pts',(38.546,4.84288525531898,-0.319570020877905));
#76008=CARTESIAN_POINT('Ctrl Pts',(38.546,4.85274434453973,-0.217873614789138));
#76009=CARTESIAN_POINT('Ctrl Pts',(38.546,4.85943963746551,-0.115893038039486));
#76010=CARTESIAN_POINT('Ctrl Pts',(38.546,4.86237760912286,-0.071142786271284));
#76011=CARTESIAN_POINT('Ctrl Pts',(38.546,4.86470620625745,-0.0263378083986588));
#76012=CARTESIAN_POINT('Ctrl Pts',(38.546,4.86642471852824,0.0185107941749964));
#76013=CARTESIAN_POINT('Ctrl Pts',(38.546,4.8673843344193,0.0435542183347263));
#76014=CARTESIAN_POINT('Ctrl Pts',(38.546,4.86815371130291,0.0686112446241784));
#76015=CARTESIAN_POINT('Ctrl Pts',(38.546,4.86873265976743,0.0936799341927062));
#76016=CARTESIAN_POINT('Ctrl Pts',(38.546,4.86919802311952,0.113830345023657));
#76017=CARTESIAN_POINT('Ctrl Pts',(38.546,4.86954030391283,0.13398943210598));
#76018=CARTESIAN_POINT('Ctrl Pts',(38.546,4.86975936328296,0.154138793044496));
#76019=CARTESIAN_POINT('Ctrl Pts',(38.546,4.87134037559417,0.299562326800043));
#76020=CARTESIAN_POINT('Ctrl Pts',(38.546,4.86651295009269,0.44468557075459));
#76021=CARTESIAN_POINT('Ctrl Pts',(38.546,4.85537168171244,0.589123037842825));
#76022=CARTESIAN_POINT('Ctrl Pts',(38.546,4.84413015250928,0.734860304811507));
#76023=CARTESIAN_POINT('Ctrl Pts',(38.546,4.82646070429186,0.879900105190756));
#76024=CARTESIAN_POINT('Ctrl Pts',(38.546,4.80240862941678,1.02385544469749));
#76025=CARTESIAN_POINT('Ctrl Pts',(38.546,4.7784458282956,1.16727646716007));
#76026=CARTESIAN_POINT('Ctrl Pts',(38.546,4.74814767146142,1.30962178718956));
#76027=CARTESIAN_POINT('Ctrl Pts',(38.546,4.7115074706548,1.45050682382756));
#76028=CARTESIAN_POINT('Ctrl Pts',(38.546,4.67545543043744,1.58913032738593));
#76029=CARTESIAN_POINT('Ctrl Pts',(38.546,4.63326321279241,1.72634071218179));
#76030=CARTESIAN_POINT('Ctrl Pts',(38.546,4.5848756392546,1.8617596047089));
#76031=CARTESIAN_POINT('Ctrl Pts',(38.546,4.57013310101999,1.90301850766277));
#76032=CARTESIAN_POINT('Ctrl Pts',(38.546,4.55481512189451,1.94411098781377));
#76033=CARTESIAN_POINT('Ctrl Pts',(38.546,4.53891924175741,1.9850259738362));
#76034=CARTESIAN_POINT('',(38.546,-4.954,-6.06690024297599E-16));
#76035=CARTESIAN_POINT('Origin',(38.546,0.,0.));
#76036=CARTESIAN_POINT('',(38.546,1.34632304271355,4.77431539461067));
#76037=CARTESIAN_POINT('Origin',(38.546,0.,0.));
#76038=CARTESIAN_POINT('Ctrl Pts',(38.546,1.34632304271247,4.77431539461098));
#76039=CARTESIAN_POINT('Ctrl Pts',(38.546,1.21424233318388,4.80662176345812));
#76040=CARTESIAN_POINT('Ctrl Pts',(38.546,1.08105150480208,4.83309789730618));
#76041=CARTESIAN_POINT('Ctrl Pts',(38.546,0.947020732932665,4.85348970562246));
#76042=CARTESIAN_POINT('Ctrl Pts',(38.546,0.803943619664192,4.87525784906835));
#76043=CARTESIAN_POINT('Ctrl Pts',(38.546,0.659908771978632,4.89009318781608));
#76044=CARTESIAN_POINT('Ctrl Pts',(38.546,0.515330126718157,4.89819217175583));
#76045=CARTESIAN_POINT('Ctrl Pts',(38.546,0.424258338069233,4.90329381696977));
#76046=CARTESIAN_POINT('Ctrl Pts',(38.546,0.332970701700517,4.90572146609836));
#76047=CARTESIAN_POINT('Ctrl Pts',(38.546,0.241571546653192,4.9055137924178));
#76048=CARTESIAN_POINT('Ctrl Pts',(38.546,0.187651338017814,4.90539127697246));
#76049=CARTESIAN_POINT('Ctrl Pts',(38.546,0.133692339195287,4.9043514370587));
#76050=CARTESIAN_POINT('Ctrl Pts',(38.546,0.0797162708863841,4.90240097324179));
#76051=CARTESIAN_POINT('Ctrl Pts',(38.546,0.0592483719030999,4.90166135107912));
#76052=CARTESIAN_POINT('Ctrl Pts',(38.546,0.0387799975818231,4.90079080921751));
#76053=CARTESIAN_POINT('Ctrl Pts',(38.546,0.0183214479839144,4.89979031654226));
#76054=CARTESIAN_POINT('Ctrl Pts',(38.546,-0.126232375798732,4.89272114278774));
#76055=CARTESIAN_POINT('Ctrl Pts',(38.546,-0.270424963023004,4.87916423615376));
#76056=CARTESIAN_POINT('Ctrl Pts',(38.546,-0.413845925691374,4.85932065155221));
#76057=CARTESIAN_POINT('Ctrl Pts',(38.546,-0.556818723029428,4.83953907466893));
#76058=CARTESIAN_POINT('Ctrl Pts',(38.546,-0.699025445885051,4.81350970909549));
#76059=CARTESIAN_POINT('Ctrl Pts',(38.546,-0.840049999303419,4.78138245765063));
#76060=CARTESIAN_POINT('Ctrl Pts',(38.546,-0.903801000427365,4.76685913959484));
#76061=CARTESIAN_POINT('Ctrl Pts',(38.546,-0.967310223053341,4.75108905211055));
#76062=CARTESIAN_POINT('Ctrl Pts',(38.546,-1.03053797068624,4.73408300031222));
#76063=CARTESIAN_POINT('Ctrl Pts',(38.546,-1.06559199633794,4.72465469393898));
#76064=CARTESIAN_POINT('Ctrl Pts',(38.546,-1.10055948881135,4.71484645759226));
#76065=CARTESIAN_POINT('Ctrl Pts',(38.546,-1.13543354587295,4.70465989520712));
#76066=CARTESIAN_POINT('Ctrl Pts',(38.546,-1.1551184438112,4.69891002100868));
#76067=CARTESIAN_POINT('Ctrl Pts',(38.546,-1.17477357027183,4.69303960478021));
#76068=CARTESIAN_POINT('Ctrl Pts',(38.546,-1.19439766842355,4.68704891182773));
#76069=CARTESIAN_POINT('Ctrl Pts',(38.546,-1.2137571243417,4.68113900681013));
#76070=CARTESIAN_POINT('Ctrl Pts',(38.546,-1.23307759653258,4.67511472144436));
#76071=CARTESIAN_POINT('Ctrl Pts',(38.546,-1.25235612728143,4.66897721777225));
#76072=CARTESIAN_POINT('Ctrl Pts',(38.546,-1.39105596230319,4.62482080575842));
#76073=CARTESIAN_POINT('Ctrl Pts',(38.546,-1.5276178035149,4.57479853248734));
#76074=CARTESIAN_POINT('Ctrl Pts',(38.546,-1.66163493395825,4.51909969878119));
#76075=CARTESIAN_POINT('Ctrl Pts',(38.546,-1.79558046144293,4.46343062396687));
#76076=CARTESIAN_POINT('Ctrl Pts',(38.546,-1.92698476075658,4.40209070867796));
#76077=CARTESIAN_POINT('Ctrl Pts',(38.546,-2.05542255410814,4.33522083355556));
#76078=CARTESIAN_POINT('Ctrl Pts',(38.546,-2.18368858884634,4.26844038286756));
#76079=CARTESIAN_POINT('Ctrl Pts',(38.546,-2.30899679754021,4.19614442386914));
#76080=CARTESIAN_POINT('Ctrl Pts',(38.546,-2.43089310525813,4.11843031770512));
#76081=CARTESIAN_POINT('Ctrl Pts',(38.546,-2.52231533604658,4.0601447380821));
#76082=CARTESIAN_POINT('Ctrl Pts',(38.546,-2.61181781860713,3.99881054397038));
#76083=CARTESIAN_POINT('Ctrl Pts',(38.546,-2.69919385199506,3.93445456336783));
#76084=CARTESIAN_POINT('Ctrl Pts',(38.546,-2.7345326321001,3.90842612331654));
#76085=CARTESIAN_POINT('Ctrl Pts',(38.546,-2.76952341085071,3.88190326087209));
#76086=CARTESIAN_POINT('Ctrl Pts',(38.546,-2.80415179400507,3.85488722970614));
#76087=CARTESIAN_POINT('Ctrl Pts',(38.546,-2.81829779538271,3.84385094157254));
#76088=CARTESIAN_POINT('Ctrl Pts',(38.546,-2.83238385045348,3.83273192268361));
#76089=CARTESIAN_POINT('Ctrl Pts',(38.546,-2.84640731961621,3.82153155251358));
#76090=CARTESIAN_POINT('Ctrl Pts',(38.546,-2.95689883089296,3.73328335853356));
#76091=CARTESIAN_POINT('Ctrl Pts',(38.546,-3.06309443210339,3.64031882545039));
#76092=CARTESIAN_POINT('Ctrl Pts',(38.546,-3.16460343412711,3.54276990989711));
#76093=CARTESIAN_POINT('Ctrl Pts',(38.546,-3.25260642961082,3.45820010225709));
#76094=CARTESIAN_POINT('Ctrl Pts',(38.546,-3.33708685923698,3.37018388722644));
#76095=CARTESIAN_POINT('Ctrl Pts',(38.546,-3.41776880234159,3.27878373378786));
#76096=CARTESIAN_POINT('Ctrl Pts',(38.546,-3.51096857413409,3.17320281797835));
#76097=CARTESIAN_POINT('Ctrl Pts',(38.546,-3.59910092973385,3.06310654550583));
#76098=CARTESIAN_POINT('Ctrl Pts',(38.546,-3.68202759143973,2.94896297151972));
#76099=CARTESIAN_POINT('Ctrl Pts',(38.546,-3.76531917476244,2.83431710482445));
#76100=CARTESIAN_POINT('Ctrl Pts',(38.546,-3.84335944226955,2.71558740333836));
#76101=CARTESIAN_POINT('Ctrl Pts',(38.546,-3.91596031882729,2.59322728048773));
#76102=CARTESIAN_POINT('Ctrl Pts',(38.546,-3.93941378432771,2.55369926022173));
#76103=CARTESIAN_POINT('Ctrl Pts',(38.546,-3.96229920896436,2.5137922632784));
#76104=CARTESIAN_POINT('Ctrl Pts',(38.546,-3.9846091093253,2.47352133654474));
#76105=CARTESIAN_POINT('Ctrl Pts',(38.546,-3.9934143104391,2.45762733418739));
#76106=CARTESIAN_POINT('Ctrl Pts',(38.546,-4.0021298559497,2.44167664182989));
#76107=CARTESIAN_POINT('Ctrl Pts',(38.546,-4.01075526095843,2.42567018232057));
#76108=CARTESIAN_POINT('Ctrl Pts',(38.546,-4.01985169352743,2.40878962083419));
#76109=CARTESIAN_POINT('Ctrl Pts',(38.546,-4.02884402453685,2.39185413189062));
#76110=CARTESIAN_POINT('Ctrl Pts',(38.546,-4.03772966494529,2.37486939831507));
#76111=CARTESIAN_POINT('Ctrl Pts',(38.546,-4.10267026727469,2.25073666526475));
#76112=CARTESIAN_POINT('Ctrl Pts',(38.546,-4.16195655546587,2.12390033921895));
#76113=CARTESIAN_POINT('Ctrl Pts',(38.546,-4.21548626120384,1.99483096966602));
#76114=CARTESIAN_POINT('Ctrl Pts',(38.546,-4.26923983167619,1.86522182355849));
#76115=CARTESIAN_POINT('Ctrl Pts',(38.546,-4.31718883006406,1.73336008190174));
#76116=CARTESIAN_POINT('Ctrl Pts',(38.546,-4.35918181423245,1.59970128041928));
#76117=CARTESIAN_POINT('Ctrl Pts',(38.546,-4.39954043011255,1.47124448376979));
#76118=CARTESIAN_POINT('Ctrl Pts',(38.546,-4.43439753246674,1.34112700894506));
#76119=CARTESIAN_POINT('Ctrl Pts',(38.546,-4.46357390460294,1.20974588256244));
#76120=CARTESIAN_POINT('Ctrl Pts',(38.546,-4.48425134443962,1.11663542579388));
#76121=CARTESIAN_POINT('Ctrl Pts',(38.546,-4.50207458172136,1.02289014857479));
#76122=CARTESIAN_POINT('Ctrl Pts',(38.546,-4.51701982161582,0.928629909937474));
#76123=CARTESIAN_POINT('Ctrl Pts',(38.546,-4.52402075405636,0.884474742995445));
#76124=CARTESIAN_POINT('Ctrl Pts',(38.546,-4.53038999373665,0.8402065928306));
#76125=CARTESIAN_POINT('Ctrl Pts',(38.546,-4.53612425080577,0.795837921409192));
#76126=CARTESIAN_POINT('Ctrl Pts',(38.546,-4.53952194720462,0.769548330047427));
#76127=CARTESIAN_POINT('Ctrl Pts',(38.546,-4.54269669918852,0.743223449100096));
#76128=CARTESIAN_POINT('Ctrl Pts',(38.546,-4.54564773289263,0.716865893342667));
#76129=CARTESIAN_POINT('Ctrl Pts',(38.546,-4.54745751221922,0.700701605065332));
#76130=CARTESIAN_POINT('Ctrl Pts',(38.546,-4.54918297077606,0.684526320540122));
#76131=CARTESIAN_POINT('Ctrl Pts',(38.546,-4.55082307057052,0.668350423530228));
#76132=CARTESIAN_POINT('Ctrl Pts',(38.546,-4.56547759744107,0.52381646395733));
#76133=CARTESIAN_POINT('Ctrl Pts',(38.546,-4.57334695024406,0.379020687625459));
#76134=CARTESIAN_POINT('Ctrl Pts',(38.546,-4.57444969521142,0.234390006360559));
#76135=CARTESIAN_POINT('Ctrl Pts',(38.546,-4.57549951960631,0.0967001307002065));
#76136=CARTESIAN_POINT('Ctrl Pts',(38.546,-4.57041614699662,-0.0408408986859376));
#76137=CARTESIAN_POINT('Ctrl Pts',(38.546,-4.55916271844398,-0.177865018424011));
#76138=CARTESIAN_POINT('Ctrl Pts',(38.546,-4.5480089654111,-0.313675468008928));
#76139=CARTESIAN_POINT('Ctrl Pts',(38.546,-4.53079389772483,-0.448978801903289));
#76140=CARTESIAN_POINT('Ctrl Pts',(38.546,-4.50743176272214,-0.583406337128876));
#76141=CARTESIAN_POINT('Ctrl Pts',(38.546,-4.48453671791127,-0.715146199194071));
#76142=CARTESIAN_POINT('Ctrl Pts',(38.546,-4.45573780575909,-0.846045505627378));
#76143=CARTESIAN_POINT('Ctrl Pts',(38.546,-4.42090797245811,-0.97573816109587));
#76144=CARTESIAN_POINT('Ctrl Pts',(38.546,-4.41413948486699,-1.00094135749399));
#76145=CARTESIAN_POINT('Ctrl Pts',(38.546,-4.407143104959,-1.02609891192132));
#76146=CARTESIAN_POINT('Ctrl Pts',(38.546,-4.39991769847472,-1.05120802372743));
#76147=CARTESIAN_POINT('Ctrl Pts',(-17.8668049533188,-1.93258782773145,
4.09016116438023));
#76148=CARTESIAN_POINT('Ctrl Pts',(-17.8469272912493,-2.61370891938372,
3.76833366711637));
#76149=CARTESIAN_POINT('Ctrl Pts',(-17.8071719671103,-3.80128785052217,
2.77774777382202));
#76150=CARTESIAN_POINT('Ctrl Pts',(-17.7276613188322,-4.98891923544753,
-0.109469461415501));
#76151=CARTESIAN_POINT('Ctrl Pts',(-17.6282730084845,-3.45849333686121,
-4.08082754129702));
#76152=CARTESIAN_POINT('Ctrl Pts',(-17.5090070360674,1.56940258829812,-5.11725866595573));
#76153=CARTESIAN_POINT('Ctrl Pts',(-17.3897410636502,5.14844039432527,-1.44815814548532));
#76154=CARTESIAN_POINT('Ctrl Pts',(-17.270475091233,4.00553813139823,3.54623540470151));
#76155=CARTESIAN_POINT('Ctrl Pts',(-17.1512091188158,-0.816602122674766,
5.28738771244033));
#76156=CARTESIAN_POINT('Ctrl Pts',(-17.0319431463987,-4.88794592317846,
2.17368458761069));
#76157=CARTESIAN_POINT('Ctrl Pts',(-16.9126771739815,-4.47285648319269,
-2.93483056265198));
#76158=CARTESIAN_POINT('Ctrl Pts',(-16.7934112015644,0.0485614395649859,
-5.3495343788269));
#76159=CARTESIAN_POINT('Ctrl Pts',(-16.6741452291472,4.52523009731703,-2.85329470276329));
#76160=CARTESIAN_POINT('Ctrl Pts',(-16.5548792567301,4.84790632702384,2.26213327989446));
#76161=CARTESIAN_POINT('Ctrl Pts',(-16.4356132843129,0.720241778271576,
5.30100788941611));
#76162=CARTESIAN_POINT('Ctrl Pts',(-16.3163473118957,-4.06856724720163,
3.47362574065601));
#76163=CARTESIAN_POINT('Ctrl Pts',(-16.1970813394785,-5.12251561539824,
-1.54247163636852));
#76164=CARTESIAN_POINT('Ctrl Pts',(-16.0778153670614,-1.47407708230512,
-5.14261359698791));
#76165=CARTESIAN_POINT('Ctrl Pts',(-15.9585493946442,3.52753486740744,-4.02192246785722));
#76166=CARTESIAN_POINT('Ctrl Pts',(-15.839283422227,5.29093324565558,0.790821500180201));
#76167=CARTESIAN_POINT('Ctrl Pts',(-15.7200174498099,2.197346173644,4.87760609314791));
#76168=CARTESIAN_POINT('Ctrl Pts',(-15.6007514773927,-2.91336583201067,
4.48683285057177));
#76169=CARTESIAN_POINT('Ctrl Pts',(-15.4814855049756,-5.34965909419724,
-0.022774426867852));
#76170=CARTESIAN_POINT('Ctrl Pts',(-15.3622195325584,-2.87505846220515,
-4.51147531916218));
#76171=CARTESIAN_POINT('Ctrl Pts',(-15.2429535601412,2.2387956178267,-4.85872047690402));
#76172=CARTESIAN_POINT('Ctrl Pts',(-15.1236875877241,5.29747440746447,-0.745745015197441));
#76173=CARTESIAN_POINT('Ctrl Pts',(-15.0044216153069,3.49316406084406,4.05181138485548));
#76174=CARTESIAN_POINT('Ctrl Pts',(-14.8851556428897,-1.51780995936451,
5.1298755888585));
#76175=CARTESIAN_POINT('Ctrl Pts',(-14.7658896704726,-5.13546091438147,
1.49880347624965));
#76176=CARTESIAN_POINT('Ctrl Pts',(-14.6466236980554,-4.03884831250948,
-3.50814409050182));
#76177=CARTESIAN_POINT('Ctrl Pts',(-14.5273577256382,0.765356598558913,
-5.29467656481004));
#76178=CARTESIAN_POINT('Ctrl Pts',(-14.4080917532211,4.86697750131595,-2.22078829592513));
#76179=CARTESIAN_POINT('Ctrl Pts',(-14.2888257808039,4.50079794053571,2.89174489712377));
#76180=CARTESIAN_POINT('Ctrl Pts',(-14.1695598083868,0.00296436731219236,
5.34970670821892));
#76181=CARTESIAN_POINT('Ctrl Pts',(-14.0502938359696,-4.49759044353025,
2.89673106351802));
#76182=CARTESIAN_POINT('Ctrl Pts',(-13.9310278635524,-4.8694356679322,-2.21539317675726));
#76183=CARTESIAN_POINT('Ctrl Pts',(-13.8117618911353,-0.771223875207531,
-5.29382511857655));
#76184=CARTESIAN_POINT('Ctrl Pts',(-13.6924959187181,4.03495798434998,-3.51261792917751));
#76185=CARTESIAN_POINT('Ctrl Pts',(-13.5732299463009,5.13711878645237,1.49311125696483));
#76186=CARTESIAN_POINT('Ctrl Pts',(-13.4539639738838,1.52349413715743,5.12819035000159));
#76187=CARTESIAN_POINT('Ctrl Pts',(-13.3346980014666,-3.48867155936125,
4.0556801405828));
#76188=CARTESIAN_POINT('Ctrl Pts',(-13.2154320290494,-5.29829760899626,
-0.73987370429712));
#76189=CARTESIAN_POINT('Ctrl Pts',(-13.0961660566323,-2.24417885919362,
-4.85623639249116));
#76190=CARTESIAN_POINT('Ctrl Pts',(-12.9769000842151,2.8700569434679,-4.51465876817511));
#76191=CARTESIAN_POINT('Ctrl Pts',(-12.8576341117979,5.34963052761172,-0.0287031331433309));
#76192=CARTESIAN_POINT('Ctrl Pts',(-12.7383681393808,2.91833658830642,4.48360147751333));
#76193=CARTESIAN_POINT('Ctrl Pts',(-12.6191021669636,-2.19193944145102,
4.88003812862352));
#76194=CARTESIAN_POINT('Ctrl Pts',(-12.4998361945465,-5.29005329274958,
0.796684888570813));
#76195=CARTESIAN_POINT('Ctrl Pts',(-12.3805702221293,-3.53199048313817,
-4.01801118450772));
#76196=CARTESIAN_POINT('Ctrl Pts',(-12.2613042497121,1.4683779898736,-5.14424306683332));
#76197=CARTESIAN_POINT('Ctrl Pts',(-12.142038277295,5.12080107761086,-1.54814953261863));
#76198=CARTESIAN_POINT('Ctrl Pts',(-12.0227723048778,4.07241808607112,3.46911827184497));
#76199=CARTESIAN_POINT('Ctrl Pts',(-11.9035063324606,-0.714373682966412,
5.30179600634471));
#76200=CARTESIAN_POINT('Ctrl Pts',(-11.7842403600435,-4.84538287016409,
2.26751747365443));
#76201=CARTESIAN_POINT('Ctrl Pts',(-11.6649743876263,-4.52841508905532,
-2.84830255292936));
#76202=CARTESIAN_POINT('Ctrl Pts',(-11.5457084152091,-0.0544412345818395,
-5.34943051209986));
#76203=CARTESIAN_POINT('Ctrl Pts',(-11.4264424427919,4.46950872374863,-2.93987455857264));
#76204=CARTESIAN_POINT('Ctrl Pts',(-11.3071764703748,4.89052762470212,2.16843496647541));
#76205=CARTESIAN_POINT('Ctrl Pts',(-11.1879104979576,0.822127460035971,
5.28615901115948));
#76206=CARTESIAN_POINT('Ctrl Pts',(-11.0686445255405,-4.00097137452672,
3.55128127751458));
#76207=CARTESIAN_POINT('Ctrl Pts',(-10.9493785531233,-5.15124826671406,
-1.44361073232473));
#76208=CARTESIAN_POINT('Ctrl Pts',(-10.8301125807061,-1.57276909104567,
-5.11329326736293));
#76209=CARTESIAN_POINT('Ctrl Pts',(-10.710846608289,3.44948468012718,-4.08906176199085));
#76210=CARTESIAN_POINT('Ctrl Pts',(-10.5915806358718,5.30517167611101,0.688857125097259));
#76211=CARTESIAN_POINT('Ctrl Pts',(-10.4723146634547,2.29080359893313,4.83441718544467));
#76212=CARTESIAN_POINT('Ctrl Pts',(-10.3530486910375,-2.82648222901952,
4.54206658480968));
#76213=CARTESIAN_POINT('Ctrl Pts',(-10.2337827186203,-5.34910666634805,
0.0801780757980781));
#76214=CARTESIAN_POINT('Ctrl Pts',(-10.1145167462031,-2.96134447573091,
-4.45531250844044));
#76215=CARTESIAN_POINT('Ctrl Pts',(-9.995250773786,2.14488029590958,-4.90090391336402));
#76216=CARTESIAN_POINT('Ctrl Pts',(-9.87598480136882,5.28214236395734,-0.847551000645274));
#76217=CARTESIAN_POINT('Ctrl Pts',(-9.75671882895166,3.57048986575489,3.98383894884689));
#76218=CARTESIAN_POINT('Ctrl Pts',(-9.6374528565345,-1.41881005763682,5.15813422393762));
#76219=CARTESIAN_POINT('Ctrl Pts',(-9.51818688411732,-5.10566709305165,
1.59735224253676));
#76220=CARTESIAN_POINT('Ctrl Pts',(-9.39892091170017,-4.10561078306872,
-3.42977123869183));
#76221=CARTESIAN_POINT('Ctrl Pts',(-9.279654939283,0.663324621354469,-5.30842454015434));
#76222=CARTESIAN_POINT('Ctrl Pts',(-9.16038896686585,4.82333959217,-2.31403669599532));
#76223=CARTESIAN_POINT('Ctrl Pts',(-9.04112299444865,4.55561293942915,2.80459647684182));
#76224=CARTESIAN_POINT('Ctrl Pts',(-8.92185702203153,0.105913061027885,
5.34865899785279));
#76225=CARTESIAN_POINT('Ctrl Pts',(-8.80259104961433,-4.44101316020701,
2.98274584278913));
#76226=CARTESIAN_POINT('Ctrl Pts',(-8.68332507719718,-4.91116675441572,
-2.12127597500409));
#76227=CARTESIAN_POINT('Ctrl Pts',(-8.56405910478001,-0.872954921887009,
-5.27800344412176));
#76228=CARTESIAN_POINT('Ctrl Pts',(-8.44479313236285,3.96661430405479,-3.58961580321287));
#76229=CARTESIAN_POINT('Ctrl Pts',(-8.32552715994568,5.16490077910572,1.39397653990334));
#76230=CARTESIAN_POINT('Ctrl Pts',(-8.20626118752853,1.62189841803372,5.09792273121));
#76231=CARTESIAN_POINT('Ctrl Pts',(-8.08699521511134,-3.40997840387161,
4.12206476622297));
#76232=CARTESIAN_POINT('Ctrl Pts',(-7.96772924269419,-5.31155452317641,
-0.637776762772118));
#76233=CARTESIAN_POINT('Ctrl Pts',(-7.84846327027703,-2.33721622703428,
-4.8121503467676));
#76234=CARTESIAN_POINT('Ctrl Pts',(-7.72919729785987,2.78264580301424,-4.56905383933861));
#76235=CARTESIAN_POINT('Ctrl Pts',(-7.60993132544269,5.34808751697683,-0.131645594550073));
#76236=CARTESIAN_POINT('Ctrl Pts',(-7.49066535302554,3.00407816434195,4.42661101005405));
#76237=CARTESIAN_POINT('Ctrl Pts',(-7.37139938060837,-2.09762255015898,
4.92131591028987));
#76238=CARTESIAN_POINT('Ctrl Pts',(-7.2521334081912,-5.27374234746165,0.898338635703456));
#76239=CARTESIAN_POINT('Ctrl Pts',(-7.13286743577404,-3.60865864715558,
-3.94929783887176));
#76240=CARTESIAN_POINT('Ctrl Pts',(-7.01360146335687,1.36911075397815,-5.17154777558412));
#76241=CARTESIAN_POINT('Ctrl Pts',(-6.89433549093971,5.09006036110679,-1.64640704933419));
#76242=CARTESIAN_POINT('Ctrl Pts',(-6.77506951852255,4.13842333057186,3.3901066338371));
#76243=CARTESIAN_POINT('Ctrl Pts',(-6.65580354610538,-0.612214140739847,
5.31456155272341));
#76244=CARTESIAN_POINT('Ctrl Pts',(-6.53653757368821,-4.80084970824945,
2.36034165548316));
#76245=CARTESIAN_POINT('Ctrl Pts',(-6.41727160127105,-4.58238897340408,
-2.76063071565767));
#76246=CARTESIAN_POINT('Ctrl Pts',(-6.29800562885389,-0.157375080700092,
-5.34739223694899));
#76247=CARTESIAN_POINT('Ctrl Pts',(-6.17873965643672,4.41210639136683,-3.02534094658233));
#76248=CARTESIAN_POINT('Ctrl Pts',(-6.05947368401956,4.93135114605077,2.07392056891087));
#76249=CARTESIAN_POINT('Ctrl Pts',(-5.94020771160239,0.923701554504711,
5.2693591726142));
#76250=CARTESIAN_POINT('Ctrl Pts',(-5.82094173918523,-3.93188995414451,
3.62761795677345));
#76251=CARTESIAN_POINT('Ctrl Pts',(-5.70167576676806,-5.17807505950615,
-1.34421327546196));
#76252=CARTESIAN_POINT('Ctrl Pts',(-5.5824097943509,-1.67087756910494,-5.08208016474257));
#76253=CARTESIAN_POINT('Ctrl Pts',(-5.46314382193374,3.37015638858599,-4.15468609744235));
#76254=CARTESIAN_POINT('Ctrl Pts',(-5.34387784951657,5.31744555918776,0.586637346988937));
#76255=CARTESIAN_POINT('Ctrl Pts',(-5.22461187709941,2.38341244602753,4.7894379382062));
#76256=CARTESIAN_POINT('Ctrl Pts',(-5.10534590468224,-2.73855172438397,
4.59561803293978));
#76257=CARTESIAN_POINT('Ctrl Pts',(-4.98607993226508,-5.34657317386386,
0.183100923884053));
#76258=CARTESIAN_POINT('Ctrl Pts',(-4.86681395984791,-3.04653369731289,
-4.39749963990275));
#76259=CARTESIAN_POINT('Ctrl Pts',(-4.74754798743075,2.05017057992043,-4.94127222939968));
#76260=CARTESIAN_POINT('Ctrl Pts',(-4.62828201501358,5.26485402104248,-0.949043091182221));
#76261=CARTESIAN_POINT('Ctrl Pts',(-4.50901604259642,3.64649329319062,3.91439105283614));
#76262=CARTESIAN_POINT('Ctrl Pts',(-4.38975007017925,-1.31928468068921,
5.18448247977621));
#76263=CARTESIAN_POINT('Ctrl Pts',(-4.27048409776209,-5.07398232684534,
1.69530941089495));
#76264=CARTESIAN_POINT('Ctrl Pts',(-4.15121812534492,-4.17085269037897,
-3.3501281299327));
#76265=CARTESIAN_POINT('Ctrl Pts',(-4.03195215292777,0.561046973578825,
-5.32020647580954));
#76266=CARTESIAN_POINT('Ctrl Pts',(-3.91268618051059,4.77791530080097,-2.40642806461773));
#76267=CARTESIAN_POINT('Ctrl Pts',(-3.79342020809343,4.60874071171544,2.71640934028442));
#76268=CARTESIAN_POINT('Ctrl Pts',(-3.67415423567627,0.208822528592261,
5.3456303466813));
#76269=CARTESIAN_POINT('Ctrl Pts',(-3.5548882632591,-4.38279109378327,3.06765592595745));
#76270=CARTESIAN_POINT('Ctrl Pts',(-3.43562229084194,-4.95107893068038,
-2.0263731329596));
#76271=CARTESIAN_POINT('Ctrl Pts',(-3.31635631842477,-0.97436265912244,
-5.26022699703307));
#76272=CARTESIAN_POINT('Ctrl Pts',(-3.19709034600761,3.89680154001646,-3.66528421947511));
#76273=CARTESIAN_POINT('Ctrl Pts',(-3.07782437359044,5.19076988807344,1.29432554671451));
#76274=CARTESIAN_POINT('Ctrl Pts',(-2.95855840117328,1.71970200914856,5.0657670348663));
#76275=CARTESIAN_POINT('Ctrl Pts',(-2.83929242875612,-3.33002232149737,
4.18692273515254));
#76276=CARTESIAN_POINT('Ctrl Pts',(-2.72002645633895,-5.32284423867826,
-0.53544361288319));
#76277=CARTESIAN_POINT('Ctrl Pts',(-2.60076048392179,-2.42938797848125,
-4.76628206276323));
#76278=CARTESIAN_POINT('Ctrl Pts',(-2.48149451150462,2.69420407591751,-4.62175670596335));
#76279=CARTESIAN_POINT('Ctrl Pts',(-2.36222853908746,5.34456377722621,-0.234539299413323));
#76280=CARTESIAN_POINT('Ctrl Pts',(-2.2429625666703,3.0887071435723,4.36798109348626));
#76281=CARTESIAN_POINT('Ctrl Pts',(-2.12369659425313,-2.00252877889888,
4.96077102288439));
#76282=CARTESIAN_POINT('Ctrl Pts',(-2.00443062183597,-5.25547820769376,
0.999659672220339));
#76283=CARTESIAN_POINT('Ctrl Pts',(-1.8851646494188,-3.68399030064885,-3.87912182285284));
#76284=CARTESIAN_POINT('Ctrl Pts',(-1.76589867700163,1.26933645129948,-5.19693713885497));
#76285=CARTESIAN_POINT('Ctrl Pts',(-1.64663270458447,5.05743447897554,-1.74405479921852));
#76286=CARTESIAN_POINT('Ctrl Pts',(-1.52736673216731,4.20289585976879,3.30983942869535));
#76287=CARTESIAN_POINT('Ctrl Pts',(-1.40810075975014,-0.509827857576372,
5.32535878673416));
#76288=CARTESIAN_POINT('Ctrl Pts',(-1.28883478733298,-4.75453849338273,
2.45229165613506));
#76289=CARTESIAN_POINT('Ctrl Pts',(-1.16956881491581,-4.63466571438527,
-2.67193644529762));
#76290=CARTESIAN_POINT('Ctrl Pts',(-1.05030284249865,-0.260250641047462,
-5.34337349018783));
#76291=CARTESIAN_POINT('Ctrl Pts',(-0.931036870081484,4.35306998183813,
-3.10968686285734));
#76292=CARTESIAN_POINT('Ctrl Pts',(-0.811770897664319,4.97034828165621,
1.97863806969469));
#76293=CARTESIAN_POINT('Ctrl Pts',(-0.692504925247154,1.02493354489289,
5.25060776295097));
#76294=CARTESIAN_POINT('Ctrl Pts',(-0.573238952829991,-3.86135231060077,
3.70261110369774));
#76295=CARTESIAN_POINT('Ctrl Pts',(-0.453972980412826,-5.20298408935945,
-1.24431797289934));
#76296=CARTESIAN_POINT('Ctrl Pts',(-0.33470700799566,-1.76836721737897,
-5.04898485205759));
#76297=CARTESIAN_POINT('Ctrl Pts',(-0.215441035578497,3.2895799187264,-4.21877169447693));
#76298=CARTESIAN_POINT('Ctrl Pts',(-0.0961750631613321,5.32775006176976,
0.484200300619735));
#76299=CARTESIAN_POINT('Ctrl Pts',(0.0230909092558323,2.4751385673978,4.74268486450319));
#76300=CARTESIAN_POINT('Ctrl Pts',(0.142356881672996,-2.64960696388247,
4.64746743815955));
#76301=CARTESIAN_POINT('Ctrl Pts',(0.261622854090164,-5.34205951311933,
0.285955958320836));
#76302=CARTESIAN_POINT('Ctrl Pts',(0.380888826507324,-3.13059459816773,
-4.33805810400583));
#76303=CARTESIAN_POINT('Ctrl Pts',(0.500154798924492,1.95470155837633,-4.9798104852985));
#76304=CARTESIAN_POINT('Ctrl Pts',(0.619420771341654,5.24561577554724,-1.05018369209291));
#76305=CARTESIAN_POINT('Ctrl Pts',(0.738686743758821,3.72114619758183,3.84349341459433));
#76306=CARTESIAN_POINT('Ctrl Pts',(0.857952716175984,-1.21927069064937,
5.20891059961017));
#76307=CARTESIAN_POINT('Ctrl Pts',(0.977218688593149,-5.040418349707,1.79263870083876));
#76308=CARTESIAN_POINT('Ctrl Pts',(1.09648466101031,-4.23454987177837,-3.26924426056382));
#76309=CARTESIAN_POINT('Ctrl Pts',(1.21575063342748,0.458561535247667,-5.33001800843103));
#76310=CARTESIAN_POINT('Ctrl Pts',(1.33501660584464,4.73072145051602,-2.49792818340231));
#76311=CARTESIAN_POINT('Ctrl Pts',(1.4542825782618,4.66016158094803,2.62721614856175));
#76312=CARTESIAN_POINT('Ctrl Pts',(1.57354855067898,0.311654656198974,5.34062187643698));
#76313=CARTESIAN_POINT('Ctrl Pts',(1.69281452309613,-4.32294580748887,3.1514298655249));
#76314=CARTESIAN_POINT('Ctrl Pts',(1.81208049551331,-4.98915741477735,-1.93071979903348));
#76315=CARTESIAN_POINT('Ctrl Pts',(1.93134646793046,-1.07540952932231,-5.24050236103854));
#76316=CARTESIAN_POINT('Ctrl Pts',(2.05061244034763,3.82554554823664,-3.73959515324518));
#76317=CARTESIAN_POINT('Ctrl Pts',(2.16987841276479,5.21471653241851,1.19419518435166));
#76318=CARTESIAN_POINT('Ctrl Pts',(2.28914438518196,1.81686868775421,5.03173517022369));
#76319=CARTESIAN_POINT('Ctrl Pts',(2.40841035759912,-3.24883292494357,4.2502300264351));
#76320=CARTESIAN_POINT('Ctrl Pts',(2.52767633001628,-5.33216257421889,-0.43291215495413));
#76321=CARTESIAN_POINT('Ctrl Pts',(2.64694230243346,-2.52065997660762,-4.71864852835388));
#76322=CARTESIAN_POINT('Ctrl Pts',(2.76620827485062,2.60476451764482,-4.67274784890289));
#76323=CARTESIAN_POINT('Ctrl Pts',(2.88547424726778,5.33906061341968,-0.337346139800582));
#76324=CARTESIAN_POINT('Ctrl Pts',(3.00474021968495,3.17219218262773,4.3077334421112));
#76325=CARTESIAN_POINT('Ctrl Pts',(3.1240061921021,-1.90669334680315,4.99838885372723));
#76326=CARTESIAN_POINT('Ctrl Pts',(3.24327216451928,-5.2352676377918,1.10061047264574));
#76327=CARTESIAN_POINT('Ctrl Pts',(3.36253813693643,-3.7579575436257,-3.8075091269903));
#76328=CARTESIAN_POINT('Ctrl Pts',(3.48180410935361,1.16909203446164,-5.22040175338702));
#76329=CARTESIAN_POINT('Ctrl Pts',(3.60107008177076,5.0229355146086,-1.84105661724222));
#76330=CARTESIAN_POINT('Ctrl Pts',(3.72033605418794,4.2658117954781,3.2283463843534));
#76331=CARTESIAN_POINT('Ctrl Pts',(3.83960202660509,-0.407252753478724,
5.33418370949033));
#76332=CARTESIAN_POINT('Ctrl Pts',(3.95886799902227,-4.7064663774845,2.54333342081128));
#76333=CARTESIAN_POINT('Ctrl Pts',(4.07813397143942,-4.68522595067329,-2.58225259084879));
#76334=CARTESIAN_POINT('Ctrl Pts',(4.1973999438566,-0.363029814411452,-5.33737576020804));
#76335=CARTESIAN_POINT('Ctrl Pts',(4.31666591627375,4.29242136001334,-3.19288106886381));
#76336=CARTESIAN_POINT('Ctrl Pts',(4.43593188869093,5.0075045884559,1.88262275785692));
#76337=CARTESIAN_POINT('Ctrl Pts',(4.55519786110808,1.12578593870418,5.22991172698201));
#76338=CARTESIAN_POINT('Ctrl Pts',(4.67446383352525,-3.78938456836793,3.77623294366524));
#76339=CARTESIAN_POINT('Ctrl Pts',(4.79372980594241,-5.22596613091239,-1.14396182207461));
#76340=CARTESIAN_POINT('Ctrl Pts',(4.91299577835959,-1.86520192939329,-5.01401958655883));
#76341=CARTESIAN_POINT('Ctrl Pts',(5.03226175077674,3.20778511302202,-4.28129481821586));
#76342=CARTESIAN_POINT('Ctrl Pts',(5.15152772319392,5.33608136745939,0.381583924793045));
#76343=CARTESIAN_POINT('Ctrl Pts',(5.27079369561107,2.56594799116161,4.69417527990397));
#76344=CARTESIAN_POINT('Ctrl Pts',(5.39005966802824,-2.5596808892866,4.69759559741243));
#76345=CARTESIAN_POINT('Ctrl Pts',(5.5093256404454,-5.33556735580349,0.388705085498125));
#76346=CARTESIAN_POINT('Ctrl Pts',(5.62859161286257,-3.21349604532058,-4.27700991564396));
#76347=CARTESIAN_POINT('Ctrl Pts',(5.74785758527973,1.85850858938807,-5.01650440794967));
#76348=CARTESIAN_POINT('Ctrl Pts',(5.86712355769689,5.22443475258933,-1.1509353447283));
#76349=CARTESIAN_POINT('Ctrl Pts',(5.98638953011406,3.79442093031935,3.77117229192225));
#76350=CARTESIAN_POINT('Ctrl Pts',(6.10565550253122,-1.11880512891234,5.2314095361888));
#76351=CARTESIAN_POINT('Ctrl Pts',(6.2249214749484,-5.00498759246291,1.88930406528444));
#76352=CARTESIAN_POINT('Ctrl Pts',(6.34418744736554,-4.29667873624274,-3.18714958690789));
#76353=CARTESIAN_POINT('Ctrl Pts',(6.46345341978273,0.355906263086912,-5.33785550419859));
#76354=CARTESIAN_POINT('Ctrl Pts',(6.58271939219988,4.68177552013038,-2.58850316416958));
#76355=CARTESIAN_POINT('Ctrl Pts',(6.70198536461705,4.70985650278392,2.5370499354549));
#76356=CARTESIAN_POINT('Ctrl Pts',(6.8212513370342,0.41437135872153,5.33363544206753));
#76357=CARTESIAN_POINT('Ctrl Pts',(6.94051730945138,-4.2614994657519,3.23403663479625));
#76358=CARTESIAN_POINT('Ctrl Pts',(7.05978328186854,-5.02538810387791,-1.83435139959879));
#76359=CARTESIAN_POINT('Ctrl Pts',(7.1790492542857,-1.17605810855195,-5.21883684139645));
#76360=CARTESIAN_POINT('Ctrl Pts',(7.29831522670288,3.75287271923664,-3.81252108256694));
#76361=CARTESIAN_POINT('Ctrl Pts',(7.41758119912002,5.23673184321061,1.09362253730968));
#76362=CARTESIAN_POINT('Ctrl Pts',(7.53684717153721,1.91336246699203,4.99583974139622));
#76363=CARTESIAN_POINT('Ctrl Pts',(7.65611314395436,-3.16644028368856,4.31196319344709));
#76364=CARTESIAN_POINT('Ctrl Pts',(7.77537911637153,-5.33950607863965,-0.330220362754721));
#76365=CARTESIAN_POINT('Ctrl Pts',(7.89464508878868,-2.6109984177212,-4.66926738519707));
#76366=CARTESIAN_POINT('Ctrl Pts',(8.01391106120587,2.51436025322183,-4.72200838296865));
#76367=CARTESIAN_POINT('Ctrl Pts',(8.13317703362301,5.33158006372075,-0.440028039951035));
#76368=CARTESIAN_POINT('Ctrl Pts',(8.25244300604019,3.25450236181101,4.2458903693777));
#76369=CARTESIAN_POINT('Ctrl Pts',(8.37170897845735,-1.81015174768696,5.0341554705982));
#76370=CARTESIAN_POINT('Ctrl Pts',(8.49097495087451,-5.21311812298558,1.20115364862579));
#76371=CARTESIAN_POINT('Ctrl Pts',(8.61024092329168,-3.83053298142016,-3.73448627391507));
#76372=CARTESIAN_POINT('Ctrl Pts',(8.72950689570885,1.06841463020081,-5.2419329287755));
#76373=CARTESIAN_POINT('Ctrl Pts',(8.848772868126,4.98657624511604,-1.93737657760491));
#76374=CARTESIAN_POINT('Ctrl Pts',(8.96803884054318,4.32714783601959,3.14565768274914));
#76375=CARTESIAN_POINT('Ctrl Pts',(9.08730481296034,-0.304526818381393,
5.34103305257461));
#76376=CARTESIAN_POINT('Ctrl Pts',(9.2065707853775,-4.65665116464621,2.63343323108956));
#76377=CARTESIAN_POINT('Ctrl Pts',(9.32583675779467,-4.73405095667114,-2.49161236781501));
#76378=CARTESIAN_POINT('Ctrl Pts',(9.44510273021184,-0.46567453527804,-5.32940126834165));
#76379=CARTESIAN_POINT('Ctrl Pts',(9.56436870262899,4.23018298784551,-3.27489275261803));
#76380=CARTESIAN_POINT('Ctrl Pts',(9.68363467504617,5.04280630516079,1.78591019383345));
#76381=CARTESIAN_POINT('Ctrl Pts',(9.80290064746333,1.2262213840307,5.20727872973531));
#76382=CARTESIAN_POINT('Ctrl Pts',(9.92216661988049,-3.71601338157262,3.84845620993417));
#76383=CARTESIAN_POINT('Ctrl Pts',(10.0414325922977,-5.24701267248705,-1.04318199110605));
#76384=CARTESIAN_POINT('Ctrl Pts',(10.1606985647148,-1.96134584123722,-4.97719731805657));
#76385=CARTESIAN_POINT('Ctrl Pts',(10.279964537132,3.12480226517166,-4.34223231246161));
#76386=CARTESIAN_POINT('Ctrl Pts',(10.3992305095491,5.34243639065652,0.278826224728918));
#76387=CARTESIAN_POINT('Ctrl Pts',(10.5184964819663,2.65580708494681,4.64392715052188));
#76388=CARTESIAN_POINT('Ctrl Pts',(10.6377624543835,-2.46880680580944,4.74598394512631));
#76389=CARTESIAN_POINT('Ctrl Pts',(10.7570284268006,-5.32709910636557,0.491310251029656));
#76390=CARTESIAN_POINT('Ctrl Pts',(10.8762943992178,-3.29520733521441,-4.21437768475455));
#76391=CARTESIAN_POINT('Ctrl Pts',(10.995560371635,1.76162729918915,-5.05134040731361));
#76392=CARTESIAN_POINT('Ctrl Pts',(11.1148263440521,5.20131879681764,-1.2512607344911));
#76393=CARTESIAN_POINT('Ctrl Pts',(11.2340923164693,3.86629035321667,3.69745446982539));
#76394=CARTESIAN_POINT('Ctrl Pts',(11.3533582888864,-1.01792520411819,5.25197095675792));
#76395=CARTESIAN_POINT('Ctrl Pts',(11.4726242613037,-4.96770317732397,1.98526970304111));
#76396=CARTESIAN_POINT('Ctrl Pts',(11.5918902337208,-4.35721627359315,-3.10387451372362));
#76397=CARTESIAN_POINT('Ctrl Pts',(11.711156206138,0.25311917672245,-5.34371606040058));
#76398=CARTESIAN_POINT('Ctrl Pts',(11.8304221785551,4.63109563736341,-2.67811946137613));
#76399=CARTESIAN_POINT('Ctrl Pts',(11.9496881509723,4.7578070721057,2.44594409511522));
#76400=CARTESIAN_POINT('Ctrl Pts',(12.0689541233894,0.51693459378251,5.32467363108372));
#76401=CARTESIAN_POINT('Ctrl Pts',(12.1882200958066,-4.19847482597077,3.31544563935193));
#76402=CARTESIAN_POINT('Ctrl Pts',(12.3074860682238,-5.05975757950666,-1.73730362586189));
#76403=CARTESIAN_POINT('Ctrl Pts',(12.4267520406409,-1.27627112038846,-5.19523846219496));
#76404=CARTESIAN_POINT('Ctrl Pts',(12.5460180130581,3.67880996828069,-3.88403499843739));
#76405=CARTESIAN_POINT('Ctrl Pts',(12.6652839854753,5.25680766681221,0.992644853889018));
#76406=CARTESIAN_POINT('Ctrl Pts',(12.7845499578925,2.00914760921968,4.95809404269169));
#76407=CARTESIAN_POINT('Ctrl Pts',(12.9038159303096,-3.08287491284709,4.37209937256074));
#76408=CARTESIAN_POINT('Ctrl Pts',(13.0230819027268,-5.34487203218452,-0.227406269436635));
#76409=CARTESIAN_POINT('Ctrl Pts',(13.1423478751439,-2.70036984388385,-4.61815692219858));
#76410=CARTESIAN_POINT('Ctrl Pts',(13.2616138475611,2.42302476496527,-4.76952006392394));
#76411=CARTESIAN_POINT('Ctrl Pts',(13.3808798199783,5.32212489864176,-0.542546970376561));
#76412=CARTESIAN_POINT('Ctrl Pts',(13.5001457923954,3.33560719654819,4.18247477961839));
#76413=CARTESIAN_POINT('Ctrl Pts',(13.6194117648126,-1.71293973690343,5.06805762689664));
#76414=CARTESIAN_POINT('Ctrl Pts',(13.7386777372298,-5.18903786661671,1.30125196277481));
#76415=CARTESIAN_POINT('Ctrl Pts',(13.8579437096469,-3.90168973483795,-3.66008030852715));
#76416=CARTESIAN_POINT('Ctrl Pts',(13.9772096820641,0.96734152561576,-5.26152269068825));
#76417=CARTESIAN_POINT('Ctrl Pts',(14.0964756544813,4.94837013659463,-2.03297900704013));
#76418=CARTESIAN_POINT('Ctrl Pts',(14.2157416268984,4.38688126484615,3.06180394864691));
#76419=CARTESIAN_POINT('Ctrl Pts',(14.3350075993156,-0.201688098081399,
5.3459042792497));
#76420=CARTESIAN_POINT('Ctrl Pts',(14.4542735717327,-4.60511130453659,2.72255771741147));
#76421=CARTESIAN_POINT('Ctrl Pts',(14.5735395441499,-4.78112264944524,-2.40004934590306));
#76422=CARTESIAN_POINT('Ctrl Pts',(14.6928055165671,-0.568146787928893,
-5.31945296803855));
#76423=CARTESIAN_POINT('Ctrl Pts',(14.8120714889842,4.16637791607122,-3.35569154009744));
#76424=CARTESIAN_POINT('Ctrl Pts',(14.9313374614014,5.07624035735161,1.68853619629629));
#76425=CARTESIAN_POINT('Ctrl Pts',(15.0506034338186,1.32620268338616,5.18271715361618));
#76426=CARTESIAN_POINT('Ctrl Pts',(15.1698694062357,-3.64126592412445,3.91925415374118));
#76427=CARTESIAN_POINT('Ctrl Pts',(15.2891353786529,-5.26611591924131,-0.942015805027344));
#76428=CARTESIAN_POINT('Ctrl Pts',(15.4084013510701,-2.05676334484598,-4.93853168412494));
#76429=CARTESIAN_POINT('Ctrl Pts',(15.5276673234872,3.0406621088803,-4.40156160827348));
#76430=CARTESIAN_POINT('Ctrl Pts',(15.6469332959044,5.34681277770121,0.175965257988861));
#76431=CARTESIAN_POINT('Ctrl Pts',(15.7661992683216,2.74468256834738,4.5919590863615));
#76432=CARTESIAN_POINT('Ctrl Pts',(15.8854652407387,-2.3770183697707,4.79261456008932));
#76433=CARTESIAN_POINT('Ctrl Pts',(16.0047312131559,-5.31665790112462,0.593733453847086));
#76434=CARTESIAN_POINT('Ctrl Pts',(16.123997185573,-3.37569820508123,-4.15018460794448));
#76435=CARTESIAN_POINT('Ctrl Pts',(16.2432631579902,1.66409356894118,-5.08430558145515));
#76436=CARTESIAN_POINT('Ctrl Pts',(16.3625291304074,5.17627646950703,-1.35112270465559));
#76437=CARTESIAN_POINT('Ctrl Pts',(16.4817951028246,3.93672784856066,3.62236725059386));
#76438=CARTESIAN_POINT('Ctrl Pts',(16.6010610752417,-0.916668278371397,
5.27058724614582));
#76439=CARTESIAN_POINT('Ctrl Pts',(16.7203270476589,-4.92857891302596,2.08050007207014));
#76440=CARTESIAN_POINT('Ctrl Pts',(16.839593020076,-4.41614006301782,-3.01944988294506));
#76441=CARTESIAN_POINT('Ctrl Pts',(16.9588589924932,0.150238344599186,-5.34759750650883));
#76442=CARTESIAN_POINT('Ctrl Pts',(17.0781249649104,4.57870057212474,-2.76674388453876));
#76443=CARTESIAN_POINT('Ctrl Pts',(17.1973909373275,4.80399552983808,2.35393236969624));
#76444=CARTESIAN_POINT('Ctrl Pts',(17.3166569097447,0.619306375843183,5.31373976260104));
#76445=CARTESIAN_POINT('Ctrl Pts',(17.4359228821619,-4.13389523008567,3.39562672837916));
#76446=CARTESIAN_POINT('Ctrl Pts',(17.555188854579,-5.09225311251117,-1.63961242064348));
#76447=CARTESIAN_POINT('Ctrl Pts',(17.6744548269962,-1.37601144972682,-5.1697159633802));
#76448=CARTESIAN_POINT('Ctrl Pts',(17.7937207994134,3.60338472540743,-3.95411041480993));
#76449=CARTESIAN_POINT('Ctrl Pts',(17.9129867718305,5.27493656789836,0.891299532400152));
#76450=CARTESIAN_POINT('Ctrl Pts',(18.0322527442477,2.10418863924757,4.91851205368746));
#76451=CARTESIAN_POINT('Ctrl Pts',(18.1515187166648,-2.99816776186809,4.43061629161259));
#76452=CARTESIAN_POINT('Ctrl Pts',(18.270784689082,-5.34825844750761,-0.124507953446764));
#76453=CARTESIAN_POINT('Ctrl Pts',(18.3900506614992,-2.78874115530351,-4.5653360687384));
#76454=CARTESIAN_POINT('Ctrl Pts',(18.5093166339163,2.33079188008128,-4.81526529524129));
#76455=CARTESIAN_POINT('Ctrl Pts',(18.6285826063335,5.31069862001794,-0.644864961947463));
#76456=CARTESIAN_POINT('Ctrl Pts',(18.7478485787507,3.41547664867964,4.11751015956628));
#76457=CARTESIAN_POINT('Ctrl Pts',(18.8671145511678,-1.61509331810011,5.10008276654765));
#76458=CARTESIAN_POINT('Ctrl Pts',(18.986380523585,-5.16303578710043,1.40086834246771));
#76459=CARTESIAN_POINT('Ctrl Pts',(19.1056464960022,-3.971401450112,-3.58431878797852));
#76460=CARTESIAN_POINT('Ctrl Pts',(19.2249124684193,0.865910154356953,-5.27916378381931));
#76461=CARTESIAN_POINT('Ctrl Pts',(19.3441784408365,4.9083313391403,-2.12782849802824));
#76462=CARTESIAN_POINT('Ctrl Pts',(19.4634444132536,4.4449899589576,2.97681623829445));
#76463=CARTESIAN_POINT('Ctrl Pts',(19.5827103856708,-0.0987746801464204,
5.3487955853977));
#76464=CARTESIAN_POINT('Ctrl Pts',(19.701976358088,-4.55186588556823,2.81067387144225));
#76465=CARTESIAN_POINT('Ctrl Pts',(19.8212423305052,-4.82642359542294,-2.30759743658899));
#76466=CARTESIAN_POINT('Ctrl Pts',(19.9405083029223,-0.670408620522066,
-5.30753454377244));
#76467=CARTESIAN_POINT('Ctrl Pts',(20.0597742753395,4.10102977567299,-3.43524750649084));
#76468=CARTESIAN_POINT('Ctrl Pts',(20.1790402477567,5.10779436232139,1.59053682888681));
#76469=CARTESIAN_POINT('Ctrl Pts',(20.2983062201738,1.42569280748336,5.15623609530228));
#76470=CARTESIAN_POINT('Ctrl Pts',(20.417572192591,-3.56516987965126,3.98860055420888));
#76471=CARTESIAN_POINT('Ctrl Pts',(20.5368381650081,-5.28326879605584,-0.840500731962909));
#76472=CARTESIAN_POINT('Ctrl Pts',(20.6561041374253,-2.1514191011895,-4.89803700505059));
#76473=CARTESIAN_POINT('Ctrl Pts',(20.7753701098425,2.95539580647574,-4.45926073232701));
#76474=CARTESIAN_POINT('Ctrl Pts',(20.8946360822597,5.34920890774529,0.0730391203798664));
#76475=CARTESIAN_POINT('Ctrl Pts',(21.0139020546768,2.83254152524977,4.53829033442592));
#76476=CARTESIAN_POINT('Ctrl Pts',(21.133168027094,-2.28434957613141,4.83747017208749));
#76477=CARTESIAN_POINT('Ctrl Pts',(21.2524339995111,-5.30424760710754,0.69593676027454));
#76478=CARTESIAN_POINT('Ctrl Pts',(21.3716999719283,-3.45493884415087,-4.08445445989859));
#76479=CARTESIAN_POINT('Ctrl Pts',(21.4909659443455,1.56594352144461,-5.11538772132217));
#76480=CARTESIAN_POINT('Ctrl Pts',(21.6102319167626,5.14931704538713,-1.45048427012945));
#76481=CARTESIAN_POINT('Ctrl Pts',(21.7294978891798,4.00570732897041,3.54593844369029));
#76482=CARTESIAN_POINT('Ctrl Pts',(21.848763861597,-0.81507185340302,5.28725150958398));
#76483=CARTESIAN_POINT('Ctrl Pts',(21.9680298340141,-4.88762928971471,2.17495990264885));
#76484=CARTESIAN_POINT('Ctrl Pts',(22.0872958064313,-4.4734282813765,-2.93390696225849));
#76485=CARTESIAN_POINT('Ctrl Pts',(22.2065617788485,0.0473018698816033,
-5.34949840498282));
#76486=CARTESIAN_POINT('Ctrl Pts',(22.3258277512656,4.5246097295625,-2.85434361052691));
#76487=CARTESIAN_POINT('Ctrl Pts',(22.4450937236827,4.84840476952531,2.26104883685696));
#76488=CARTESIAN_POINT('Ctrl Pts',(22.5643596961,0.72144879027182,5.30083788611039));
#76489=CARTESIAN_POINT('Ctrl Pts',(22.6836256685171,-4.06778459593354,3.47455020583862));
#76490=CARTESIAN_POINT('Ctrl Pts',(22.8028916409343,-5.12286266777649,-1.54131396506679));
#76491=CARTESIAN_POINT('Ctrl Pts',(22.9221576133515,-1.47524215652576,-5.14227879751937));
#76492=CARTESIAN_POINT('Ctrl Pts',(23.0414235857686,3.52662492527076,-4.02272137840373));
#76493=CARTESIAN_POINT('Ctrl Pts',(23.1606895581858,5.29111183221057,0.789624107312617));
#76494=CARTESIAN_POINT('Ctrl Pts',(23.2799555306029,2.19845035747676,4.87710843405375));
#76495=CARTESIAN_POINT('Ctrl Pts',(23.3992215030201,-2.91235020307306,4.48749227815132));
#76496=CARTESIAN_POINT('Ctrl Pts',(23.5184874754372,-5.34966407040875,-0.0215635244252718));
#76497=CARTESIAN_POINT('Ctrl Pts',(23.6377534478544,-2.87607962259252,-4.51082438766087));
#76498=CARTESIAN_POINT('Ctrl Pts',(23.7570194202716,2.2376957581383,-4.85922713461897));
#76499=CARTESIAN_POINT('Ctrl Pts',(23.8762853926887,5.2973054597101,-0.746944119953741));
#76500=CARTESIAN_POINT('Ctrl Pts',(23.9955513651059,3.49408113758448,4.05102056965703));
#76501=CARTESIAN_POINT('Ctrl Pts',(24.1148173375231,-1.51664872988588,5.13021902865199));
#76502=CARTESIAN_POINT('Ctrl Pts',(24.2340833099402,-5.13512151462232,1.49996589356924));
#76503=CARTESIAN_POINT('Ctrl Pts',(24.3533492823574,-4.03964230866261,-3.50722977146794));
#76504=CARTESIAN_POINT('Ctrl Pts',(24.4726152547746,0.764158082763927,-5.29484967457566));
#76505=CARTESIAN_POINT('Ctrl Pts',(24.5918812271917,4.86647468160752,-2.22188992190905));
#76506=CARTESIAN_POINT('Ctrl Pts',(24.7111471996089,4.50145239709396,2.89072602792189));
#76507=CARTESIAN_POINT('Ctrl Pts',(24.8304131720261,0.00417532019002488,
5.34970590018823));
#76508=CARTESIAN_POINT('Ctrl Pts',(24.9496791444432,-4.49693462782816,2.89774905829474));
#76509=CARTESIAN_POINT('Ctrl Pts',(25.0689451168604,-4.86993701684925,-2.21429088055959));
#76510=CARTESIAN_POINT('Ctrl Pts',(25.1882110892776,-0.772422159146575,
-5.29365040967637));
#76511=CARTESIAN_POINT('Ctrl Pts',(25.3074770616947,4.03416276912766,-3.51353118728043));
#76512=CARTESIAN_POINT('Ctrl Pts',(25.4267430341119,5.13745663366157,1.49194838686019));
#76513=CARTESIAN_POINT('Ctrl Pts',(25.546009006529,1.52465490894722,5.12784536237498));
#76514=CARTESIAN_POINT('Ctrl Pts',(25.6652749789462,-3.48775343124658,4.05646972805612));
#76515=CARTESIAN_POINT('Ctrl Pts',(25.7845409513634,-5.2984649501547,-0.738674369252185));
#76516=CARTESIAN_POINT('Ctrl Pts',(25.9038069237805,-2.24527805335948,-4.85572827852936));
#76517=CARTESIAN_POINT('Ctrl Pts',(26.0230728961977,2.86903493736783,-4.51530831505123));
#76518=CARTESIAN_POINT('Ctrl Pts',(26.1423388686148,5.34962389335311,-0.0299140681537413));
#76519=CARTESIAN_POINT('Ctrl Pts',(26.2616048410321,2.91935141602282,4.48294077158877));
#76520=CARTESIAN_POINT('Ctrl Pts',(26.3808708134492,-2.19083474590394,4.88053416830044));
#76521=CARTESIAN_POINT('Ctrl Pts',(26.5001367858664,-5.28987282061753,0.797882318077011));
#76522=CARTESIAN_POINT('Ctrl Pts',(26.6194027582835,-3.53289990469077,-4.01721158457497));
#76523=CARTESIAN_POINT('Ctrl Pts',(26.7386687307007,1.4672135077607,-5.14457531526681));
#76524=CARTESIAN_POINT('Ctrl Pts',(26.8579347031179,5.12045050920806,-1.54930863115098));
#76525=CARTESIAN_POINT('Ctrl Pts',(26.977200675535,4.073203247058,3.46819635545099));
#76526=CARTESIAN_POINT('Ctrl Pts',(27.0964666479522,-0.713173556682066,
5.30195757526005));
#76527=CARTESIAN_POINT('Ctrl Pts',(27.2157326203693,-4.8448694735804,2.2686142104326));
#76528=CARTESIAN_POINT('Ctrl Pts',(27.3349985927865,-4.5290597112821,-2.8472774335229));
#76529=CARTESIAN_POINT('Ctrl Pts',(27.4542645652037,-0.0556521236575815,
-5.34941805180156));
#76530=CARTESIAN_POINT('Ctrl Pts',(27.5735305376208,4.46884314287686,-2.94088619571898));
#76531=CARTESIAN_POINT('Ctrl Pts',(27.692796510038,4.89101834366639,2.16732789714115));
#76532=CARTESIAN_POINT('Ctrl Pts',(27.8120624824552,0.823324007385604,5.2859727799782));
#76533=CARTESIAN_POINT('Ctrl Pts',(27.9313284548724,-4.00016740839022,3.55218684146269));
#76534=CARTESIAN_POINT('Ctrl Pts',(28.0505944272895,-5.15157490868226,-1.44244466515798));
#76535=CARTESIAN_POINT('Ctrl Pts',(28.1698603997067,-1.57392648948877,-5.11293712629961));
#76536=CARTESIAN_POINT('Ctrl Pts',(28.2891263721238,3.44855899679427,-4.08984247831593));
#76537=CARTESIAN_POINT('Ctrl Pts',(28.408392344541,5.30532746904341,0.687656235354114));
#76538=CARTESIAN_POINT('Ctrl Pts',(28.5276583169582,2.291897852936,4.83389851812331));
#76539=CARTESIAN_POINT('Ctrl Pts',(28.6469242893753,-2.82545402003632,4.54270626746531));
#76540=CARTESIAN_POINT('Ctrl Pts',(28.7661902617925,-5.34908838029851,0.0813888909092254));
#76541=CARTESIAN_POINT('Ctrl Pts',(28.8854562342096,-2.96235289888958,-4.45464206802835));
#76542=CARTESIAN_POINT('Ctrl Pts',(29.0047222066268,2.14377087841479,-4.90138930025648));
#76543=CARTESIAN_POINT('Ctrl Pts',(29.123988179044,5.28195037803777,-0.848746638140402));
#76544=CARTESIAN_POINT('Ctrl Pts',(29.2432541514612,3.57139155113628,3.98303063511691));
#76545=CARTESIAN_POINT('Ctrl Pts',(29.3625201238783,-1.41764243240855,5.15845525187946));
#76546=CARTESIAN_POINT('Ctrl Pts',(29.4817860962955,-5.10530538757201,1.5985079140987));
#76547=CARTESIAN_POINT('Ctrl Pts',(29.6010520687126,-4.10638703665957,-3.42884180984799));
#76548=CARTESIAN_POINT('Ctrl Pts',(29.7203180411298,0.662122995951101,-5.30857455349746));
#76549=CARTESIAN_POINT('Ctrl Pts',(29.839584013547,4.8228156661174,-2.31512844189271));
#76550=CARTESIAN_POINT('Ctrl Pts',(29.9588499859641,4.55624766770592,2.8035652020832));
#76551=CARTESIAN_POINT('Ctrl Pts',(30.0781159583813,0.107123774146093,5.34863488647531));
#76552=CARTESIAN_POINT('Ctrl Pts',(30.1973819307985,-4.44033787577436,2.98375102861677));
#76553=CARTESIAN_POINT('Ctrl Pts',(30.3166479032156,-4.91164679800034,-2.12016423503002));
#76554=CARTESIAN_POINT('Ctrl Pts',(30.4359138756328,-0.874149621850558,
-5.27780570790802));
#76555=CARTESIAN_POINT('Ctrl Pts',(30.55517984805,3.96580166144261,-3.59051358915504));
#76556=CARTESIAN_POINT('Ctrl Pts',(30.6744458204671,5.16521618558982,1.39280738364225));
#76557=CARTESIAN_POINT('Ctrl Pts',(30.7937117928843,1.62305233596266,5.09755546968683));
#76558=CARTESIAN_POINT('Ctrl Pts',(30.9129777653015,-3.40904525103163,4.12283653911075));
#76559=CARTESIAN_POINT('Ctrl Pts',(31.0322437377186,-5.31169875345763,-0.636574429524205));
#76560=CARTESIAN_POINT('Ctrl Pts',(31.1515097101358,-2.33830543955411,-4.81162117411165));
#76561=CARTESIAN_POINT('Ctrl Pts',(31.270775682553,2.78161148635255,-4.56968359854373));
#76562=CARTESIAN_POINT('Ctrl Pts',(31.3900416549701,5.34805758082949,-0.132856177649306));
#76563=CARTESIAN_POINT('Ctrl Pts',(31.5093076273873,3.00508008957021,4.42593089723243));
#76564=CARTESIAN_POINT('Ctrl Pts',(31.6285735998045,-2.09650851344057,4.92179059945456));
#76565=CARTESIAN_POINT('Ctrl Pts',(31.7478395722216,-5.27353886553098,0.8995323704801));
#76566=CARTESIAN_POINT('Ctrl Pts',(31.8671055446388,-3.60955251287627,-3.94848088618859));
#76567=CARTESIAN_POINT('Ctrl Pts',(31.986371517056,1.36794009374822,-5.17185755330946));
#76568=CARTESIAN_POINT('Ctrl Pts',(32.1056374894731,5.08968755204155,-1.64755918691883));
#76569=CARTESIAN_POINT('Ctrl Pts',(32.2249034618903,4.13919060489128,3.3891697786018));
#76570=CARTESIAN_POINT('Ctrl Pts',(32.3441694343074,-0.611011127479355,
5.31469999660417));
#76571=CARTESIAN_POINT('Ctrl Pts',(32.4634354067246,-4.80031530123962,2.36142830941194));
#76572=CARTESIAN_POINT('Ctrl Pts',(32.5827013791417,-4.58301374895963,-2.75959338103551));
#76573=CARTESIAN_POINT('Ctrl Pts',(32.701967351559,-0.15858550575743,-5.34735647672489));
#76574=CARTESIAN_POINT('Ctrl Pts',(32.821233323976,4.41142146589973,-3.02633958801825));
#76575=CARTESIAN_POINT('Ctrl Pts',(32.9404992963933,4.93182046980722,2.07280426123612));
#76576=CARTESIAN_POINT('Ctrl Pts',(33.0597652688104,0.924894296461516,5.26914994967698));
#76577=CARTESIAN_POINT('Ctrl Pts',(33.1790312412276,-3.93106871030145,3.6285078815811));
#76578=CARTESIAN_POINT('Ctrl Pts',(33.2982972136447,-5.17837920130185,-1.34304113836196));
#76579=CARTESIAN_POINT('Ctrl Pts',(33.417563186062,-1.67202789967526,-5.08170181676528));
#76580=CARTESIAN_POINT('Ctrl Pts',(33.536829158479,3.36921585264198,-4.15544885543223));
#76581=CARTESIAN_POINT('Ctrl Pts',(33.6560951308963,5.31757821346333,0.585433681563546));
#76582=CARTESIAN_POINT('Ctrl Pts',(33.7753611033134,2.38449651621095,4.78889830921323));
#76583=CARTESIAN_POINT('Ctrl Pts',(33.8946270757306,-2.73751139581363,4.59623781038317));
#76584=CARTESIAN_POINT('Ctrl Pts',(34.0138930481477,-5.34653159039126,0.184311162880282));
#76585=CARTESIAN_POINT('Ctrl Pts',(34.1331590205649,-3.04752903183865,-4.39680991764522));
#76586=CARTESIAN_POINT('Ctrl Pts',(34.252424992982,2.04905202712797,-4.94173617688352));
#76587=CARTESIAN_POINT('Ctrl Pts',(34.3716909653993,5.26463906194561,-0.95023481270979));
#76588=CARTESIAN_POINT('Ctrl Pts',(34.4909569378164,3.64737925647783,3.91356553684459));
#76589=CARTESIAN_POINT('Ctrl Pts',(34.6102229102336,-1.31811109383836,5.18478097860004));
#76590=CARTESIAN_POINT('Ctrl Pts',(34.7294888826507,-5.0735984487402,1.69645790782622));
#76591=CARTESIAN_POINT('Ctrl Pts',(34.8487548550679,-4.17161091433314,-3.34918393505835));
#76592=CARTESIAN_POINT('Ctrl Pts',(34.968020827485,0.559842683756944,-5.32033333739675));
#76593=CARTESIAN_POINT('Ctrl Pts',(35.0872867999022,4.7773704624956,-2.40750952598498));
#76594=CARTESIAN_POINT('Ctrl Pts',(35.2065527723194,4.60935547635934,2.71536604189249));
#76595=CARTESIAN_POINT('Ctrl Pts',(35.3258187447365,0.210032554159402,5.34558294083782));
#76596=CARTESIAN_POINT('Ctrl Pts',(35.4450847171537,-4.38209659193005,3.06864793069408));
#76597=CARTESIAN_POINT('Ctrl Pts',(35.5643506895709,-4.951537488818,-2.02525236124853));
#76598=CARTESIAN_POINT('Ctrl Pts',(35.6836166619881,-0.975553337067666,
-5.26000630617043));
#76599=CARTESIAN_POINT('Ctrl Pts',(35.8028826344052,3.89597177940602,-3.66616620183877));
#76600=CARTESIAN_POINT('Ctrl Pts',(35.9221486068224,5.19106272102259,1.29315053937908));
#76601=CARTESIAN_POINT('Ctrl Pts',(36.0414145792395,1.72084867623149,5.06537763153141));
#76602=CARTESIAN_POINT('Ctrl Pts',(36.1606805516567,-3.32907454724463,4.18767641509399));
#76603=CARTESIAN_POINT('Ctrl Pts',(36.2799465240739,-5.322965195057,-0.53423874092893));
#76604=CARTESIAN_POINT('Ctrl Pts',(36.399212496491,-2.4304670141352,-4.76573200043202));
#76605=CARTESIAN_POINT('Ctrl Pts',(36.5184784689082,2.69315822717824,-4.62236649547752));
#76606=CARTESIAN_POINT('Ctrl Pts',(36.6377444413254,5.34450979925368,-0.235748984964162));
#76607=CARTESIAN_POINT('Ctrl Pts',(36.7570104137425,3.08969722168957,4.36728164088206));
#76608=CARTESIAN_POINT('Ctrl Pts',(36.8762763861597,-2.00140852293053,4.96122453667856));
#76609=CARTESIAN_POINT('Ctrl Pts',(36.9955423585768,-5.25524664538787,1.00084860358074));
#76610=CARTESIAN_POINT('Ctrl Pts',(37.114808330994,-3.68487805339145,-3.87828655393761));
#76611=CARTESIAN_POINT('Ctrl Pts',(37.2340743034112,1.26817861053563,-5.1972267358067));
#76612=CARTESIAN_POINT('Ctrl Pts',(37.3533402758283,5.05700430786462,-1.745194981863));
#76613=CARTESIAN_POINT('Ctrl Pts',(37.4726062482455,4.20371193315622,3.30887930675979));
#76614=CARTESIAN_POINT('Ctrl Pts',(37.5918722206627,-0.508749602332581,
5.32549053072501));
#76615=CARTESIAN_POINT('Ctrl Pts',(37.7111381930799,-4.75374167366011,2.45333653102065));
#76616=CARTESIAN_POINT('Ctrl Pts',(37.830404165497,-4.63572933387,-2.67082784760058));
#76617=CARTESIAN_POINT('Ctrl Pts',(37.9496701379142,-0.260588162173769,
-5.34342727819689));
#76618=CARTESIAN_POINT('Ctrl Pts',(38.0689361103313,4.35070685430609,-3.11045822607375));
#76619=CARTESIAN_POINT('Ctrl Pts',(38.1882020827485,4.97397191480465,1.9771100447851));
#76620=CARTESIAN_POINT('Ctrl Pts',(38.3074680551657,1.01988032406546,5.25111166397229));
#76621=CARTESIAN_POINT('Ctrl Pts',(38.4068563655133,-3.03575591970712,3.96049046164289));
#76622=CARTESIAN_POINT('Ctrl Pts',(38.4863670137914,-4.54515679744195,1.22768957972598));
#76623=CARTESIAN_POINT('Ctrl Pts',(38.5261223379305,-4.57497191465336,-0.318504194825992));
#76624=CARTESIAN_POINT('Ctrl Pts',(38.546,-4.39991769847472,-1.05120802372743));
#76625=CARTESIAN_POINT('Ctrl Pts',(-17.7840033022126,-1.9938567537982,4.21983174306485));
#76626=CARTESIAN_POINT('Ctrl Pts',(-17.764125640143,-2.69657146060628,3.88780133297438));
#76627=CARTESIAN_POINT('Ctrl Pts',(-17.724370316004,-3.92180026446256,2.86581084683925));
#76628=CARTESIAN_POINT('Ctrl Pts',(-17.6448596677259,-5.14708318505065,
-0.112939977084765));
#76629=CARTESIAN_POINT('Ctrl Pts',(-17.5454713573783,-3.56813811963232,
-4.21020221567445));
#76630=CARTESIAN_POINT('Ctrl Pts',(-17.426205384961,1.6191574350232,-5.27949136677745));
#76631=CARTESIAN_POINT('Ctrl Pts',(-17.3069394125439,5.3116616510009,-1.49406917373198));
#76632=CARTESIAN_POINT('Ctrl Pts',(-17.1876734401267,4.13252590194496,3.65866187852482));
#76633=CARTESIAN_POINT('Ctrl Pts',(-17.0684074677096,-0.842490899558503,
5.45501402271219));
#76634=CARTESIAN_POINT('Ctrl Pts',(-16.9491414952924,-5.04290871094292,
2.24259701600285));
#76635=CARTESIAN_POINT('Ctrl Pts',(-16.8298755228753,-4.61465967021616,
-3.02787363897754));
#76636=CARTESIAN_POINT('Ctrl Pts',(-16.7106095504581,0.0501009852498292,
-5.5191309278913));
#76637=CARTESIAN_POINT('Ctrl Pts',(-16.5913435780409,4.66869368758116,-2.94375284374969));
#76638=CARTESIAN_POINT('Ctrl Pts',(-16.4720776056238,5.00159973752036,2.33384980148805));
#76639=CARTESIAN_POINT('Ctrl Pts',(-16.3528116332066,0.743075638461223,
5.46906600082232));
#76640=CARTESIAN_POINT('Ctrl Pts',(-16.2335456607894,-4.19755323287798,
3.58375026676195));
#76641=CARTESIAN_POINT('Ctrl Pts',(-16.1142796883723,-5.28491497754428,
-1.59137268981239));
#76642=CARTESIAN_POINT('Ctrl Pts',(-15.9950137159551,-1.52080981986866,
-5.30565012642365));
#76643=CARTESIAN_POINT('Ctrl Pts',(-15.8757477435379,3.63936847718576,-4.14942967182103));
#76644=CARTESIAN_POINT('Ctrl Pts',(-15.7564817711208,5.45867196013972,0.815892952732853));
#76645=CARTESIAN_POINT('Ctrl Pts',(-15.6372157987036,2.26700874645107,5.03224107677712));
#76646=CARTESIAN_POINT('Ctrl Pts',(-15.5179498262864,-3.00572841093485,
4.62907913105125));
#76647=CARTESIAN_POINT('Ctrl Pts',(-15.3986838538693,-5.5192595971191,-0.0234964456327061));
#76648=CARTESIAN_POINT('Ctrl Pts',(-15.2794178814521,-2.96620658071756,
-4.65450284102427));
#76649=CARTESIAN_POINT('Ctrl Pts',(-15.160151909035,2.30977226438264,-5.01275672892111));
#76650=CARTESIAN_POINT('Ctrl Pts',(-15.0408859366178,5.46542049672021,-0.769387405749975));
#76651=CARTESIAN_POINT('Ctrl Pts',(-14.9216199642006,3.60390801126691,4.18026615861146));
#76652=CARTESIAN_POINT('Ctrl Pts',(-14.8023539917834,-1.56592916246069,
5.29250828460176));
#76653=CARTESIAN_POINT('Ctrl Pts',(-14.6830880193663,-5.29827068197203,
1.54632011588519));
#76654=CARTESIAN_POINT('Ctrl Pts',(-14.5638220469491,-4.16689211735099,
-3.61936295353509));
#76655=CARTESIAN_POINT('Ctrl Pts',(-14.444556074532,0.789620736094701,-5.46253395392374));
#76656=CARTESIAN_POINT('Ctrl Pts',(-14.3252901021148,5.02127552618045,-2.29119405547708));
#76657=CARTESIAN_POINT('Ctrl Pts',(-14.2060241296976,4.64348695694276,2.98342202649576));
#76658=CARTESIAN_POINT('Ctrl Pts',(-14.0867581572805,0.00305834679333195,
5.51930872065043));
#76659=CARTESIAN_POINT('Ctrl Pts',(-13.9674921848633,-4.64017777250366,
2.98856626956584));
#76660=CARTESIAN_POINT('Ctrl Pts',(-13.8482262124461,-5.02381162417254,
-2.28562789458371));
#76661=CARTESIAN_POINT('Ctrl Pts',(-13.728960240029,-0.795674023300409,
-5.46165551424887));
#76662=CARTESIAN_POINT('Ctrl Pts',(-13.6096942676118,4.16287845392856,-3.62397862653602));
#76663=CARTESIAN_POINT('Ctrl Pts',(-13.4904282951946,5.29998111364186,1.54044743589541));
#76664=CARTESIAN_POINT('Ctrl Pts',(-13.3711623227775,1.57179354601877,5.29076961853536));
#76665=CARTESIAN_POINT('Ctrl Pts',(-13.2518963503603,-3.59927308379099,
4.18425756568985));
#76666=CARTESIAN_POINT('Ctrl Pts',(-13.1326303779432,-5.46626979625021,
-0.763329956394489));
#76667=CARTESIAN_POINT('Ctrl Pts',(-13.013364405526,-2.31532617091257,-5.01019389145924));
#76668=CARTESIAN_POINT('Ctrl Pts',(-12.8940984331088,2.96104649858842,-4.65778721507616));
#76669=CARTESIAN_POINT('Ctrl Pts',(-12.7748324606917,5.51923012488573,-0.0296131099717272));
#76670=CARTESIAN_POINT('Ctrl Pts',(-12.6555664882745,3.01085675535932,4.6257453136155));
#76671=CARTESIAN_POINT('Ctrl Pts',(-12.5363005158573,-2.26143060436429,
5.03475021519175));
#76672=CARTESIAN_POINT('Ctrl Pts',(-12.4170345434402,-5.45776411004393,
0.821942228410921));
#76673=CARTESIAN_POINT('Ctrl Pts',(-12.297768571023,-3.64396534951881,-4.14539438886518));
#76674=CARTESIAN_POINT('Ctrl Pts',(-12.1785025986058,1.51493004883248,-5.30733125543085));
#76675=CARTESIAN_POINT('Ctrl Pts',(-12.0592366261887,5.28314608368199,-1.59723059268359));
#76676=CARTESIAN_POINT('Ctrl Pts',(-11.9399706537715,4.20152615507953,3.57909989744786));
#76677=CARTESIAN_POINT('Ctrl Pts',(-11.8207046813543,-0.737021506645064,
5.46987910346027));
#76678=CARTESIAN_POINT('Ctrl Pts',(-11.7014387089372,-4.99899627938499,
2.33940469060478));
#76679=CARTESIAN_POINT('Ctrl Pts',(-11.58217273652,-4.67197965326751,-2.93860242754666));
#76680=CARTESIAN_POINT('Ctrl Pts',(-11.4629067641029,-0.056167187694204,
-5.51902376827236));
#76681=CARTESIAN_POINT('Ctrl Pts',(-11.3436407916857,4.61120577659153,-3.03307754494631));
#76682=CARTESIAN_POINT('Ctrl Pts',(-11.2243748192685,5.04557226027564,2.23718096587329));
#76683=CARTESIAN_POINT('Ctrl Pts',(-11.1051088468514,0.848191406958907,
5.45374636785483));
#76684=CARTESIAN_POINT('Ctrl Pts',(-10.9858428744342,-4.1278143649581,3.66386772088927));
#76685=CARTESIAN_POINT('Ctrl Pts',(-10.866576902017,-5.31455854150475,-1.48937759371077));
#76686=CARTESIAN_POINT('Ctrl Pts',(-10.7473109295999,-1.62263066617103,
-5.27540025295996));
#76687=CARTESIAN_POINT('Ctrl Pts',(-10.6280449571827,3.55884386101522,-4.2186974862679));
#76688=CARTESIAN_POINT('Ctrl Pts',(-10.5087789847655,5.47336179224965,0.71069599609851));
#76689=CARTESIAN_POINT('Ctrl Pts',(-10.3895130123484,2.36342905704779,4.98768294902862));
#76690=CARTESIAN_POINT('Ctrl Pts',(-10.2702470399312,-2.91609033284473,
4.68606394305692));
#76691=CARTESIAN_POINT('Ctrl Pts',(-10.150981067514,-5.5186896556229,0.0827199652415343));
#76692=CARTESIAN_POINT('Ctrl Pts',(-10.0317150950969,-3.05522812393436,
-4.59655949797773));
#76693=CARTESIAN_POINT('Ctrl Pts',(-9.91244912267972,2.21287954043883,-5.05627750892255));
#76694=CARTESIAN_POINT('Ctrl Pts',(-9.79318315026254,5.44960238069073,-0.874420951314895));
#76695=CARTESIAN_POINT('Ctrl Pts',(-9.67391717784538,3.68368527993848,4.11013878915217));
#76696=CARTESIAN_POINT('Ctrl Pts',(-9.55465120542822,-1.46379066202483,
5.32166280456567));
#76697=CARTESIAN_POINT('Ctrl Pts',(-9.43538523301106,-5.26753230567291,
1.64799317851164));
#76698=CARTESIAN_POINT('Ctrl Pts',(-9.31611926059388,-4.23577116176733,
-3.53850544338552));
#76699=CARTESIAN_POINT('Ctrl Pts',(-9.19685328817674,0.684354034145503,
-5.47671778200023));
#76700=CARTESIAN_POINT('Ctrl Pts',(-9.07758731575955,4.97625416227462,-2.38739871411816));
#76701=CARTESIAN_POINT('Ctrl Pts',(-8.95832134334239,4.70003975841694,2.89351073559937));
#76702=CARTESIAN_POINT('Ctrl Pts',(-8.83905537092524,0.109270827962002,
5.51822779467152));
#76703=CARTESIAN_POINT('Ctrl Pts',(-8.71978939850806,-4.58180681681053,
3.07730797957519));
#76704=CARTESIAN_POINT('Ctrl Pts',(-8.60052342609089,-5.06686571332418,
-2.18852689059757));
#76705=CARTESIAN_POINT('Ctrl Pts',(-8.48125745367375,-0.900630254309538,
-5.44533224447794));
#76706=CARTESIAN_POINT('Ctrl Pts',(-8.36199148125656,4.09236807060697,-3.7034175679236));
#76707=CARTESIAN_POINT('Ctrl Pts',(-8.24272550883941,5.32864388016197,1.43816984606865));
#76708=CARTESIAN_POINT('Ctrl Pts',(-8.12345953642224,1.67331754260636,5.25954242395045));
#76709=CARTESIAN_POINT('Ctrl Pts',(-8.00419356400508,-3.5180851153586,4.25274678635124));
#76710=CARTESIAN_POINT('Ctrl Pts',(-7.88492759158791,-5.47994699502656,
-0.657996230557716));
#76711=CARTESIAN_POINT('Ctrl Pts',(-7.76566161917075,-2.41131310695906,
-4.96471018368004));
#76712=CARTESIAN_POINT('Ctrl Pts',(-7.64639564675358,2.8708641584899,-4.71390677583113));
#76713=CARTESIAN_POINT('Ctrl Pts',(-7.52712967433642,5.5176381961095,-0.135819161248244));
#76714=CARTESIAN_POINT('Ctrl Pts',(-7.40786370191926,3.09931660075761,4.56694807458954));
#76715=CARTESIAN_POINT('Ctrl Pts',(-7.28859772950209,-2.1641235800721,5.07733662838151));
#76716=CARTESIAN_POINT('Ctrl Pts',(-7.16933175708492,-5.44093605806279,
0.926818709241918));
#76717=CARTESIAN_POINT('Ctrl Pts',(-7.05006578466777,-3.72306412807567,
-4.07450262068451));
#76718=CARTESIAN_POINT('Ctrl Pts',(-6.93079981225059,1.41251573892071,-5.33550160669358));
#76719=CARTESIAN_POINT('Ctrl Pts',(-6.81153383983344,5.25143079274477,-1.69860317223912));
#76720=CARTESIAN_POINT('Ctrl Pts',(-6.69226786741626,4.26962396706275,3.49758334963045));
#76721=CARTESIAN_POINT('Ctrl Pts',(-6.57300189499911,-0.631623195473639,
5.4830493565778));
#76722=CARTESIAN_POINT('Ctrl Pts',(-6.45373592258193,-4.95305128046833,
2.43517168199283));
#76723=CARTESIAN_POINT('Ctrl Pts',(-6.33446995016478,-4.72766467430163,
-2.8481511257462));
#76724=CARTESIAN_POINT('Ctrl Pts',(-6.2152039777476,-0.162364350551328,
-5.51692087358507));
#76725=CARTESIAN_POINT('Ctrl Pts',(-6.09593800533044,4.55198361526935,-3.12125347801937));
#76726=CARTESIAN_POINT('Ctrl Pts',(-5.97667203291329,5.0876900117107,2.13967017375761));
#76727=CARTESIAN_POINT('Ctrl Pts',(-5.85740606049611,0.952985709893719,
5.43641392320959));
#76728=CARTESIAN_POINT('Ctrl Pts',(-5.73814008807895,-4.05654285293957,
3.74262450561013));
#76729=CARTESIAN_POINT('Ctrl Pts',(-5.61887411566179,-5.34223582541585,
-1.38682893443001));
#76730=CARTESIAN_POINT('Ctrl Pts',(-5.49960814324461,-1.72384948209047,
-5.24319759982638));
#76731=CARTESIAN_POINT('Ctrl Pts',(-5.38034217082747,3.47700062078207,-4.28640231322372));
#76732=CARTESIAN_POINT('Ctrl Pts',(-5.26107619841028,5.48602479483962,0.605235539384232));
#76733=CARTESIAN_POINT('Ctrl Pts',(-5.14181022599314,2.45897388693394,4.94127772252337));
#76734=CARTESIAN_POINT('Ctrl Pts',(-5.02254425357596,-2.82537216313636,
4.74131313535636));
#76735=CARTESIAN_POINT('Ctrl Pts',(-4.9032782811588,-5.51607584370304,0.188905781395227));
#76736=CARTESIAN_POINT('Ctrl Pts',(-4.78401230874163,-3.14311810355895,
-4.53691378525191));
#76737=CARTESIAN_POINT('Ctrl Pts',(-4.66474633632447,2.11516723770901,-5.09792562364841));
#76738=CARTESIAN_POINT('Ctrl Pts',(-4.54548036390731,5.43176594459808,-0.979130650543266));
#76739=CARTESIAN_POINT('Ctrl Pts',(-4.42621439149014,3.76209824773743,4.0384891831104));
#76740=CARTESIAN_POINT('Ctrl Pts',(-4.30694841907298,-1.36111002720254,
5.34884638044292));
#76741=CARTESIAN_POINT('Ctrl Pts',(-4.18768244665581,-5.23484303577975,
1.74905588775117));
#76742=CARTESIAN_POINT('Ctrl Pts',(-4.06841647423865,-4.30308143644391,
-3.45633740526884));
#76743=CARTESIAN_POINT('Ctrl Pts',(-3.94915050182148,0.578833873119023,
-5.48887324093558));
#76744=CARTESIAN_POINT('Ctrl Pts',(-3.82988452940432,4.92938978238305,-2.48271917080172));
#76745=CARTESIAN_POINT('Ctrl Pts',(-3.71061855698715,4.75485184305665,2.80252779795483));
#76746=CARTESIAN_POINT('Ctrl Pts',(-3.59135258456999,0.215442839390763,
5.51510312602438));
#76747=CARTESIAN_POINT('Ctrl Pts',(-3.47208661215283,-4.52173893337813,
3.16490997124739));
#76748=CARTESIAN_POINT('Ctrl Pts',(-3.35282063973566,-5.10804322725765,
-2.09061533912767));
#76749=CARTESIAN_POINT('Ctrl Pts',(-3.2335546673185,-1.00525292597957,-5.42699222982105));
#76750=CARTESIAN_POINT('Ctrl Pts',(-3.11428869490133,4.02034202910876,-3.7814849036735));
#76751=CARTESIAN_POINT('Ctrl Pts',(-2.99502272248417,5.35533311875175,1.33535961258734));
#76752=CARTESIAN_POINT('Ctrl Pts',(-2.875756750067,1.77422180573573,5.2263672939988));
#76753=CARTESIAN_POINT('Ctrl Pts',(-2.75649077764984,-3.43559418140904,
4.31966095062996));
#76754=CARTESIAN_POINT('Ctrl Pts',(-2.63722480523267,-5.49159462892905,
-0.552418807831753));
#76755=CARTESIAN_POINT('Ctrl Pts',(-2.51795883281551,-2.50640698393315,
-4.91738773523297));
#76756=CARTESIAN_POINT('Ctrl Pts',(-2.39869286039835,2.77961855900976,-4.76828048400439));
#76757=CARTESIAN_POINT('Ctrl Pts',(-2.27942688798118,5.51400274306588,-0.241974910250199));
#76758=CARTESIAN_POINT('Ctrl Pts',(-2.16016091556402,3.18662857663998,4.5064594109201));
#76759=CARTESIAN_POINT('Ctrl Pts',(-2.04089494314685,-2.06601504634835,
5.11804258833305));
#76760=CARTESIAN_POINT('Ctrl Pts',(-1.92162897072969,-5.42209288938195,
1.03135193151629));
#76761=CARTESIAN_POINT('Ctrl Pts',(-1.80236299831252,-3.80078402465012,
-4.00210181101047));
#76762=CARTESIAN_POINT('Ctrl Pts',(-1.68309702589536,1.30957828666277,-5.3616958901853));
#76763=CARTESIAN_POINT('Ctrl Pts',(-1.56383105347819,5.21777057068265,-1.79934665349586));
#76764=CARTESIAN_POINT('Ctrl Pts',(-1.44456508106103,4.33614047199418,3.41477142937312));
#76765=CARTESIAN_POINT('Ctrl Pts',(-1.32529910864386,-0.525990954986324,
5.49418889582449));
#76766=CARTESIAN_POINT('Ctrl Pts',(-1.2060331362267,-4.90527185890021,2.53003677799559));
#76767=CARTESIAN_POINT('Ctrl Pts',(-1.08676716380953,-4.78159874734929,
-2.75664497661135));
#76768=CARTESIAN_POINT('Ctrl Pts',(-0.967501191392371,-0.268501379800935,
-5.51277472029953));
#76769=CARTESIAN_POINT('Ctrl Pts',(-0.848235218975206,4.49107557157286,
-3.20827341698774));
#76770=CARTESIAN_POINT('Ctrl Pts',(-0.72896924655804,5.12792347540635,2.04136692882621));
#76771=CARTESIAN_POINT('Ctrl Pts',(-0.609703274140877,1.05742706300564,
5.41706803669216));
#76772=CARTESIAN_POINT('Ctrl Pts',(-0.490437301723711,-3.98376895104567,
3.81999516392536));
#76773=CARTESIAN_POINT('Ctrl Pts',(-0.371171329306549,-5.36793454745627,
-1.28376664622291));
#76774=CARTESIAN_POINT('Ctrl Pts',(-0.251905356889381,-1.82442984943385,
-5.20905306483082));
#76775=CARTESIAN_POINT('Ctrl Pts',(-0.132639384472219,3.39386963117249,
-4.35251961906362));
#76776=CARTESIAN_POINT('Ctrl Pts',(-0.0133734120550536,5.49665598156906,
0.499550926342804));
#76777=CARTESIAN_POINT('Ctrl Pts',(0.105892560362111,2.55360800599929,4.89304243384675));
#76778=CARTESIAN_POINT('Ctrl Pts',(0.225158532779274,-2.73360758255891,
4.79480632479614));
#76779=CARTESIAN_POINT('Ctrl Pts',(0.344424505196442,-5.51141908615201,
0.295021634000305));
#76780=CARTESIAN_POINT('Ctrl Pts',(0.463690477613603,-3.22984399124939,
-4.4755877714462));
#76781=CARTESIAN_POINT('Ctrl Pts',(0.58295645003077,2.01667155712322,-5.13768565975176));
#76782=CARTESIAN_POINT('Ctrl Pts',(0.702222422447934,5.41191778806855,-1.08347771685263));
#76783=CARTESIAN_POINT('Ctrl Pts',(0.821488394865098,3.83911787679396,3.96534387358896));
#76784=CARTESIAN_POINT('Ctrl Pts',(0.940754367282264,-1.25792528876334,
5.37404894615022));
#76785=CARTESIAN_POINT('Ctrl Pts',(1.06002033969943,-5.20021497823882,1.84947081291638));
#76786=CARTESIAN_POINT('Ctrl Pts',(1.17928631211659,-4.36879801268882,-3.37288927064835));
#76787=CARTESIAN_POINT('Ctrl Pts',(1.29855228453375,0.473099333942919,-5.49899582905383));
#76788=CARTESIAN_POINT('Ctrl Pts',(1.41781825695092,4.88069974316303,-2.57712012231041));
#76789=CARTESIAN_POINT('Ctrl Pts',(1.53708422936808,4.80790291061196,2.71050691012911));
#76790=CARTESIAN_POINT('Ctrl Pts',(1.65635020178525,0.321535058949422,5.50993587200387));
#76791=CARTESIAN_POINT('Ctrl Pts',(1.77561617420242,-4.45999636905643,3.25133980010278));
#76792=CARTESIAN_POINT('Ctrl Pts',(1.89488214661958,-5.1473289153913,-1.99192950289544));
#76793=CARTESIAN_POINT('Ctrl Pts',(2.01414811903674,-1.10950329002883,-5.40664226273052));
#76794=CARTESIAN_POINT('Ctrl Pts',(2.13341409145391,3.94682700514964,-3.85815172059762));
#76795=CARTESIAN_POINT('Ctrl Pts',(2.25268006387108,5.38003894472928,1.23205481246771));
#76796=CARTESIAN_POINT('Ctrl Pts',(2.37194603628823,1.8744689642876,5.19125651549326));
#76797=CARTESIAN_POINT('Ctrl Pts',(2.4912120087054,-3.3518308334604,4.38497527605265));
#76798=CARTESIAN_POINT('Ctrl Pts',(2.61047798112256,-5.50120838411536,-0.446636790096184));
#76799=CARTESIAN_POINT('Ctrl Pts',(2.72974395353974,-2.6005725826633,-4.86824407256134));
#76800=CARTESIAN_POINT('Ctrl Pts',(2.84900992595689,2.68734349406327,-4.82088820163304));
#76801=CARTESIAN_POINT('Ctrl Pts',(2.96827589837406,5.50832511218907,-0.348041040907454));
#76802=CARTESIAN_POINT('Ctrl Pts',(3.08754187079122,3.27276034595634,4.44430172531797));
#76803=CARTESIAN_POINT('Ctrl Pts',(3.20680784320839,-1.96714133887937,5.1568530191));
#76804=CARTESIAN_POINT('Ctrl Pts',(3.32607381562555,-5.40124158279764,1.13550318008635));
#76805=CARTESIAN_POINT('Ctrl Pts',(3.44533978804272,-3.87709625473508,-3.92821877436172));
#76806=CARTESIAN_POINT('Ctrl Pts',(3.56460576045988,1.20615581619359,-5.38590440453517));
#76807=CARTESIAN_POINT('Ctrl Pts',(3.68387173287705,5.18217788396745,-1.8994237248827));
#76808=CARTESIAN_POINT('Ctrl Pts',(3.80313770529422,4.40105103467883,3.3306948070757));
#76809=CARTESIAN_POINT('Ctrl Pts',(3.92240367771138,-0.420163907365567,
5.50329359553678));
#76810=CARTESIAN_POINT('Ctrl Pts',(4.04166965012854,-4.85567571036938,2.6239648441733));
#76811=CARTESIAN_POINT('Ctrl Pts',(4.1609356225457,-4.83376189727187,-2.66411787055516));
#76812=CARTESIAN_POINT('Ctrl Pts',(4.28020159496287,-0.374538966305925,
-5.50658684399396));
#76813=CARTESIAN_POINT('Ctrl Pts',(4.39946756738004,4.42850420353529,-3.29410513296082));
#76814=CARTESIAN_POINT('Ctrl Pts',(4.5187335397972,5.16625775041094,1.94230763887896));
#76815=CARTESIAN_POINT('Ctrl Pts',(4.63799951221437,1.16147678517189,5.39571587328648));
#76816=CARTESIAN_POINT('Ctrl Pts',(4.75726548463153,-3.90951961197424,3.89595104067253));
#76817=CARTESIAN_POINT('Ctrl Pts',(4.8765314570487,-5.39164518979235,-1.1802288994588));
#76818=CARTESIAN_POINT('Ctrl Pts',(4.99579742946586,-1.92433451704137,-5.17297929381628));
#76819=CARTESIAN_POINT('Ctrl Pts',(5.11506340188302,3.30948168075747,-4.41702491644086));
#76820=CARTESIAN_POINT('Ctrl Pts',(5.23432937430019,5.5052514150489,0.393681298553378));
#76821=CARTESIAN_POINT('Ctrl Pts',(5.35359534671735,2.64729636534932,4.84299494752337));
#76822=CARTESIAN_POINT('Ctrl Pts',(5.47286131913452,-2.64083057723855,4.84652369952428));
#76823=CARTESIAN_POINT('Ctrl Pts',(5.59212729155168,-5.50472110765647,0.40102822176287));
#76824=CARTESIAN_POINT('Ctrl Pts',(5.71139326396885,-3.31537366702065,-4.41260416939415));
#76825=CARTESIAN_POINT('Ctrl Pts',(5.83065923638601,1.9174289777522,-5.17554289162062));
#76826=CARTESIAN_POINT('Ctrl Pts',(5.94992520880318,5.39006526210777,-1.18742350404059));
#76827=CARTESIAN_POINT('Ctrl Pts',(6.06919118122034,3.91471564195373,3.89072995084103));
#76828=CARTESIAN_POINT('Ctrl Pts',(6.18845715363751,-1.15427466242746,5.39726116761145));
#76829=CARTESIAN_POINT('Ctrl Pts',(6.30772312605466,-5.16366095797147,1.94920076412104));
#76830=CARTESIAN_POINT('Ctrl Pts',(6.42698909847183,-4.43289655157051,-3.28819194555351));
#76831=CARTESIAN_POINT('Ctrl Pts',(6.546255070889,0.367189576687042,-5.50708179733159));
#76832=CARTESIAN_POINT('Ctrl Pts',(6.66552104330615,4.83020207756152,-2.67056660610614));
#76833=CARTESIAN_POINT('Ctrl Pts',(6.78478701572333,4.85917331297616,2.61748215317485));
#76834=CARTESIAN_POINT('Ctrl Pts',(6.90405298814047,0.427508194096852,5.50272794636521));
#76835=CARTESIAN_POINT('Ctrl Pts',(7.02331896055767,-4.39660199095344,3.3365654558053));
#76836=CARTESIAN_POINT('Ctrl Pts',(7.14258493297481,-5.18470822779373,-1.89250593139799));
#76837=CARTESIAN_POINT('Ctrl Pts',(7.26185090539199,-1.21334273606982,-5.38428988006359));
#76838=CARTESIAN_POINT('Ctrl Pts',(7.38111687780915,3.87185022591093,-3.93338962420994));
#76839=CARTESIAN_POINT('Ctrl Pts',(7.50038285022631,5.40275220799211,1.12829370589621));
#76840=CARTESIAN_POINT('Ctrl Pts',(7.61964882264348,1.97402189051019,5.1542230921367));
#76841=CARTESIAN_POINT('Ctrl Pts',(7.73891479506064,-3.26682609428515,4.44866557266632));
#76842=CARTESIAN_POINT('Ctrl Pts',(7.8581807674778,-5.50878470001459,-0.34068935500509));
#76843=CARTESIAN_POINT('Ctrl Pts',(7.97744673989498,-2.69377502777718,-4.81729739661697));
#76844=CARTESIAN_POINT('Ctrl Pts',(8.09671271231213,2.5940731388404,-4.87171044481049));
#76845=CARTESIAN_POINT('Ctrl Pts',(8.21597868472929,5.50060740625855,-0.453978270341479));
#76846=CARTESIAN_POINT('Ctrl Pts',(8.33524465714647,3.35768000876078,4.38049803863634));
#76847=CARTESIAN_POINT('Ctrl Pts',(8.45451062956363,-1.86753907674248,5.19375354676834));
#76848=CARTESIAN_POINT('Ctrl Pts',(8.57377660198079,-5.37838986084429,1.23923388127339));
#76849=CARTESIAN_POINT('Ctrl Pts',(8.69304257439796,-3.95197255517013,-3.85288087421746));
#76850=CARTESIAN_POINT('Ctrl Pts',(8.81230854681512,1.10228663128005,-5.40811818382607));
#76851=CARTESIAN_POINT('Ctrl Pts',(8.93157451923229,5.14466591478258,-1.99879732164191));
#76852=CARTESIAN_POINT('Ctrl Pts',(9.05084049164945,4.46433161470217,3.24538462153554));
#76853=CARTESIAN_POINT('Ctrl Pts',(9.17010646406662,-0.314181246942596,
5.51036008367861));
#76854=CARTESIAN_POINT('Ctrl Pts',(9.28937243648378,-4.80428120341128,2.71692109312688));
#76855=CARTESIAN_POINT('Ctrl Pts',(9.40863840890095,-4.88413480481383,-2.57060407611415));
#76856=CARTESIAN_POINT('Ctrl Pts',(9.52790438131811,-0.480437837759446,
-5.49835953642338));
#76857=CARTESIAN_POINT('Ctrl Pts',(9.64717035373527,4.36429268522211,-3.37871683712107));
#76858=CARTESIAN_POINT('Ctrl Pts',(9.76643632615244,5.20267863916058,1.842528991726));
#76859=CARTESIAN_POINT('Ctrl Pts',(9.8857022985696,1.26509634031525,5.3723653410253));
#76860=CARTESIAN_POINT('Ctrl Pts',(10.0049682709868,-3.83382233486901,3.97046400467101));
#76861=CARTESIAN_POINT('Ctrl Pts',(10.1242342434039,-5.41335897090002,-1.07625404059861));
#76862=CARTESIAN_POINT('Ctrl Pts',(10.2435002158211,-2.02352648400704,-5.13498964714156));
#76863=CARTESIAN_POINT('Ctrl Pts',(10.3627661882383,3.22386802363844,-4.47989431503581));
#76864=CARTESIAN_POINT('Ctrl Pts',(10.4820321606554,5.5118079118561,0.287665866117311));
#76865=CARTESIAN_POINT('Ctrl Pts',(10.6012981330726,2.74000426636313,4.7911537992472));
#76866=CARTESIAN_POINT('Ctrl Pts',(10.7205641054897,-2.54707550826514,4.89644610538342));
#76867=CARTESIAN_POINT('Ctrl Pts',(10.8398300779069,-5.495984388894,0.506886283856618));
#76868=CARTESIAN_POINT('Ctrl Pts',(10.9590960503241,-3.39967545391932,-4.34798630583716));
#76869=CARTESIAN_POINT('Ctrl Pts',(11.0783620227413,1.81747625528963,-5.21148329836976));
#76870=CARTESIAN_POINT('Ctrl Pts',(11.1976279951584,5.36621646006394,-1.29092951452332));
#76871=CARTESIAN_POINT('Ctrl Pts',(11.3168939675756,3.98886354466695,3.81467504903838));
#76872=CARTESIAN_POINT('Ctrl Pts',(11.4361599399927,-1.05019653646226,5.41847444789871));
#76873=CARTESIAN_POINT('Ctrl Pts',(11.5554259124099,-5.12519451320274,2.04820880516737));
#76874=CARTESIAN_POINT('Ctrl Pts',(11.6746918848271,-4.49535331341717,-3.20227679866655));
#76875=CARTESIAN_POINT('Ctrl Pts',(11.7939578572442,0.261143826315328,-5.51312815103241));
#76876=CARTESIAN_POINT('Ctrl Pts',(11.9132238296614,4.77791548800185,-2.76302401314953));
#76877=CARTESIAN_POINT('Ctrl Pts',(12.0324898020786,4.90864406153351,2.5234879799398));
#76878=CARTESIAN_POINT('Ctrl Pts',(12.1517557744957,0.533322996396297,5.49348201865112));
#76879=CARTESIAN_POINT('Ctrl Pts',(12.2710217469129,-4.3315792779465,3.42055537399901));
#76880=CARTESIAN_POINT('Ctrl Pts',(12.3902877193301,-5.22016732058297,-1.79238144736173));
#76881=CARTESIAN_POINT('Ctrl Pts',(12.5095536917472,-1.3167328059034,-5.35994336029645));
#76882=CARTESIAN_POINT('Ctrl Pts',(12.6288196641644,3.79543945995277,-4.00717074923971));
#76883=CARTESIAN_POINT('Ctrl Pts',(12.7480856365815,5.42346449640753,1.02411472205801));
#76884=CARTESIAN_POINT('Ctrl Pts',(12.8673516089987,2.07284371376895,5.115280739707));
#76885=CARTESIAN_POINT('Ctrl Pts',(12.9866175814159,-3.18061144642024,4.51070825199652));
#76886=CARTESIAN_POINT('Ctrl Pts',(13.1058835538331,-5.51432077064615,-0.234615741476998));
#76887=CARTESIAN_POINT('Ctrl Pts',(13.2251495262502,-2.78597980061803,-4.76456657611972));
#76888=CARTESIAN_POINT('Ctrl Pts',(13.3444154986674,2.49984203714938,-4.92072839090208));
#76889=CARTESIAN_POINT('Ctrl Pts',(13.4636814710845,5.49085248362037,-0.55974736341345));
#76890=CARTESIAN_POINT('Ctrl Pts',(13.5829474435017,3.44135611402541,4.31507198134501));
#76891=CARTESIAN_POINT('Ctrl Pts',(13.7022134159189,-1.76724514884449,5.22873050477977));
#76892=CARTESIAN_POINT('Ctrl Pts',(13.8214793883361,-5.35354618693448,1.34250561715309));
#76893=CARTESIAN_POINT('Ctrl Pts',(13.9407453607532,-4.02538519460857,-3.77611601288347));
#76894=CARTESIAN_POINT('Ctrl Pts',(14.0600113331704,0.998009201135608,-5.42832900091525));
#76895=CARTESIAN_POINT('Ctrl Pts',(14.1792773055875,5.10524855614116,-2.09743063955568));
#76896=CARTESIAN_POINT('Ctrl Pts',(14.2985432780047,4.52595877533329,3.15887246841535));
#76897=CARTESIAN_POINT('Ctrl Pts',(14.4178092504219,-0.208082225682183,
5.51538574309033));
#76898=CARTESIAN_POINT('Ctrl Pts',(14.537075222839,-4.75110737260535,2.80887109738119));
#76899=CARTESIAN_POINT('Ctrl Pts',(14.6563411952562,-4.93269881375749,-2.47613822725719));
#76900=CARTESIAN_POINT('Ctrl Pts',(14.7756071676734,-0.586158773228975,
-5.48809584467104));
#76901=CARTESIAN_POINT('Ctrl Pts',(14.8948731400905,4.29846479814849,-3.46207719249681));
#76902=CARTESIAN_POINT('Ctrl Pts',(15.0141391125077,5.23717265273706,1.74206794160044));
#76903=CARTESIAN_POINT('Ctrl Pts',(15.1334050849249,1.36824735167569,5.34702508806171));
#76904=CARTESIAN_POINT('Ctrl Pts',(15.252671057342,-3.75670515513534,4.04350645914012));
#76905=CARTESIAN_POINT('Ctrl Pts',(15.3719370297592,-5.43306784881692,-0.971880577993402));
#76906=CARTESIAN_POINT('Ctrl Pts',(15.4912030021763,-2.12196901338186,-5.09509819473345));
#76907=CARTESIAN_POINT('Ctrl Pts',(15.6104689745935,3.13706036787251,-4.54110453040358));
#76908=CARTESIAN_POINT('Ctrl Pts',(15.7297349470107,5.51632304371251,0.181543893136862));
#76909=CARTESIAN_POINT('Ctrl Pts',(15.8490009194278,2.83169737354434,4.73753818901663));
#76910=CARTESIAN_POINT('Ctrl Pts',(15.968266891845,-2.45237709896633,4.94455505300465));
#76911=CARTESIAN_POINT('Ctrl Pts',(16.0875328642621,-5.48521216561456,0.612556614463475));
#76912=CARTESIAN_POINT('Ctrl Pts',(16.2067988366793,-3.4827181297554,-4.28175811278522));
#76913=CARTESIAN_POINT('Ctrl Pts',(16.3260648090965,1.71685040843935,-5.24549356903332));
#76914=CARTESIAN_POINT('Ctrl Pts',(16.4453307815136,5.34038021463043,-1.39395741359364));
#76915=CARTESIAN_POINT('Ctrl Pts',(16.5645967539308,4.06153412335787,3.73720733603697));
#76916=CARTESIAN_POINT('Ctrl Pts',(16.683862726348,-0.945729457464844,5.43768093041616));
#76917=CARTESIAN_POINT('Ctrl Pts',(16.8031286987652,-5.08482989044738,2.14645826722576));
#76918=CARTESIAN_POINT('Ctrl Pts',(16.9223946711823,-4.55614516660902,-3.11517564970488));
#76919=CARTESIAN_POINT('Ctrl Pts',(17.0416606435995,0.155001358158474,-5.51713265081576));
#76920=CARTESIAN_POINT('Ctrl Pts',(17.1609266160166,4.723859339457,-2.85445810071785));
#76921=CARTESIAN_POINT('Ctrl Pts',(17.2801925884338,4.9562968341919,2.42855920230665));
#76922=CARTESIAN_POINT('Ctrl Pts',(17.399458560851,0.63894027605163,5.48220151320319));
#76923=CARTESIAN_POINT('Ctrl Pts',(17.5187245332682,-4.26495231198646,3.50327844799843));
#76924=CARTESIAN_POINT('Ctrl Pts',(17.6379905056853,-5.25369306105365,-1.69159313310433));
#76925=CARTESIAN_POINT('Ctrl Pts',(17.7572564781025,-1.41963520776255,-5.33361172045822));
#76926=CARTESIAN_POINT('Ctrl Pts',(17.8765224505196,3.71762300692966,-4.07946776995188));
#76927=CARTESIAN_POINT('Ctrl Pts',(17.9957884229368,5.44216813892813,0.919556444903994));
#76928=CARTESIAN_POINT('Ctrl Pts',(18.115054395354,2.17089783420263,5.07444388097677));
#76929=CARTESIAN_POINT('Ctrl Pts',(18.2343203677711,-3.09321882050645,4.57108033578427));
#76930=CARTESIAN_POINT('Ctrl Pts',(18.3535863401883,-5.51781454565922,-0.128455235161643));
#76931=CARTESIAN_POINT('Ctrl Pts',(18.4728523126055,-2.87715275202947,-4.71007114056864));
#76932=CARTESIAN_POINT('Ctrl Pts',(18.5921182850226,2.40468508862193,-4.96792388551679));
#76933=CARTESIAN_POINT('Ctrl Pts',(18.7113842574398,5.4790639571286,-0.665309147256506));
#76934=CARTESIAN_POINT('Ctrl Pts',(18.830650229857,3.52375767128937,4.24804778477804));
#76935=CARTESIAN_POINT('Ctrl Pts',(18.9499162022741,-1.66629670025835,5.26177093899355));
#76936=CARTESIAN_POINT('Ctrl Pts',(19.0691821746913,-5.32671976222436,1.44528013978514));
#76937=CARTESIAN_POINT('Ctrl Pts',(19.1884481471084,-4.09730698378862,-3.69795262115746));
#76938=CARTESIAN_POINT('Ctrl Pts',(19.3077141195256,0.893362146171608,-5.4465293704814));
#76939=CARTESIAN_POINT('Ctrl Pts',(19.4269800919428,5.06394040674028,-2.19528714857806));
#76940=CARTESIAN_POINT('Ctrl Pts',(19.5462460643599,4.58590969220547,3.07119038854062));
#76941=CARTESIAN_POINT('Ctrl Pts',(19.6655120367771,-0.101906138644027,
5.51836871245802));
#76942=CARTESIAN_POINT('Ctrl Pts',(19.7847780091943,-4.69617391152509,2.89978080213661));
#76943=CARTESIAN_POINT('Ctrl Pts',(19.9040439816114,-4.97943593783279,-2.38075531055748));
#76944=CARTESIAN_POINT('Ctrl Pts',(20.0233099540286,-0.691662617683489,
-5.47579957001972));
#76945=CARTESIAN_POINT('Ctrl Pts',(20.1425759264457,4.23104492247119,-3.54415532556908));
#76946=CARTESIAN_POINT('Ctrl Pts',(20.2618418988629,5.26972701586384,1.64096169547102));
#76947=CARTESIAN_POINT('Ctrl Pts',(20.3811078712801,1.47089161602474,5.31970449946583));
#76948=CARTESIAN_POINT('Ctrl Pts',(20.5003738436973,-3.67819663405649,4.1150513519207));
#76949=CARTESIAN_POINT('Ctrl Pts',(20.6196398161144,-5.45076452412087,-0.867147167621348));
#76950=CARTESIAN_POINT('Ctrl Pts',(20.7389057885316,-2.21962564578078,-5.05331971087533));
#76951=CARTESIAN_POINT('Ctrl Pts',(20.8581717609487,3.04909086372826,-4.60063289259834));
#76952=CARTESIAN_POINT('Ctrl Pts',(20.9774377333659,5.51879513838413,0.0753546831722458));
#76953=CARTESIAN_POINT('Ctrl Pts',(21.0967037057831,2.92234172723827,4.68216797402346));
#76954=CARTESIAN_POINT('Ctrl Pts',(21.2159696782002,-2.35677042204708,4.99083272465557));
#76955=CARTESIAN_POINT('Ctrl Pts',(21.3352356506174,-5.47240842744157,0.718000077294374));
#76956=CARTESIAN_POINT('Ctrl Pts',(21.4545016230345,-3.56447093866641,-4.21394411865316));
#76957=CARTESIAN_POINT('Ctrl Pts',(21.5737675954518,1.6155887052047,-5.27756110749501));
#76958=CARTESIAN_POINT('Ctrl Pts',(21.6930335678689,5.31256609457409,-1.49646904361904));
#76959=CARTESIAN_POINT('Ctrl Pts',(21.8122995402861,4.13270046359602,3.6583555029442));
#76960=CARTESIAN_POINT('Ctrl Pts',(21.9315655127032,-0.840912116085472,
5.45487350181007));
#76961=CARTESIAN_POINT('Ctrl Pts',(22.0508314851204,-5.04258203923305,2.2439127624158));
#76962=CARTESIAN_POINT('Ctrl Pts',(22.1700974575376,-4.61524959614565,-3.02692075763577));
#76963=CARTESIAN_POINT('Ctrl Pts',(22.2893634299547,0.048801483367409,-5.51909381356669));
#76964=CARTESIAN_POINT('Ctrl Pts',(22.4086294023719,4.66805365227747,-2.94483500508725));
#76965=CARTESIAN_POINT('Ctrl Pts',(22.527895374789,5.00211398216874,2.33273097830009));
#76966=CARTESIAN_POINT('Ctrl Pts',(22.6471613472062,0.744320916421722,5.46889060789352));
#76967=CARTESIAN_POINT('Ctrl Pts',(22.7664273196234,-4.1967457691786,3.58470404030929));
#76968=CARTESIAN_POINT('Ctrl Pts',(22.8856932920405,-5.28527303254098,-1.59017831680098));
#76969=CARTESIAN_POINT('Ctrl Pts',(23.0049592644577,-1.52201183049409,-5.30530471279124));
#76970=CARTESIAN_POINT('Ctrl Pts',(23.1242252368749,3.63842968710919,-4.15025391026752));
#76971=CARTESIAN_POINT('Ctrl Pts',(23.243491209292,5.45885620843297,0.81465759886084));
#76972=CARTESIAN_POINT('Ctrl Pts',(23.3627571817092,2.26814793627769,5.03172764037246));
#76973=CARTESIAN_POINT('Ctrl Pts',(23.4820231541264,-3.00468058346354,4.62975946449548));
#76974=CARTESIAN_POINT('Ctrl Pts',(23.6012891265435,-5.51926473109169,-0.0222471538909869));
#76975=CARTESIAN_POINT('Ctrl Pts',(23.7205550989607,-2.96726011500245,-4.65383127300986));
#76976=CARTESIAN_POINT('Ctrl Pts',(23.8398210713778,2.30863753578895,-5.01327944923028));
#76977=CARTESIAN_POINT('Ctrl Pts',(23.959087043795,5.46524619280696,-0.77062452578279));
#76978=CARTESIAN_POINT('Ctrl Pts',(24.0783530162122,3.60485416213592,4.17945027216024));
#76979=CARTESIAN_POINT('Ctrl Pts',(24.1976189886294,-1.56473111846732,5.29286261248375));
#76980=CARTESIAN_POINT('Ctrl Pts',(24.3168849610465,-5.29792052220578,1.5475193853777));
#76981=CARTESIAN_POINT('Ctrl Pts',(24.4361509334637,-4.16771128560285,-3.61841964780034));
#76982=CARTESIAN_POINT('Ctrl Pts',(24.5554169058808,0.788384223695067,-5.46271255179668));
#76983=CARTESIAN_POINT('Ctrl Pts',(24.6746828782981,5.0207567655543,-2.29233060636324));
#76984=CARTESIAN_POINT('Ctrl Pts',(24.7939488507152,4.64416216176915,2.98237085603393));
#76985=CARTESIAN_POINT('Ctrl Pts',(24.9132148231324,0.00430769056925928,
5.51930788700271));
#76986=CARTESIAN_POINT('Ctrl Pts',(25.0324807955495,-4.63950116544441,2.98961653788056));
#76987=CARTESIAN_POINT('Ctrl Pts',(25.1517467679667,-5.02432886737874,-2.28449065223597));
#76988=CARTESIAN_POINT('Ctrl Pts',(25.2710127403838,-0.796910296493555,
-5.46147526654391));
#76989=CARTESIAN_POINT('Ctrl Pts',(25.390278712801,4.1620580279593,-3.62492083770507));
#76990=CARTESIAN_POINT('Ctrl Pts',(25.5095446852181,5.3003296716376,1.53924769926319));
#76991=CARTESIAN_POINT('Ctrl Pts',(25.6288106576354,1.57299111781316,5.29041369374921));
#76992=CARTESIAN_POINT('Ctrl Pts',(25.7480766300525,-3.59832584821597,4.18507218549331));
#76993=CARTESIAN_POINT('Ctrl Pts',(25.8673426024697,-5.46644244263356,-0.762092598772189));
#76994=CARTESIAN_POINT('Ctrl Pts',(25.9866085748868,-2.31646021288461,-5.00966966873574));
#76995=CARTESIAN_POINT('Ctrl Pts',(26.105874547304,2.95999209177915,-4.65845735456855));
#76996=CARTESIAN_POINT('Ctrl Pts',(26.2251405197212,5.5192232803009,-0.0308624353137705));
#76997=CARTESIAN_POINT('Ctrl Pts',(26.3444064921383,3.01190375620826,4.62506366129882));
#76998=CARTESIAN_POINT('Ctrl Pts',(26.4636724645555,-2.26029088660046,5.03526198083872));
#76999=CARTESIAN_POINT('Ctrl Pts',(26.5829384369726,-5.45757791639507,0.823177620083097));
#77000=CARTESIAN_POINT('Ctrl Pts',(26.7022044093898,-3.6449036025072,-4.1445694391768));
#77001=CARTESIAN_POINT('Ctrl Pts',(26.821470381807,1.51372864908642,-5.30767403715261));
#77002=CARTESIAN_POINT('Ctrl Pts',(26.9407363542241,5.28278440119203,-1.59842643817319));
#77003=CARTESIAN_POINT('Ctrl Pts',(27.0600023266413,4.20233620806344,3.57814875349353));
#77004=CARTESIAN_POINT('Ctrl Pts',(27.1792682990585,-0.735783332698646,
5.47004579460281));
#77005=CARTESIAN_POINT('Ctrl Pts',(27.2985342714756,-4.9984666065644,2.34053619728246));
#77006=CARTESIAN_POINT('Ctrl Pts',(27.4178002438929,-4.67264471198416,-2.93754480872971));
#77007=CARTESIAN_POINT('Ctrl Pts',(27.5370662163099,-0.0574164656453142,
-5.51901091294461));
#77008=CARTESIAN_POINT('Ctrl Pts',(27.6563321887272,4.61051909477695,-3.0341212540744));
#77009=CARTESIAN_POINT('Ctrl Pts',(27.7755981611443,5.04607853652714,2.23603879906599));
#77010=CARTESIAN_POINT('Ctrl Pts',(27.8948641335615,0.849425888507462,5.45355423257733));
#77011=CARTESIAN_POINT('Ctrl Pts',(28.0141301059786,-4.126984910644,3.66480199397535));
#77012=CARTESIAN_POINT('Ctrl Pts',(28.1333960783958,-5.31489553901918,-1.48817455865981));
#77013=CARTESIAN_POINT('Ctrl Pts',(28.252662050813,-1.62382475767335,-5.27503282113916));
#77014=CARTESIAN_POINT('Ctrl Pts',(28.3719280232301,3.5578888306985,-4.21950295368066));
#77015=CARTESIAN_POINT('Ctrl Pts',(28.4911939956473,5.47352252429297,0.709457034489319));
#77016=CARTESIAN_POINT('Ctrl Pts',(28.6104599680644,2.36455800223863,4.9871478383719));
#77017=CARTESIAN_POINT('Ctrl Pts',(28.7297259404816,-2.91502952650204,4.68672390560296));
#77018=CARTESIAN_POINT('Ctrl Pts',(28.8489919128988,-5.51867078984984,0.0839691668831474));
#77019=CARTESIAN_POINT('Ctrl Pts',(28.9682578853159,-3.05626851718156,-4.59586780256059));
#77020=CARTESIAN_POINT('Ctrl Pts',(29.0875238577331,2.21173495102714,-5.05677828405932));
#77021=CARTESIAN_POINT('Ctrl Pts',(29.2067898301503,5.4494043082322,-0.875654494163783));
#77022=CARTESIAN_POINT('Ctrl Pts',(29.3260558025674,3.68461555149545,4.10930484941263));
#77023=CARTESIAN_POINT('Ctrl Pts',(29.4453217749846,-1.46258601951706,5.32199401007199));
#77024=CARTESIAN_POINT('Ctrl Pts',(29.5645877474018,-5.26715913302683,1.64918548838541));
#77025=CARTESIAN_POINT('Ctrl Pts',(29.6838537198189,-4.2365720249636,-3.53754654881376));
#77026=CARTESIAN_POINT('Ctrl Pts',(29.8031196922361,0.683114313553423,-5.47687255122367));
#77027=CARTESIAN_POINT('Ctrl Pts',(29.9223856646533,4.97571362616884,-2.38852507168894));
#77028=CARTESIAN_POINT('Ctrl Pts',(30.0416516370704,4.70069460951519,2.89244676628684));
#77029=CARTESIAN_POINT('Ctrl Pts',(30.1609176094876,0.11051992437719,5.51820291888986));
#77030=CARTESIAN_POINT('Ctrl Pts',(30.2801835819047,-4.58111012380261,3.0783450328581));
#77031=CARTESIAN_POINT('Ctrl Pts',(30.3994495543219,-5.06736097575394,-2.18737990507693));
#77032=CARTESIAN_POINT('Ctrl Pts',(30.518715526739,-0.901862829904248,-5.44512823942338));
#77033=CARTESIAN_POINT('Ctrl Pts',(30.6379814991563,4.09152966474647,-3.70434381641723));
#77034=CARTESIAN_POINT('Ctrl Pts',(30.7572474715734,5.3289692859932,1.43696362398964));
#77035=CARTESIAN_POINT('Ctrl Pts',(30.8765134439906,1.67450804325163,5.25916351911732));
#77036=CARTESIAN_POINT('Ctrl Pts',(30.9957794164077,-3.51712237872867,4.25354302679248));
#77037=CARTESIAN_POINT('Ctrl Pts',(31.1150453888249,-5.48009579784741,-0.656755779680257));
#77038=CARTESIAN_POINT('Ctrl Pts',(31.2343113612421,-2.41243685083647,-4.9641642346376));
#77039=CARTESIAN_POINT('Ctrl Pts',(31.3535773336592,2.8697970508367,-4.71455650032301));
#77040=CARTESIAN_POINT('Ctrl Pts',(31.4728433060764,5.51760731089503,-0.137068123522462));
#77041=CARTESIAN_POINT('Ctrl Pts',(31.5921092784935,3.10035029007019,4.566246400118));
#77042=CARTESIAN_POINT('Ctrl Pts',(31.7113752509108,-2.1629742249933,5.07782636663992));
#77043=CARTESIAN_POINT('Ctrl Pts',(31.8306412233279,-5.44072612513458,0.928050289050349));
#77044=CARTESIAN_POINT('Ctrl Pts',(31.949907195745,-3.72398633206484,-4.07365976811063));
#77045=CARTESIAN_POINT('Ctrl Pts',(32.0691731681622,1.41130796519246,-5.33582120531725));
#77046=CARTESIAN_POINT('Ctrl Pts',(32.1884391405794,5.25104616449558,-1.69979183609775));
#77047=CARTESIAN_POINT('Ctrl Pts',(32.3077051129965,4.27041556631729,3.49661679322797));
#77048=CARTESIAN_POINT('Ctrl Pts',(32.4269710854137,-0.630382043025125,
5.48319218955167));
#77049=CARTESIAN_POINT('Ctrl Pts',(32.5462370578309,-4.95249993112703,2.43629278616405));
#77050=CARTESIAN_POINT('Ctrl Pts',(32.6655030302481,-4.72830925714705,-2.84708090445397));
#77051=CARTESIAN_POINT('Ctrl Pts',(32.7847690026652,-0.163613149773239,
-5.51688397965284));
#77052=CARTESIAN_POINT('Ctrl Pts',(32.9040349750824,4.5512769755768,-3.12228377943339));
#77053=CARTESIAN_POINT('Ctrl Pts',(33.0233009474995,5.08817421446106,2.13851847572625));
#77054=CARTESIAN_POINT('Ctrl Pts',(33.1425669199167,0.954216265406902,5.4361980672674));
#77055=CARTESIAN_POINT('Ctrl Pts',(33.2618328923338,-4.05569557316294,3.74354264374733));
#77056=CARTESIAN_POINT('Ctrl Pts',(33.381098864751,-5.3425496094337,-1.38561963701042));
#77057=CARTESIAN_POINT('Ctrl Pts',(33.5003648371682,-1.72503628164692,-5.24280725706473));
#77058=CARTESIAN_POINT('Ctrl Pts',(33.6196308095854,3.47603026698121,-4.28718925296732));
#77059=CARTESIAN_POINT('Ctrl Pts',(33.7388967820025,5.48616165466014,0.603993714095214));
#77060=CARTESIAN_POINT('Ctrl Pts',(33.8581627544197,2.46009232544721,4.94072098564613));
#77061=CARTESIAN_POINT('Ctrl Pts',(33.9774287268369,-2.82429885297868,4.74195256163424));
#77062=CARTESIAN_POINT('Ctrl Pts',(34.096694699254,-5.51603294190759,0.190154388657318));
#77063=CARTESIAN_POINT('Ctrl Pts',(34.2159606716712,-3.14414499322367,-4.53620219669603));
#77064=CARTESIAN_POINT('Ctrl Pts',(34.3352266440883,2.11401322338287,-5.09840427968194));
#77065=CARTESIAN_POINT('Ctrl Pts',(34.4544926165055,5.43154417064249,-0.980360153276489));
#77066=CARTESIAN_POINT('Ctrl Pts',(34.5737585889227,3.7630122987619,4.03763749574514));
#77067=CARTESIAN_POINT('Ctrl Pts',(34.6930245613398,-1.35989923407058,5.34915434258951));
#77068=CARTESIAN_POINT('Ctrl Pts',(34.812290533757,-5.23444698756834,1.75024079553662));
#77069=CARTESIAN_POINT('Ctrl Pts',(34.9315565061742,-4.30386369840905,-3.45536327653838));
#77070=CARTESIAN_POINT('Ctrl Pts',(35.0508224785913,0.577591403638233,-5.48900412442188));
#77071=CARTESIAN_POINT('Ctrl Pts',(35.1700884510085,4.92882767104235,-2.48383491779139));
#77072=CARTESIAN_POINT('Ctrl Pts',(35.2893544234257,4.75548609761399,2.80145142382315));
#77073=CARTESIAN_POINT('Ctrl Pts',(35.4086203958428,0.216691226457424,5.51505421727112));
#77074=CARTESIAN_POINT('Ctrl Pts',(35.52788636826,-4.52102241369882,3.16593342555851));
#77075=CARTESIAN_POINT('Ctrl Pts',(35.6471523406772,-5.10851632308625,-2.08945903553642));
#77076=CARTESIAN_POINT('Ctrl Pts',(35.7664183130943,-1.00648135204571,-5.42676454238525));
#77077=CARTESIAN_POINT('Ctrl Pts',(35.8856842855115,4.01948596255725,-3.782394847567));
#77078=CARTESIAN_POINT('Ctrl Pts',(36.0049502579287,5.35563523539815,1.33414735393709));
#77079=CARTESIAN_POINT('Ctrl Pts',(36.1242162303458,1.77540482566106,5.22596554539102));
#77080=CARTESIAN_POINT('Ctrl Pts',(36.243482202763,-3.43461635982299,4.32043852452331));
#77081=CARTESIAN_POINT('Ctrl Pts',(36.3627481751802,-5.49171941999376,-0.551175737763215));
#77082=CARTESIAN_POINT('Ctrl Pts',(36.4820141475973,-2.50752022830702,-4.91682023424888));
#77083=CARTESIAN_POINT('Ctrl Pts',(36.6012801200145,2.77853955367696,-4.76890960570523));
#77084=CARTESIAN_POINT('Ctrl Pts',(36.7205460924316,5.51394705382706,-0.243222946520996));
#77085=CARTESIAN_POINT('Ctrl Pts',(36.8398120648488,3.18765004325205,4.50573778353591));
#77086=CARTESIAN_POINT('Ctrl Pts',(36.959078037266,-2.06485927485046,5.11851047989713));
#77087=CARTESIAN_POINT('Ctrl Pts',(37.0783440096832,-5.42185398584499,1.03257855562554));
#77088=CARTESIAN_POINT('Ctrl Pts',(37.1976099821003,-3.80169992186118,-4.00124006152411));
#77089=CARTESIAN_POINT('Ctrl Pts',(37.3168759545175,1.30838373881677,-5.36199466824331));
#77090=CARTESIAN_POINT('Ctrl Pts',(37.4361419269346,5.21732676183604,-1.80052298340626));
#77091=CARTESIAN_POINT('Ctrl Pts',(37.5554078993518,4.33698241739598,3.41378086864505));
#77092=CARTESIAN_POINT('Ctrl Pts',(37.6746738717689,-0.524878515764003,
5.4943248165015));
#77093=CARTESIAN_POINT('Ctrl Pts',(37.7939398441862,-4.9044497775631,2.53111477860059));
#77094=CARTESIAN_POINT('Ctrl Pts',(37.9132058166033,-4.78269608681437,-2.75550123298751));
#77095=CARTESIAN_POINT('Ctrl Pts',(38.0324717890204,-0.268849601375951,
-5.51283021355248));
#77096=CARTESIAN_POINT('Ctrl Pts',(38.1517377614376,4.48863752569352,-3.20906923476978));
#77097=CARTESIAN_POINT('Ctrl Pts',(38.2710037338548,5.13166198877306,2.03979046086845));
#77098=CARTESIAN_POINT('Ctrl Pts',(38.3902697062719,1.0522136396721,5.41758791291211));
#77099=CARTESIAN_POINT('Ctrl Pts',(38.4896580166196,-3.1319986375449,4.08605008372047));
#77100=CARTESIAN_POINT('Ctrl Pts',(38.5691686648977,-4.689252124851,1.26661108229022));
#77101=CARTESIAN_POINT('Ctrl Pts',(38.6089239890367,-4.72001247217602,-0.328601748833628));
#77102=CARTESIAN_POINT('Ctrl Pts',(38.6288016511063,-4.53940850365245,-1.08453452292322));
#77103=CARTESIAN_POINT('Ctrl Pts',(-17.7012016511063,-2.05512567986496,
4.34950232174947));
#77104=CARTESIAN_POINT('Ctrl Pts',(-17.6813239890368,-2.77943400182884,
4.00726899883239));
#77105=CARTESIAN_POINT('Ctrl Pts',(-17.6415686648977,-4.04231267840295,
2.95387391985648));
#77106=CARTESIAN_POINT('Ctrl Pts',(-17.5620580166196,-5.30524713465376,
-0.116410492754025));
#77107=CARTESIAN_POINT('Ctrl Pts',(-17.462669706272,-3.67778290240344,-4.33957689005188));
#77108=CARTESIAN_POINT('Ctrl Pts',(-17.3434037338548,1.66891228174828,-5.44172406759916));
#77109=CARTESIAN_POINT('Ctrl Pts',(-17.2241377614376,5.47488290767653,-1.53998020197864));
#77110=CARTESIAN_POINT('Ctrl Pts',(-17.1048717890205,4.25951367249169,3.77108835234815));
#77111=CARTESIAN_POINT('Ctrl Pts',(-16.9856058166033,-0.86837967644224,
5.62264033298406));
#77112=CARTESIAN_POINT('Ctrl Pts',(-16.8663398441862,-5.1978714987074,2.31150944439501));
#77113=CARTESIAN_POINT('Ctrl Pts',(-16.747073871769,-4.75646285723963,-3.12091671530309));
#77114=CARTESIAN_POINT('Ctrl Pts',(-16.6278078993518,0.051640530934677,
-5.6887274769557));
#77115=CARTESIAN_POINT('Ctrl Pts',(-16.5085419269346,4.81215727784529,-3.03421098473609));
#77116=CARTESIAN_POINT('Ctrl Pts',(-16.3892759545175,5.15529314801688,2.40556632308164));
#77117=CARTESIAN_POINT('Ctrl Pts',(-16.2700099821003,0.765909498650872,
5.63712411222854));
#77118=CARTESIAN_POINT('Ctrl Pts',(-16.1507440096831,-4.32653921855433,
3.69387479286789));
#77119=CARTESIAN_POINT('Ctrl Pts',(-16.031478037266,-5.4473143396903,-1.64027374325625));
#77120=CARTESIAN_POINT('Ctrl Pts',(-15.9122120648488,-1.56754255743221,
-5.4686866558594));
#77121=CARTESIAN_POINT('Ctrl Pts',(-15.7929460924317,3.75120208696408,-4.27693687578484));
#77122=CARTESIAN_POINT('Ctrl Pts',(-15.6736801200145,5.62641067462387,0.840964405285497));
#77123=CARTESIAN_POINT('Ctrl Pts',(-15.5544141475974,2.33667131925813,5.18687606040634));
#77124=CARTESIAN_POINT('Ctrl Pts',(-15.4351481751802,-3.09809098985903,
4.77132541153072));
#77125=CARTESIAN_POINT('Ctrl Pts',(-15.315882202763,-5.68886010004097,-0.0242184643975601));
#77126=CARTESIAN_POINT('Ctrl Pts',(-15.1966162303458,-3.05735469922997,
-4.79753036288636));
#77127=CARTESIAN_POINT('Ctrl Pts',(-15.0773502579287,2.38074891093858,-5.1667929809382));
#77128=CARTESIAN_POINT('Ctrl Pts',(-14.9580842855115,5.63336658597595,-0.793029796302506));
#77129=CARTESIAN_POINT('Ctrl Pts',(-14.8388183130943,3.71465196168976,4.30872093236743));
#77130=CARTESIAN_POINT('Ctrl Pts',(-14.7195523406772,-1.61404836555687,
5.45514098034502));
#77131=CARTESIAN_POINT('Ctrl Pts',(-14.60028636826,-5.46108044956259,1.59383675552073));
#77132=CARTESIAN_POINT('Ctrl Pts',(-14.4810203958429,-4.29493592219251,
-3.73058181656837));
#77133=CARTESIAN_POINT('Ctrl Pts',(-14.3617544234257,0.813884873630489,
-5.63039134303743));
#77134=CARTESIAN_POINT('Ctrl Pts',(-14.2424884510085,5.17557355104494,-2.36159981502903));
#77135=CARTESIAN_POINT('Ctrl Pts',(-14.1232224785913,4.7861759733498,3.07509915586776));
#77136=CARTESIAN_POINT('Ctrl Pts',(-14.0039565061742,0.00315232627448166,
5.68891073308194));
#77137=CARTESIAN_POINT('Ctrl Pts',(-13.884690533757,-4.78276510147707,3.08040147561366));
#77138=CARTESIAN_POINT('Ctrl Pts',(-13.7654245613399,-5.17818758041288,
-2.35586261241017));
#77139=CARTESIAN_POINT('Ctrl Pts',(-13.6461585889227,-0.820124171393288,
-5.62948590992118));
#77140=CARTESIAN_POINT('Ctrl Pts',(-13.5268926165055,4.29079892350715,-3.73533932389453));
#77141=CARTESIAN_POINT('Ctrl Pts',(-13.4076266440884,5.46284344083135,1.58778361482599));
#77142=CARTESIAN_POINT('Ctrl Pts',(-13.2883606716712,1.62009295488011,5.45334888706914));
#77143=CARTESIAN_POINT('Ctrl Pts',(-13.169094699254,-3.70987460822074,4.3128349907969));
#77144=CARTESIAN_POINT('Ctrl Pts',(-13.0498287268369,-5.63424198350418,
-0.786786208491855));
#77145=CARTESIAN_POINT('Ctrl Pts',(-12.9305627544197,-2.38647348263151,
-5.16415139042731));
#77146=CARTESIAN_POINT('Ctrl Pts',(-12.8112967820026,3.05203605370893,-4.80091566197721));
#77147=CARTESIAN_POINT('Ctrl Pts',(-12.6920308095854,5.68882972215975,-0.0305230868001199));
#77148=CARTESIAN_POINT('Ctrl Pts',(-12.5727648371682,3.10337692241222,4.76788914971767));
#77149=CARTESIAN_POINT('Ctrl Pts',(-12.453498864751,-2.33092176727756,5.18946230175999));
#77150=CARTESIAN_POINT('Ctrl Pts',(-12.3342328923339,-5.62547492733827,
0.847199568251026));
#77151=CARTESIAN_POINT('Ctrl Pts',(-12.2149669199167,-3.75594021589945,
-4.27277759322264));
#77152=CARTESIAN_POINT('Ctrl Pts',(-12.0957009474995,1.56148210779135,-5.47041944402838));
#77153=CARTESIAN_POINT('Ctrl Pts',(-11.9764349750824,5.44549108975312,-1.64631165274856));
#77154=CARTESIAN_POINT('Ctrl Pts',(-11.8571690026652,4.33063422408794,3.68908152305075));
#77155=CARTESIAN_POINT('Ctrl Pts',(-11.7379030302481,-0.759669330323711,
5.63796220057583));
#77156=CARTESIAN_POINT('Ctrl Pts',(-11.6186370578309,-5.1526096886059,2.41129190755513));
#77157=CARTESIAN_POINT('Ctrl Pts',(-11.4993710854137,-4.8155442174797,-3.02890230216396));
#77158=CARTESIAN_POINT('Ctrl Pts',(-11.3801051129966,-0.0578931408065744,
-5.68861702444486));
#77159=CARTESIAN_POINT('Ctrl Pts',(-11.2608391405794,4.75290282943444,-3.12628053131998));
#77160=CARTESIAN_POINT('Ctrl Pts',(-11.1415731681623,5.20061689584915,2.30592696527117));
#77161=CARTESIAN_POINT('Ctrl Pts',(-11.0223071957451,0.874255353881844,
5.62133372455018));
#77162=CARTESIAN_POINT('Ctrl Pts',(-10.9030412233279,-4.25465735538948,
3.77645416426396));
#77163=CARTESIAN_POINT('Ctrl Pts',(-10.7837752509108,-5.47786881629542,
-1.53514445509681));
#77164=CARTESIAN_POINT('Ctrl Pts',(-10.6645092784936,-1.67249224129637,
-5.43750723855698));
#77165=CARTESIAN_POINT('Ctrl Pts',(-10.5452433060764,3.66820304190325,-4.34833321054495));
#77166=CARTESIAN_POINT('Ctrl Pts',(-10.4259773336592,5.64155190838829,0.73253486709976));
#77167=CARTESIAN_POINT('Ctrl Pts',(-10.3067113612421,2.43605451516245,5.14094871261257));
#77168=CARTESIAN_POINT('Ctrl Pts',(-10.1874453888249,-3.00569843666994,
4.83006130130418));
#77169=CARTESIAN_POINT('Ctrl Pts',(-10.0681794164078,-5.68827264489775,
0.0852618546849905));
#77170=CARTESIAN_POINT('Ctrl Pts',(-9.94891344399059,-3.1491117721378,-4.73780648751502));
#77171=CARTESIAN_POINT('Ctrl Pts',(-9.82964747157344,2.28087878496807,-5.21165110448109));
#77172=CARTESIAN_POINT('Ctrl Pts',(-9.71038149915626,5.61706239742414,-0.901290901984511));
#77173=CARTESIAN_POINT('Ctrl Pts',(-9.5911155267391,3.79688069412207,4.23643862945746));
#77174=CARTESIAN_POINT('Ctrl Pts',(-9.47184955432194,-1.50877126641284,
5.48519138519372));
#77175=CARTESIAN_POINT('Ctrl Pts',(-9.35258358190478,-5.42939751829416,
1.6986341144865));
#77176=CARTESIAN_POINT('Ctrl Pts',(-9.2333176094876,-4.36593154046596,-3.6472396480792));
#77177=CARTESIAN_POINT('Ctrl Pts',(-9.11405163707046,0.705383446936543,
-5.64501102384613));
#77178=CARTESIAN_POINT('Ctrl Pts',(-8.99478566465327,5.12916873237924,-2.460760732241));
#77179=CARTESIAN_POINT('Ctrl Pts',(-8.87551969223612,4.84446657740473,2.98242499435692));
#77180=CARTESIAN_POINT('Ctrl Pts',(-8.75625371981895,0.112628594896119,
5.68779659149025));
#77181=CARTESIAN_POINT('Ctrl Pts',(-8.63698774740179,-4.72260047341405,
3.17187011636125));
#77182=CARTESIAN_POINT('Ctrl Pts',(-8.51772177498462,-5.22256467223263,
-2.25577780619104));
#77183=CARTESIAN_POINT('Ctrl Pts',(-8.39845580256746,-0.928305586732074,
-5.61266104483412));
#77184=CARTESIAN_POINT('Ctrl Pts',(-8.27918983015029,4.21812183715915,-3.81721933263432));
#77185=CARTESIAN_POINT('Ctrl Pts',(-8.15992385773312,5.49238698121822,1.48236315223396));
#77186=CARTESIAN_POINT('Ctrl Pts',(-8.04065788531597,1.72473666717901,5.42116211669091));
#77187=CARTESIAN_POINT('Ctrl Pts',(-7.9213919128988,-3.62619182684559,4.38342880647951));
#77188=CARTESIAN_POINT('Ctrl Pts',(-7.80212594048163,-5.64833946687671,
-0.678215698343313));
#77189=CARTESIAN_POINT('Ctrl Pts',(-7.68285996806448,-2.48540998688384,
-5.11727002059248));
#77190=CARTESIAN_POINT('Ctrl Pts',(-7.5635939956473,2.95908251396557,-4.85875971232364));
#77191=CARTESIAN_POINT('Ctrl Pts',(-7.44432802323015,5.68718887524218,-0.139992727946421));
#77192=CARTESIAN_POINT('Ctrl Pts',(-7.32506205081298,3.19455503717327,4.70728513912503));
#77193=CARTESIAN_POINT('Ctrl Pts',(-7.20579607839581,-2.23062460998521,
5.23335734647315));
#77194=CARTESIAN_POINT('Ctrl Pts',(-7.08653010597865,-5.60812976866394,
0.955298782780381));
#77195=CARTESIAN_POINT('Ctrl Pts',(-6.96726413356148,-3.83746960899577,
-4.19970740249727));
#77196=CARTESIAN_POINT('Ctrl Pts',(-6.84799816114433,1.45592072386326,-5.49945543780306));
#77197=CARTESIAN_POINT('Ctrl Pts',(-6.72873218872714,5.41280122438276,-1.75079929514405));
#77198=CARTESIAN_POINT('Ctrl Pts',(-6.60946621631,4.40082460355363,3.60506006542379));
#77199=CARTESIAN_POINT('Ctrl Pts',(-6.49020024389281,-0.651032250207427,
5.65153716043219));
#77200=CARTESIAN_POINT('Ctrl Pts',(-6.37093427147566,-5.10525285268721,
2.51000170850249));
#77201=CARTESIAN_POINT('Ctrl Pts',(-6.2516682990585,-4.87294037519916,-2.93567153583473));
#77202=CARTESIAN_POINT('Ctrl Pts',(-6.13240232664133,-0.167353620402568,
-5.68644951022114));
#77203=CARTESIAN_POINT('Ctrl Pts',(-6.01313635422417,4.69186083917187,-3.21716600945641));
#77204=CARTESIAN_POINT('Ctrl Pts',(-5.893870381807,5.24402887737063,2.20541977860435));
#77205=CARTESIAN_POINT('Ctrl Pts',(-5.77460440938983,0.982269865282724,
5.60346867380498));
#77206=CARTESIAN_POINT('Ctrl Pts',(-5.65533843697268,-4.18119575173463,
3.85763105444682));
#77207=CARTESIAN_POINT('Ctrl Pts',(-5.5360724645555,-5.50639659132553,-1.42944459339804));
#77208=CARTESIAN_POINT('Ctrl Pts',(-5.41680649213835,-1.776821395076,-5.40431503491021));
#77209=CARTESIAN_POINT('Ctrl Pts',(-5.29754051972118,3.58384485297817,-4.41811852900509));
#77210=CARTESIAN_POINT('Ctrl Pts',(-5.17827454730401,5.65460403049147,0.62383373177952));
#77211=CARTESIAN_POINT('Ctrl Pts',(-5.05900857488685,2.53453532784034,5.09311750684054));
#77212=CARTESIAN_POINT('Ctrl Pts',(-4.93974260246969,-2.91219260188876,
4.88700823777294));
#77213=CARTESIAN_POINT('Ctrl Pts',(-4.82047663005252,-5.68557851354222,
0.1947106389064));
#77214=CARTESIAN_POINT('Ctrl Pts',(-4.70121065763536,-3.239702509805,-4.67632793060106));
#77215=CARTESIAN_POINT('Ctrl Pts',(-4.5819446852182,2.18016389549758,-5.25457901789715));
#77216=CARTESIAN_POINT('Ctrl Pts',(-4.46267871280102,5.59867786815369,-1.00921820990431));
#77217=CARTESIAN_POINT('Ctrl Pts',(-4.34341274038386,3.87770320228423,4.16258731338466));
#77218=CARTESIAN_POINT('Ctrl Pts',(-4.2241467679667,-1.40293537371587,5.51321028110963));
#77219=CARTESIAN_POINT('Ctrl Pts',(-4.10488079554954,-5.39570374471416,
1.8028023646074));
#77220=CARTESIAN_POINT('Ctrl Pts',(-3.98561482313236,-4.43531018250885,
-3.56254668060498));
#77221=CARTESIAN_POINT('Ctrl Pts',(-3.86634885071521,0.596620772659216,
-5.65754000606162));
#77222=CARTESIAN_POINT('Ctrl Pts',(-3.74708287829804,5.08086426396513,-2.55901027698571));
#77223=CARTESIAN_POINT('Ctrl Pts',(-3.62781690588088,4.90096297439784,2.88864625562525));
#77224=CARTESIAN_POINT('Ctrl Pts',(-3.50855093346371,0.222063150189269,
5.68457590536746));
#77225=CARTESIAN_POINT('Ctrl Pts',(-3.38928496104655,-4.66068677297299,
3.26216401653732));
#77226=CARTESIAN_POINT('Ctrl Pts',(-3.27001898862938,-5.26500752383492,
-2.15485754529572));
#77227=CARTESIAN_POINT('Ctrl Pts',(-3.15075301621222,-1.03614319283671,
-5.59375746260904));
#77228=CARTESIAN_POINT('Ctrl Pts',(-3.03148704379506,4.14388251820106,-3.89768558787187));
#77229=CARTESIAN_POINT('Ctrl Pts',(-2.91222107137789,5.51989634943005,1.37639367846015));
#77230=CARTESIAN_POINT('Ctrl Pts',(-2.79295509896073,1.82874160232291,5.38696755313132));
#77231=CARTESIAN_POINT('Ctrl Pts',(-2.67368912654356,-3.54116604132071,
4.45239916610736));
#77232=CARTESIAN_POINT('Ctrl Pts',(-2.55442315412639,-5.66034501917984,
-0.569394002780302));
#77233=CARTESIAN_POINT('Ctrl Pts',(-2.43515718170923,-2.58342598938507,
-5.06849340770272));
#77234=CARTESIAN_POINT('Ctrl Pts',(-2.31589120929207,2.86503304210203,-4.91480426204542));
#77235=CARTESIAN_POINT('Ctrl Pts',(-2.1966252368749,5.68344170890555,-0.249410521087079));
#77236=CARTESIAN_POINT('Ctrl Pts',(-2.07735926445774,3.28455000970767,4.64493772835394));
#77237=CARTESIAN_POINT('Ctrl Pts',(-1.95809329204057,-2.12950131379783,
5.2753141537817));
#77238=CARTESIAN_POINT('Ctrl Pts',(-1.83882731962341,-5.58870757107013,
1.06304419081225));
#77239=CARTESIAN_POINT('Ctrl Pts',(-1.71956134720624,-3.9175777486514,-4.1250817991681));
#77240=CARTESIAN_POINT('Ctrl Pts',(-1.60029537478908,1.34982012202607,-5.52645464151563));
#77241=CARTESIAN_POINT('Ctrl Pts',(-1.48102940237192,5.37810666238975,-1.85463850777319));
#77242=CARTESIAN_POINT('Ctrl Pts',(-1.36176342995475,4.46938508421958,3.51970343005089));
#77243=CARTESIAN_POINT('Ctrl Pts',(-1.24249745753759,-0.542154052396278,
5.66301900491482));
#77244=CARTESIAN_POINT('Ctrl Pts',(-1.12323148512042,-5.05600522441769,
2.60778189985613));
#77245=CARTESIAN_POINT('Ctrl Pts',(-1.00396551270326,-4.92853178031331,
-2.84135350792509));
#77246=CARTESIAN_POINT('Ctrl Pts',(-0.884699540286091,-0.276752118554405,
-5.68217595041124));
#77247=CARTESIAN_POINT('Ctrl Pts',(-0.765433567868929,4.62908116130758,
-3.30685997111815));
#77248=CARTESIAN_POINT('Ctrl Pts',(-0.646167595451762,5.28549866915649,
2.10409578795772));
#77249=CARTESIAN_POINT('Ctrl Pts',(-0.526901623034598,1.08992058111838,
5.58352831043335));
#77250=CARTESIAN_POINT('Ctrl Pts',(-0.407635650617434,-4.10618559149057,
3.93737922415298));
#77251=CARTESIAN_POINT('Ctrl Pts',(-0.28836967820027,-5.53288500555307,
-1.32321531954648));
#77252=CARTESIAN_POINT('Ctrl Pts',(-0.169103705783104,-1.88049248148874,
-5.36912127760405));
#77253=CARTESIAN_POINT('Ctrl Pts',(-0.0498377333659409,3.4981593436186,
-4.4862675436503));
#77254=CARTESIAN_POINT('Ctrl Pts',(0.0694282390512246,5.66556190136835,
0.514901552065876));
#77255=CARTESIAN_POINT('Ctrl Pts',(0.188694211468389,2.6320774446008,5.0434000031903));
#77256=CARTESIAN_POINT('Ctrl Pts',(0.307960183885553,-2.81760820123537,
4.94214521143273));
#77257=CARTESIAN_POINT('Ctrl Pts',(0.42722615630272,-5.68077865918469,0.30408730967977));
#77258=CARTESIAN_POINT('Ctrl Pts',(0.546492128719881,-3.32909338433106,
-4.61311743888657));
#77259=CARTESIAN_POINT('Ctrl Pts',(0.665758101137048,2.07864155587013,-5.29556083420501));
#77260=CARTESIAN_POINT('Ctrl Pts',(0.785024073554211,5.57821980058984,-1.11677174161236));
#77261=CARTESIAN_POINT('Ctrl Pts',(0.904290045971376,3.9570895560061,4.08719433258361));
#77262=CARTESIAN_POINT('Ctrl Pts',(1.02355601838854,-1.29657988687734,5.53918729269027));
#77263=CARTESIAN_POINT('Ctrl Pts',(1.1428219908057,-5.36001160677062,1.906302924994));
#77264=CARTESIAN_POINT('Ctrl Pts',(1.26208796322287,-4.50304615359929,-3.47653428073288));
#77265=CARTESIAN_POINT('Ctrl Pts',(1.38135393564004,0.487637132638168,-5.66797364967663));
#77266=CARTESIAN_POINT('Ctrl Pts',(1.5006199080572,5.03067803581005,-2.65631206121851));
#77267=CARTESIAN_POINT('Ctrl Pts',(1.61988588047436,4.95564424027588,2.79379767169646));
#77268=CARTESIAN_POINT('Ctrl Pts',(1.73915185289153,0.331415461699871,5.67924986757076));
#77269=CARTESIAN_POINT('Ctrl Pts',(1.85841782530869,-4.59704693062398,3.35124973468065));
#77270=CARTESIAN_POINT('Ctrl Pts',(1.97768379772587,-5.30550041600524,-2.0531392067574));
#77271=CARTESIAN_POINT('Ctrl Pts',(2.09694977014301,-1.14359705073535,-5.57278216442251));
#77272=CARTESIAN_POINT('Ctrl Pts',(2.21621574256019,4.06810846206265,-3.97670828795007));
#77273=CARTESIAN_POINT('Ctrl Pts',(2.33548171497736,5.54536135704005,1.26991444058375));
#77274=CARTESIAN_POINT('Ctrl Pts',(2.45474768739451,1.93206924082099,5.35077786076283));
#77275=CARTESIAN_POINT('Ctrl Pts',(2.57401365981169,-3.45482874197723,4.5197205256702));
#77276=CARTESIAN_POINT('Ctrl Pts',(2.69327963222884,-5.67025419401183,-0.460361425238242));
#77277=CARTESIAN_POINT('Ctrl Pts',(2.81254560464602,-2.68048518871897,-5.0178396167688));
#77278=CARTESIAN_POINT('Ctrl Pts',(2.93181157706317,2.76992247048173,-4.9690285543632));
#77279=CARTESIAN_POINT('Ctrl Pts',(3.05107754948034,5.67758961095845,-0.358735942014323));
#77280=CARTESIAN_POINT('Ctrl Pts',(3.17034352189751,3.37332850928496,4.58087000852475));
#77281=CARTESIAN_POINT('Ctrl Pts',(3.28960949431467,-2.0275893309556,5.31531718447277));
#77282=CARTESIAN_POINT('Ctrl Pts',(3.40887546673183,-5.56721552780348,1.17039588752695));
#77283=CARTESIAN_POINT('Ctrl Pts',(3.52814143914899,-3.99623496584445,-4.04892842173314));
#77284=CARTESIAN_POINT('Ctrl Pts',(3.64740741156616,1.24321959792553,-5.55140705568331));
#77285=CARTESIAN_POINT('Ctrl Pts',(3.76667338398331,5.34142025332629,-1.95779083252319));
#77286=CARTESIAN_POINT('Ctrl Pts',(3.8859393564005,4.53629027387955,3.43304322979801));
#77287=CARTESIAN_POINT('Ctrl Pts',(4.00520532881765,-0.433075061252413,
5.67240348158324));
#77288=CARTESIAN_POINT('Ctrl Pts',(4.12447130123483,-5.00488504325426,2.70459626753531));
#77289=CARTESIAN_POINT('Ctrl Pts',(4.24373727365198,-4.98229784387044,-2.74598315026152));
#77290=CARTESIAN_POINT('Ctrl Pts',(4.36300324606915,-0.386048118200402,
-5.67579792777988));
#77291=CARTESIAN_POINT('Ctrl Pts',(4.48226921848632,4.56458704705725,-3.39532919705783));
#77292=CARTESIAN_POINT('Ctrl Pts',(4.60153519090347,5.32501091236597,2.001992519901));
#77293=CARTESIAN_POINT('Ctrl Pts',(4.72080116332065,1.1971676316396,5.56152001959095));
#77294=CARTESIAN_POINT('Ctrl Pts',(4.8400671357378,-4.02965465558056,4.01566913767982));
#77295=CARTESIAN_POINT('Ctrl Pts',(4.95933310815498,-5.55732424867229,-1.21649597684299));
#77296=CARTESIAN_POINT('Ctrl Pts',(5.07859908057214,-1.98346710468945,-5.33193900107375));
#77297=CARTESIAN_POINT('Ctrl Pts',(5.1978650529893,3.41117824849293,-4.55275501466583));
#77298=CARTESIAN_POINT('Ctrl Pts',(5.31713102540647,5.67442146263842,0.405778672313702));
#77299=CARTESIAN_POINT('Ctrl Pts',(5.43639699782363,2.72864473953703,4.99181461514278));
#77300=CARTESIAN_POINT('Ctrl Pts',(5.55566297024079,-2.7219802651905,4.99545180163613));
#77301=CARTESIAN_POINT('Ctrl Pts',(5.67492894265797,-5.67387485950943,0.413351358027617));
#77302=CARTESIAN_POINT('Ctrl Pts',(5.79419491507511,-3.41725128872073,-4.54819842314435));
#77303=CARTESIAN_POINT('Ctrl Pts',(5.91346088749229,1.97634936611633,-5.33458137529157));
#77304=CARTESIAN_POINT('Ctrl Pts',(6.03272685990945,5.55569577162621,-1.22391166335287));
#77305=CARTESIAN_POINT('Ctrl Pts',(6.15199283232661,4.03501035358811,4.01028760975979));
#77306=CARTESIAN_POINT('Ctrl Pts',(6.27125880474378,-1.18974419594258,5.56311279903411));
#77307=CARTESIAN_POINT('Ctrl Pts',(6.39052477716094,-5.32233432348004,2.00909746295764));
#77308=CARTESIAN_POINT('Ctrl Pts',(6.5097907495781,-4.56911436689826,-3.38923430419911));
#77309=CARTESIAN_POINT('Ctrl Pts',(6.62905672199528,0.378472890287174,-5.6763080904646));
#77310=CARTESIAN_POINT('Ctrl Pts',(6.74832269441244,4.97862863499266,-2.75263004804271));
#77311=CARTESIAN_POINT('Ctrl Pts',(6.86758866682961,5.00849012316842,2.69791437089479));
#77312=CARTESIAN_POINT('Ctrl Pts',(6.98685463924676,0.440645029472168,5.67182045066288));
#77313=CARTESIAN_POINT('Ctrl Pts',(7.10612061166394,-4.53170451615497,3.43909427681434));
#77314=CARTESIAN_POINT('Ctrl Pts',(7.2253865840811,-5.34402835170955,-1.95066046319719));
#77315=CARTESIAN_POINT('Ctrl Pts',(7.34465255649826,-1.25062736358769,-5.54974291873073));
#77316=CARTESIAN_POINT('Ctrl Pts',(7.46391852891543,3.99082773258522,-4.05425816585295));
#77317=CARTESIAN_POINT('Ctrl Pts',(7.58318450133259,5.5687725727736,1.16296487448275));
#77318=CARTESIAN_POINT('Ctrl Pts',(7.70245047374976,2.03468131402836,5.31260644287717));
#77319=CARTESIAN_POINT('Ctrl Pts',(7.82171644616693,-3.36721190488176,4.58536795188556));
#77320=CARTESIAN_POINT('Ctrl Pts',(7.94098241858407,-5.67806332138952,-0.351158347255461));
#77321=CARTESIAN_POINT('Ctrl Pts',(8.06024839100126,-2.77655163783317,-4.96532740803687));
#77322=CARTESIAN_POINT('Ctrl Pts',(8.17951436341841,2.67378602445897,-5.02141250665233));
#77323=CARTESIAN_POINT('Ctrl Pts',(8.29878033583558,5.66963474879634,-0.467928500731923));
#77324=CARTESIAN_POINT('Ctrl Pts',(8.41804630825273,3.46085765571055,4.51510570789498));
#77325=CARTESIAN_POINT('Ctrl Pts',(8.53731228066991,-1.924926405798,5.35335162293848));
#77326=CARTESIAN_POINT('Ctrl Pts',(8.65657825308706,-5.54366159870302,1.27731411392098));
#77327=CARTESIAN_POINT('Ctrl Pts',(8.77584422550424,-4.07341212892009,-3.97127547451985));
#77328=CARTESIAN_POINT('Ctrl Pts',(8.89511019792139,1.13615863235927,-5.57430343887665));
#77329=CARTESIAN_POINT('Ctrl Pts',(9.01437617033858,5.30275558444914,-2.0602180656789));
#77330=CARTESIAN_POINT('Ctrl Pts',(9.13364214275572,4.60151539338473,3.34511156032194));
#77331=CARTESIAN_POINT('Ctrl Pts',(9.25290811517291,-0.323835675503795,
5.6796871147826));
#77332=CARTESIAN_POINT('Ctrl Pts',(9.37217408759004,-4.95191124217634,2.8004089551642));
#77333=CARTESIAN_POINT('Ctrl Pts',(9.49144006000724,-5.03421865295653,-2.64959578441329));
#77334=CARTESIAN_POINT('Ctrl Pts',(9.61070603242439,-0.495201140240849,
-5.66731780450512));
#77335=CARTESIAN_POINT('Ctrl Pts',(9.72997200484155,4.4984023825987,-3.48254092162411));
#77336=CARTESIAN_POINT('Ctrl Pts',(9.84923797725872,5.36255097316036,1.89914778961855));
#77337=CARTESIAN_POINT('Ctrl Pts',(9.96850394967589,1.3039712965998,5.53745195231529));
#77338=CARTESIAN_POINT('Ctrl Pts',(10.087769922093,-3.95163128816538,4.09247179940786));
#77339=CARTESIAN_POINT('Ctrl Pts',(10.2070358945102,-5.579705269313,-1.10932609009118));
#77340=CARTESIAN_POINT('Ctrl Pts',(10.3263018669274,-2.08570712677686,-5.29278197622656));
#77341=CARTESIAN_POINT('Ctrl Pts',(10.4455678393445,3.32293378210522,-4.61755631761001));
#77342=CARTESIAN_POINT('Ctrl Pts',(10.5648338117617,5.68117943305569,0.296505507505705));
#77343=CARTESIAN_POINT('Ctrl Pts',(10.6840997841789,2.82420144777943,4.9383804479725));
#77344=CARTESIAN_POINT('Ctrl Pts',(10.803365756596,-2.62534421072083,5.04690826564054));
#77345=CARTESIAN_POINT('Ctrl Pts',(10.9226317290132,-5.66486967142244,0.522462316683581));
#77346=CARTESIAN_POINT('Ctrl Pts',(11.0418977014304,-3.50414357262422,-4.48159492691976));
#77347=CARTESIAN_POINT('Ctrl Pts',(11.1611636738475,1.87332521139011,-5.37162618942592));
#77348=CARTESIAN_POINT('Ctrl Pts',(11.2804296462647,5.53111412331024,-1.33059829455554));
#77349=CARTESIAN_POINT('Ctrl Pts',(11.3996956186819,4.11143673611723,3.93189562825137));
#77350=CARTESIAN_POINT('Ctrl Pts',(11.518961591099,-1.08246786880633,5.58497793903952));
#77351=CARTESIAN_POINT('Ctrl Pts',(11.6382275635162,-5.2826858490815,2.11114790729363));
#77352=CARTESIAN_POINT('Ctrl Pts',(11.7574935359334,-4.63349035324122,-3.30067908360948));
#77353=CARTESIAN_POINT('Ctrl Pts',(11.8767595083505,0.26916847590822,-5.68254024166424));
#77354=CARTESIAN_POINT('Ctrl Pts',(11.9960254807677,4.92473533864029,-2.84792856492294));
#77355=CARTESIAN_POINT('Ctrl Pts',(12.1152914531848,5.05948105096134,2.60103186476439));
#77356=CARTESIAN_POINT('Ctrl Pts',(12.234557425602,0.549711399010078,5.66229040621851));
#77357=CARTESIAN_POINT('Ctrl Pts',(12.3538233980192,-4.46468372992222,3.52566510864608));
#77358=CARTESIAN_POINT('Ctrl Pts',(12.4730893704364,-5.38057706165928,-1.84745926886156));
#77359=CARTESIAN_POINT('Ctrl Pts',(12.5923553428535,-1.35719449141834,-5.52464825839795));
#77360=CARTESIAN_POINT('Ctrl Pts',(12.7116213152707,3.91206895162486,-4.13030650004202));
#77361=CARTESIAN_POINT('Ctrl Pts',(12.8308872876878,5.59012132600284,1.05558459022699));
#77362=CARTESIAN_POINT('Ctrl Pts',(12.950153260105,2.13653981831823,5.27246743672232));
#77363=CARTESIAN_POINT('Ctrl Pts',(13.0694192325222,-3.27834797999339,4.64931713143229));
#77364=CARTESIAN_POINT('Ctrl Pts',(13.1886852049393,-5.68376950910777,-0.241825213517352));
#77365=CARTESIAN_POINT('Ctrl Pts',(13.3079511773565,-2.87158975735222,-4.91097623004087));
#77366=CARTESIAN_POINT('Ctrl Pts',(13.4272171497737,2.5766593093335,-5.07193671788022));
#77367=CARTESIAN_POINT('Ctrl Pts',(13.5464831221908,5.65958006859897,-0.576947756450346));
#77368=CARTESIAN_POINT('Ctrl Pts',(13.665749094608,3.54710503150264,4.44766918307164));
#77369=CARTESIAN_POINT('Ctrl Pts',(13.7850150670252,-1.82155056078556,5.3894033826629));
#77370=CARTESIAN_POINT('Ctrl Pts',(13.9042810394423,-5.51805450725224,1.38375927153138));
#77371=CARTESIAN_POINT('Ctrl Pts',(14.0235470118595,-4.14908065437921,-3.89215171723979));
#77372=CARTESIAN_POINT('Ctrl Pts',(14.1428129842766,1.02867687665546,-5.59513531114225));
#77373=CARTESIAN_POINT('Ctrl Pts',(14.2620789566938,5.26212697568769,-2.16188227207122));
#77374=CARTESIAN_POINT('Ctrl Pts',(14.3813449291109,4.66503628582042,3.25594098818379));
#77375=CARTESIAN_POINT('Ctrl Pts',(14.5006109015282,-0.214476353282968,
5.68486720693096));
#77376=CARTESIAN_POINT('Ctrl Pts',(14.6198768739453,-4.89710344067411,2.89518447735091));
#77377=CARTESIAN_POINT('Ctrl Pts',(14.7391428463625,-5.08427497806974,-2.55222710861131));
#77378=CARTESIAN_POINT('Ctrl Pts',(14.8584088187796,-0.60417075852906,-5.65673872130355));
#77379=CARTESIAN_POINT('Ctrl Pts',(14.9776747911968,4.43055168022577,-3.56846284489617));
#77380=CARTESIAN_POINT('Ctrl Pts',(15.0969407636139,5.3981049481225,1.79559968690459));
#77381=CARTESIAN_POINT('Ctrl Pts',(15.2162067360311,1.41029201996522,5.51133302250725));
#77382=CARTESIAN_POINT('Ctrl Pts',(15.3354727084483,-3.87214438614622,4.16775876453906));
#77383=CARTESIAN_POINT('Ctrl Pts',(15.4547386808655,-5.60001977839254,-1.00174535095946));
#77384=CARTESIAN_POINT('Ctrl Pts',(15.5740046532826,-2.18717468191774,-5.25166470534197));
#77385=CARTESIAN_POINT('Ctrl Pts',(15.6932706256998,3.23345862686471,-4.68064745253368));
#77386=CARTESIAN_POINT('Ctrl Pts',(15.8125365981169,5.68583330972381,0.187122528284859));
#77387=CARTESIAN_POINT('Ctrl Pts',(15.9318025705342,2.91871217874129,4.88311729167176));
#77388=CARTESIAN_POINT('Ctrl Pts',(16.0510685429512,-2.52773582816196,5.09649554591999));
#77389=CARTESIAN_POINT('Ctrl Pts',(16.1703345153685,-5.6537664301045,0.631379775079858));
#77390=CARTESIAN_POINT('Ctrl Pts',(16.2896004877856,-3.58973805442955,-4.41333161762595));
#77391=CARTESIAN_POINT('Ctrl Pts',(16.4088664602028,1.76960724793751,-5.4066815566115));
#77392=CARTESIAN_POINT('Ctrl Pts',(16.5281324326199,5.50448395975385,-1.43679212253169));
#77393=CARTESIAN_POINT('Ctrl Pts',(16.6473984050371,4.18634039815506,3.85204742148009));
#77394=CARTESIAN_POINT('Ctrl Pts',(16.7666643774543,-0.974790636558288,
5.6047746146865));
#77395=CARTESIAN_POINT('Ctrl Pts',(16.8859303498714,-5.24108086786879,2.21241646238138));
#77396=CARTESIAN_POINT('Ctrl Pts',(17.0051963222886,-4.69615027020021,-3.21090141646471));
#77397=CARTESIAN_POINT('Ctrl Pts',(17.1244622947058,0.159764371717757,-5.68666779512269));
#77398=CARTESIAN_POINT('Ctrl Pts',(17.2437282671229,4.86901810678927,-2.94217231689695));
#77399=CARTESIAN_POINT('Ctrl Pts',(17.3629942395401,5.1085981385457,2.50318603491707));
#77400=CARTESIAN_POINT('Ctrl Pts',(17.4822602119573,0.658574176260086,5.65066326380534));
#77401=CARTESIAN_POINT('Ctrl Pts',(17.6015261843744,-4.39600939388725,3.61093016761771));
#77402=CARTESIAN_POINT('Ctrl Pts',(17.7207921567916,-5.41513300959612,-1.74357384556518));
#77403=CARTESIAN_POINT('Ctrl Pts',(17.8400581292087,-1.46325896579829,-5.49750747753623));
#77404=CARTESIAN_POINT('Ctrl Pts',(17.9593241016259,3.83186128845189,-4.20482512509383));
#77405=CARTESIAN_POINT('Ctrl Pts',(18.0785900740431,5.6093997099579,0.947813357407833));
#77406=CARTESIAN_POINT('Ctrl Pts',(18.1978560464602,2.23760702915769,5.23037570826609));
#77407=CARTESIAN_POINT('Ctrl Pts',(18.3171220188774,-3.18826987914481,4.71154437995594));
#77408=CARTESIAN_POINT('Ctrl Pts',(18.4363879912946,-5.68737064381084,-0.132402516876524));
#77409=CARTESIAN_POINT('Ctrl Pts',(18.5556539637117,-2.96556434875542,-4.85480621239888));
#77410=CARTESIAN_POINT('Ctrl Pts',(18.6749199361289,2.47857829716258,-5.12058247579229));
#77411=CARTESIAN_POINT('Ctrl Pts',(18.7941859085461,5.64742929423926,-0.685753332565547));
#77412=CARTESIAN_POINT('Ctrl Pts',(18.9134518809632,3.63203869389911,4.3785854099898));
#77413=CARTESIAN_POINT('Ctrl Pts',(19.0327178533804,-1.7175000824166,5.42345911143944));
#77414=CARTESIAN_POINT('Ctrl Pts',(19.1519838257975,-5.49040373734829,1.48969193710258));
#77415=CARTESIAN_POINT('Ctrl Pts',(19.2712497982147,-4.22321251746525,-3.8115864543364));
#77416=CARTESIAN_POINT('Ctrl Pts',(19.3905157706319,0.920814137986261,-5.61389495714349));
#77417=CARTESIAN_POINT('Ctrl Pts',(19.5097817430491,5.21954947434026,-2.26274579912789));
#77418=CARTESIAN_POINT('Ctrl Pts',(19.6290477154662,4.72682942545333,3.16556453878679));
#77419=CARTESIAN_POINT('Ctrl Pts',(19.7483136878834,-0.105037597141629,
5.68794183951833));
#77420=CARTESIAN_POINT('Ctrl Pts',(19.8675796603006,-4.84048193748196,2.98888773283097));
#77421=CARTESIAN_POINT('Ctrl Pts',(19.9868456327177,-5.13244828024263,-2.45391318452596));
#77422=CARTESIAN_POINT('Ctrl Pts',(20.1061116051349,-0.712916614844916,
-5.644064596267));
#77423=CARTESIAN_POINT('Ctrl Pts',(20.225377577552,4.36106006926938,-3.65306314464733));
#77424=CARTESIAN_POINT('Ctrl Pts',(20.3446435499692,5.43165966940629,1.69138656205524));
#77425=CARTESIAN_POINT('Ctrl Pts',(20.4639095223863,1.51609042456612,5.48317290362938));
#77426=CARTESIAN_POINT('Ctrl Pts',(20.5831754948035,-3.79122338846171,4.24150214963253));
#77427=CARTESIAN_POINT('Ctrl Pts',(20.7024414672207,-5.6182602521859,-0.893793603279791));
#77428=CARTESIAN_POINT('Ctrl Pts',(20.8217074396379,-2.28783219037207,-5.20860241670007));
#77429=CARTESIAN_POINT('Ctrl Pts',(20.940973412055,3.14278592098079,-4.74200505286967));
#77430=CARTESIAN_POINT('Ctrl Pts',(21.0602393844722,5.68838136902297,0.0776702459646251));
#77431=CARTESIAN_POINT('Ctrl Pts',(21.1795053568894,3.01214192922678,4.826045613621));
#77432=CARTESIAN_POINT('Ctrl Pts',(21.2987713293065,-2.42919126796274,5.14419527722365));
#77433=CARTESIAN_POINT('Ctrl Pts',(21.4180373017237,-5.64056924777562,0.740063394314221));
#77434=CARTESIAN_POINT('Ctrl Pts',(21.5373032741408,-3.67400303318194,-4.34343377740774));
#77435=CARTESIAN_POINT('Ctrl Pts',(21.656569246558,1.66523388896478,-5.43973449366784));
#77436=CARTESIAN_POINT('Ctrl Pts',(21.7758352189752,5.47581514376105,-1.54245381710865));
#77437=CARTESIAN_POINT('Ctrl Pts',(21.8951011913923,4.25969359822163,3.77077256219813));
#77438=CARTESIAN_POINT('Ctrl Pts',(22.0143671638095,-0.866752378767923,
5.62249549403613));
#77439=CARTESIAN_POINT('Ctrl Pts',(22.1336331362266,-5.1975347887514,2.31286562218276));
#77440=CARTESIAN_POINT('Ctrl Pts',(22.2528991086438,-4.7570709109148,-3.11993455301305));
#77441=CARTESIAN_POINT('Ctrl Pts',(22.372165081061,0.0503010968532085,-5.68868922215055));
#77442=CARTESIAN_POINT('Ctrl Pts',(22.4914310534782,4.81149757499245,-3.03532639964759));
#77443=CARTESIAN_POINT('Ctrl Pts',(22.6106970258953,5.15582319481218,2.40441311974323));
#77444=CARTESIAN_POINT('Ctrl Pts',(22.7299629983125,0.767193042571622,5.63694332967666));
#77445=CARTESIAN_POINT('Ctrl Pts',(22.8492289707296,-4.32570694242367,3.69485787477996));
#77446=CARTESIAN_POINT('Ctrl Pts',(22.9684949431469,-5.44768339730547,-1.63904266853516));
#77447=CARTESIAN_POINT('Ctrl Pts',(23.0877609155639,-1.56878150446242,-5.46833062806312));
#77448=CARTESIAN_POINT('Ctrl Pts',(23.2070268879812,3.75023444894761,-4.27778644213131));
#77449=CARTESIAN_POINT('Ctrl Pts',(23.3262928603983,5.62660058465537,0.839691090409063));
#77450=CARTESIAN_POINT('Ctrl Pts',(23.4455588328155,2.3378455150786,5.18634684669117));
#77451=CARTESIAN_POINT('Ctrl Pts',(23.5648248052326,-3.09701096385403,4.77202665083964));
#77452=CARTESIAN_POINT('Ctrl Pts',(23.6840907776498,-5.68886539177463,-0.0229307833566997));
#77453=CARTESIAN_POINT('Ctrl Pts',(23.8033567500669,-3.05844060741237,-4.79683815835885));
#77454=CARTESIAN_POINT('Ctrl Pts',(23.9226227224842,2.37957931343959,-5.16733176384159));
#77455=CARTESIAN_POINT('Ctrl Pts',(24.0418886949013,5.63318692590381,-0.794304931611839));
#77456=CARTESIAN_POINT('Ctrl Pts',(24.1611546673185,3.71562718668736,4.30787997466344));
#77457=CARTESIAN_POINT('Ctrl Pts',(24.2804206397356,-1.61281350704876,5.45550619631551));
#77458=CARTESIAN_POINT('Ctrl Pts',(24.3996866121528,-5.46071952978924,1.59507287718616));
#77459=CARTESIAN_POINT('Ctrl Pts',(24.51895258457,-4.2957802625431,-3.72960952413273));
#77460=CARTESIAN_POINT('Ctrl Pts',(24.6382185569871,0.812610364626208,-5.63057542901771));
#77461=CARTESIAN_POINT('Ctrl Pts',(24.7574845294043,5.17503884950108,-2.36277129081743));
#77462=CARTESIAN_POINT('Ctrl Pts',(24.8767505018215,4.78687192644435,3.07401568414598));
#77463=CARTESIAN_POINT('Ctrl Pts',(24.9960164742386,0.00444006094848726,
5.68890987381718));
#77464=CARTESIAN_POINT('Ctrl Pts',(25.1152824466558,-4.78206770306065,3.08148401746638));
#77465=CARTESIAN_POINT('Ctrl Pts',(25.2345484190729,-5.17872071790823,-2.35469042391236));
#77466=CARTESIAN_POINT('Ctrl Pts',(25.3538143914901,-0.821398433840538,
-5.62930012341145));
#77467=CARTESIAN_POINT('Ctrl Pts',(25.4730803639073,4.28995328679094,-3.73631048812972));
#77468=CARTESIAN_POINT('Ctrl Pts',(25.5923463363244,5.46320270961362,1.58654701166618));
#77469=CARTESIAN_POINT('Ctrl Pts',(25.7116123087416,1.62132732667911,5.45298202512345));
#77470=CARTESIAN_POINT('Ctrl Pts',(25.8308782811588,-3.70889826518536,4.31367464293049));
#77471=CARTESIAN_POINT('Ctrl Pts',(25.950144253576,-5.63441993511243,-0.785510828292191));
#77472=CARTESIAN_POINT('Ctrl Pts',(26.0694102259931,-2.38764237240975,-5.16361105894212));
#77473=CARTESIAN_POINT('Ctrl Pts',(26.1886761984103,3.05094924619048,-4.80160639408587));
#77474=CARTESIAN_POINT('Ctrl Pts',(26.3079421708274,5.68882266724869,-0.031810802473794));
#77475=CARTESIAN_POINT('Ctrl Pts',(26.4272081432446,3.1044560963937,4.76718655100886));
#77476=CARTESIAN_POINT('Ctrl Pts',(26.5464741156617,-2.32974702729697,5.18998979337701));
#77477=CARTESIAN_POINT('Ctrl Pts',(26.6657400880789,-5.62528301217263,0.848472922089174));
#77478=CARTESIAN_POINT('Ctrl Pts',(26.7850060604961,-3.75690730032363,-4.27192729377863));
#77479=CARTESIAN_POINT('Ctrl Pts',(26.9042720329132,1.56024379041213,-5.47077275903843));
#77480=CARTESIAN_POINT('Ctrl Pts',(27.0235380053304,5.44511829317601,-1.6475442451954));
#77481=CARTESIAN_POINT('Ctrl Pts',(27.1428039777475,4.33146916906887,3.68810115153607));
#77482=CARTESIAN_POINT('Ctrl Pts',(27.2620699501648,-0.75839310871523,5.63813401394555));
#77483=CARTESIAN_POINT('Ctrl Pts',(27.3813359225819,-5.1520637395484,2.41245818413233));
#77484=CARTESIAN_POINT('Ctrl Pts',(27.5006018949991,-4.81622971268621,-3.02781218393652));
#77485=CARTESIAN_POINT('Ctrl Pts',(27.6198678674162,-0.0591808076330519,
-5.68860377408766));
#77486=CARTESIAN_POINT('Ctrl Pts',(27.7391338398334,4.75219504667706,-3.12735631242981));
#77487=CARTESIAN_POINT('Ctrl Pts',(27.8583998122506,5.20113872938789,2.30474970099082));
#77488=CARTESIAN_POINT('Ctrl Pts',(27.9776657846677,0.875527769629323,5.62113568517647));
#77489=CARTESIAN_POINT('Ctrl Pts',(28.0969317570849,-4.25380241289778,3.77741714648801));
#77490=CARTESIAN_POINT('Ctrl Pts',(28.2161977295021,-5.4782161693561,-1.53390445216165));
#77491=CARTESIAN_POINT('Ctrl Pts',(28.3354637019192,-1.67372302585793,-5.4371285159787));
#77492=CARTESIAN_POINT('Ctrl Pts',(28.4547296743364,3.66721866460272,-4.34916342904541));
#77493=CARTESIAN_POINT('Ctrl Pts',(28.5739956467536,5.64171757954254,0.731257833624528));
#77494=CARTESIAN_POINT('Ctrl Pts',(28.6932616191707,2.43721815154126,5.14039715862049));
#77495=CARTESIAN_POINT('Ctrl Pts',(28.8125275915879,-3.00460503296775,4.83074154374061));
#77496=CARTESIAN_POINT('Ctrl Pts',(28.9317935640051,-5.68825319940117,0.0865494428570666));
#77497=CARTESIAN_POINT('Ctrl Pts',(29.0510595364222,-3.15018413547354,-4.73709353709283));
#77498=CARTESIAN_POINT('Ctrl Pts',(29.1703255088394,2.27969902363949,-5.21216726786216));
#77499=CARTESIAN_POINT('Ctrl Pts',(29.2895914812565,5.61685823842664,-0.902562350187162));
#77500=CARTESIAN_POINT('Ctrl Pts',(29.4088574536737,3.79783955185462,4.23557906370835));
#77501=CARTESIAN_POINT('Ctrl Pts',(29.5281234260908,-1.50752960662557,5.48553276826453));
#77502=CARTESIAN_POINT('Ctrl Pts',(29.6473893985081,-5.42901287848164,1.69986306267211));
#77503=CARTESIAN_POINT('Ctrl Pts',(29.7666553709251,-4.36675701326764,-3.64625128777951));
#77504=CARTESIAN_POINT('Ctrl Pts',(29.8859213433424,0.704105631155751,-5.6451705489499));
#77505=CARTESIAN_POINT('Ctrl Pts',(30.0051873157595,5.12861158622029,-2.46192170148515));
#77506=CARTESIAN_POINT('Ctrl Pts',(30.1244532881767,4.84514155132446,2.98132833049047));
#77507=CARTESIAN_POINT('Ctrl Pts',(30.2437192605939,0.113916074608287,5.68777095130442));
#77508=CARTESIAN_POINT('Ctrl Pts',(30.362985233011,-4.72188237183086,3.17293903709944));
#77509=CARTESIAN_POINT('Ctrl Pts',(30.4822512054282,-5.22307515350755,-2.25459557512384));
#77510=CARTESIAN_POINT('Ctrl Pts',(30.6015171778453,-0.929576037957939,
-5.61245077093875));
#77511=CARTESIAN_POINT('Ctrl Pts',(30.7207831502625,4.21725766805032,-3.81817404367943));
#77512=CARTESIAN_POINT('Ctrl Pts',(30.8400491226797,5.49272238639658,1.48111986433704));
#77513=CARTESIAN_POINT('Ctrl Pts',(30.9593150950968,1.7259637505406,5.42077156854781));
#77514=CARTESIAN_POINT('Ctrl Pts',(31.078581067514,-3.62519950642571,4.38424951447422));
#77515=CARTESIAN_POINT('Ctrl Pts',(31.1978470399311,-5.64849284223719,-0.676937129836315));
#77516=CARTESIAN_POINT('Ctrl Pts',(31.3171130123484,-2.48656826211884,-5.11670729516354));
#77517=CARTESIAN_POINT('Ctrl Pts',(31.4363789847655,2.95798261532084,-4.85942940210229));
#77518=CARTESIAN_POINT('Ctrl Pts',(31.5556449571827,5.68715704096057,-0.141280069395615));
#77519=CARTESIAN_POINT('Ctrl Pts',(31.6749109295998,3.19562049057018,4.70656190300357));
#77520=CARTESIAN_POINT('Ctrl Pts',(31.7941769020171,-2.22943993654606,5.23386213382527));
#77521=CARTESIAN_POINT('Ctrl Pts',(31.9134428744341,-5.60791338473815,0.956568207620598));
#77522=CARTESIAN_POINT('Ctrl Pts',(32.0327088468514,-3.83842015125344,-4.19883865003266));
#77523=CARTESIAN_POINT('Ctrl Pts',(32.1519748192685,1.45467583663671,-5.49978485732504));
#77524=CARTESIAN_POINT('Ctrl Pts',(32.2712407916857,5.41240477694961,-1.75202448527666));
#77525=CARTESIAN_POINT('Ctrl Pts',(32.3905067641028,4.40164052774331,3.60406380785415));
#77526=CARTESIAN_POINT('Ctrl Pts',(32.50977273652,-0.649752958570897,5.65168438249916));
#77527=CARTESIAN_POINT('Ctrl Pts',(32.6290387089371,-5.10468456101445,2.51115726291617));
#77528=CARTESIAN_POINT('Ctrl Pts',(32.7483046813543,-4.87360476533446,-2.93456842787243));
#77529=CARTESIAN_POINT('Ctrl Pts',(32.8675706537715,-0.168640793789048,
-5.6864114825808));
#77530=CARTESIAN_POINT('Ctrl Pts',(32.9868366261887,4.69113248525386,-3.21822797084853));
#77531=CARTESIAN_POINT('Ctrl Pts',(33.1061025986057,5.24452795911491,2.20423269021639));
#77532=CARTESIAN_POINT('Ctrl Pts',(33.2253685710231,0.983538234352283,5.60324618485782));
#77533=CARTESIAN_POINT('Ctrl Pts',(33.3446345434401,-4.18032243602443,3.85857740591355));
#77534=CARTESIAN_POINT('Ctrl Pts',(33.4639005158574,-5.50672001756556,-1.42819813565887));
#77535=CARTESIAN_POINT('Ctrl Pts',(33.5831664882745,-1.77804466361857,-5.4039126973642));
#77536=CARTESIAN_POINT('Ctrl Pts',(33.7024324606916,3.58284468132043,-4.41892965050241));
#77537=CARTESIAN_POINT('Ctrl Pts',(33.8216984331088,5.65474509585696,0.622553746626874));
#77538=CARTESIAN_POINT('Ctrl Pts',(33.940964405526,2.53568813468345,5.09254366207905));
#77539=CARTESIAN_POINT('Ctrl Pts',(34.0602303779431,-2.91108631014372,4.88766731288531));
#77540=CARTESIAN_POINT('Ctrl Pts',(34.1794963503603,-5.68553429342391,0.195997614434357));
#77541=CARTESIAN_POINT('Ctrl Pts',(34.2987623227774,-3.24076095460869,-4.67559447574684));
#77542=CARTESIAN_POINT('Ctrl Pts',(34.4180282951946,2.17897441963776,-5.25507238248037));
#77543=CARTESIAN_POINT('Ctrl Pts',(34.5372942676118,5.59844927933938,-1.01048549384319));
#77544=CARTESIAN_POINT('Ctrl Pts',(34.656560240029,3.87864534104596,4.1617094546457));
#77545=CARTESIAN_POINT('Ctrl Pts',(34.7758262124461,-1.40168737430279,5.51352770657897));
#77546=CARTESIAN_POINT('Ctrl Pts',(34.8950921848633,-5.39529552639648,1.80402368324702));
#77547=CARTESIAN_POINT('Ctrl Pts',(35.0143581572804,-4.43611648248496,-3.56154261801842));
#77548=CARTESIAN_POINT('Ctrl Pts',(35.1336241296976,0.595340123519527,-5.657674911447));
#77549=CARTESIAN_POINT('Ctrl Pts',(35.2528901021148,5.08028487958908,-2.5601603095978));
#77550=CARTESIAN_POINT('Ctrl Pts',(35.3721560745319,4.90161671886864,2.88753680575381));
#77551=CARTESIAN_POINT('Ctrl Pts',(35.4914220469491,0.223349898755441,5.68452549370444));
#77552=CARTESIAN_POINT('Ctrl Pts',(35.6106880193663,-4.65994823546759,3.26321892042295));
#77553=CARTESIAN_POINT('Ctrl Pts',(35.7299539917834,-5.26549515735449,-2.15366570982432));
#77554=CARTESIAN_POINT('Ctrl Pts',(35.8492199642006,-1.03740936702376,-5.59352277860006));
#77555=CARTESIAN_POINT('Ctrl Pts',(35.9684859366177,4.14300014570849,-3.89862349329523));
#77556=CARTESIAN_POINT('Ctrl Pts',(36.087751909035,5.5202077497737,1.3751441684951));
#77557=CARTESIAN_POINT('Ctrl Pts',(36.2070178814521,1.82996097509064,5.38655345925063));
#77558=CARTESIAN_POINT('Ctrl Pts',(36.3262838538692,-3.54015817240135,4.45320063395262));
#77559=CARTESIAN_POINT('Ctrl Pts',(36.4455498262865,-5.66047364493052,-0.568112734597499));
#77560=CARTESIAN_POINT('Ctrl Pts',(36.5648157987035,-2.58457344247884,-5.06790846806574));
#77561=CARTESIAN_POINT('Ctrl Pts',(36.6840817711207,2.86392088017567,-4.91545271593295));
#77562=CARTESIAN_POINT('Ctrl Pts',(36.8033477435379,5.68338430840045,-0.250696908077834));
#77563=CARTESIAN_POINT('Ctrl Pts',(36.9226137159551,3.28560286481452,4.64419392618976));
#77564=CARTESIAN_POINT('Ctrl Pts',(37.0418796883722,-2.12831002677038,5.27579642311569));
#77565=CARTESIAN_POINT('Ctrl Pts',(37.1611456607894,-5.58846132630211,1.06430850767035));
#77566=CARTESIAN_POINT('Ctrl Pts',(37.2804116332066,-3.9185217903309,-4.12419356911063));
#77567=CARTESIAN_POINT('Ctrl Pts',(37.3996776056237,1.34858886709791,-5.5267626006799));
#77568=CARTESIAN_POINT('Ctrl Pts',(37.5189435780409,5.37764921580746,-1.85585098494954));
#77569=CARTESIAN_POINT('Ctrl Pts',(37.6382095504581,4.47025290163574,3.51868243053033));
#77570=CARTESIAN_POINT('Ctrl Pts',(37.7574755228752,-0.541007429195424,
5.66315910227798));
#77571=CARTESIAN_POINT('Ctrl Pts',(37.8767414952924,-5.0551578814661,2.60889302618054));
#77572=CARTESIAN_POINT('Ctrl Pts',(37.9960074677095,-4.92966283975873,-2.84017461837445));
#77573=CARTESIAN_POINT('Ctrl Pts',(38.1152734401267,-0.277111040578141,
-5.68223314890805));
#77574=CARTESIAN_POINT('Ctrl Pts',(38.2345394125439,4.62656819708096,-3.30768024346582));
#77575=CARTESIAN_POINT('Ctrl Pts',(38.3538053849611,5.28935206274146,2.1024708769518));
#77576=CARTESIAN_POINT('Ctrl Pts',(38.4730713573782,1.08454695527874,5.58406416185194));
#77577=CARTESIAN_POINT('Ctrl Pts',(38.5724596677259,-3.22824135538267,4.21160970579805));
#77578=CARTESIAN_POINT('Ctrl Pts',(38.6519703160039,-4.83334745226005,1.30553258485445));
#77579=CARTESIAN_POINT('Ctrl Pts',(38.691725640143,-4.86505302969868,-0.338699302841263));
#77580=CARTESIAN_POINT('Ctrl Pts',(38.7116033022125,-4.67889930883017,-1.11786102211901));
#77581=CARTESIAN_POINT('Ctrl Pts',(-17.6184,-2.11639460593172,4.47917290043409));
#77582=CARTESIAN_POINT('Ctrl Pts',(-17.5985223379305,-2.8622965430514,4.1267366646904));
#77583=CARTESIAN_POINT('Ctrl Pts',(-17.5587670137914,-4.16282509234333,
3.04193699287371));
#77584=CARTESIAN_POINT('Ctrl Pts',(-17.4792563655133,-5.46341108425688,
-0.119881008423284));
#77585=CARTESIAN_POINT('Ctrl Pts',(-17.3798680551657,-3.78742768517455,
-4.46895156442932));
#77586=CARTESIAN_POINT('Ctrl Pts',(-17.2606020827485,1.71866712847336,-5.60395676842087));
#77587=CARTESIAN_POINT('Ctrl Pts',(-17.1413361103314,5.63810416435217,-1.58589123022531));
#77588=CARTESIAN_POINT('Ctrl Pts',(-17.0220701379142,4.38650144303843,3.88351482617148));
#77589=CARTESIAN_POINT('Ctrl Pts',(-16.902804165497,-0.894268453325975,
5.79026664325592));
#77590=CARTESIAN_POINT('Ctrl Pts',(-16.7835381930799,-5.35283428647187,
2.38042187278717));
#77591=CARTESIAN_POINT('Ctrl Pts',(-16.6642722206627,-4.89826604426309,
-3.21395979162865));
#77592=CARTESIAN_POINT('Ctrl Pts',(-16.5450062482455,0.0531800766195173,
-5.8583240260201));
#77593=CARTESIAN_POINT('Ctrl Pts',(-16.4257402758284,4.95562086810942,-3.12466912572249));
#77594=CARTESIAN_POINT('Ctrl Pts',(-16.3064743034112,5.30898655851339,2.47728284467523));
#77595=CARTESIAN_POINT('Ctrl Pts',(-16.187208330994,0.78874335884052,5.80518222363476));
#77596=CARTESIAN_POINT('Ctrl Pts',(-16.0679423585769,-4.45552520423068,
3.80399931897383));
#77597=CARTESIAN_POINT('Ctrl Pts',(-15.9486763861597,-5.60971370183634,
-1.68917479670012));
#77598=CARTESIAN_POINT('Ctrl Pts',(-15.8294104137426,-1.61427529499575,
-5.63172318529513));
#77599=CARTESIAN_POINT('Ctrl Pts',(-15.7101444413254,3.8630356967424,-4.40444407974865));
#77600=CARTESIAN_POINT('Ctrl Pts',(-15.5908784689082,5.79414938910801,0.866035857838147));
#77601=CARTESIAN_POINT('Ctrl Pts',(-15.471612496491,2.40633389206521,5.34151104403555));
#77602=CARTESIAN_POINT('Ctrl Pts',(-15.3523465240739,-3.19045356878321,
4.9135716920102));
#77603=CARTESIAN_POINT('Ctrl Pts',(-15.2330805516567,-5.85846060296283,
-0.0249404831624147));
#77604=CARTESIAN_POINT('Ctrl Pts',(-15.1138145792395,-3.14850281774238,
-4.94055788474845));
#77605=CARTESIAN_POINT('Ctrl Pts',(-14.9945486068224,2.45172555749452,-5.32082923295528));
#77606=CARTESIAN_POINT('Ctrl Pts',(-14.8752826344052,5.80131267523169,-0.816672186855044));
#77607=CARTESIAN_POINT('Ctrl Pts',(-14.7560166619881,3.82539591211262,4.43717570612341));
#77608=CARTESIAN_POINT('Ctrl Pts',(-14.6367506895709,-1.66216756865306,
5.61777367608827));
#77609=CARTESIAN_POINT('Ctrl Pts',(-14.5174847171538,-5.62389021715314,
1.64135339515628));
#77610=CARTESIAN_POINT('Ctrl Pts',(-14.3982187447366,-4.42297972703404,
-3.84180067960166));
#77611=CARTESIAN_POINT('Ctrl Pts',(-14.2789527723194,0.838149011166279,
-5.79824873215111));
#77612=CARTESIAN_POINT('Ctrl Pts',(-14.1596867999022,5.32987157590943,-2.43200557458098));
#77613=CARTESIAN_POINT('Ctrl Pts',(-14.0404208274851,4.92886498975685,3.16677628523976));
#77614=CARTESIAN_POINT('Ctrl Pts',(-13.9211548550679,0.00324630575561585,
5.85851274551346));
#77615=CARTESIAN_POINT('Ctrl Pts',(-13.8018888826508,-4.92535243045046,
3.17223668166147));
#77616=CARTESIAN_POINT('Ctrl Pts',(-13.6826229102336,-5.33256353665323,
-2.42609733023661));
#77617=CARTESIAN_POINT('Ctrl Pts',(-13.5633569378164,-0.844574319486159,
-5.7973163055935));
#77618=CARTESIAN_POINT('Ctrl Pts',(-13.4440909653992,4.41871939308572,-3.84670002125304));
#77619=CARTESIAN_POINT('Ctrl Pts',(-13.3248249929821,5.62570576802085,1.63511979375657));
#77620=CARTESIAN_POINT('Ctrl Pts',(-13.2055590205649,1.66839236374145,5.61592815560291));
#77621=CARTESIAN_POINT('Ctrl Pts',(-13.0862930481478,-3.82047613265049,
4.44141241590395));
#77622=CARTESIAN_POINT('Ctrl Pts',(-12.9670270757306,-5.80221417075813,
-0.810242460589229));
#77623=CARTESIAN_POINT('Ctrl Pts',(-12.8477611033134,-2.45762079435045,
-5.31810888939538));
#77624=CARTESIAN_POINT('Ctrl Pts',(-12.7284951308963,3.14302560882944,-4.94404410887827));
#77625=CARTESIAN_POINT('Ctrl Pts',(-12.6092291584791,5.85842931943376,-0.0314330636285068));
#77626=CARTESIAN_POINT('Ctrl Pts',(-12.4899631860619,3.19589708946511,4.91003298581984));
#77627=CARTESIAN_POINT('Ctrl Pts',(-12.3706972136448,-2.40041293019083,
5.34417438832823));
#77628=CARTESIAN_POINT('Ctrl Pts',(-12.2514312412276,-5.79318574463262,
0.872456908091129));
#77629=CARTESIAN_POINT('Ctrl Pts',(-12.1321652688104,-3.86791508228008,
-4.4001607975801));
#77630=CARTESIAN_POINT('Ctrl Pts',(-12.0128992963933,1.60803416675023,-5.63350763262592));
#77631=CARTESIAN_POINT('Ctrl Pts',(-11.8936333239761,5.60783609582425,-1.69539271281352));
#77632=CARTESIAN_POINT('Ctrl Pts',(-11.7743673515589,4.45974229309636,3.79906314865365));
#77633=CARTESIAN_POINT('Ctrl Pts',(-11.6551013791418,-0.78231715400237,
5.80604529769138));
#77634=CARTESIAN_POINT('Ctrl Pts',(-11.5358354067246,-5.3062230978268,2.48317912450548));
#77635=CARTESIAN_POINT('Ctrl Pts',(-11.4165694343075,-4.95910878169189,
-3.11920217678126));
#77636=CARTESIAN_POINT('Ctrl Pts',(-11.2973034618903,-0.0596190939189362,
-5.85821028061735));
#77637=CARTESIAN_POINT('Ctrl Pts',(-11.1780374894731,4.89459988227734,-3.21948351769366));
#77638=CARTESIAN_POINT('Ctrl Pts',(-11.0587715170559,5.35566153142266,2.37467296466905));
#77639=CARTESIAN_POINT('Ctrl Pts',(-10.9395055446388,0.900319300804774,
5.78892108124553));
#77640=CARTESIAN_POINT('Ctrl Pts',(-10.8202395722216,-4.38150034582086,
3.88904060763863));
#77641=CARTESIAN_POINT('Ctrl Pts',(-10.7009735998045,-5.64117909108611,
-1.58091131648284));
#77642=CARTESIAN_POINT('Ctrl Pts',(-10.5817076273873,-1.72235381642172,
-5.59961422415402));
#77643=CARTESIAN_POINT('Ctrl Pts',(-10.4624416549701,3.77756222279128,-4.47796893482199));
#77644=CARTESIAN_POINT('Ctrl Pts',(-10.343175682553,5.80974202452692,0.754373738101006));
#77645=CARTESIAN_POINT('Ctrl Pts',(-10.2239097101358,2.50867997327711,5.29421447619652));
#77646=CARTESIAN_POINT('Ctrl Pts',(-10.1046437377186,-3.09530654049515,
4.97405865955143));
#77647=CARTESIAN_POINT('Ctrl Pts',(-9.98537776530148,-5.8578556341726,0.0878037441284453));
#77648=CARTESIAN_POINT('Ctrl Pts',(-9.86611179288431,-3.24299542034126,
-4.87905347705231));
#77649=CARTESIAN_POINT('Ctrl Pts',(-9.74684582046715,2.34887802949731,-5.36702470003963));
#77650=CARTESIAN_POINT('Ctrl Pts',(-9.62757984805,5.78452241415752,-0.928160852654129));
#77651=CARTESIAN_POINT('Ctrl Pts',(-9.50831387563281,3.91007610830566,4.36273846976275));
#77652=CARTESIAN_POINT('Ctrl Pts',(-9.38904790321567,-1.55375187080085,
5.64871996582177));
#77653=CARTESIAN_POINT('Ctrl Pts',(-9.26978193079848,-5.59126273091542,
1.74927505046137));
#77654=CARTESIAN_POINT('Ctrl Pts',(-9.15051595838133,-4.49609191916458,
-3.75597385277289));
#77655=CARTESIAN_POINT('Ctrl Pts',(-9.03124998596417,0.726412859727577,
-5.81330426569202));
#77656=CARTESIAN_POINT('Ctrl Pts',(-8.911984013547,5.28208330248386,-2.53412275036385));
#77657=CARTESIAN_POINT('Ctrl Pts',(-8.79271804112984,4.98889339639251,3.07133925311447));
#77658=CARTESIAN_POINT('Ctrl Pts',(-8.67345206871268,0.115986361830236,
5.85736538830899));
#77659=CARTESIAN_POINT('Ctrl Pts',(-8.5541860962955,-4.86339413001757,3.26643225314731));
#77660=CARTESIAN_POINT('Ctrl Pts',(-8.43492012387835,-5.37826363114107,
-2.32302872178451));
#77661=CARTESIAN_POINT('Ctrl Pts',(-8.31565415146118,-0.955980919154609,
-5.7799898451903));
#77662=CARTESIAN_POINT('Ctrl Pts',(-8.19638817904402,4.34387560371134,-3.93102109734504));
#77663=CARTESIAN_POINT('Ctrl Pts',(-8.07712220662684,5.65613008227446,1.52655645839927));
#77664=CARTESIAN_POINT('Ctrl Pts',(-7.95785623420969,1.77615579175165,5.58278180943137));
#77665=CARTESIAN_POINT('Ctrl Pts',(-7.83859026179252,-3.73429853833258,
4.51411082660778));
#77666=CARTESIAN_POINT('Ctrl Pts',(-7.71932428937535,-5.81673193872685,
-0.698435166128912));
#77667=CARTESIAN_POINT('Ctrl Pts',(-7.6000583169582,-2.55950686680862,-5.26982985750491));
#77668=CARTESIAN_POINT('Ctrl Pts',(-7.48079234454101,3.04730086944123,-5.00361264881616));
#77669=CARTESIAN_POINT('Ctrl Pts',(-7.36152637212387,5.85673955437486,-0.144166294644587));
#77670=CARTESIAN_POINT('Ctrl Pts',(-7.24226039970669,3.28979347358892,4.84762220366051));
#77671=CARTESIAN_POINT('Ctrl Pts',(-7.12299442728954,-2.29712563989832,
5.3893780645648));
#77672=CARTESIAN_POINT('Ctrl Pts',(-7.00372845487236,-5.77532347926509,
0.983778856318835));
#77673=CARTESIAN_POINT('Ctrl Pts',(-6.88446248245522,-3.95187508991586,
-4.32491218431002));
#77674=CARTESIAN_POINT('Ctrl Pts',(-6.76519651003803,1.49932570880582,-5.66340926891253));
#77675=CARTESIAN_POINT('Ctrl Pts',(-6.64593053762087,5.57417165602073,-1.80299541804897));
#77676=CARTESIAN_POINT('Ctrl Pts',(-6.52666456520372,4.53202524004452,3.71253678121714));
#77677=CARTESIAN_POINT('Ctrl Pts',(-6.40739859278654,-0.670441304941221,
5.82002496428659));
#77678=CARTESIAN_POINT('Ctrl Pts',(-6.28813262036937,-5.25745442490609,
2.58483173501215));
#77679=CARTESIAN_POINT('Ctrl Pts',(-6.16886664795223,-5.01821607609671,
-3.02319194592326));
#77680=CARTESIAN_POINT('Ctrl Pts',(-6.04960067553504,-0.172342890253803,
-5.85597814685722));
#77681=CARTESIAN_POINT('Ctrl Pts',(-5.93033470311789,4.83173806307439,-3.31307854089344));
#77682=CARTESIAN_POINT('Ctrl Pts',(-5.81106873070073,5.40036774303056,2.27116938345109));
#77683=CARTESIAN_POINT('Ctrl Pts',(-5.69180275828355,1.01155402067174,5.77052342440038));
#77684=CARTESIAN_POINT('Ctrl Pts',(-5.5725367858664,-4.3058486505297,3.9726376032835));
#77685=CARTESIAN_POINT('Ctrl Pts',(-5.45327081344922,-5.67055735723522,
-1.47206025236609));
#77686=CARTESIAN_POINT('Ctrl Pts',(-5.33400484103207,-1.82979330806154,
-5.56543246999403));
#77687=CARTESIAN_POINT('Ctrl Pts',(-5.21473886861489,3.69068908517426,-4.54983474478646));
#77688=CARTESIAN_POINT('Ctrl Pts',(-5.09547289619774,5.82318326614332,0.642431924174813));
#77689=CARTESIAN_POINT('Ctrl Pts',(-4.97620692378057,2.61009676874675,5.24495729115771));
#77690=CARTESIAN_POINT('Ctrl Pts',(-4.85694095136341,-2.99901304064116,
5.03270334018952));
#77691=CARTESIAN_POINT('Ctrl Pts',(-4.73767497894624,-5.85508118338141,
0.200515496417569));
#77692=CARTESIAN_POINT('Ctrl Pts',(-4.61840900652908,-3.33628691605105,
-4.8157420759502));
#77693=CARTESIAN_POINT('Ctrl Pts',(-4.49914303411192,2.24516055328616,-5.41123241214589));
#77694=CARTESIAN_POINT('Ctrl Pts',(-4.37987706169475,5.76558979170929,-1.03930576926535));
#77695=CARTESIAN_POINT('Ctrl Pts',(-4.26061108927759,3.99330815683104,4.28668544365891));
#77696=CARTESIAN_POINT('Ctrl Pts',(-4.14134511686042,-1.4447607202292,5.67757418177634));
#77697=CARTESIAN_POINT('Ctrl Pts',(-4.02207914444326,-5.55656445364856,
1.85654884146363));
#77698=CARTESIAN_POINT('Ctrl Pts',(-3.90281317202609,-4.56753892857381,
-3.66875595594112));
#77699=CARTESIAN_POINT('Ctrl Pts',(-3.78354719960893,0.614407672199417,
-5.82620677118766));
#77700=CARTESIAN_POINT('Ctrl Pts',(-3.66428122719176,5.2323387455472,-2.63530138316969));
#77701=CARTESIAN_POINT('Ctrl Pts',(-3.5450152547746,5.04707410573905,2.97476471329566));
#77702=CARTESIAN_POINT('Ctrl Pts',(-3.42574928235743,0.228683460987768,
5.85404868471053));
#77703=CARTESIAN_POINT('Ctrl Pts',(-3.30648330994027,-4.79963461256785,
3.35941806182726));
#77704=CARTESIAN_POINT('Ctrl Pts',(-3.1872173375231,-5.42197182041219,-2.21909975146378));
#77705=CARTESIAN_POINT('Ctrl Pts',(-3.06795136510594,-1.06703345969384,
-5.76052269539703));
#77706=CARTESIAN_POINT('Ctrl Pts',(-2.94868539268877,4.26742300729336,-4.01388627207025));
#77707=CARTESIAN_POINT('Ctrl Pts',(-2.82941942027161,5.68445958010836,1.41742774433296));
#77708=CARTESIAN_POINT('Ctrl Pts',(-2.71015344785444,1.88326139891008,5.54756781226383));
#77709=CARTESIAN_POINT('Ctrl Pts',(-2.59088747543728,-3.64673790123239,
4.58513738158476));
#77710=CARTESIAN_POINT('Ctrl Pts',(-2.47162150302012,-5.82909540943063,
-0.586369197728859));
#77711=CARTESIAN_POINT('Ctrl Pts',(-2.35235553060295,-2.66044499483698,
-5.21959908017247));
#77712=CARTESIAN_POINT('Ctrl Pts',(-2.23308955818579,2.95044752519428,-5.06132804008646));
#77713=CARTESIAN_POINT('Ctrl Pts',(-2.11382358576862,5.85288067474523,-0.256846131923952));
#77714=CARTESIAN_POINT('Ctrl Pts',(-1.99455761335146,3.38247144277536,4.78341604578777));
#77715=CARTESIAN_POINT('Ctrl Pts',(-1.8752916409343,-2.1929875812473,5.43258571923035));
#77716=CARTESIAN_POINT('Ctrl Pts',(-1.75602566851713,-5.7553222527583,1.0947364501082));
#77717=CARTESIAN_POINT('Ctrl Pts',(-1.63675969609996,-4.03437147265267,
-4.24806178732573));
#77718=CARTESIAN_POINT('Ctrl Pts',(-1.5174937236828,1.39006195738937,-5.69121339284596));
#77719=CARTESIAN_POINT('Ctrl Pts',(-1.39822775126564,5.53844275409686,-1.90993036205053));
#77720=CARTESIAN_POINT('Ctrl Pts',(-1.27896177884847,4.60262969644498,3.62463543072867));
#77721=CARTESIAN_POINT('Ctrl Pts',(-1.15969580643131,-0.558317149806238,
5.83184911400515));
#77722=CARTESIAN_POINT('Ctrl Pts',(-1.04042983401414,-5.20673858993517,
2.68552702171667));
#77723=CARTESIAN_POINT('Ctrl Pts',(-0.921163861596979,-5.07546481327733,
-2.92606203923883));
#77724=CARTESIAN_POINT('Ctrl Pts',(-0.801897889179813,-0.285002857307873,
-5.85157718052293));
#77725=CARTESIAN_POINT('Ctrl Pts',(-0.68263191676265,4.7670867510423,-3.40544652524855));
#77726=CARTESIAN_POINT('Ctrl Pts',(-0.563365944345483,5.44307386290664,
2.16682464708923));
#77727=CARTESIAN_POINT('Ctrl Pts',(-0.44409997192832,1.12241409923112,5.74998858417455));
#77728=CARTESIAN_POINT('Ctrl Pts',(-0.324833999511155,-4.22860223193546,
4.05476328438059));
#77729=CARTESIAN_POINT('Ctrl Pts',(-0.205568027093992,-5.69783546364988,
-1.36266399287005));
#77730=CARTESIAN_POINT('Ctrl Pts',(-0.0863020546768254,-1.93655511354362,
-5.52918949037728));
#77731=CARTESIAN_POINT('Ctrl Pts',(0.0329639177403375,3.60244905606469,
-4.62001546823699));
#77732=CARTESIAN_POINT('Ctrl Pts',(0.152229890157503,5.83446782116765,0.530252177788952));
#77733=CARTESIAN_POINT('Ctrl Pts',(0.271495862574667,2.71054688320229,5.19375757253385));
#77734=CARTESIAN_POINT('Ctrl Pts',(0.390761834991831,-2.90160881991181,
5.08948409806933));
#77735=CARTESIAN_POINT('Ctrl Pts',(0.510027807408999,-5.85013823221736,
0.313152985359231));
#77736=CARTESIAN_POINT('Ctrl Pts',(0.629293779826159,-3.42834277741273,
-4.75064710632693));
#77737=CARTESIAN_POINT('Ctrl Pts',(0.748559752243327,2.14061155461703,-5.45343600865826));
#77738=CARTESIAN_POINT('Ctrl Pts',(0.867825724660488,5.74452181311114,-1.15006576637208));
#77739=CARTESIAN_POINT('Ctrl Pts',(0.987091697077656,4.07506123521824,4.20904479157825));
#77740=CARTESIAN_POINT('Ctrl Pts',(1.10635766949482,-1.33523448499132,5.70432563923033));
#77741=CARTESIAN_POINT('Ctrl Pts',(1.22562364191199,-5.51980823530243,1.96313503707162));
#77742=CARTESIAN_POINT('Ctrl Pts',(1.34488961432914,-4.63729429450974,-3.5801792908174));
#77743=CARTESIAN_POINT('Ctrl Pts',(1.46415558674632,0.502174931333422,-5.83695147029944));
#77744=CARTESIAN_POINT('Ctrl Pts',(1.58342155916348,5.18065632845705,-2.7355040001266));
#77745=CARTESIAN_POINT('Ctrl Pts',(1.70268753158064,5.10338556993982,2.87708843326382));
#77746=CARTESIAN_POINT('Ctrl Pts',(1.82195350399781,0.341295864450316,5.84856386313765));
#77747=CARTESIAN_POINT('Ctrl Pts',(1.94121947641497,-4.73409749219153,3.45115966925853));
#77748=CARTESIAN_POINT('Ctrl Pts',(2.06048544883214,-5.46367191661918,-2.11434891061935));
#77749=CARTESIAN_POINT('Ctrl Pts',(2.17975142124929,-1.17769081144187,-5.7389220661145));
#77750=CARTESIAN_POINT('Ctrl Pts',(2.29901739366647,4.18938991897566,-4.09526485530251));
#77751=CARTESIAN_POINT('Ctrl Pts',(2.41828336608364,5.71068376935081,1.30777406869979));
#77752=CARTESIAN_POINT('Ctrl Pts',(2.53754933850079,1.98966951735438,5.5102992060324));
#77753=CARTESIAN_POINT('Ctrl Pts',(2.65681531091796,-3.55782665049407,4.65446577528774));
#77754=CARTESIAN_POINT('Ctrl Pts',(2.77608128333512,-5.8393000039083,-0.474086060380299));
#77755=CARTESIAN_POINT('Ctrl Pts',(2.89534725575229,-2.76039779477465,-5.16743516097626));
#77756=CARTESIAN_POINT('Ctrl Pts',(3.01461322816945,2.85250144690018,-5.11716890709337));
#77757=CARTESIAN_POINT('Ctrl Pts',(3.13387920058662,5.84685410972783,-0.369430843121191));
#77758=CARTESIAN_POINT('Ctrl Pts',(3.25314517300378,3.47389667261357,4.71743829173152));
#77759=CARTESIAN_POINT('Ctrl Pts',(3.37241114542095,-2.08803732303183,5.47378134984554));
#77760=CARTESIAN_POINT('Ctrl Pts',(3.4916771178381,-5.73318947280932,1.20528859496755));
#77761=CARTESIAN_POINT('Ctrl Pts',(3.61094309025528,-4.11537367695382,-4.16963806910456));
#77762=CARTESIAN_POINT('Ctrl Pts',(3.73020906267244,1.28028337965748,-5.71690970683145));
#77763=CARTESIAN_POINT('Ctrl Pts',(3.8494750350896,5.50066262268514,-2.01615794016368));
#77764=CARTESIAN_POINT('Ctrl Pts',(3.96874100750677,4.67152951308028,3.53539165252032));
#77765=CARTESIAN_POINT('Ctrl Pts',(4.08800697992393,-0.445986215139254,
5.84151336762971));
#77766=CARTESIAN_POINT('Ctrl Pts',(4.20727295234111,-5.15409437613914,2.78522769089733));
#77767=CARTESIAN_POINT('Ctrl Pts',(4.32653892475825,-5.13083379046902,-2.82784842996788));
#77768=CARTESIAN_POINT('Ctrl Pts',(4.44580489717543,-0.39755727009488,-5.84500901156581));
#77769=CARTESIAN_POINT('Ctrl Pts',(4.56507086959259,4.7006698905792,-3.49655326115484));
#77770=CARTESIAN_POINT('Ctrl Pts',(4.68433684200975,5.483764074321,2.06167740092304));
#77771=CARTESIAN_POINT('Ctrl Pts',(4.80360281442692,1.23285847810731,5.72732416589543));
#77772=CARTESIAN_POINT('Ctrl Pts',(4.92286878684409,-4.14978969918686,4.1353872346871));
#77773=CARTESIAN_POINT('Ctrl Pts',(5.04213475926125,-5.72300330755224,-1.25276305422717));
#77774=CARTESIAN_POINT('Ctrl Pts',(5.16140073167841,-2.04259969233753,-5.49089870833121));
#77775=CARTESIAN_POINT('Ctrl Pts',(5.28066670409558,3.51287481622839,-4.68848511289082));
#77776=CARTESIAN_POINT('Ctrl Pts',(5.39993267651275,5.84359151022793,0.417876046074028));
#77777=CARTESIAN_POINT('Ctrl Pts',(5.51919864892991,2.80999311372474,5.14063428276219));
#77778=CARTESIAN_POINT('Ctrl Pts',(5.63846462134707,-2.80312995314244,5.14437990374799));
#77779=CARTESIAN_POINT('Ctrl Pts',(5.75773059376424,-5.84302861136241,0.425674494292362));
#77780=CARTESIAN_POINT('Ctrl Pts',(5.8769965661814,-3.51912891042079,-4.68379267689455));
#77781=CARTESIAN_POINT('Ctrl Pts',(5.99626253859856,2.03526975448046,-5.49361985896253));
#77782=CARTESIAN_POINT('Ctrl Pts',(6.11552851101573,5.72132628114465,-1.26039982266515));
#77783=CARTESIAN_POINT('Ctrl Pts',(6.23479448343289,4.15530506522249,4.12984526867857));
#77784=CARTESIAN_POINT('Ctrl Pts',(6.35406045585006,-1.2252137294577,5.72896443045676));
#77785=CARTESIAN_POINT('Ctrl Pts',(6.47332642826722,-5.4810076889886,2.06899416179424));
#77786=CARTESIAN_POINT('Ctrl Pts',(6.59259240068438,-4.70533218222602,-3.49027666284472));
#77787=CARTESIAN_POINT('Ctrl Pts',(6.71185837310156,0.389756203887297,-5.8455343835976));
#77788=CARTESIAN_POINT('Ctrl Pts',(6.83112434551871,5.1270551924238,-2.83469348997928));
#77789=CARTESIAN_POINT('Ctrl Pts',(6.95039031793589,5.15780693336066,2.77834658861474));
#77790=CARTESIAN_POINT('Ctrl Pts',(7.06965629035304,0.453781864847495,5.84091295496054));
#77791=CARTESIAN_POINT('Ctrl Pts',(7.18892226277022,-4.66680704135651,3.54162309782339));
#77792=CARTESIAN_POINT('Ctrl Pts',(7.30818823518737,-5.50334847562537,-2.00881499499638));
#77793=CARTESIAN_POINT('Ctrl Pts',(7.42745420760454,-1.28791199110556,-5.71519595739787));
#77794=CARTESIAN_POINT('Ctrl Pts',(7.54672018002171,4.1098052392595,-4.17512670749595));
#77795=CARTESIAN_POINT('Ctrl Pts',(7.66598615243887,5.7347929375551,1.19763604306929));
#77796=CARTESIAN_POINT('Ctrl Pts',(7.78525212485604,2.09534073754652,5.47098979361764));
#77797=CARTESIAN_POINT('Ctrl Pts',(7.9045180972732,-3.46759771547835,4.72207033110479));
#77798=CARTESIAN_POINT('Ctrl Pts',(8.02378406969036,-5.84734194276446,-0.361627339505832));
#77799=CARTESIAN_POINT('Ctrl Pts',(8.14305004210753,-2.85932824788915,-5.11335741945677));
#77800=CARTESIAN_POINT('Ctrl Pts',(8.26231601452469,2.75349891007753,-5.17111456849417));
#77801=CARTESIAN_POINT('Ctrl Pts',(8.38158198694186,5.83866209133414,-0.481878731122364));
#77802=CARTESIAN_POINT('Ctrl Pts',(8.50084795935901,3.56403530266033,4.64971337715362));
#77803=CARTESIAN_POINT('Ctrl Pts',(8.62011393177619,-1.98231373485353,5.51294969910862));
#77804=CARTESIAN_POINT('Ctrl Pts',(8.73937990419334,-5.70893333656173,1.31539434656858));
#77805=CARTESIAN_POINT('Ctrl Pts',(8.85864587661052,-4.19485170267006,-4.08967007482224));
#77806=CARTESIAN_POINT('Ctrl Pts',(8.97791184902767,1.1700306334385,-5.74048869392723));
#77807=CARTESIAN_POINT('Ctrl Pts',(9.09717782144485,5.46084525411568,-2.1216388097159));
#77808=CARTESIAN_POINT('Ctrl Pts',(9.21644379386201,4.73869917206731,3.44483849910834));
#77809=CARTESIAN_POINT('Ctrl Pts',(9.33570976627917,-0.333490104064998,
5.8490141458866));
#77810=CARTESIAN_POINT('Ctrl Pts',(9.45497573869634,-5.0995412809414,2.88389681720152));
#77811=CARTESIAN_POINT('Ctrl Pts',(9.5742417111135,-5.18430250109922,-2.72858749271244));
#77812=CARTESIAN_POINT('Ctrl Pts',(9.69350768353068,-0.509964442722255,
-5.83627607258685));
#77813=CARTESIAN_POINT('Ctrl Pts',(9.81277365594782,4.6325120799753,-3.58636500612715));
#77814=CARTESIAN_POINT('Ctrl Pts',(9.93203962836501,5.52242330716014,1.95576658751111));
#77815=CARTESIAN_POINT('Ctrl Pts',(10.0513056007822,1.34284625288435,5.70253856360527));
#77816=CARTESIAN_POINT('Ctrl Pts',(10.1705715731993,-4.06944024146176,4.2144795941447));
#77817=CARTESIAN_POINT('Ctrl Pts',(10.2898375456165,-5.74605156772597,-1.14239813958374));
#77818=CARTESIAN_POINT('Ctrl Pts',(10.4091035180337,-2.14788776954667,-5.45057430531156));
#77819=CARTESIAN_POINT('Ctrl Pts',(10.5283694904508,3.42199954057199,-4.75521832018421));
#77820=CARTESIAN_POINT('Ctrl Pts',(10.647635462868,5.85055095425527,0.305345148894098));
#77821=CARTESIAN_POINT('Ctrl Pts',(10.7669014352851,2.90839862919574,5.08560709669781));
#77822=CARTESIAN_POINT('Ctrl Pts',(10.8861674077023,-2.70361291317653,5.19737042589766));
#77823=CARTESIAN_POINT('Ctrl Pts',(11.0054333801195,-5.83375495395087,0.538038349510541));
#77824=CARTESIAN_POINT('Ctrl Pts',(11.1246993525366,-3.60861169132913,-4.61520354800236));
#77825=CARTESIAN_POINT('Ctrl Pts',(11.2439653249538,1.92917416749059,-5.53176908048207));
#77826=CARTESIAN_POINT('Ctrl Pts',(11.363231297371,5.69601178655655,-1.37026707458776));
#77827=CARTESIAN_POINT('Ctrl Pts',(11.4824972697881,4.23400992756751,4.04911620746435));
#77828=CARTESIAN_POINT('Ctrl Pts',(11.6017632422053,-1.11473920115039,5.75148143018032));
#77829=CARTESIAN_POINT('Ctrl Pts',(11.7210292146225,-5.44017718496026,2.17408700941989));
#77830=CARTESIAN_POINT('Ctrl Pts',(11.8402951870396,-4.77162739306525,-3.39908136855241));
#77831=CARTESIAN_POINT('Ctrl Pts',(11.9595611594568,0.277193125501102,-5.85195233229607));
#77832=CARTESIAN_POINT('Ctrl Pts',(12.078827131874,5.07155518927873,-2.93283311669634));
#77833=CARTESIAN_POINT('Ctrl Pts',(12.1980931042911,5.21031804038915,2.67857574958897));
#77834=CARTESIAN_POINT('Ctrl Pts',(12.3173590767083,0.566099801623865,5.83109879378591));
#77835=CARTESIAN_POINT('Ctrl Pts',(12.4366250491254,-4.59778818189795,3.63077484329315));
#77836=CARTESIAN_POINT('Ctrl Pts',(12.5558910215426,-5.54098680273559,-1.90253709036138));
#77837=CARTESIAN_POINT('Ctrl Pts',(12.6751569939598,-1.39765617693328,-5.68935315649946));
#77838=CARTESIAN_POINT('Ctrl Pts',(12.794422966377,4.02869844329693,-4.25344225084433));
#77839=CARTESIAN_POINT('Ctrl Pts',(12.9136889387941,5.75677815559816,1.08705445839597));
#77840=CARTESIAN_POINT('Ctrl Pts',(13.0329549112113,2.20023592286751,5.42965413373763));
#77841=CARTESIAN_POINT('Ctrl Pts',(13.1522208836285,-3.37608451356654,4.78792601086807));
#77842=CARTESIAN_POINT('Ctrl Pts',(13.2714868560456,-5.85321824756939,-0.249034685557716));
#77843=CARTESIAN_POINT('Ctrl Pts',(13.3907528284628,-2.95719971408639,-5.057385883962));
#77844=CARTESIAN_POINT('Ctrl Pts',(13.5100188008799,2.65347658151761,-5.22314504485836));
#77845=CARTESIAN_POINT('Ctrl Pts',(13.6292847732971,5.82830765357758,-0.594148149487238));
#77846=CARTESIAN_POINT('Ctrl Pts',(13.7485507457143,3.65285394897987,4.58026638479827));
#77847=CARTESIAN_POINT('Ctrl Pts',(13.8678167181314,-1.87585597272662,5.55007626054603));
#77848=CARTESIAN_POINT('Ctrl Pts',(13.9870826905486,-5.68256282757001,1.42501292590967));
#77849=CARTESIAN_POINT('Ctrl Pts',(14.1063486629658,-4.27277611414985,-4.00818742159612));
#77850=CARTESIAN_POINT('Ctrl Pts',(14.2256146353829,1.05934455217531,-5.76194162136924));
#77851=CARTESIAN_POINT('Ctrl Pts',(14.3448806078001,5.41900539523421,-2.22633390458677));
#77852=CARTESIAN_POINT('Ctrl Pts',(14.4641465802173,4.80411379630757,3.35300950795224));
#77853=CARTESIAN_POINT('Ctrl Pts',(14.5834125526344,-0.220870480883753,
5.85434867077158));
#77854=CARTESIAN_POINT('Ctrl Pts',(14.7026785250516,-5.04309950874287,2.98149785732063));
#77855=CARTESIAN_POINT('Ctrl Pts',(14.8219444974687,-5.23585114238199,-2.62831598996543));
#77856=CARTESIAN_POINT('Ctrl Pts',(14.9412104698859,-0.622182743829148,
-5.82538159793605));
#77857=CARTESIAN_POINT('Ctrl Pts',(15.0604764423031,4.56263856230305,-3.67484849729553));
#77858=CARTESIAN_POINT('Ctrl Pts',(15.1797424147202,5.55903724350795,1.84913143220874));
#77859=CARTESIAN_POINT('Ctrl Pts',(15.2990083871374,1.45233668825476,5.67564095695279));
#77860=CARTESIAN_POINT('Ctrl Pts',(15.4182743595546,-3.98758361715711,4.29201106993799));
#77861=CARTESIAN_POINT('Ctrl Pts',(15.5375403319718,-5.76697170796816,-1.03161012392551));
#77862=CARTESIAN_POINT('Ctrl Pts',(15.6568063043889,-2.25238035045361,-5.40823121595048));
#77863=CARTESIAN_POINT('Ctrl Pts',(15.7760722768061,3.32985688585691,-4.82019037466379));
#77864=CARTESIAN_POINT('Ctrl Pts',(15.8953382492232,5.85534357573511,0.192701163432864));
#77865=CARTESIAN_POINT('Ctrl Pts',(16.0146042216404,3.00572698393825,5.02869639432689));
#77866=CARTESIAN_POINT('Ctrl Pts',(16.1338701940575,-2.60309455735759,5.24843603883532));
#77867=CARTESIAN_POINT('Ctrl Pts',(16.2531361664747,-5.82232069459445,0.650202935696243));
#77868=CARTESIAN_POINT('Ctrl Pts',(16.3724021388919,-3.69675797910371,-4.54490512246668));
#77869=CARTESIAN_POINT('Ctrl Pts',(16.491668111309,1.82236408743567,-5.56786954418967));
#77870=CARTESIAN_POINT('Ctrl Pts',(16.6109340837262,5.66858770487726,-1.47962683146975));
#77871=CARTESIAN_POINT('Ctrl Pts',(16.7302000561434,4.31114667295226,3.96688750692321));
#77872=CARTESIAN_POINT('Ctrl Pts',(16.8494660285605,-1.00385181565173,5.77186829895683));
#77873=CARTESIAN_POINT('Ctrl Pts',(16.9687320009777,-5.39733184529022,2.27837465753701));
#77874=CARTESIAN_POINT('Ctrl Pts',(17.0879979733949,-4.83615537379139,-3.30662718322454));
#77875=CARTESIAN_POINT('Ctrl Pts',(17.207263945812,0.164527385277041,-5.85620293942961));
#77876=CARTESIAN_POINT('Ctrl Pts',(17.3265299182292,5.01417687412153,-3.02988653307605));
#77877=CARTESIAN_POINT('Ctrl Pts',(17.4457958906464,5.26089944289952,2.57781286752749));
#77878=CARTESIAN_POINT('Ctrl Pts',(17.5650618630635,0.678208076468528,5.81912501440749));
#77879=CARTESIAN_POINT('Ctrl Pts',(17.6843278354807,-4.52706647578802,3.71858188723699));
#77880=CARTESIAN_POINT('Ctrl Pts',(17.8035938078979,-5.57657295813861,-1.79555455802603));
#77881=CARTESIAN_POINT('Ctrl Pts',(17.922859780315,-1.50688272383402,-5.66140323461425));
#77882=CARTESIAN_POINT('Ctrl Pts',(18.0421257527322,3.94609956997411,-4.33018248023578));
#77883=CARTESIAN_POINT('Ctrl Pts',(18.1613917251494,5.77663128098768,0.976070269911672));
#77884=CARTESIAN_POINT('Ctrl Pts',(18.2806576975665,2.30431622411275,5.3863075355554));
#77885=CARTESIAN_POINT('Ctrl Pts',(18.3999236699837,-3.28332093778318,4.85200842412762));
#77886=CARTESIAN_POINT('Ctrl Pts',(18.5191896424009,-5.85692674196245,-0.136349798591407));
#77887=CARTESIAN_POINT('Ctrl Pts',(18.638455614818,-3.05397594548137,-4.99954128422911));
#77888=CARTESIAN_POINT('Ctrl Pts',(18.7577215872352,2.55247150570324,-5.2732410660678));
#77889=CARTESIAN_POINT('Ctrl Pts',(18.8769875596523,5.81579463134992,-0.706197517874579));
#77890=CARTESIAN_POINT('Ctrl Pts',(18.9962535320695,3.74031971650885,4.50912303520155));
#77891=CARTESIAN_POINT('Ctrl Pts',(19.1155195044867,-1.76870346457484,5.58514728388534));
#77892=CARTESIAN_POINT('Ctrl Pts',(19.2347854769038,-5.65408771247222,1.53410373442001));
#77893=CARTESIAN_POINT('Ctrl Pts',(19.354051449321,-4.34911805114188,-3.92522028751534));
#77894=CARTESIAN_POINT('Ctrl Pts',(19.4733174217381,0.948266129800921,-5.78126054380557));
#77895=CARTESIAN_POINT('Ctrl Pts',(19.5925833941553,5.37515854194023,-2.33020444967771));
#77896=CARTESIAN_POINT('Ctrl Pts',(19.7118493665725,4.86774915870119,3.25993868903297));
#77897=CARTESIAN_POINT('Ctrl Pts',(19.8311153389897,-0.108169055639234,
5.85751496657865));
#77898=CARTESIAN_POINT('Ctrl Pts',(19.9503813114068,-4.98478996343882,3.07799466352533));
#77899=CARTESIAN_POINT('Ctrl Pts',(20.069647283824,-5.28546062265248,-2.52707105849445));
#77900=CARTESIAN_POINT('Ctrl Pts',(20.1889132562411,-0.734170612006343,
-5.81232962251428));
#77901=CARTESIAN_POINT('Ctrl Pts',(20.3081792286583,4.49107521606757,-3.76197096372558));
#77902=CARTESIAN_POINT('Ctrl Pts',(20.4274452010755,5.59359232294874,1.74181142863946));
#77903=CARTESIAN_POINT('Ctrl Pts',(20.5467111734926,1.5612892331075,5.64664130779292));
#77904=CARTESIAN_POINT('Ctrl Pts',(20.6659771459098,-3.90425014286694,4.36795294734436));
#77905=CARTESIAN_POINT('Ctrl Pts',(20.785243118327,-5.78575598025094,-0.920440038938236));
#77906=CARTESIAN_POINT('Ctrl Pts',(20.9045090907441,-2.35603873496334,-5.36388512252482));
#77907=CARTESIAN_POINT('Ctrl Pts',(21.0237750631613,3.23648097823332,-4.88337721314099));
#77908=CARTESIAN_POINT('Ctrl Pts',(21.1430410355785,5.85796759966182,0.0799858087570004));
#77909=CARTESIAN_POINT('Ctrl Pts',(21.2623070079956,3.10194213121528,4.96992325321854));
#77910=CARTESIAN_POINT('Ctrl Pts',(21.3815729804128,-2.5016121138784,5.29755782979173));
#77911=CARTESIAN_POINT('Ctrl Pts',(21.50083895283,-5.80873006810966,0.762126711334059));
#77912=CARTESIAN_POINT('Ctrl Pts',(21.6201049252471,-3.78353512769747,-4.47292343616231));
#77913=CARTESIAN_POINT('Ctrl Pts',(21.7393708976643,1.71487907272487,-5.60190787984068));
#77914=CARTESIAN_POINT('Ctrl Pts',(21.8586368700815,5.63906419294801,-1.58843859059823));
#77915=CARTESIAN_POINT('Ctrl Pts',(21.9779028424986,4.38668673284723,3.88318962145203));
#77916=CARTESIAN_POINT('Ctrl Pts',(22.0971688149158,-0.892592641450376,
5.79011748626221));
#77917=CARTESIAN_POINT('Ctrl Pts',(22.2164347873329,-5.35248753826974,2.38181848194971));
#77918=CARTESIAN_POINT('Ctrl Pts',(22.3357007597501,-4.89889222568395,-3.21294834839033));
#77919=CARTESIAN_POINT('Ctrl Pts',(22.4549667321672,0.0518007103390068,
-5.85828463073442));
#77920=CARTESIAN_POINT('Ctrl Pts',(22.5742327045845,4.95494149770743,-3.12581779420793));
#77921=CARTESIAN_POINT('Ctrl Pts',(22.6934986770016,5.3095324074556,2.47609526118635));
#77922=CARTESIAN_POINT('Ctrl Pts',(22.8127646494188,0.79006516872153,5.80499605145979));
#77923=CARTESIAN_POINT('Ctrl Pts',(22.9320306218359,-4.45466811566874,3.80501170925063));
#77924=CARTESIAN_POINT('Ctrl Pts',(23.0512965942531,-5.61009376206996,-1.68790702026934));
#77925=CARTESIAN_POINT('Ctrl Pts',(23.1705625666702,-1.61555117843076,-5.63135654333499));
#77926=CARTESIAN_POINT('Ctrl Pts',(23.2898285390874,3.86203921078604,-4.4053189739951));
#77927=CARTESIAN_POINT('Ctrl Pts',(23.4090945115046,5.79434496087777,0.864724581957292));
#77928=CARTESIAN_POINT('Ctrl Pts',(23.5283604839218,2.40754309387953,5.34096605300986));
#77929=CARTESIAN_POINT('Ctrl Pts',(23.6476264563389,-3.18934134424452,4.9142938371838));
#77930=CARTESIAN_POINT('Ctrl Pts',(23.7668924287561,-5.85846605245757,-0.0236144128224182));
#77931=CARTESIAN_POINT('Ctrl Pts',(23.8861584011732,-3.1496210998223,-4.93984504370784));
#77932=CARTESIAN_POINT('Ctrl Pts',(24.0054243735904,2.45052109109024,-5.3213840784529));
#77933=CARTESIAN_POINT('Ctrl Pts',(24.1246903460076,5.80112765900066,-0.817985337440891));
#77934=CARTESIAN_POINT('Ctrl Pts',(24.2439563184247,3.8264002112388,4.43630967716665));
#77935=CARTESIAN_POINT('Ctrl Pts',(24.3632222908419,-1.6608958956302,5.61814978014727));
#77936=CARTESIAN_POINT('Ctrl Pts',(24.482488263259,-5.62351853737269,1.64262636899463));
#77937=CARTESIAN_POINT('Ctrl Pts',(24.6017542356763,-4.42384923948336,-3.84079940046513));
#77938=CARTESIAN_POINT('Ctrl Pts',(24.7210202080934,0.836836505557353,-5.79843830623873));
#77939=CARTESIAN_POINT('Ctrl Pts',(24.8402861805106,5.32932093344786,-2.43321197527163));
#77940=CARTESIAN_POINT('Ctrl Pts',(24.9595521529278,4.92958169111955,3.16566051225803));
#77941=CARTESIAN_POINT('Ctrl Pts',(25.0788181253449,0.00457243132771929,
5.85851186063166));
#77942=CARTESIAN_POINT('Ctrl Pts',(25.1980840977621,-4.92463424067689,3.17335149705221));
#77943=CARTESIAN_POINT('Ctrl Pts',(25.3173500701792,-5.33311256843772,-2.42489019558874));
#77944=CARTESIAN_POINT('Ctrl Pts',(25.4366160425964,-0.845886571187518,
-5.797124980279));
#77945=CARTESIAN_POINT('Ctrl Pts',(25.5558820150136,4.41784854562258,-3.84770013855436));
#77946=CARTESIAN_POINT('Ctrl Pts',(25.6751479874307,5.62607574758965,1.63384632406917));
#77947=CARTESIAN_POINT('Ctrl Pts',(25.7944139598479,1.66966353554507,5.61555035649768));
#77948=CARTESIAN_POINT('Ctrl Pts',(25.9136799322651,-3.81947068215475,4.44227710036768));
#77949=CARTESIAN_POINT('Ctrl Pts',(26.0329459046822,-5.80239742759128,-0.808929057812192));
#77950=CARTESIAN_POINT('Ctrl Pts',(26.1522118770994,-2.45882453193489,-5.31755244914851));
#77951=CARTESIAN_POINT('Ctrl Pts',(26.2714778495165,3.14190640060181,-4.94475543360317));
#77952=CARTESIAN_POINT('Ctrl Pts',(26.3907438219337,5.85842205419648,-0.032759169633832));
#77953=CARTESIAN_POINT('Ctrl Pts',(26.5100097943509,3.19700843657914,4.90930944071892));
#77954=CARTESIAN_POINT('Ctrl Pts',(26.629275766768,-2.39920316799348,5.34471760591528));
#77955=CARTESIAN_POINT('Ctrl Pts',(26.7485417391852,-5.79298810795018,0.873768224095266));
#77956=CARTESIAN_POINT('Ctrl Pts',(26.8678077116024,-3.86891099814006,-4.39928514838047));
#77957=CARTESIAN_POINT('Ctrl Pts',(26.9870736840195,1.60675893173784,-5.63387148092423));
#77958=CARTESIAN_POINT('Ctrl Pts',(27.1063396564367,5.60745218515998,-1.69666205221763));
#77959=CARTESIAN_POINT('Ctrl Pts',(27.2256056288539,4.46060213007431,3.79805354957861));
#77960=CARTESIAN_POINT('Ctrl Pts',(27.344871601271,-0.781002884731814,5.8062222332883));
#77961=CARTESIAN_POINT('Ctrl Pts',(27.4641375736882,-5.3056608725324,2.4843801709822));
#77962=CARTESIAN_POINT('Ctrl Pts',(27.5834035461053,-4.95981471338826,-3.11807955914333));
#77963=CARTESIAN_POINT('Ctrl Pts',(27.7026695185225,-0.0609451496207866,
-5.85819663523071));
#77964=CARTESIAN_POINT('Ctrl Pts',(27.8219354909397,4.89387099857715,-3.22059137078522));
#77965=CARTESIAN_POINT('Ctrl Pts',(27.9412014633569,5.35619892224863,2.37346060291565));
#77966=CARTESIAN_POINT('Ctrl Pts',(28.060467435774,0.901629650751189,5.78871713777561));
#77967=CARTESIAN_POINT('Ctrl Pts',(28.1797334081912,-4.38061991515157,3.89003229900066));
#77968=CARTESIAN_POINT('Ctrl Pts',(28.2989993806083,-5.64153679969301,-1.57963434566348));
#77969=CARTESIAN_POINT('Ctrl Pts',(28.4182653530255,-1.72362129404252,-5.59922421081825));
#77970=CARTESIAN_POINT('Ctrl Pts',(28.5375313254427,3.77654849850695,-4.47882390441015));
#77971=CARTESIAN_POINT('Ctrl Pts',(28.6567972978598,5.8099126347921,0.753058632759737));
#77972=CARTESIAN_POINT('Ctrl Pts',(28.776063270277,2.50987830084389,5.29364647886908));
#77973=CARTESIAN_POINT('Ctrl Pts',(28.8953292426942,-3.09418053943347,4.97475918187826));
#77974=CARTESIAN_POINT('Ctrl Pts',(29.0145952151113,-5.8578356089525,0.0891297188309879));
#77975=CARTESIAN_POINT('Ctrl Pts',(29.1338611875285,-3.24409975376552,-4.87831927162507));
#77976=CARTESIAN_POINT('Ctrl Pts',(29.2531271599456,2.34766309625184,-5.367556251665));
#77977=CARTESIAN_POINT('Ctrl Pts',(29.3723931323628,5.78431216862107,-0.929470206210548));
#77978=CARTESIAN_POINT('Ctrl Pts',(29.49165910478,3.91106355221379,4.36185327800407));
#77979=CARTESIAN_POINT('Ctrl Pts',(29.6109250771972,-1.55247319373407,5.64907152645706));
#77980=CARTESIAN_POINT('Ctrl Pts',(29.7301910496143,-5.59086662393646,1.75054063695882));
#77981=CARTESIAN_POINT('Ctrl Pts',(29.8494570220315,-4.49694200157167,-3.75495602674528));
#77982=CARTESIAN_POINT('Ctrl Pts',(29.9687229944486,0.725096948758073,-5.81346854667612));
#77983=CARTESIAN_POINT('Ctrl Pts',(30.0879889668658,5.28150954627173,-2.53531833128137));
#77984=CARTESIAN_POINT('Ctrl Pts',(30.207254939283,4.98958849313373,3.07020989469409));
#77985=CARTESIAN_POINT('Ctrl Pts',(30.3265209117001,0.117312224839382,5.85733898371898));
#77986=CARTESIAN_POINT('Ctrl Pts',(30.4457868841173,-4.86265461985911,3.26753304134077));
#77987=CARTESIAN_POINT('Ctrl Pts',(30.5650528565344,-5.37878933126115,-2.32181124517074));
#77988=CARTESIAN_POINT('Ctrl Pts',(30.6843188289516,-0.957289246011629,
-5.77977330245411));
#77989=CARTESIAN_POINT('Ctrl Pts',(30.8035848013688,4.34298567135418,-3.93200427094161));
#77990=CARTESIAN_POINT('Ctrl Pts',(30.9228507737859,5.65647548679995,1.52527610468443));
#77991=CARTESIAN_POINT('Ctrl Pts',(31.0421167462031,1.77741945782958,5.58237961797831));
#77992=CARTESIAN_POINT('Ctrl Pts',(31.1613827186203,-3.73327663412274,4.51495600215594));
#77993=CARTESIAN_POINT('Ctrl Pts',(31.2806486910374,-5.81688988662698,-0.697118479992365));
#77994=CARTESIAN_POINT('Ctrl Pts',(31.3999146634546,-2.5606996734012,-5.26925035568949));
#77995=CARTESIAN_POINT('Ctrl Pts',(31.5191806358718,3.04616817980498,-5.00430230388157));
#77996=CARTESIAN_POINT('Ctrl Pts',(31.6384466082889,5.85670677102611,-0.145492015268766));
#77997=CARTESIAN_POINT('Ctrl Pts',(31.7577125807061,3.29089069107016,4.84687740588913));
#77998=CARTESIAN_POINT('Ctrl Pts',(31.8769785531233,-2.2959056480988,5.38989790101063));
#77999=CARTESIAN_POINT('Ctrl Pts',(31.9962445255404,-5.77510064434174,0.985086126190849));
#78000=CARTESIAN_POINT('Ctrl Pts',(32.1155104979576,-3.95285397044202,-4.3240175319547));
#78001=CARTESIAN_POINT('Ctrl Pts',(32.2347764703747,1.49804370808096,-5.66374850933283));
#78002=CARTESIAN_POINT('Ctrl Pts',(32.3540424427919,5.57376338940363,-1.80425713445558));
#78003=CARTESIAN_POINT('Ctrl Pts',(32.4733084152091,4.53286548916933,3.71151082248032));
#78004=CARTESIAN_POINT('Ctrl Pts',(32.5925743876263,-0.669123874116674,
5.82017657544665));
#78005=CARTESIAN_POINT('Ctrl Pts',(32.7118403600434,-5.25686919090186,2.58602173966828));
#78006=CARTESIAN_POINT('Ctrl Pts',(32.8311063324606,-5.01890027352189,-3.02205595129089));
#78007=CARTESIAN_POINT('Ctrl Pts',(32.9503723048778,-0.173668437804856,
-5.85593898550875));
#78008=CARTESIAN_POINT('Ctrl Pts',(33.0696382772949,4.83098799493092,-3.31417216226366));
#78009=CARTESIAN_POINT('Ctrl Pts',(33.1889042497121,5.40088170376875,2.26994690470652));
#78010=CARTESIAN_POINT('Ctrl Pts',(33.3081702221293,1.01286020329767,5.77029430244824));
#78011=CARTESIAN_POINT('Ctrl Pts',(33.4274361945464,-4.30494929888592,3.97361216807977));
#78012=CARTESIAN_POINT('Ctrl Pts',(33.5467021669636,-5.67089042569741,-1.47077663430731));
#78013=CARTESIAN_POINT('Ctrl Pts',(33.6659681393807,-1.83105304559022,-5.56501813766366));
#78014=CARTESIAN_POINT('Ctrl Pts',(33.7852341117979,3.68965909565966,-4.5506700480375));
#78015=CARTESIAN_POINT('Ctrl Pts',(33.904500084215,5.82332853705378,0.641113779158535));
#78016=CARTESIAN_POINT('Ctrl Pts',(34.0237660566323,2.6112839439197,5.24436633851196));
#78017=CARTESIAN_POINT('Ctrl Pts',(34.1430320290494,-2.99787376730876,5.03338206413637));
#78018=CARTESIAN_POINT('Ctrl Pts',(34.2622980014666,-5.85503564494024,0.201840840211394));
#78019=CARTESIAN_POINT('Ctrl Pts',(34.3815639738837,-3.3373769159937,-4.81498675479765));
#78020=CARTESIAN_POINT('Ctrl Pts',(34.5008299463009,2.24393561589265,-5.41174048527879));
#78021=CARTESIAN_POINT('Ctrl Pts',(34.6200959187181,5.76535438803626,-1.04061083440989));
#78022=CARTESIAN_POINT('Ctrl Pts',(34.7393618911352,3.99427838333004,4.28578141354626));
#78023=CARTESIAN_POINT('Ctrl Pts',(34.8586278635524,-1.44347551453501,5.67790107056843));
#78024=CARTESIAN_POINT('Ctrl Pts',(34.9778938359695,-5.55614406522461,1.85780657095742));
#78025=CARTESIAN_POINT('Ctrl Pts',(35.0971598083867,-4.56836926656086,-3.66772195949845));
#78026=CARTESIAN_POINT('Ctrl Pts',(35.2164257808039,0.613088843400821,-5.82634569847212));
#78027=CARTESIAN_POINT('Ctrl Pts',(35.335691753221,5.23174208813583,-2.6364857014042));
#78028=CARTESIAN_POINT('Ctrl Pts',(35.4549577256382,5.0477473401233,2.97362218768447));
#78029=CARTESIAN_POINT('Ctrl Pts',(35.5742236980554,0.230008571053462,5.85399677013775));
#78030=CARTESIAN_POINT('Ctrl Pts',(35.6934896704726,-4.79887405723636,3.36050441528738));
#78031=CARTESIAN_POINT('Ctrl Pts',(35.8127556428897,-5.42247399162274,-2.21787238411221));
#78032=CARTESIAN_POINT('Ctrl Pts',(35.9320216153069,-1.0683373820018,-5.76028101481488));
#78033=CARTESIAN_POINT('Ctrl Pts',(36.051287587724,4.26651432885973,-4.01485213902346));
#78034=CARTESIAN_POINT('Ctrl Pts',(36.1705535601412,5.68478026414927,1.41614098305311));
#78035=CARTESIAN_POINT('Ctrl Pts',(36.2898195325583,1.88451712452022,5.54714137311024));
#78036=CARTESIAN_POINT('Ctrl Pts',(36.4090855049756,-3.64569998497971,4.58596274338194));
#78037=CARTESIAN_POINT('Ctrl Pts',(36.5283514773927,-5.82922786986728,-0.585049731431784));
#78038=CARTESIAN_POINT('Ctrl Pts',(36.6476174498099,-2.66162665665066,-5.2189967018826));
#78039=CARTESIAN_POINT('Ctrl Pts',(36.766883422227,2.94930220667439,-5.06199582616066));
#78040=CARTESIAN_POINT('Ctrl Pts',(36.8861493946442,5.85282156297383,-0.258170869634671));
#78041=CARTESIAN_POINT('Ctrl Pts',(37.0054153670614,3.383555686377,4.7826500688436));
#78042=CARTESIAN_POINT('Ctrl Pts',(37.1246813394785,-2.19176077869031,5.43308236633426));
#78043=CARTESIAN_POINT('Ctrl Pts',(37.2439473118957,-5.75506866675922,1.09603845971515));
#78044=CARTESIAN_POINT('Ctrl Pts',(37.3632132843128,-4.03534365880062,-4.24714707669714));
#78045=CARTESIAN_POINT('Ctrl Pts',(37.48247925673,1.38879399537905,-5.69153053311651));
#78046=CARTESIAN_POINT('Ctrl Pts',(37.6017452291472,5.53797166977889,-1.91117898649279));
#78047=CARTESIAN_POINT('Ctrl Pts',(37.7210112015643,4.60352338587549,3.62358399241559));
#78048=CARTESIAN_POINT('Ctrl Pts',(37.8402771739815,-0.557136342626843,
5.83199338805448));
#78049=CARTESIAN_POINT('Ctrl Pts',(37.9595431463987,-5.20586598536909,2.68667127376048));
#78050=CARTESIAN_POINT('Ctrl Pts',(38.0788091188158,-5.0766295927031,-2.92484800376138));
#78051=CARTESIAN_POINT('Ctrl Pts',(38.198075091233,-0.285372479780323,-5.85163608426362));
#78052=CARTESIAN_POINT('Ctrl Pts',(38.3173410636502,4.76449886846839,-3.40629125216186));
#78053=CARTESIAN_POINT('Ctrl Pts',(38.4366070360673,5.44704213670987,2.16515129303516));
#78054=CARTESIAN_POINT('Ctrl Pts',(38.5558730084845,1.11688027088538,5.75054041079176));
#78055=CARTESIAN_POINT('Ctrl Pts',(38.6552613188321,-3.32448407322045,4.33716932787563));
#78056=CARTESIAN_POINT('Ctrl Pts',(38.7347719671102,-4.97744277966909,1.34445408741869));
#78057=CARTESIAN_POINT('Ctrl Pts',(38.7745272912493,-5.01009358722135,-0.348796856848898));
#78058=CARTESIAN_POINT('Ctrl Pts',(38.7944049533188,-4.8183901140079,-1.1511875213148));
#78059=CARTESIAN_POINT('Ctrl Pts',(38.0164112878558,-4.94597286168509,0.000644103793583921));
#78060=CARTESIAN_POINT('Ctrl Pts',(38.0372105648425,-4.94504990619645,-0.865885476849175));
#78061=CARTESIAN_POINT('Ctrl Pts',(38.0580098418292,-4.72867855578625,-1.73287776724594));
#78062=CARTESIAN_POINT('Ctrl Pts',(38.0788091188158,-4.29962613932685,-2.47739280425836));
#78063=CARTESIAN_POINT('Ctrl Pts',(38.1185644429549,-3.47954388839537,-3.90044403059553));
#78064=CARTESIAN_POINT('Ctrl Pts',(38.1583197670939,-1.88245818408785,-4.87604005742951));
#78065=CARTESIAN_POINT('Ctrl Pts',(38.198075091233,-0.242270107226094,-4.95628059882961));
#78066=CARTESIAN_POINT('Ctrl Pts',(38.237830415372,1.39791796963594,-5.03652114022972));
#78067=CARTESIAN_POINT('Ctrl Pts',(38.2775857395111,3.08120841905215,-4.22140619619581));
#78068=CARTESIAN_POINT('Ctrl Pts',(38.3173410636502,4.0366108551339,-2.8852749666459));
#78069=CARTESIAN_POINT('Ctrl Pts',(38.3570963877892,4.99201329121554,-1.54914373709615));
#78070=CARTESIAN_POINT('Ctrl Pts',(38.3968517119283,5.21952771396271,0.308003777969546));
#78071=CARTESIAN_POINT('Ctrl Pts',(38.4366070360673,4.61159128103222,1.83414238846176));
#78072=CARTESIAN_POINT('Ctrl Pts',(38.4730713573782,4.05398069912805,3.23394505296223));
#78073=CARTESIAN_POINT('Ctrl Pts',(38.5095356786891,2.79351375556776,4.3552732712842));
#78074=CARTESIAN_POINT('Ctrl Pts',(38.546,1.34632304271355,4.77431539461067));
#78075=CARTESIAN_POINT('',(-17.6184,-2.62535040627153,-3.68399909158375));
#78076=CARTESIAN_POINT('Ctrl Pts',(-17.6184,-2.63197694108733,-3.68657593761835));
#78077=CARTESIAN_POINT('Ctrl Pts',(-17.6184,-2.73716117210554,-3.61958470141671));
#78078=CARTESIAN_POINT('Ctrl Pts',(-17.6184,-2.83916784935626,-3.54816356962529));
#78079=CARTESIAN_POINT('Ctrl Pts',(-17.6184,-2.93765889762381,-3.47237117351613));
#78080=CARTESIAN_POINT('Ctrl Pts',(-17.6184,-3.0439083914269,-3.39060837514641));
#78081=CARTESIAN_POINT('Ctrl Pts',(-17.6184,-3.14606771222116,-3.30375913852623));
#78082=CARTESIAN_POINT('Ctrl Pts',(-17.6184,-3.24404505736733,-3.21224748954631));
#78083=CARTESIAN_POINT('Ctrl Pts',(-17.6184,-3.30825262600525,-3.15227709052925));
#78084=CARTESIAN_POINT('Ctrl Pts',(-17.6184,-3.37066364900808,-3.09030339612478));
#78085=CARTESIAN_POINT('Ctrl Pts',(-17.6184,-3.43124502544207,-3.02643626197717));
#78086=CARTESIAN_POINT('Ctrl Pts',(-17.6184,-3.45627312892573,-3.00005070693135));
#78087=CARTESIAN_POINT('Ctrl Pts',(-17.6184,-3.4809888798162,-2.97334190334144));
#78088=CARTESIAN_POINT('Ctrl Pts',(-17.6184,-3.50538962958215,-2.94631727874148));
#78089=CARTESIAN_POINT('Ctrl Pts',(-17.6184,-3.52549305907404,-2.92405207622101));
#78090=CARTESIAN_POINT('Ctrl Pts',(-17.6184,-3.54538564420158,-2.90156890295012));
#78091=CARTESIAN_POINT('Ctrl Pts',(-17.6184,-3.56504672982455,-2.87889429908813));
#78092=CARTESIAN_POINT('Ctrl Pts',(-17.6184,-3.65439596746517,-2.77585021455875));
#78093=CARTESIAN_POINT('Ctrl Pts',(-17.6184,-3.7390390925291,-2.66877877171196));
#78094=CARTESIAN_POINT('Ctrl Pts',(-17.6184,-3.81888410590975,-2.55811744250654));
#78095=CARTESIAN_POINT('Ctrl Pts',(-17.6184,-3.90082700708385,-2.44454854222162));
#78096=CARTESIAN_POINT('Ctrl Pts',(-17.6184,-3.97771685155179,-2.32719808251997));
#78097=CARTESIAN_POINT('Ctrl Pts',(-17.6184,-4.04941690653803,-2.20649857516439));
#78098=CARTESIAN_POINT('Ctrl Pts',(-17.6184,-4.08078568059451,-2.15369254069632));
#78099=CARTESIAN_POINT('Ctrl Pts',(-17.6184,-4.11116057774341,-2.10024501648371));
#78100=CARTESIAN_POINT('Ctrl Pts',(-17.6184,-4.14052760413295,-2.04619031750335));
#78101=CARTESIAN_POINT('Ctrl Pts',(-17.6184,-4.16412477109697,-2.00275596565207));
#78102=CARTESIAN_POINT('Ctrl Pts',(-17.6184,-4.18707117346303,-1.95892956580614));
#78103=CARTESIAN_POINT('Ctrl Pts',(-17.6184,-4.20935877075171,-1.91472849022619));
#78104=CARTESIAN_POINT('Ctrl Pts',(-17.6184,-4.21851295458813,-1.8965737844324));
#78105=CARTESIAN_POINT('Ctrl Pts',(-17.6184,-4.22755205088212,-1.87836365074964));
#78106=CARTESIAN_POINT('Ctrl Pts',(-17.6184,-4.23647441528938,-1.86010226714326));
#78107=CARTESIAN_POINT('Ctrl Pts',(-17.6184,-4.29849811267229,-1.73315850213925));
#78108=CARTESIAN_POINT('Ctrl Pts',(-17.6184,-4.35490596821788,-1.60369781509999));
#78109=CARTESIAN_POINT('Ctrl Pts',(-17.6184,-4.4055941948389,-1.47217017248125));
#78110=CARTESIAN_POINT('Ctrl Pts',(-17.6184,-4.45675075636739,-1.33942727751611));
#78111=CARTESIAN_POINT('Ctrl Pts',(-17.6184,-4.50208192177669,-1.204578337258));
#78112=CARTESIAN_POINT('Ctrl Pts',(-17.6184,-4.54143888287325,-1.06805365986625));
#78113=CARTESIAN_POINT('Ctrl Pts',(-17.6184,-4.58077531682645,-0.931600188724784));
#78114=CARTESIAN_POINT('Ctrl Pts',(-17.6184,-4.61414414231629,-0.793471953457049));
#78115=CARTESIAN_POINT('Ctrl Pts',(-17.6184,-4.64134914051464,-0.654077827943033));
#78116=CARTESIAN_POINT('Ctrl Pts',(-17.6184,-4.66175288916341,-0.54953223380752));
#78117=CARTESIAN_POINT('Ctrl Pts',(-17.6184,-4.6786885469106,-0.444274077934729));
#78118=CARTESIAN_POINT('Ctrl Pts',(-17.6184,-4.69205381237269,-0.338472159449352));
#78119=CARTESIAN_POINT('Ctrl Pts',(-17.6184,-4.69780146049362,-0.292972711668202));
#78120=CARTESIAN_POINT('Ctrl Pts',(-17.6184,-4.70288858877598,-0.247372681820807));
#78121=CARTESIAN_POINT('Ctrl Pts',(-17.6184,-4.70730603495934,-0.201685461789799));
#78122=CARTESIAN_POINT('Ctrl Pts',(-17.6184,-4.70953517448911,-0.178630695766913));
#78123=CARTESIAN_POINT('Ctrl Pts',(-17.6184,-4.71159393181158,-0.155550821171334));
#78124=CARTESIAN_POINT('Ctrl Pts',(-17.6184,-4.71347929372106,-0.132472198343172));
#78125=CARTESIAN_POINT('Ctrl Pts',(-17.6184,-4.72517039895951,0.0106380484937822));
#78126=CARTESIAN_POINT('Ctrl Pts',(-17.6184,-4.73021838483544,0.153891258577337));
#78127=CARTESIAN_POINT('Ctrl Pts',(-17.6184,-4.72847670664429,0.29686064475732));
#78128=CARTESIAN_POINT('Ctrl Pts',(-17.6184,-4.7271730108818,0.403877304824889));
#78129=CARTESIAN_POINT('Ctrl Pts',(-17.6184,-4.72206419852149,0.510735518131823));
#78130=CARTESIAN_POINT('Ctrl Pts',(-17.6184,-4.71307035555621,0.617261392298407));
#78131=CARTESIAN_POINT('Ctrl Pts',(-17.6184,-4.70132235933636,0.756408314460109));
#78132=CARTESIAN_POINT('Ctrl Pts',(-17.6184,-4.68294770909115,0.894988563534377));
#78133=CARTESIAN_POINT('Ctrl Pts',(-17.6184,-4.65822406848993,1.03262123260427));
#78134=CARTESIAN_POINT('Ctrl Pts',(-17.6184,-4.63316934564393,1.17209698513291));
#78135=CARTESIAN_POINT('Ctrl Pts',(-17.6184,-4.60159422545019,1.31060035998519));
#78136=CARTESIAN_POINT('Ctrl Pts',(-17.6184,-4.56373468707362,1.44772796830018));
#78137=CARTESIAN_POINT('Ctrl Pts',(-17.6184,-4.55297010560545,1.48671738482605));
#78138=CARTESIAN_POINT('Ctrl Pts',(-17.6184,-4.54169715893265,1.52559549794463));
#78139=CARTESIAN_POINT('Ctrl Pts',(-17.6184,-4.52992054380946,1.56435280087288));
#78140=CARTESIAN_POINT('Ctrl Pts',(-17.6184,-4.52310938075615,1.58676860600784));
#78141=CARTESIAN_POINT('Ctrl Pts',(-17.6184,-4.51612973269326,1.60914399728935));
#78142=CARTESIAN_POINT('Ctrl Pts',(-17.6184,-4.50898246146665,1.63147711431087));
#78143=CARTESIAN_POINT('Ctrl Pts',(-17.6184,-4.50302481877714,1.6500929926144));
#78144=CARTESIAN_POINT('Ctrl Pts',(-17.6184,-4.49695039804118,1.66868024935221));
#78145=CARTESIAN_POINT('Ctrl Pts',(-17.6184,-4.49076502234239,1.68722232347077));
#78146=CARTESIAN_POINT('Ctrl Pts',(-17.6184,-4.44573327332057,1.82221525982782));
#78147=CARTESIAN_POINT('Ctrl Pts',(-17.6184,-4.39476378955444,1.95500777029891));
#78148=CARTESIAN_POINT('Ctrl Pts',(-17.6184,-4.3381737036556,2.08521764827832));
#78149=CARTESIAN_POINT('Ctrl Pts',(-17.6184,-4.2796106428686,2.21996720516727));
#78150=CARTESIAN_POINT('Ctrl Pts',(-17.6184,-4.2150281457401,2.35195174008015));
#78151=CARTESIAN_POINT('Ctrl Pts',(-17.6184,-4.14472053045541,2.48074070343891));
#78152=CARTESIAN_POINT('Ctrl Pts',(-17.6184,-4.07441291517072,2.60952966679768));
#78153=CARTESIAN_POINT('Ctrl Pts',(-17.6184,-3.9983797687207,2.73512390207661));
#78154=CARTESIAN_POINT('Ctrl Pts',(-17.6184,-3.91686351059182,2.85707332817252));
#78155=CARTESIAN_POINT('Ctrl Pts',(-17.6184,-3.8601159990715,2.94196837391093));
#78156=CARTESIAN_POINT('Ctrl Pts',(-17.6184,-3.80071014382092,3.02509662626796));
#78157=CARTESIAN_POINT('Ctrl Pts',(-17.6184,-3.73873295306836,3.10635975427808));
#78158=CARTESIAN_POINT('Ctrl Pts',(-17.6184,-3.71153664712141,3.14201895187533));
#78159=CARTESIAN_POINT('Ctrl Pts',(-17.6184,-3.68384508470585,3.17731890463176));
#78160=CARTESIAN_POINT('Ctrl Pts',(-17.6184,-3.65566502692804,3.21225077861425));
#78161=CARTESIAN_POINT('Ctrl Pts',(-17.6184,-3.63992931102603,3.23175670188976));
#78162=CARTESIAN_POINT('Ctrl Pts',(-17.6184,-3.62404127145717,3.25114784869207));
#78163=CARTESIAN_POINT('Ctrl Pts',(-17.6184,-3.60800203978635,3.2704226332339));
#78164=CARTESIAN_POINT('Ctrl Pts',(-17.6184,-3.59510956928472,3.28591586858525));
#78165=CARTESIAN_POINT('Ctrl Pts',(-17.6184,-3.58211862855319,3.30133475112244));
#78166=CARTESIAN_POINT('Ctrl Pts',(-17.6184,-3.56904120736592,3.31666531967021));
#78167=CARTESIAN_POINT('Ctrl Pts',(-17.6184,-3.47465808930856,3.4273099827433));
#78168=CARTESIAN_POINT('Ctrl Pts',(-17.6184,-3.37564227864469,3.53351659865466));
#78169=CARTESIAN_POINT('Ctrl Pts',(-17.6184,-3.27231843400203,3.63505679843972));
#78170=CARTESIAN_POINT('Ctrl Pts',(-17.6184,-3.16806457753583,3.73751095556628));
#78171=CARTESIAN_POINT('Ctrl Pts',(-17.6184,-3.05942437423569,3.83521489577629));
#78172=CARTESIAN_POINT('Ctrl Pts',(-17.6184,-2.94668631586489,3.92790671043383));
#78173=CARTESIAN_POINT('Ctrl Pts',(-17.6184,-2.83436660052935,4.02025456870566));
#78174=CARTESIAN_POINT('Ctrl Pts',(-17.6184,-2.717978894366,4.10762796058369));
#78175=CARTESIAN_POINT('Ctrl Pts',(-17.6184,-2.59777092570975,4.18973263300831));
#78176=CARTESIAN_POINT('Ctrl Pts',(-17.6184,-2.47949248010661,4.2705193989748));
#78177=CARTESIAN_POINT('Ctrl Pts',(-17.6184,-2.35751491506182,4.34620565556445));
#78178=CARTESIAN_POINT('Ctrl Pts',(-17.6184,-2.23204533204169,4.41646995878763));
#78179=CARTESIAN_POINT('Ctrl Pts',(-17.6184,-2.19381761648338,4.43787788677195));
#78180=CARTESIAN_POINT('Ctrl Pts',(-17.6184,-2.15526556691906,4.45878218778325));
#78181=CARTESIAN_POINT('Ctrl Pts',(-17.6184,-2.11639460593215,4.47917290043388));
#78182=CARTESIAN_POINT('Ctrl Pts',(-17.6184,-2.63197694108751,-3.68657593761822));
#78183=CARTESIAN_POINT('Ctrl Pts',(-17.5819356786891,-1.50670517901651,
-4.47812843616949));
#78184=CARTESIAN_POINT('Ctrl Pts',(-17.5057160332392,1.66816188487742,-5.01601419576036));
#78185=CARTESIAN_POINT('Ctrl Pts',(-17.3897410636502,5.14844039432527,-1.44815814548532));
#78186=CARTESIAN_POINT('Ctrl Pts',(-17.270475091233,4.00553813139823,3.54623540470151));
#78187=CARTESIAN_POINT('Ctrl Pts',(-17.1512091188158,-0.816602122674766,
5.28738771244033));
#78188=CARTESIAN_POINT('Ctrl Pts',(-17.0550486435592,-4.09920106397465,
2.77690491316815));
#78189=CARTESIAN_POINT('Ctrl Pts',(-16.9986434924416,-4.51947609461455,
0.635058848558144));
#78190=CARTESIAN_POINT('Ctrl Pts',(-16.9819936654631,-4.51703452062264,
0.00191132365274384));
#78191=CARTESIAN_POINT('Origin',(-17.6184,-1.12989188470299E-15,0.));
#78192=CARTESIAN_POINT('',(-17.6184,-4.954,-6.06690024297599E-16));
#78193=CARTESIAN_POINT('Origin',(-17.6184,0.,0.));
#78194=CARTESIAN_POINT('Origin',(-17.6184,0.,0.));
#78195=CARTESIAN_POINT('',(-17.6184,2.62535040627109,-3.68399909158407));
#78196=CARTESIAN_POINT('Ctrl Pts',(-17.6184,2.12303769703984,4.48323345254434));
#78197=CARTESIAN_POINT('Ctrl Pts',(-17.6184,2.24381940709171,4.4207770582956));
#78198=CARTESIAN_POINT('Ctrl Pts',(-17.6184,2.36160609121881,4.35319682073143));
#78199=CARTESIAN_POINT('Ctrl Pts',(-17.6184,2.4760271263133,4.28047879555117));
#78200=CARTESIAN_POINT('Ctrl Pts',(-17.6184,2.59817096823974,4.20285269327472));
#78201=CARTESIAN_POINT('Ctrl Pts',(-17.6184,2.71648030536387,4.11937188811111));
#78202=CARTESIAN_POINT('Ctrl Pts',(-17.6184,2.83077226006603,4.0304564910319));
#78203=CARTESIAN_POINT('Ctrl Pts',(-17.6184,2.90276609647662,3.97444764449161));
#78204=CARTESIAN_POINT('Ctrl Pts',(-17.6184,2.9731652237438,3.91628154560514));
#78205=CARTESIAN_POINT('Ctrl Pts',(-17.6184,3.04191642491439,3.85605590927701));
#78206=CARTESIAN_POINT('Ctrl Pts',(-17.6184,3.0824756587865,3.8205262657604));
#78207=CARTESIAN_POINT('Ctrl Pts',(-17.6184,3.12246124783005,3.78427974006281));
#78208=CARTESIAN_POINT('Ctrl Pts',(-17.6184,3.16186122468888,3.74733565762945));
#78209=CARTESIAN_POINT('Ctrl Pts',(-17.6184,3.17680182420591,3.73332634127531));
#78210=CARTESIAN_POINT('Ctrl Pts',(-17.6184,3.19165673930132,3.71921803818185));
#78211=CARTESIAN_POINT('Ctrl Pts',(-17.6184,3.20641884358392,3.70501824795818));
#78212=CARTESIAN_POINT('Ctrl Pts',(-17.6184,3.31072331864878,3.60468691057177));
#78213=CARTESIAN_POINT('Ctrl Pts',(-17.6184,3.41049168111438,3.49970317250891));
#78214=CARTESIAN_POINT('Ctrl Pts',(-17.6184,3.50554675464997,3.39048828312545));
#78215=CARTESIAN_POINT('Ctrl Pts',(-17.6184,3.60030478700596,3.28161468346346));
#78216=CARTESIAN_POINT('Ctrl Pts',(-17.6184,3.69037927330835,3.16853559672437));
#78217=CARTESIAN_POINT('Ctrl Pts',(-17.6184,3.77555511792418,3.05163746945272));
#78218=CARTESIAN_POINT('Ctrl Pts',(-17.6184,3.81405934856761,2.99879299841104));
#78219=CARTESIAN_POINT('Ctrl Pts',(-17.6184,3.85156195266768,2.94516773799131));
#78220=CARTESIAN_POINT('Ctrl Pts',(-17.6184,3.88804011199047,2.89079592116327));
#78221=CARTESIAN_POINT('Ctrl Pts',(-17.6184,3.90826393821039,2.86065168704605));
#78222=CARTESIAN_POINT('Ctrl Pts',(-17.6184,3.92817284751982,2.83027797047312));
#78223=CARTESIAN_POINT('Ctrl Pts',(-17.6184,3.94776269178357,2.79968051659357));
#78224=CARTESIAN_POINT('Ctrl Pts',(-17.6184,3.95882030543706,2.78240958685949));
#78225=CARTESIAN_POINT('Ctrl Pts',(-17.6184,3.96977625803069,2.76506737090552));
#78226=CARTESIAN_POINT('Ctrl Pts',(-17.6184,3.98062977664469,2.74765489470299));
#78227=CARTESIAN_POINT('Ctrl Pts',(-17.6184,3.99133694893152,2.73047720429022));
#78228=CARTESIAN_POINT('Ctrl Pts',(-17.6184,4.00193956608098,2.71323892588693));
#78229=CARTESIAN_POINT('Ctrl Pts',(-17.6184,4.0124361625168,2.69594287926482));
#78230=CARTESIAN_POINT('Ctrl Pts',(-17.6184,4.08795407340856,2.57150622824435));
#78231=CARTESIAN_POINT('Ctrl Pts',(-17.6184,4.15800542572808,2.44405359890784));
#78232=CARTESIAN_POINT('Ctrl Pts',(-17.6184,4.22240808518171,2.31399496854479));
#78233=CARTESIAN_POINT('Ctrl Pts',(-17.6184,4.28677631677449,2.18400586388871));
#78234=CARTESIAN_POINT('Ctrl Pts',(-17.6184,4.34550224287882,2.05141278203371));
#78235=CARTESIAN_POINT('Ctrl Pts',(-17.6184,4.39835791748156,1.91660140410854));
#78236=CARTESIAN_POINT('Ctrl Pts',(-17.6184,4.45114294408316,1.78197021789321));
#78237=CARTESIAN_POINT('Ctrl Pts',(-17.6184,4.49807375121929,1.64512592017646));
#78238=CARTESIAN_POINT('Ctrl Pts',(-17.6184,4.53887208607825,1.50644031813667));
#78239=CARTESIAN_POINT('Ctrl Pts',(-17.6184,4.56947083722247,1.40242611660682));
#78240=CARTESIAN_POINT('Ctrl Pts',(-17.6184,4.59661905930676,1.29737586205953));
#78241=CARTESIAN_POINT('Ctrl Pts',(-17.6184,4.62017859187827,1.191445622251));
#78242=CARTESIAN_POINT('Ctrl Pts',(-17.6184,4.62970711520508,1.148602719576));
#78243=CARTESIAN_POINT('Ctrl Pts',(-17.6184,4.63864840540407,1.10561588280141));
#78244=CARTESIAN_POINT('Ctrl Pts',(-17.6184,4.64699243736825,1.06249551694592));
#78245=CARTESIAN_POINT('Ctrl Pts',(-17.6184,4.65040106524143,1.04488037817516));
#78246=CARTESIAN_POINT('Ctrl Pts',(-17.6184,4.65371013823636,1.02724228268309));
#78247=CARTESIAN_POINT('Ctrl Pts',(-17.6184,4.65691857348069,1.00958400498525));
#78248=CARTESIAN_POINT('Ctrl Pts',(-17.6184,4.68219783989241,0.87045440681626));
#78249=CARTESIAN_POINT('Ctrl Pts',(-17.6184,4.70113960444395,0.730593445780796));
#78250=CARTESIAN_POINT('Ctrl Pts',(-17.6184,4.71353612598034,0.59035734446077));
#78251=CARTESIAN_POINT('Ctrl Pts',(-17.6184,4.72428327942915,0.468779779695929));
#78252=CARTESIAN_POINT('Ctrl Pts',(-17.6184,4.73011040694146,0.346919744006319));
#78253=CARTESIAN_POINT('Ctrl Pts',(-17.6184,4.73085060001627,0.225005660692869));
#78254=CARTESIAN_POINT('Ctrl Pts',(-17.6184,4.73170563360439,0.0841766801921896));
#78255=CARTESIAN_POINT('Ctrl Pts',(-17.6184,4.72577375269981,-0.0567251366648641));
#78256=CARTESIAN_POINT('Ctrl Pts',(-17.6184,4.71325836366559,-0.197256136884384));
#78257=CARTESIAN_POINT('Ctrl Pts',(-17.6184,4.70068788818754,-0.338405683840902));
#78258=CARTESIAN_POINT('Ctrl Pts',(-17.6184,4.68147549611962,-0.479181965102924));
#78259=CARTESIAN_POINT('Ctrl Pts',(-17.6184,4.65577743932771,-0.619119634047808));
#78260=CARTESIAN_POINT('Ctrl Pts',(-17.6184,4.64747570444936,-0.664326376194986));
#78261=CARTESIAN_POINT('Ctrl Pts',(-17.6184,4.6384967543993,-0.709445425498875));
#78262=CARTESIAN_POINT('Ctrl Pts',(-17.6184,4.62884483854091,-0.754460522413662));
#78263=CARTESIAN_POINT('Ctrl Pts',(-17.6184,4.62503524587868,-0.772227894758371));
#78264=CARTESIAN_POINT('Ctrl Pts',(-17.6184,4.62112080895723,-0.789979069125397));
#78265=CARTESIAN_POINT('Ctrl Pts',(-17.6184,4.61710176889132,-0.807713031086456));
#78266=CARTESIAN_POINT('Ctrl Pts',(-17.6184,4.61286384600412,-0.826412810646483));
#78267=CARTESIAN_POINT('Ctrl Pts',(-17.6184,4.60851138104239,-0.845085572518443));
#78268=CARTESIAN_POINT('Ctrl Pts',(-17.6184,4.60404615614281,-0.863725337721086));
#78269=CARTESIAN_POINT('Ctrl Pts',(-17.6184,4.57140957603825,-0.99996443067781));
#78270=CARTESIAN_POINT('Ctrl Pts',(-17.6184,4.5327344910388,-1.1345251091489));
#78271=CARTESIAN_POINT('Ctrl Pts',(-17.6184,4.48825308683246,-1.26698550606458));
#78272=CARTESIAN_POINT('Ctrl Pts',(-17.6184,4.4435856042334,-1.40000002257693));
#78273=CARTESIAN_POINT('Ctrl Pts',(-17.6184,4.39306276857063,-1.53089744915004));
#78274=CARTESIAN_POINT('Ctrl Pts',(-17.6184,4.33686983674132,-1.65923491503709));
#78275=CARTESIAN_POINT('Ctrl Pts',(-17.6184,4.2828641903748,-1.78257690081076));
#78276=CARTESIAN_POINT('Ctrl Pts',(-17.6184,4.22362068596107,-1.90355486374681));
#78277=CARTESIAN_POINT('Ctrl Pts',(-17.6184,4.15926519043502,-2.02175178363005));
#78278=CARTESIAN_POINT('Ctrl Pts',(-17.6184,4.11365597924993,-2.10551880673066));
#78279=CARTESIAN_POINT('Ctrl Pts',(-17.6184,4.06547835815844,-2.18788846192158));
#78280=CARTESIAN_POINT('Ctrl Pts',(-17.6184,4.01479316151161,-2.26875477322379));
#78281=CARTESIAN_POINT('Ctrl Pts',(-17.6184,3.99105024278133,-2.30663570067969));
#78282=CARTESIAN_POINT('Ctrl Pts',(-17.6184,3.96675696552567,-2.34418662407999));
#78283=CARTESIAN_POINT('Ctrl Pts',(-17.6184,3.94191903989479,-2.38139598871097));
#78284=CARTESIAN_POINT('Ctrl Pts',(-17.6184,3.92720191601446,-2.40344351542156));
#78285=CARTESIAN_POINT('Ctrl Pts',(-17.6184,3.91229356663274,-2.42537111682055));
#78286=CARTESIAN_POINT('Ctrl Pts',(-17.6184,3.89719512685908,-2.4471763135535));
#78287=CARTESIAN_POINT('Ctrl Pts',(-17.6184,3.88793571226168,-2.46054877852041));
#78288=CARTESIAN_POINT('Ctrl Pts',(-17.6184,3.87860551837951,-2.47387411422051));
#78289=CARTESIAN_POINT('Ctrl Pts',(-17.6184,3.86921058723167,-2.48714381222199));
#78290=CARTESIAN_POINT('Ctrl Pts',(-17.6184,3.78526556952311,-2.60571041118819));
#78291=CARTESIAN_POINT('Ctrl Pts',(-17.6184,3.69603451419748,-2.72001500601706));
#78292=CARTESIAN_POINT('Ctrl Pts',(-17.6184,3.6018119705952,-2.82974803590307));
#78293=CARTESIAN_POINT('Ctrl Pts',(-17.6184,3.51211118207048,-2.93421495997094));
#78294=CARTESIAN_POINT('Ctrl Pts',(-17.6184,3.41788563088132,-3.03453885711949));
#78295=CARTESIAN_POINT('Ctrl Pts',(-17.6184,3.31934941853852,-3.13041809444619));
#78296=CARTESIAN_POINT('Ctrl Pts',(-17.6184,3.22168601847118,-3.22544805440257));
#78297=CARTESIAN_POINT('Ctrl Pts',(-17.6184,3.11978748274982,-3.31611220668362));
#78298=CARTESIAN_POINT('Ctrl Pts',(-17.6184,3.01383146888639,-3.40207631807092));
#78299=CARTESIAN_POINT('Ctrl Pts',(-17.6184,2.90999389424987,-3.48632169977948));
#78300=CARTESIAN_POINT('Ctrl Pts',(-17.6184,2.8022589807078,-3.56605343912507));
#78301=CARTESIAN_POINT('Ctrl Pts',(-17.6184,2.69077155688435,-3.6409121095589));
#78302=CARTESIAN_POINT('Ctrl Pts',(-17.6184,2.66910594838121,-3.65545956783772));
#78303=CARTESIAN_POINT('Ctrl Pts',(-17.6184,2.64729856962228,-3.66982284730888));
#78304=CARTESIAN_POINT('Ctrl Pts',(-17.6184,2.62535040627071,-3.68399909158434));
#78305=CARTESIAN_POINT('Origin',(-17.6184,0.,0.));
#78306=CARTESIAN_POINT('Origin',(-19.0048063345371,0.,0.));
#78307=CARTESIAN_POINT('Ctrl Pts',(-17.6184,2.62535040627071,-3.68399909158434));
#78308=CARTESIAN_POINT('Ctrl Pts',(-17.5985223379305,3.23883466326236,-3.24680811968291));
#78309=CARTESIAN_POINT('Ctrl Pts',(-17.5587670137914,4.23254591953354,-2.06184536971571));
#78310=CARTESIAN_POINT('Ctrl Pts',(-17.4792563655133,4.8909587174436,0.989874372427294));
#78311=CARTESIAN_POINT('Ctrl Pts',(-17.3798680551657,2.68243561037911,4.62805141939821));
#78312=CARTESIAN_POINT('Ctrl Pts',(-17.2606020827485,-2.44949610129593,
4.7591308229798));
#78313=CARTESIAN_POINT('Ctrl Pts',(-17.1772481758723,-4.45802737904165,
1.79294945179082));
#78314=CARTESIAN_POINT('Ctrl Pts',(-17.1336495931351,-4.53003253390568,
0.147368644500374));
#78315=CARTESIAN_POINT('Ctrl Pts',(-17.129806334537,-4.52905226269683,0.0022285783852446));
#78316=CARTESIAN_POINT('Ctrl Pts',(-17.8668049533188,2.87504524181639,-4.03438109968666));
#78317=CARTESIAN_POINT('Ctrl Pts',(-17.8469272912493,3.54687746268103,-3.55560926773309));
#78318=CARTESIAN_POINT('Ctrl Pts',(-17.8071719671102,4.63509974807851,-2.25794572236962));
#78319=CARTESIAN_POINT('Ctrl Pts',(-17.7276613188321,5.35613362502683,1.0840204788079));
#78320=CARTESIAN_POINT('Ctrl Pts',(-17.6282730084845,2.93755977094575,5.06822143834209));
#78321=CARTESIAN_POINT('Ctrl Pts',(-17.5090070360674,-2.68246558404474,
5.21176769207864));
#78322=CARTESIAN_POINT('Ctrl Pts',(-17.3897410636502,-5.82968193086184,
0.563986199967765));
#78323=CARTESIAN_POINT('Ctrl Pts',(-17.270475091233,-3.63071138506581,-4.59793593777515));
#78324=CARTESIAN_POINT('Ctrl Pts',(-17.1512091188158,1.90400000504956,-5.54091032617354));
#78325=CARTESIAN_POINT('Ctrl Pts',(-17.0319431463987,5.68939374674768,-1.39643871054889));
#78326=CARTESIAN_POINT('Ctrl Pts',(-16.9126771739815,4.25280175532545,4.02941979983046));
#78327=CARTESIAN_POINT('Ctrl Pts',(-16.7934112015644,-1.08819795636646,
5.75661471108102));
#78328=CARTESIAN_POINT('Ctrl Pts',(-16.6741452291472,-5.43003511364721,
2.19919371409573));
#78329=CARTESIAN_POINT('Ctrl Pts',(-16.55487925673,-4.78730836808999,-3.37697293683734));
#78330=CARTESIAN_POINT('Ctrl Pts',(-16.4356132843129,0.250143793580362,
-5.85317724934502));
#78331=CARTESIAN_POINT('Ctrl Pts',(-16.3163473118957,5.05793681468126,-2.95624591066989));
#78332=CARTESIAN_POINT('Ctrl Pts',(-16.1970813394786,5.2226486393331,2.65445654805712));
#78333=CARTESIAN_POINT('Ctrl Pts',(-16.0778153670614,0.593051366503517,
5.82842001816422));
#78334=CARTESIAN_POINT('Ctrl Pts',(-15.9585493946442,-4.58095211955662,
3.65199249477323));
#78335=CARTESIAN_POINT('Ctrl Pts',(-15.839283422227,-5.54972387549991,-1.87689883035945));
#78336=CARTESIAN_POINT('Ctrl Pts',(-15.7200174498099,-1.42394462969,-5.68283061407078));
#78337=CARTESIAN_POINT('Ctrl Pts',(-15.6007514773927,4.00899028053514,-4.27202255834164));
#78338=CARTESIAN_POINT('Ctrl Pts',(-15.4814855049755,5.76174238590305,1.06042746340526));
#78339=CARTESIAN_POINT('Ctrl Pts',(-15.3622195325584,2.22531528333639,5.41942369241641));
#78340=CARTESIAN_POINT('Ctrl Pts',(-15.2429535601412,-3.35391234047839,
4.80348342455471));
#78341=CARTESIAN_POINT('Ctrl Pts',(-15.1236875877241,-5.85430698164175,
-0.221970816878097));
#78342=CARTESIAN_POINT('Ctrl Pts',(-15.0044216153069,-2.98054988927022,
-5.04365973784862));
#78343=CARTESIAN_POINT('Ctrl Pts',(-14.8851556428897,2.62930000449966,-5.23535697450904));
#78344=CARTESIAN_POINT('Ctrl Pts',(-14.7658896704726,5.82549835830257,-0.621087821490262));
#78345=CARTESIAN_POINT('Ctrl Pts',(-14.6466236980554,3.67399081555006,4.56332912214217));
#78346=CARTESIAN_POINT('Ctrl Pts',(-14.5273577256382,-1.85017621709516,
5.55868951756596));
#78347=CARTESIAN_POINT('Ctrl Pts',(-14.4080917532211,-5.67591375177504,
1.45126988361524));
#78348=CARTESIAN_POINT('Ctrl Pts',(-14.2888257808039,-4.29126145322842,
-3.98839019282699));
#78349=CARTESIAN_POINT('Ctrl Pts',(-14.1695598083868,1.03269401679673,-5.76677763206729));
#78350=CARTESIAN_POINT('Ctrl Pts',(-14.0502938359695,5.40865439039165,-2.25136378138128));
#78351=CARTESIAN_POINT('Ctrl Pts',(-13.9310278635524,4.81956436383399,3.33076275547831));
#78352=CARTESIAN_POINT('Ctrl Pts',(-13.8117618911352,-0.193801692465541,
5.85530717336233));
#78353=CARTESIAN_POINT('Ctrl Pts',(-13.6924959187181,-5.02926117512766,
3.0047817263303));
#78354=CARTESIAN_POINT('Ctrl Pts',(-13.5732299463009,-5.24794661246699,
-2.60408094021077));
#78355=CARTESIAN_POINT('Ctrl Pts',(-13.4539639738837,-0.649108587035416,
-5.8224427204324));
#78356=CARTESIAN_POINT('Ctrl Pts',(-13.3346980014666,4.5455998004388,-3.69590363033771));
#78357=CARTESIAN_POINT('Ctrl Pts',(-13.2154320290494,5.5675268492086,1.82341053354003));
#78358=CARTESIAN_POINT('Ctrl Pts',(-13.0961660566323,1.47856135155213,5.6688656290462));
#78359=CARTESIAN_POINT('Ctrl Pts',(-12.9769000842151,-3.96769767979603,
4.31040094564622));
#78360=CARTESIAN_POINT('Ctrl Pts',(-12.8576341117979,-5.77167944021737,
-1.00493662977195));
#78361=CARTESIAN_POINT('Ctrl Pts',(-12.7383681393807,-2.27736013621432,
-5.39775990578199));
#78362=CARTESIAN_POINT('Ctrl Pts',(-12.6191021669636,3.30753605425009,-4.83553372858896));
#78363=CARTESIAN_POINT('Ctrl Pts',(-12.4998361945464,5.85617183240789,0.165628076719709));
#78364=CARTESIAN_POINT('Ctrl Pts',(-12.3805702221293,3.02894400371043,5.01474619625683));
#78365=CARTESIAN_POINT('Ctrl Pts',(-12.2613042497121,-2.57880159371761,
5.26041476793657));
#78366=CARTESIAN_POINT('Ctrl Pts',(-12.1420382772949,-5.81925230402365,
0.677114327570302));
#78367=CARTESIAN_POINT('Ctrl Pts',(-12.0227723048778,-3.71773089063149,
-4.52776525620864));
#78368=CARTESIAN_POINT('Ctrl Pts',(-11.9035063324606,1.79660264081118,-5.57623530184263));
#78369=CARTESIAN_POINT('Ctrl Pts',(-11.7842403600434,5.66168628186157,-1.50581859341225));
#78370=CARTESIAN_POINT('Ctrl Pts',(-11.6649743876263,4.32944065950869,3.94691332135362));
#78371=CARTESIAN_POINT('Ctrl Pts',(-11.5457084152091,-0.977155980123466,
5.77644764375084));
#78372=CARTESIAN_POINT('Ctrl Pts',(-11.426442442792,-5.38674047221298,2.30330377404027));
#78373=CARTESIAN_POINT('Ctrl Pts',(-11.3071764703748,-4.85139115892997,
-3.28423278918257));
#78374=CARTESIAN_POINT('Ctrl Pts',(-11.1879104979576,0.137450626958296,
-5.85690093100732));
#78375=CARTESIAN_POINT('Ctrl Pts',(-11.0686445255404,5.00011513452361,-3.05303616617843));
#78376=CARTESIAN_POINT('Ctrl Pts',(-10.9493785531233,5.27276115372783,2.55346255234429));
#78377=CARTESIAN_POINT('Ctrl Pts',(-10.8301125807061,0.705104394058296,
5.81592718179702));
#78378=CARTESIAN_POINT('Ctrl Pts',(-10.710846608289,-4.5098259018956,3.73947209176336));
#78379=CARTESIAN_POINT('Ctrl Pts',(-10.5915806358718,-5.58481467409041,
-1.7697531597797));
#78380=CARTESIAN_POINT('Ctrl Pts',(-10.4723146634546,-1.53304097812696,
-5.65437587624569));
#78381=CARTESIAN_POINT('Ctrl Pts',(-10.3530486910375,3.92603759856465,-4.34838015416571));
#78382=CARTESIAN_POINT('Ctrl Pts',(-10.2337827186203,5.78108213232227,0.949352710972031));
#78383=CARTESIAN_POINT('Ctrl Pts',(-10.1145167462031,2.32919409429188,5.37559634474182));
#78384=CARTESIAN_POINT('Ctrl Pts',(-9.99525077378599,-3.26085349969837,
4.867136287797));
#78385=CARTESIAN_POINT('Ctrl Pts',(-9.8759848013688,-5.85749445228765,-0.109269995448056));
#78386=CARTESIAN_POINT('Ctrl Pts',(-9.75671882895166,-3.07705765603928,
-4.98536832860881));
#78387=CARTESIAN_POINT('Ctrl Pts',(-9.63745285653448,2.52806440264535,-5.28498548404467));
#78388=CARTESIAN_POINT('Ctrl Pts',(-9.51818688411733,5.81246743072405,-0.733078138575955));
#78389=CARTESIAN_POINT('Ctrl Pts',(-9.39892091170016,3.76112673046111,4.49178215276483));
#78390=CARTESIAN_POINT('Ctrl Pts',(-9.27965493928299,-1.74286271196533,
5.59326476735425));
#78391=CARTESIAN_POINT('Ctrl Pts',(-9.16038896686583,-5.64693458142209,
1.56022787554418));
#78392=CARTESIAN_POINT('Ctrl Pts',(-9.04112299444866,-4.36721899120011,
-3.90507099466665));
#78393=CARTESIAN_POINT('Ctrl Pts',(-8.9218570220315,0.921527465916119,-5.78558279865112));
#78394=CARTESIAN_POINT('Ctrl Pts',(-8.80259104961434,5.36432778133606,-2.35503049765218));
#78395=CARTESIAN_POINT('Ctrl Pts',(-8.68332507719717,4.88276875071711,3.23739872698841));
#78396=CARTESIAN_POINT('Ctrl Pts',(-8.56405910477999,-0.0810868345228415,
5.85795238250983));
#78397=CARTESIAN_POINT('Ctrl Pts',(-8.44479313236285,-4.97050611987588,
3.10100791723629));
#78398=CARTESIAN_POINT('Ctrl Pts',(-8.32552715994566,-5.29708747591468,
-2.5026077325449));
#78399=CARTESIAN_POINT('Ctrl Pts',(-8.20626118752852,-0.761034913578503,
-5.80887313089209));
#78400=CARTESIAN_POINT('Ctrl Pts',(-8.08699521511134,4.47363442649844,-3.7826943054566));
#78401=CARTESIAN_POINT('Ctrl Pts',(-7.96772924269418,5.60158538602889,1.71593191983633));
#78402=CARTESIAN_POINT('Ctrl Pts',(-7.84846327027702,1.5873786563333,5.63936256964411));
#78403=CARTESIAN_POINT('Ctrl Pts',(-7.72919729785985,-3.88401399500086,
4.38595673452477));
#78404=CARTESIAN_POINT('Ctrl Pts',(-7.6099313254427,-5.78994953855466,-0.893680889062952));
#78405=CARTESIAN_POINT('Ctrl Pts',(-7.49066535302551,-2.38081238605224,
-5.35293504284386));
#78406=CARTESIAN_POINT('Ctrl Pts',(-7.37139938060837,3.21386901399082,-4.89828818582527));
#78407=CARTESIAN_POINT('Ctrl Pts',(-7.25213340819118,5.85827471107363,0.0529017965749914));
#78408=CARTESIAN_POINT('Ctrl Pts',(-7.13286743577404,3.1248863953615,4.95552885235978));
#78409=CARTESIAN_POINT('Ctrl Pts',(-7.01360146335686,-2.47709313132159,
5.30906684919723));
#78410=CARTESIAN_POINT('Ctrl Pts',(-6.8943354909397,-5.80514436550315,0.788974071914089));
#78411=CARTESIAN_POINT('Ctrl Pts',(-6.77506951852254,-3.80417431749705,
-4.45538314318551));
#78412=CARTESIAN_POINT('Ctrl Pts',(-6.65580354610538,1.68896140679477,-5.6097763375061));
#78413=CARTESIAN_POINT('Ctrl Pts',(-6.5365375736882,5.63166001619102,-1.6144926919999));
#78414=CARTESIAN_POINT('Ctrl Pts',(-6.41727160127105,4.40459295039272,3.86286708700112));
#78415=CARTESIAN_POINT('Ctrl Pts',(-6.29800562885387,-0.865813625013472,
5.79418225095022));
#78416=CARTESIAN_POINT('Ctrl Pts',(-6.17873965643672,-5.3414183929878,2.40653916268516));
#78417=CARTESIAN_POINT('Ctrl Pts',(-6.05947368401955,-4.9136942338729,-3.19026490537854));
#78418=CARTESIAN_POINT('Ctrl Pts',(-5.94020771160238,0.0247155340402711,
-5.85846143051762));
#78419=CARTESIAN_POINT('Ctrl Pts',(-5.82094173918523,4.94043687275883,-3.14869253766872));
#78420=CARTESIAN_POINT('Ctrl Pts',(-5.70167576676805,5.32092332659016,2.45152118959525));
#78421=CARTESIAN_POINT('Ctrl Pts',(-5.58240979435089,0.816894966838531,
5.80128122087176));
#78422=CARTESIAN_POINT('Ctrl Pts',(-5.46314382193373,-4.43702872531231,
3.82556626935662));
#78423=CARTESIAN_POINT('Ctrl Pts',(-5.34387784951656,-5.61783743217928,
-1.66195179716236));
#78424=CARTESIAN_POINT('Ctrl Pts',(-5.2246118770994,-1.64156935489994,-5.62382709936382));
#78425=CARTESIAN_POINT('Ctrl Pts',(-5.10534590468224,3.84163076018247,-4.42312720740718));
#78426=CARTESIAN_POINT('Ctrl Pts',(-4.98607993226507,5.79828083785774,0.837926318847652));
#78427=CARTESIAN_POINT('Ctrl Pts',(-4.8668139598479,2.4322102320196,5.32977809835875));
#78428=CARTESIAN_POINT('Ctrl Pts',(-4.74754798743074,-3.16658694754665,
4.92898653823612));
#78429=CARTESIAN_POINT('Ctrl Pts',(-4.62828201501358,-5.85851253651964,
0.00347130061708939));
#78430=CARTESIAN_POINT('Ctrl Pts',(-4.50901604259641,-3.17242579308605,
-4.92523053042676));
#78431=CARTESIAN_POINT('Ctrl Pts',(-4.38975007017924,2.42589249931285,-5.33265663363612));
#78432=CARTESIAN_POINT('Ctrl Pts',(-4.27048409776208,5.79728378642323,-0.844796952030536));
#78433=CARTESIAN_POINT('Ctrl Pts',(-4.15121812534491,3.84686966584789,4.41857159775248));
#78434=CARTESIAN_POINT('Ctrl Pts',(-4.03195215292775,-1.63490371616564,
5.62576848344769));
#78435=CARTESIAN_POINT('Ctrl Pts',(-3.91268618051059,-5.61586400048129,
1.66860801825474));
#78436=CARTESIAN_POINT('Ctrl Pts',(-3.79342020809342,-4.44155907653154,
-3.82030550612983));
#78437=CARTESIAN_POINT('Ctrl Pts',(-3.67415423567626,0.810019616109184,
-5.80224520440182));
#78438=CARTESIAN_POINT('Ctrl Pts',(-3.55488826325909,5.31801442840983,-2.457824999814));
#78439=CARTESIAN_POINT('Ctrl Pts',(-3.43562229084193,4.94416474492404,3.14283568859967));
#78440=CARTESIAN_POINT('Ctrl Pts',(-3.31635631842476,0.0316580549198027,
5.85842802789658));
#78441=CARTESIAN_POINT('Ctrl Pts',(-3.1970903460076,-4.90991017736459,3.19608561222904));
#78442=CARTESIAN_POINT('Ctrl Pts',(-3.07782437359043,-5.34426649872899,
-2.4002076537351));
#78443=CARTESIAN_POINT('Ctrl Pts',(-2.95855840117328,-0.872679381606534,
-5.79315215469129));
#78444=CARTESIAN_POINT('Ctrl Pts',(-2.8392924287561,4.40001218775717,-3.8680840138335));
#78445=CARTESIAN_POINT('Ctrl Pts',(-2.72002645633894,5.63356930772102,1.60781778992187));
#78446=CARTESIAN_POINT('Ctrl Pts',(-2.60076048392178,1.69560805616505,5.6077709038756));
#78447=CARTESIAN_POINT('Ctrl Pts',(-2.48149451150461,-3.79889181848672,
4.45988813109932));
#78448=CARTESIAN_POINT('Ctrl Pts',(-2.36222853908745,-5.80607525881414,
-0.782094162791051));
#78449=CARTESIAN_POINT('Ctrl Pts',(-2.24296256667028,-2.48338287312981,
-5.30612765544998));
#78450=CARTESIAN_POINT('Ctrl Pts',(-2.12369659425312,3.11901167833903,-4.95922850258693));
#78451=CARTESIAN_POINT('Ctrl Pts',(-2.00443062183595,5.85820790660474,-0.0598440763921811));
#78452=CARTESIAN_POINT('Ctrl Pts',(-1.88516464941879,3.21967144741286,4.89447616821248));
#78453=CARTESIAN_POINT('Ctrl Pts',(-1.76589867700162,-2.37446724742266,
5.35575265312009));
#78454=CARTESIAN_POINT('Ctrl Pts',(-1.64663270458446,-5.78888642131629,
0.900541610135457));
#78455=CARTESIAN_POINT('Ctrl Pts',(-1.5273667321673,-3.88920882223712,-4.38135092494524));
#78456=CARTESIAN_POINT('Ctrl Pts',(-1.40810075975013,1.58069464542428,-5.64123972442342));
#78457=CARTESIAN_POINT('Ctrl Pts',(-1.28883478733297,5.59954799688826,-1.72256884362577));
#78458=CARTESIAN_POINT('Ctrl Pts',(-1.1695688149158,4.47811394682395,3.77739019294359));
#78459=CARTESIAN_POINT('Ctrl Pts',(-1.05030284249864,-0.754150605320021,
5.80977091243547));
#78460=CARTESIAN_POINT('Ctrl Pts',(-0.931036870081473,-5.29411805463789,
2.50888326034566));
#78461=CARTESIAN_POINT('Ctrl Pts',(-0.81177089766431,-4.97417746252431,
-3.09511546825006));
#78462=CARTESIAN_POINT('Ctrl Pts',(-0.692504925247144,-0.0880287125757489,
-5.85785217773957));
#78463=CARTESIAN_POINT('Ctrl Pts',(-0.573238952829979,4.87892886024161,
-3.24318275266551));
#78464=CARTESIAN_POINT('Ctrl Pts',(-0.453972980412814,5.36711483092438,
2.3486718762222));
#78465=CARTESIAN_POINT('Ctrl Pts',(-0.334707007995651,0.92838299265408,
5.78448668504272));
#78466=CARTESIAN_POINT('Ctrl Pts',(-0.215441035578486,-4.36258824129331,
3.91024360205536));
#78467=CARTESIAN_POINT('Ctrl Pts',(-0.0961750631613217,-5.6487795559977,
-1.55353491052762));
#78468=CARTESIAN_POINT('Ctrl Pts',(0.0230909092558439,-1.74948975654047,
-5.59119546986562));
#78469=CARTESIAN_POINT('Ctrl Pts',(0.142356881673008,3.75580112722664,-4.49623610180878));
#78470=CARTESIAN_POINT('Ctrl Pts',(0.261622854090171,5.81333207971762,0.726189590542047));
#78471=CARTESIAN_POINT('Ctrl Pts',(0.380888826507337,2.53432557117091,5.28198590397543));
#78472=CARTESIAN_POINT('Ctrl Pts',(0.500154798924501,-3.07114761148953,
4.98901127869317));
#78473=CARTESIAN_POINT('Ctrl Pts',(0.619420771341668,-5.85736084953548,
0.116211311043978));
#78474=CARTESIAN_POINT('Ctrl Pts',(0.738686743758829,-3.2666189837402,-4.86326861334576));
#78475=CARTESIAN_POINT('Ctrl Pts',(0.857952716175997,2.32282213725285,-5.37835276912677));
#78476=CARTESIAN_POINT('Ctrl Pts',(0.977218688593157,5.77995304771692,-0.956202884681618));
#78477=CARTESIAN_POINT('Ctrl Pts',(1.09648466101033,3.93118786636879,4.34372457112565));
#78478=CARTESIAN_POINT('Ctrl Pts',(1.21575063342749,-1.52633921393369,5.65618862790959));
#78479=CARTESIAN_POINT('Ctrl Pts',(1.33501660584466,-5.58271351615443,1.77637017173568));
#78480=CARTESIAN_POINT('Ctrl Pts',(1.45428257826181,-4.51425417655669,-3.73412512108611));
#78481=CARTESIAN_POINT('Ctrl Pts',(1.57354855067899,0.698211765707205,-5.81675867822566));
#78482=CARTESIAN_POINT('Ctrl Pts',(1.69281452309614,5.26973148430123,-2.55970921665918));
#78483=CARTESIAN_POINT('Ctrl Pts',(1.81208049551331,5.00372960771586,3.04710866287265));
#78484=CARTESIAN_POINT('Ctrl Pts',(1.93134646793048,0.144391219417513,5.85673393336599));
#78485=CARTESIAN_POINT('Ctrl Pts',(2.05061244034764,-4.84749579003301,3.28997959812789));
#78486=CARTESIAN_POINT('Ctrl Pts',(2.16987841276481,-5.38946620758809,-2.29691862889217));
#78487=CARTESIAN_POINT('Ctrl Pts',(2.28914438518197,-0.98400064223475,-5.77528561428499));
#78488=CARTESIAN_POINT('Ctrl Pts',(2.40841035759913,4.32476035110414,-3.95204113035316));
#78489=CARTESIAN_POINT('Ctrl Pts',(2.5276763300163,5.6634667686517,1.49910818517671));
#78490=CARTESIAN_POINT('Ctrl Pts',(2.64694230243346,1.80320946697538,5.5741023320976));
#78491=CARTESIAN_POINT('Ctrl Pts',(2.76620827485063,-3.71236267628471,4.53216775397974));
#78492=CARTESIAN_POINT('Ctrl Pts',(2.88547424726779,-5.82005062863969,-0.670217778454638));
#78493=CARTESIAN_POINT('Ctrl Pts',(3.00474021968496,-2.58503360922216,-5.25735507928439));
#78494=CARTESIAN_POINT('Ctrl Pts',(3.12400619210212,3.02299917886025,-5.01833210888796));
#78495=CARTESIAN_POINT('Ctrl Pts',(3.24327216451929,5.85597144374314,-0.172567785379327));
#78496=CARTESIAN_POINT('Ctrl Pts',(3.36253813693645,3.31326405507003,4.83161075541754));
#78497=CARTESIAN_POINT('Ctrl Pts',(3.48180410935361,-2.27096195076241,5.40045488905101));
#78498=CARTESIAN_POINT('Ctrl Pts',(3.60107008177078,-5.77048449279005,1.01177562184265));
#78499=CARTESIAN_POINT('Ctrl Pts',(3.72033605418794,-3.97280291129088,-4.30569602021837));
#78500=CARTESIAN_POINT('Ctrl Pts',(3.83960202660511,1.47184245460874,-5.67061380974733));
#78501=CARTESIAN_POINT('Ctrl Pts',(3.95886799902227,5.56536211702939,-1.83000702097551));
#78502=CARTESIAN_POINT('Ctrl Pts',(4.07813397143944,4.54997641940911,3.69051429658614));
#78503=CARTESIAN_POINT('Ctrl Pts',(4.1973999438566,-0.642208276797606,5.82320785475656));
#78504=CARTESIAN_POINT('Ctrl Pts',(4.31666591627376,-5.24485697541764,2.61029816264319));
#78505=CARTESIAN_POINT('Ctrl Pts',(4.43593188869093,-5.03281844418643,-2.99881971754596));
#78506=CARTESIAN_POINT('Ctrl Pts',(4.55519786110809,-0.200740356689758,
-5.85507339831722));
#78507=CARTESIAN_POINT('Ctrl Pts',(4.67446383352526,4.81561387721088,-3.33647181557097));
#78508=CARTESIAN_POINT('Ctrl Pts',(4.79372980594242,5.41131855914629,2.24495270371661));
#78509=CARTESIAN_POINT('Ctrl Pts',(4.91299577835959,1.03952718056155,5.76554979436997));
#78510=CARTESIAN_POINT('Ctrl Pts',(5.03226175077675,-4.28653201977527,3.99347272858184));
#78511=CARTESIAN_POINT('Ctrl Pts',(5.15152772319392,-5.67762958575462,-1.44454265338526));
#78512=CARTESIAN_POINT('Ctrl Pts',(5.27079369561108,-1.85676221341805,-5.55649307327102));
#78513=CARTESIAN_POINT('Ctrl Pts',(5.39005966802825,3.66858048774337,-4.56767976060429));
#78514=CARTESIAN_POINT('Ctrl Pts',(5.50932564044541,5.82623028349186,0.614183909108646));
#78515=CARTESIAN_POINT('Ctrl Pts',(5.62859161286257,2.63550229209064,5.23223746201096));
#78516=CARTESIAN_POINT('Ctrl Pts',(5.74785758527974,-2.9745708386434,5.0471882782771));
#78517=CARTESIAN_POINT('Ctrl Pts',(5.8671235576969,-5.85403981787645,0.228908281201479));
#78518=CARTESIAN_POINT('Ctrl Pts',(5.98638953011408,-3.3596023424104,-4.79950552571371));
#78519=CARTESIAN_POINT('Ctrl Pts',(6.10565550253123,2.21889148982482,-5.42205696639832));
#78520=CARTESIAN_POINT('Ctrl Pts',(6.2249214749484,5.76048163325456,-1.06725467598998));
#78521=CARTESIAN_POINT('Ctrl Pts',(6.34418744736557,4.01405010375492,4.26726879338893));
#78522=CARTESIAN_POINT('Ctrl Pts',(6.46345341978272,-1.41720941345036,5.6845139342703));
#78523=CARTESIAN_POINT('Ctrl Pts',(6.5827193921999,-5.54749540612569,1.88347442496573));
#78524=CARTESIAN_POINT('Ctrl Pts',(6.70198536461705,-4.58527736776309,-3.64656175748683));
#78525=CARTESIAN_POINT('Ctrl Pts',(6.82125133703423,0.586145324104315,-5.82911784488152));
#78526=CARTESIAN_POINT('Ctrl Pts',(6.94051730945138,5.21949683118455,-2.66064541413169));
#78527=CARTESIAN_POINT('Ctrl Pts',(7.05978328186856,5.06144127852277,2.95025310347291));
#78528=CARTESIAN_POINT('Ctrl Pts',(7.17904925428571,0.257070906874864,5.85287072634652));
#78529=CARTESIAN_POINT('Ctrl Pts',(7.29831522670289,-4.78328607380694,3.38265510015582));
#78530=CARTESIAN_POINT('Ctrl Pts',(7.41758119912004,-5.43266986223127,-2.19277891235983));
#78531=CARTESIAN_POINT('Ctrl Pts',(7.53684717153722,-1.09495746628347,-5.75528012676322));
#78532=CARTESIAN_POINT('Ctrl Pts',(7.65611314395437,4.24790678697028,-4.03453456047874));
#78533=CARTESIAN_POINT('Ctrl Pts',(7.77537911637154,5.6912666959334,1.38984336752211));
#78534=CARTESIAN_POINT('Ctrl Pts',(7.8946450887887,1.91014303727615,5.53836932387422));
#78535=CARTESIAN_POINT('Ctrl Pts',(8.01391106120587,-3.62445861551272,4.60276883353065));
#78536=CARTESIAN_POINT('Ctrl Pts',(8.13317703362303,-5.83187047208342,-0.558093170830226));
#78537=CARTESIAN_POINT('Ctrl Pts',(8.25244300604019,-2.68572694674573,-5.20663537786251));
#78538=CARTESIAN_POINT('Ctrl Pts',(8.37170897845736,2.92586707494877,-5.0755771149906));
#78539=CARTESIAN_POINT('Ctrl Pts',(8.49097495087453,5.85156615078993,-0.285227581792945));
#78540=CARTESIAN_POINT('Ctrl Pts',(8.61024092329168,3.40562955517506,4.76695589694342));
#78541=CARTESIAN_POINT('Ctrl Pts',(8.72950689570887,-2.16661557578352,5.44315700097451));
#78542=CARTESIAN_POINT('Ctrl Pts',(8.84877286812601,-5.749945395302,1.12263491016946));
#78543=CARTESIAN_POINT('Ctrl Pts',(8.96803884054319,-4.05492562457292,-4.22844644871701));
#78544=CARTESIAN_POINT('Ctrl Pts',(9.08730481296034,1.36244514907805,-5.69788771442885));
#78545=CARTESIAN_POINT('Ctrl Pts',(9.20657078537752,5.52911503776992,-1.93676743301625));
#78546=CARTESIAN_POINT('Ctrl Pts',(9.32583675779466,4.6201537530093,3.60227157347134));
#78547=CARTESIAN_POINT('Ctrl Pts',(9.44510273021186,-0.530028098646155,
5.83448810137882));
#78548=CARTESIAN_POINT('Ctrl Pts',(9.564368702629,-5.19365339976557,2.71074630933791));
#78549=CARTESIAN_POINT('Ctrl Pts',(9.68363467504617,-5.08959546046003,-2.90141331756615));
#78550=CARTESIAN_POINT('Ctrl Pts',(9.80290064746334,-0.313377654176505,
-5.85012612140531));
#78551=CARTESIAN_POINT('Ctrl Pts',(9.92216661988049,4.75051537313899,-3.4285251756485));
#78552=CARTESIAN_POINT('Ctrl Pts',(10.0414325922977,5.45351813986867,2.14040208573271));
#78553=CARTESIAN_POINT('Ctrl Pts',(10.1606985647148,1.1502863669621,5.74447756236082));
#78554=CARTESIAN_POINT('Ctrl Pts',(10.279964537132,-4.20888822910284,4.07522282401896));
#78555=CARTESIAN_POINT('Ctrl Pts',(10.3992305095492,-5.70437683649141,-1.33501539234042));
#78556=CARTESIAN_POINT('Ctrl Pts',(10.5184964819663,-1.96334699587643,-5.51973276203376));
#78557=CARTESIAN_POINT('Ctrl Pts',(10.6377624543835,3.58000114495498,-4.63743172376764));
#78558=CARTESIAN_POINT('Ctrl Pts',(10.7570284268007,5.83697067217415,0.50195075721085));
#78559=CARTESIAN_POINT('Ctrl Pts',(10.8762943992178,2.73570292275234,5.18055119740459));
#78560=CARTESIAN_POINT('Ctrl Pts',(10.995560371635,-2.87689239738814,5.10349599043008));
#78561=CARTESIAN_POINT('Ctrl Pts',(11.1148263440521,-5.84855067152691,0.341520472399031));
#78562=CARTESIAN_POINT('Ctrl Pts',(11.2340923164693,-3.45134143158132,-4.73396488296396));
#78563=CARTESIAN_POINT('Ctrl Pts',(11.3533582888865,2.11413904900531,-5.4637530390709));
#78564=CARTESIAN_POINT('Ctrl Pts',(11.4726242613036,5.73887675451073,-1.17791119657705));
#78565=CARTESIAN_POINT('Ctrl Pts',(11.5918902337208,4.09542568897112,4.18923258086744));
#78566=CARTESIAN_POINT('Ctrl Pts',(11.711156206138,-1.30755473226162,5.71073391190888));
#78567=CARTESIAN_POINT('Ctrl Pts',(11.8304221785551,-5.51022271384947,1.98988111058489));
#78568=CARTESIAN_POINT('Ctrl Pts',(11.9496881509723,-4.65460234584999,-3.55764784548636));
#78569=CARTESIAN_POINT('Ctrl Pts',(12.0689541233895,0.473861796467209,-5.83931812700205));
#78570=CARTESIAN_POINT('Ctrl Pts',(12.1882200958066,5.16732907407318,-2.76059620928582));
#78571=CARTESIAN_POINT('Ctrl Pts',(12.3074860682238,5.11727838312716,2.85230488203232));
#78572=CARTESIAN_POINT('Ctrl Pts',(12.426752040641,0.369655385002119,5.84683983762381));
#78573=CARTESIAN_POINT('Ctrl Pts',(12.5460180130581,-4.71730480953397,3.47407779481591));
#78574=CARTESIAN_POINT('Ctrl Pts',(12.6652839854753,-5.47386146166072,-2.08782707354593));
#78575=CARTESIAN_POINT('Ctrl Pts',(12.7845499578925,-1.20550875954632,-5.7331431014011));
#78576=CARTESIAN_POINT('Ctrl Pts',(12.9038159303096,4.1694799590057,-4.1155337517672));
#78577=CARTESIAN_POINT('Ctrl Pts',(13.0230819027268,5.71695879352572,1.28006380450929));
#78578=CARTESIAN_POINT('Ctrl Pts',(13.1423478751439,2.01636916292184,5.50058511335874));
#78579=CARTESIAN_POINT('Ctrl Pts',(13.2616138475611,-3.5352121925064,4.6716652217854));
#78580=CARTESIAN_POINT('Ctrl Pts',(13.3808798199783,-5.84153041152292,-0.445761866626982));
#78581=CARTESIAN_POINT('Ctrl Pts',(13.5001457923954,-2.78542559270095,-5.15398733584129));
#78582=CARTESIAN_POINT('Ctrl Pts',(13.6194117648126,2.82765134065804,-5.13094231951208));
#78583=CARTESIAN_POINT('Ctrl Pts',(13.7386777372298,5.84499365929882,-0.397781740710223));
#78584=CARTESIAN_POINT('Ctrl Pts',(13.8579437096469,3.49673373904406,4.70053553850163));
#78585=CARTESIAN_POINT('Ctrl Pts',(13.9772096820641,-2.06146676843229,5.48384317364516));
#78586=CARTESIAN_POINT('Ctrl Pts',(14.0964756544813,-5.72727673575607,1.23307841703323));
#78587=CARTESIAN_POINT('Ctrl Pts',(14.2157416268984,-4.13554654693988,-4.14963082075738));
#78588=CARTESIAN_POINT('Ctrl Pts',(14.3350075993156,1.25254324545183,-5.72305133724644));
#78589=CARTESIAN_POINT('Ctrl Pts',(14.4542735717327,5.49082018365544,-2.04281053973388));
#78590=CARTESIAN_POINT('Ctrl Pts',(14.5735395441499,4.68861995659749,3.51269470536248));
#78591=CARTESIAN_POINT('Ctrl Pts',(14.6928055165671,-0.417651618155915,
5.84360747452608));
#78592=CARTESIAN_POINT('Ctrl Pts',(14.8120714889842,-5.14052629154732,2.81019049823969));
#78593=CARTESIAN_POINT('Ctrl Pts',(14.9313374614014,-5.14448748328812,-2.80293234395298));
#78594=CARTESIAN_POINT('Ctrl Pts',(15.0506034338186,-0.425898888445909,
-5.84301217928782));
#78595=CARTESIAN_POINT('Ctrl Pts',(15.1698694062357,4.68365745804696,-3.51930873981908));
#78596=CARTESIAN_POINT('Ctrl Pts',(15.2891353786529,5.4936979439647,2.03505874386071));
#78597=CARTESIAN_POINT('Ctrl Pts',(15.4084013510701,1.26061953084691,5.72127779337208));
#78598=CARTESIAN_POINT('Ctrl Pts',(15.5276673234872,-4.1296856255962,4.1554636112268));
#78599=CARTESIAN_POINT('Ctrl Pts',(15.6469332959044,-5.72901140203915,-1.22499369214346));
#78600=CARTESIAN_POINT('Ctrl Pts',(15.7661992683216,-2.06920462894793,-5.48092815078119));
#78601=CARTESIAN_POINT('Ctrl Pts',(15.8854652407387,3.49009590529609,-4.70546615781277));
#78602=CARTESIAN_POINT('Ctrl Pts',(16.0047312131559,5.8455492679312,0.389531701758518));
#78603=CARTESIAN_POINT('Ctrl Pts',(16.1239971855731,2.8348903526364,5.12694625279165));
#78604=CARTESIAN_POINT('Ctrl Pts',(16.2432631579902,-2.77814846411986,5.15791356090758));
#78605=CARTESIAN_POINT('Ctrl Pts',(16.3625291304074,-5.84089544345886,0.454006177344968));
#78606=CARTESIAN_POINT('Ctrl Pts',(16.4817951028245,-3.54180227456795,-4.66667095886892));
#78607=CARTESIAN_POINT('Ctrl Pts',(16.6010610752417,2.00860361113205,-5.50342554449801));
#78608=CARTESIAN_POINT('Ctrl Pts',(16.7203270476589,5.71514641311463,-1.28813146345738));
#78609=CARTESIAN_POINT('Ctrl Pts',(16.839593020076,4.17528448358166,4.10964483521964));
#78610=CARTESIAN_POINT('Ctrl Pts',(16.9588589924932,-1.19741578230951,5.73483884993833));
#78611=CARTESIAN_POINT('Ctrl Pts',(17.0781249649104,-5.47090924371988,2.09555081958569));
#78612=CARTESIAN_POINT('Ctrl Pts',(17.1973909373275,-4.72220343547024,-3.46741631543117));
#78613=CARTESIAN_POINT('Ctrl Pts',(17.3166569097447,0.361402768363106,-5.84735574678891));
#78614=CARTESIAN_POINT('Ctrl Pts',(17.4359228821619,5.11324753392925,-2.85952458413149));
#78615=CARTESIAN_POINT('Ctrl Pts',(17.555188854579,5.17122024157952,2.75330027486351));
#78616=CARTESIAN_POINT('Ctrl Pts',(17.6744548269962,0.482102956771366,5.83864350081062));
#78617=CARTESIAN_POINT('Ctrl Pts',(17.7937207994134,-4.64957643417624,3.56421382260364));
#78618=CARTESIAN_POINT('Ctrl Pts',(17.9129867718305,-5.5130257500676,-1.98210198263782));
#78619=CARTESIAN_POINT('Ctrl Pts',(18.0322527442477,-1.31561357801008,-5.70888273691459));
#78620=CARTESIAN_POINT('Ctrl Pts',(18.1515187166649,4.08950891353811,-4.19500870518504));
#78621=CARTESIAN_POINT('Ctrl Pts',(18.270784689082,5.74053354604842,1.1698101543319));
#78622=CARTESIAN_POINT('Ctrl Pts',(18.3900506614992,2.12184850177754,5.46076369439205));
#78623=CARTESIAN_POINT('Ctrl Pts',(18.5093166339163,-3.4446564607618,4.73883140213048));
#78624=CARTESIAN_POINT('Ctrl Pts',(18.6285826063335,-5.84902686928229,-0.333265469106851));
#78625=CARTESIAN_POINT('Ctrl Pts',(18.7478485787507,-2.88409262248423,-5.09943045206206));
#78626=CARTESIAN_POINT('Ctrl Pts',(18.8671145511678,2.72838835137739,-5.18440721727702));
#78627=CARTESIAN_POINT('Ctrl Pts',(18.986380523585,5.83625640347177,-0.510188576332255));
#78628=CARTESIAN_POINT('Ctrl Pts',(19.1056464960022,3.58654286513676,4.63237427967802));
#78629=CARTESIAN_POINT('Ctrl Pts',(19.2249124684194,-1.95555447184578,5.52249833844519));
#78630=CARTESIAN_POINT('Ctrl Pts',(19.3441784408365,-5.70248690976545,1.3430652383406));
#78631=CARTESIAN_POINT('Ctrl Pts',(19.4634444132536,-4.21463581945459,-4.06927832666386));
#78632=CARTESIAN_POINT('Ctrl Pts',(19.5827103856708,1.14217744723407,-5.74609535854703));
#78633=CARTESIAN_POINT('Ctrl Pts',(19.701976358088,5.45049173764998,-2.14809706677667));
#78634=CARTESIAN_POINT('Ctrl Pts',(19.8212423305052,4.75534967288414,3.42181686813988));
#78635=CARTESIAN_POINT('Ctrl Pts',(19.9405083029223,-0.305120455320437,
5.85056259672785));
#78636=CARTESIAN_POINT('Ctrl Pts',(20.0597742753395,-5.08549532703213,2.90859389898618));
#78637=CARTESIAN_POINT('Ctrl Pts',(20.1790402477566,-5.19747418274383,-2.70341327033015));
#78638=CARTESIAN_POINT('Ctrl Pts',(20.2983062201738,-0.538262385893262,
-5.83373420669972));
#78639=CARTESIAN_POINT('Ctrl Pts',(20.417572192591,4.615064893575,-3.60878888528781));
#78640=CARTESIAN_POINT('Ctrl Pts',(20.5368381650081,5.53184309035626,1.92896169328567));
#78641=CARTESIAN_POINT('Ctrl Pts',(20.6561041374253,1.37048580898969,5.69595907971992));
#78642=CARTESIAN_POINT('Ctrl Pts',(20.7753701098424,-4.04895354290072,4.23416537205587));
#78643=CARTESIAN_POINT('Ctrl Pts',(20.8946360822597,-5.7515241586875,-1.11451830066622));
#78644=CARTESIAN_POINT('Ctrl Pts',(21.0139020546768,-2.17429590697344,-5.44009361127219));
#78645=CARTESIAN_POINT('Ctrl Pts',(21.133168027094,3.39889806626329,-4.77175786536124));
#78646=CARTESIAN_POINT('Ctrl Pts',(21.2524339995111,5.85196289357594,0.276968378513138));
#78647=CARTESIAN_POINT('Ctrl Pts',(21.3716999719283,2.93302784647445,5.07144248141408));
#78648=CARTESIAN_POINT('Ctrl Pts',(21.4909659443455,-2.67837560985263,5.21042083550184));
#78649=CARTESIAN_POINT('Ctrl Pts',(21.6102319167626,-5.83107696887886,0.566323735593342));
#78650=CARTESIAN_POINT('Ctrl Pts',(21.7294978891798,-3.63095136809929,-4.5976486765502));
#78651=CARTESIAN_POINT('Ctrl Pts',(21.848763861597,1.90232426253526,-5.54105978948566));
#78652=CARTESIAN_POINT('Ctrl Pts',(21.9680298340141,5.68929939788601,-1.39787465521763));
#78653=CARTESIAN_POINT('Ctrl Pts',(22.0872958064313,4.253596910913,4.02853503273303));
#78654=CARTESIAN_POINT('Ctrl Pts',(22.2065617788484,-1.08683335489076,5.75681982080229));
#78655=CARTESIAN_POINT('Ctrl Pts',(22.3258277512656,-5.42956955595747,2.20044441590912));
#78656=CARTESIAN_POINT('Ctrl Pts',(22.4450937236828,-4.78805559974015,-3.37590058566347));
#78657=CARTESIAN_POINT('Ctrl Pts',(22.5643596961,0.248809890357853,-5.85322772741205));
#78658=CARTESIAN_POINT('Ctrl Pts',(22.6836256685171,5.05727224050727,-2.95739389934458));
#78659=CARTESIAN_POINT('Ctrl Pts',(22.8028916409343,5.22324687585818,2.65327594952422));
#78660=CARTESIAN_POINT('Ctrl Pts',(22.9221576133514,0.594371975859776,5.82828475151976));
#78661=CARTESIAN_POINT('Ctrl Pts',(23.0414235857686,-4.58012603175932,3.65302980054727));
#78662=CARTESIAN_POINT('Ctrl Pts',(23.1606895581858,-5.5501482224826,-1.87564279620591));
#78663=CARTESIAN_POINT('Ctrl Pts',(23.2799555306029,-1.42523114301903,-5.68250801842407));
#78664=CARTESIAN_POINT('Ctrl Pts',(23.3992215030202,4.00802326881451,-4.27292998621875));
#78665=CARTESIAN_POINT('Ctrl Pts',(23.5184874754372,5.76198222230599,1.0591232507672));
#78666=CARTESIAN_POINT('Ctrl Pts',(23.6377534478545,2.22654198829003,5.4189198153199));
#78667=CARTESIAN_POINT('Ctrl Pts',(23.7570194202715,-3.35282495869293,4.80424249875583));
#78668=CARTESIAN_POINT('Ctrl Pts',(23.8762853926888,-5.85435706895763,-0.220645642675769));
#78669=CARTESIAN_POINT('Ctrl Pts',(23.9955513651059,-2.9816914935637,-5.04298493232878));
#78670=CARTESIAN_POINT('Ctrl Pts',(24.1148173375231,2.62811487035934,-5.23595200691163));
#78671=CARTESIAN_POINT('Ctrl Pts',(24.2340833099403,5.82535761925768,-0.62240645742347));
#78672=CARTESIAN_POINT('Ctrl Pts',(24.3533492823574,3.67502367155342,4.56249736482195));
#78673=CARTESIAN_POINT('Ctrl Pts',(24.4726152547746,-1.84891791192818,5.55910817896513));
#78674=CARTESIAN_POINT('Ctrl Pts',(24.5918812271917,-5.67558509854319,1.4525546391377));
#78675=CARTESIAN_POINT('Ctrl Pts',(24.7111471996089,-4.29216415044515,-3.98741872595776));
#78676=CARTESIAN_POINT('Ctrl Pts',(24.8304131720261,1.03138862973723,-5.76701124369755));
#78677=CARTESIAN_POINT('Ctrl Pts',(24.9496791444432,5.40814463588299,-2.25258802000187));
#78678=CARTESIAN_POINT('Ctrl Pts',(25.0689451168604,4.82031818770908,3.32967171951333));
#78679=CARTESIAN_POINT('Ctrl Pts',(25.1882110892775,-0.192476287421281,
5.85535089207007));
#78680=CARTESIAN_POINT('Ctrl Pts',(25.3074770616947,-5.02858088760561,3.00592006668398));
#78681=CARTESIAN_POINT('Ctrl Pts',(25.4267430341119,-5.24853593456004,-2.6028929547943));
#78682=CARTESIAN_POINT('Ctrl Pts',(25.5460090065291,-0.650426531333829,
-5.82229563985052));
#78683=CARTESIAN_POINT('Ctrl Pts',(25.6652749789462,4.5447630838118,-3.6969324719972));
#78684=CARTESIAN_POINT('Ctrl Pts',(25.7845409513634,5.56793945152552,1.82215022833782));
#78685=CARTESIAN_POINT('Ctrl Pts',(25.9038069237805,1.47984451108115,5.66853079849693));
#78686=CARTESIAN_POINT('Ctrl Pts',(26.0230728961977,-3.96672188112297,4.31129895835422));
#78687=CARTESIAN_POINT('Ctrl Pts',(26.1423388686148,-5.77190676856384,-1.00363013381062));
#78688=CARTESIAN_POINT('Ctrl Pts',(26.2616048410321,-2.27858190812287,-5.39724426707374));
#78689=CARTESIAN_POINT('Ctrl Pts',(26.3808708134492,3.30644140408296,-4.83628229447494));
#78690=CARTESIAN_POINT('Ctrl Pts',(26.5001367858664,5.85620917374429,0.164302476667459));
#78691=CARTESIAN_POINT('Ctrl Pts',(26.6194027582835,3.03007905785472,5.01406043976691));
#78692=CARTESIAN_POINT('Ctrl Pts',(26.7386687307008,-2.57761078667377,5.26099836750677));
#78693=CARTESIAN_POINT('Ctrl Pts',(26.8579347031178,-5.81909888417815,0.678431548973455));
#78694=CARTESIAN_POINT('Ctrl Pts',(26.9772006755351,-3.71875569472669,-4.5269235992474));
#78695=CARTESIAN_POINT('Ctrl Pts',(27.0964666479522,1.79534036506138,-5.57664183573476));
#78696=CARTESIAN_POINT('Ctrl Pts',(27.2157326203694,5.66134528158068,-1.50710012713492));
#78697=CARTESIAN_POINT('Ctrl Pts',(27.3349985927865,4.33033396700724,3.94593321340702));
#78698=CARTESIAN_POINT('Ctrl Pts',(27.4542645652037,-0.975848405549228,
5.77666868358165));
#78699=CARTESIAN_POINT('Ctrl Pts',(27.5735305376208,-5.38621896121736,2.30452305093883));
#78700=CARTESIAN_POINT('Ctrl Pts',(27.6927965100381,-4.85213444951138,-3.28313455014414));
#78701=CARTESIAN_POINT('Ctrl Pts',(27.8120624824551,0.136124862590045,-5.85693189411237));
#78702=CARTESIAN_POINT('Ctrl Pts',(27.9313284548724,4.9994239249365,-3.05416790783649));
#78703=CARTESIAN_POINT('Ctrl Pts',(28.0505944272895,5.27333901726761,2.55226895123699));
#78704=CARTESIAN_POINT('Ctrl Pts',(28.1698603997067,0.706420862073846,5.81576742623987));
#78705=CARTESIAN_POINT('Ctrl Pts',(28.2891263721238,-4.50897932408263,3.74049283457156));
#78706=CARTESIAN_POINT('Ctrl Pts',(28.408392344541,-5.58521513014738,-1.76848894270167));
#78707=CARTESIAN_POINT('Ctrl Pts',(28.5276583169582,-1.53432085637788,-5.65402871412675));
#78708=CARTESIAN_POINT('Ctrl Pts',(28.6469242893753,3.92505320403234,-4.34926873577631));
#78709=CARTESIAN_POINT('Ctrl Pts',(28.7661902617925,5.78129687852069,0.948044088053002));
#78710=CARTESIAN_POINT('Ctrl Pts',(28.8854562342096,2.33041084795627,5.37506897353082));
#78711=CARTESIAN_POINT('Ctrl Pts',(29.0047222066268,-3.25975169721106,4.86787428586805));
#78712=CARTESIAN_POINT('Ctrl Pts',(29.123988179044,-5.85751903644455,-0.107944097453046));
#78713=CARTESIAN_POINT('Ctrl Pts',(29.2432541514612,-3.07818605901322,-4.98467168192475));
#78714=CARTESIAN_POINT('Ctrl Pts',(29.3625201238783,2.52686803510449,-5.28555759817761));
#78715=CARTESIAN_POINT('Ctrl Pts',(29.4817860962955,5.81230134315328,-0.734393822729839));
#78716=CARTESIAN_POINT('Ctrl Pts',(29.6010520687127,3.76214338835384,4.49093067369687));
#78717=CARTESIAN_POINT('Ctrl Pts',(29.7203180411298,-1.7415965828236,5.59365913630631));
#78718=CARTESIAN_POINT('Ctrl Pts',(29.839584013547,-5.64658126550127,1.56150606869626));
#78719=CARTESIAN_POINT('Ctrl Pts',(29.9588499859641,-4.36810282635358,-3.90408233633562));
#78720=CARTESIAN_POINT('Ctrl Pts',(30.0781159583813,0.920217824944716,-5.78579124624626));
#78721=CARTESIAN_POINT('Ctrl Pts',(30.1973819307985,5.36379456211742,-2.35624469991655));
#78722=CARTESIAN_POINT('Ctrl Pts',(30.3166479032156,4.88350143919435,3.23629338655699));
#78723=CARTESIAN_POINT('Ctrl Pts',(30.4359138756328,-0.079760833593354,
5.85797058714965));
#78724=CARTESIAN_POINT('Ctrl Pts',(30.55517984805,-4.96980405222106,3.10213295540542));
#78725=CARTESIAN_POINT('Ctrl Pts',(30.6744458204671,-5.29765382739722,-2.50140862626428));
#78726=CARTESIAN_POINT('Ctrl Pts',(30.7937117928843,-0.762349783414896,
-5.80870071515249));
#78727=CARTESIAN_POINT('Ctrl Pts',(30.9129777653015,4.47277806588579,-3.78370685489987));
#78728=CARTESIAN_POINT('Ctrl Pts',(31.0322437377186,5.601973658747,1.71466390793955));
#78729=CARTESIAN_POINT('Ctrl Pts',(31.1515097101358,1.5886551347986,5.63900310810021));
#78730=CARTESIAN_POINT('Ctrl Pts',(31.270775682553,-3.88302109575688,4.38683580276175));
#78731=CARTESIAN_POINT('Ctrl Pts',(31.3900416549701,-5.79015168272125,-0.89237026035508));
#78732=CARTESIAN_POINT('Ctrl Pts',(31.5093076273873,-2.38202400880994,-5.35239598796079));
#78733=CARTESIAN_POINT('Ctrl Pts',(31.6285735998044,3.21276016120207,-4.89901554774815));
#78734=CARTESIAN_POINT('Ctrl Pts',(31.7478395722217,5.85828653577487,0.0515757234056574));
#78735=CARTESIAN_POINT('Ctrl Pts',(31.8671055446387,3.12600804268317,4.95482137998596));
#78736=CARTESIAN_POINT('Ctrl Pts',(31.986371517056,-2.47589131405855,5.30962742491925));
#78737=CARTESIAN_POINT('Ctrl Pts',(32.1056374894731,-5.80496562558577,0.790288096995977));
#78738=CARTESIAN_POINT('Ctrl Pts',(32.2249034618903,-3.80518273505212,-4.45452192085157));
#78739=CARTESIAN_POINT('Ctrl Pts',(32.3441694343074,1.68769154149534,-5.61015850500237));
#78740=CARTESIAN_POINT('Ctrl Pts',(32.4634354067246,5.63129441734489,-1.61576742623007));
#78741=CARTESIAN_POINT('Ctrl Pts',(32.5827013791418,4.40546723136434,3.8618699698282));
#78742=CARTESIAN_POINT('Ctrl Pts',(32.7019673515589,-0.86450203890803,5.79437808700892));
#78743=CARTESIAN_POINT('Ctrl Pts',(32.8212333239761,-5.34087351491845,2.40774817788913));
#78744=CARTESIAN_POINT('Ctrl Pts',(32.9404992963932,-4.9144162524043,-3.1891525659006));
#78745=CARTESIAN_POINT('Ctrl Pts',(33.0597652688104,0.0233894193275074,
-5.85846687500652));
#78746=CARTESIAN_POINT('Ctrl Pts',(33.1790312412276,4.93972401204274,-3.14981076817866));
#78747=CARTESIAN_POINT('Ctrl Pts',(33.2982972136447,5.3214781135754,2.4503166891698));
#78748=CARTESIAN_POINT('Ctrl Pts',(33.4175631860619,0.818208116748437,5.80109616091408));
#78749=CARTESIAN_POINT('Ctrl Pts',(33.536829158479,-4.43616266119279,3.82657053168034));
#78750=CARTESIAN_POINT('Ctrl Pts',(33.6560951308962,-5.61821348560732,-1.6606801078555));
#78751=CARTESIAN_POINT('Ctrl Pts',(33.7753611033134,-1.6428423153869,-5.62345537167841));
#78752=CARTESIAN_POINT('Ctrl Pts',(33.8946270757306,3.8406294481618,-4.42399668087533));
#78753=CARTESIAN_POINT('Ctrl Pts',(34.0138930481477,5.79847036127596,0.836613805705633));
#78754=CARTESIAN_POINT('Ctrl Pts',(34.1331590205649,2.43341661168203,5.32922740971606));
#78755=CARTESIAN_POINT('Ctrl Pts',(34.2524249929821,-3.16547114712599,4.92970319666262));
#78756=CARTESIAN_POINT('Ctrl Pts',(34.3716909653992,-5.85851160067448,0.00479742617581129));
#78757=CARTESIAN_POINT('Ctrl Pts',(34.4909569378164,-3.17354058089109,-4.92451229786949));
#78758=CARTESIAN_POINT('Ctrl Pts',(34.6102229102335,2.4246853435919,-5.33320561904289));
#78759=CARTESIAN_POINT('Ctrl Pts',(34.7294888826507,5.79709241073807,-0.846109196369897));
#78760=CARTESIAN_POINT('Ctrl Pts',(34.8487548550679,3.84786974963835,4.41770071189267));
#78761=CARTESIAN_POINT('Ctrl Pts',(34.9680208274851,-1.63363023218451,5.62613841410746));
#78762=CARTESIAN_POINT('Ctrl Pts',(35.0872867999022,-5.61548615275964,1.66987917552219));
#78763=CARTESIAN_POINT('Ctrl Pts',(35.2065527723194,-4.4424237219931,-3.81930002242228));
#78764=CARTESIAN_POINT('Ctrl Pts',(35.3258187447365,0.808706205598543,-5.80242841082625));
#78765=CARTESIAN_POINT('Ctrl Pts',(35.4450847171537,5.31745794329846,-2.45902871594494));
#78766=CARTESIAN_POINT('Ctrl Pts',(35.5643506895709,4.94487602407868,3.14171645294316));
#78767=CARTESIAN_POINT('Ctrl Pts',(35.6836166619881,0.0329841655221652,
5.85842071197083));
#78768=CARTESIAN_POINT('Ctrl Pts',(35.8028826344052,-4.90918659888947,3.1971969310834));
#78769=CARTESIAN_POINT('Ctrl Pts',(35.9221486068224,-5.34480965219109,-2.39899786982601));
#78770=CARTESIAN_POINT('Ctrl Pts',(36.0414145792395,-0.873990723536196,
-5.79295446929697));
#78771=CARTESIAN_POINT('Ctrl Pts',(36.1606805516567,4.39913656401214,-3.86907989292384));
#78772=CARTESIAN_POINT('Ctrl Pts',(36.2799465240739,5.6339329860754,1.60654253501617));
#78773=CARTESIAN_POINT('Ctrl Pts',(36.399212496491,1.69687761054767,5.60738695574555));
#78774=CARTESIAN_POINT('Ctrl Pts',(36.5184784689082,-3.79788262273949,4.46074790787285));
#78775=CARTESIAN_POINT('Ctrl Pts',(36.6377444413253,-5.8062513152231,-0.78077984606419));
#78776=CARTESIAN_POINT('Ctrl Pts',(36.7570104137426,-2.48458547192956,-5.30556546129872));
#78777=CARTESIAN_POINT('Ctrl Pts',(36.8762763861596,3.11789202290122,-4.95993424442102));
#78778=CARTESIAN_POINT('Ctrl Pts',(36.9955423585769,5.85818853286327,-0.0611704102445672));
#78779=CARTESIAN_POINT('Ctrl Pts',(37.114808330994,3.22079005536847,4.89374777128489));
#78780=CARTESIAN_POINT('Ctrl Pts',(37.2340743034112,-2.37327534445112,5.35628899208556));
#78781=CARTESIAN_POINT('Ctrl Pts',(37.3533402758283,-5.78864353195016,0.901853861538382));
#78782=CARTESIAN_POINT('Ctrl Pts',(37.4726062482455,-3.89027435237813,-4.38047408248273));
#78783=CARTESIAN_POINT('Ctrl Pts',(37.5918722206627,1.57955796423474,-5.64159049656991));
#78784=CARTESIAN_POINT('Ctrl Pts',(37.7111381930798,5.59889145836505,-1.72384938880929));
#78785=CARTESIAN_POINT('Ctrl Pts',(37.830404165497,4.47947502597244,3.77640129668631));
#78786=CARTESIAN_POINT('Ctrl Pts',(37.9496701379142,-0.753797156194961,
5.80989413817872));
#78787=CARTESIAN_POINT('Ctrl Pts',(38.0689361103313,-5.29172052081598,2.51017245988127));
#78788=CARTESIAN_POINT('Ctrl Pts',(38.1882020827485,-4.97837853386125,-3.09417052848874));
#78789=CARTESIAN_POINT('Ctrl Pts',(38.3074680551657,-0.0824858617694694,
-5.85741598647027));
#78790=CARTESIAN_POINT('Ctrl Pts',(38.4068563655133,4.03899355773438,-3.68100514101762));
#78791=CARTESIAN_POINT('Ctrl Pts',(38.4863670137914,5.13673732082221,-0.443168429242001));
#78792=CARTESIAN_POINT('Ctrl Pts',(38.5261223379305,4.8694790910934,1.22917467492147));
#78793=CARTESIAN_POINT('Ctrl Pts',(38.546,4.53891924175741,1.9850259738362));
#78794=CARTESIAN_POINT('Ctrl Pts',(-17.7840033022126,2.79181362996783,-3.91758709698588));
#78795=CARTESIAN_POINT('Ctrl Pts',(-17.764125640143,3.44419652954148,-3.45267555171637));
#78796=CARTESIAN_POINT('Ctrl Pts',(-17.724370316004,4.50091513856352,-2.19257893815165));
#78797=CARTESIAN_POINT('Ctrl Pts',(-17.6448596677259,5.20107532249908,1.05263844334769));
#78798=CARTESIAN_POINT('Ctrl Pts',(-17.5454713573782,2.85251838409021,4.92149809869413));
#78799=CARTESIAN_POINT('Ctrl Pts',(-17.4262053849611,-2.60480908979514,
5.06088873571236));
#78800=CARTESIAN_POINT('Ctrl Pts',(-17.3069394125439,-5.66091456100895,
0.547658985425077));
#78801=CARTESIAN_POINT('Ctrl Pts',(-17.1876734401267,-3.5256034875135,-4.4648272083155));
#78802=CARTESIAN_POINT('Ctrl Pts',(-17.0684074677096,1.84887983265183,-5.38050279906848));
#78803=CARTESIAN_POINT('Ctrl Pts',(-16.9491414952924,5.52468767357187,-1.35601227028438));
#78804=CARTESIAN_POINT('Ctrl Pts',(-16.8298755228753,4.12968454665724,3.91276942512457));
#78805=CARTESIAN_POINT('Ctrl Pts',(-16.7106095504581,-1.05669498430824,
5.58996261315058));
#78806=CARTESIAN_POINT('Ctrl Pts',(-16.5913435780409,-5.27283738738912,
2.13552778114678));
#78807=CARTESIAN_POINT('Ctrl Pts',(-16.4720776056237,-4.648717369209,-3.27921068370341));
#78808=CARTESIAN_POINT('Ctrl Pts',(-16.3528116332066,0.242902213228417,
-5.68372969776847));
#78809=CARTESIAN_POINT('Ctrl Pts',(-16.2335456607894,4.91151121149745,-2.87066356623015));
#78810=CARTESIAN_POINT('Ctrl Pts',(-16.1142796883723,5.07145468313125,2.57761090616478));
#78811=CARTESIAN_POINT('Ctrl Pts',(-15.9950137159551,0.575882724972399,
5.65968918026788));
#78812=CARTESIAN_POINT('Ctrl Pts',(-15.8757477435379,-4.44833506603484,
3.54626851611126));
#78813=CARTESIAN_POINT('Ctrl Pts',(-15.7564817711208,-5.38906119904768,
-1.82256322803374));
#78814=CARTESIAN_POINT('Ctrl Pts',(-15.6372157987036,-1.38272190213506,
-5.51831454142211));
#78815=CARTESIAN_POINT('Ctrl Pts',(-15.5179498262864,3.89293133367724,-4.1483489137632));
#78816=CARTESIAN_POINT('Ctrl Pts',(-15.3986838538693,5.59494184347711,1.02972843796234));
#78817=CARTESIAN_POINT('Ctrl Pts',(-15.2794178814521,2.16089313957021,5.26253316330437));
#78818=CARTESIAN_POINT('Ctrl Pts',(-15.160151909035,-3.25681768400598,4.66442416312198));
#78819=CARTESIAN_POINT('Ctrl Pts',(-15.0408859366178,-5.68482672468769,
-0.215544834913055));
#78820=CARTESIAN_POINT('Ctrl Pts',(-14.9216199642006,-2.89426395266302,
-4.89764745133195));
#78821=CARTESIAN_POINT('Ctrl Pts',(-14.8023539917834,2.5531826362492,-5.08379511619378));
#78822=CARTESIAN_POINT('Ctrl Pts',(-14.6830880193663,5.65685210149595,-0.603107533830891));
#78823=CARTESIAN_POINT('Ctrl Pts',(-14.5638220469491,3.56762999275445,4.43122224858523));
#78824=CARTESIAN_POINT('Ctrl Pts',(-14.444556074532,-1.79661422561301,5.39776728873189));
#78825=CARTESIAN_POINT('Ctrl Pts',(-14.3252901021148,-5.51159792000934,
1.40925609896829));
#78826=CARTESIAN_POINT('Ctrl Pts',(-14.2060241296976,-4.16703084898607,
-3.87292761171638));
#78827=CARTESIAN_POINT('Ctrl Pts',(-14.0867581572805,1.00279786548942,-5.59983132092501));
#78828=CARTESIAN_POINT('Ctrl Pts',(-13.9674921848633,5.25207562902259,-2.18618754218488));
#78829=CARTESIAN_POINT('Ctrl Pts',(-13.8482262124461,4.68003956451101,3.23433827185923));
#78830=CARTESIAN_POINT('Ctrl Pts',(-13.7289602400289,-0.188191197364887,
5.68579796118773));
#78831=CARTESIAN_POINT('Ctrl Pts',(-13.6096942676118,-4.88366572225456,
2.91779428602944));
#78832=CARTESIAN_POINT('Ctrl Pts',(-13.4904282951946,-5.09602028828365,
-2.52869365555675));
#78833=CARTESIAN_POINT('Ctrl Pts',(-13.3711623227775,-0.630317107451957,
-5.65388492333468));
#78834=CARTESIAN_POINT('Ctrl Pts',(-13.2518963503603,4.41400618489981,-3.58890843877865));
#78835=CARTESIAN_POINT('Ctrl Pts',(-13.1326303779431,5.40634878253714,1.77062339977217));
#78836=CARTESIAN_POINT('Ctrl Pts',(-13.013364405526,1.43575748790641,5.50475383810973));
#78837=CARTESIAN_POINT('Ctrl Pts',(-12.8940984331088,-3.85283414011536,
4.18561625940866));
#78838=CARTESIAN_POINT('Ctrl Pts',(-12.7748324606917,-5.60459122334528,
-0.975844045667388));
#78839=CARTESIAN_POINT('Ctrl Pts',(-12.6555664882745,-2.21143131111649,
-5.24149653615046));
#78840=CARTESIAN_POINT('Ctrl Pts',(-12.5363005158573,3.21178397597373,-4.69554662142142));
#78841=CARTESIAN_POINT('Ctrl Pts',(-12.4170345434402,5.68663758863899,0.160833198506063));
#78842=CARTESIAN_POINT('Ctrl Pts',(-12.297768571023,2.94125707344572,4.86957094723645));
#78843=CARTESIAN_POINT('Ctrl Pts',(-12.1785025986058,-2.50414613780997,
5.10812749476314));
#78844=CARTESIAN_POINT('Ctrl Pts',(-12.0592366261887,-5.65078686842909,
0.657512091031845));
#78845=CARTESIAN_POINT('Ctrl Pts',(-11.9399706537715,-3.61010380708337,
-4.39668794484507));
#78846=CARTESIAN_POINT('Ctrl Pts',(-11.8207046813543,1.74459158669925,-5.41480512833859));
#78847=CARTESIAN_POINT('Ctrl Pts',(-11.7014387089372,5.49778233065907,-1.46222564160138));
#78848=CARTESIAN_POINT('Ctrl Pts',(-11.58217273652,4.20410477983222,3.83265148199726));
#78849=CARTESIAN_POINT('Ctrl Pts',(-11.4629067641028,-0.948867636666955,
5.60922138895852));
#78850=CARTESIAN_POINT('Ctrl Pts',(-11.3436407916857,-5.23079611155017,
2.236623889181));
#78851=CARTESIAN_POINT('Ctrl Pts',(-11.2243748192685,-4.71094498438226,
-3.18915533274683));
#78852=CARTESIAN_POINT('Ctrl Pts',(-11.1051088468514,0.133471476625133,
-5.68734558007435));
#78853=CARTESIAN_POINT('Ctrl Pts',(-10.9858428744342,4.85536344991656,-2.96465177575344));
#78854=CARTESIAN_POINT('Ctrl Pts',(-10.866576902017,5.12011645675633,2.47954065333013));
#78855=CARTESIAN_POINT('Ctrl Pts',(-10.7473109295998,0.684691854323342,
5.64755800739461));
#78856=CARTESIAN_POINT('Ctrl Pts',(-10.6280449571827,-4.37926792892479,
3.63121560761055));
#78857=CARTESIAN_POINT('Ctrl Pts',(-10.5087789847655,-5.42313613058841,
-1.71851938929136));
#78858=CARTESIAN_POINT('Ctrl Pts',(-10.3895130123484,-1.48865994725382,
-5.49068355887553));
#78859=CARTESIAN_POINT('Ctrl Pts',(-10.2702470399312,3.8123801045003,-4.22249598236326));
#78860=CARTESIAN_POINT('Ctrl Pts',(-10.150981067514,5.61372171061381,0.921869262990718));
#78861=CARTESIAN_POINT('Ctrl Pts',(-10.0317150950969,2.26176469319736,5.21997460289508));
#78862=CARTESIAN_POINT('Ctrl Pts',(-9.91244912267971,-3.16645286598505,
4.72623429695976));
#78863=CARTESIAN_POINT('Ctrl Pts',(-9.79318315026253,-5.6879219191093,-0.106106665105973));
#78864=CARTESIAN_POINT('Ctrl Pts',(-9.67391717784538,-2.98797785140271,
-4.84104355917095));
#78865=CARTESIAN_POINT('Ctrl Pts',(-9.5546512054282,2.4548777716912,-5.13198689674088));
#78866=CARTESIAN_POINT('Ctrl Pts',(-9.43538523301105,5.64419841497453,-0.711855768160145));
#78867=CARTESIAN_POINT('Ctrl Pts',(-9.31611926059388,3.65224335165753,4.36174654038232));
#78868=CARTESIAN_POINT('Ctrl Pts',(-9.19685328817672,-1.69240741107544,
5.43134159643826));
#78869=CARTESIAN_POINT('Ctrl Pts',(-9.07758731575955,-5.48345768708367,
1.51505979295432));
#78870=CARTESIAN_POINT('Ctrl Pts',(-8.95832134334239,-4.24078944127668,
-3.79202047687245));
#78871=CARTESIAN_POINT('Ctrl Pts',(-8.83905537092521,0.894849549605194,
-5.6180920841363));
#78872=CARTESIAN_POINT('Ctrl Pts',(-8.71978939850807,5.20903226068468,-2.28685314119865));
#78873=CARTESIAN_POINT('Ctrl Pts',(-8.60052342609088,4.74141420523234,3.14367710121201));
#78874=CARTESIAN_POINT('Ctrl Pts',(-8.48125745367373,-0.0787393973975508,
5.68836659240252));
#78875=CARTESIAN_POINT('Ctrl Pts',(-8.36199148125656,-4.82661160648078,
3.01123476043447));
#78876=CARTESIAN_POINT('Ctrl Pts',(-8.2427255088394,-5.14373853993627,-2.4301580637971));
#78877=CARTESIAN_POINT('Ctrl Pts',(-8.12345953642222,-0.739003203743718,
-5.64070816893767));
#78878=CARTESIAN_POINT('Ctrl Pts',(-8.00419356400507,4.34412418480804,-3.67318655246773));
#78879=CARTESIAN_POINT('Ctrl Pts',(-7.8849275915879,5.43942133594559,1.66625625649949));
#78880=CARTESIAN_POINT('Ctrl Pts',(-7.76566161917074,1.54142456759122,5.47610488255017));
#78881=CARTESIAN_POINT('Ctrl Pts',(-7.64639564675358,-3.7715730704045,4.25898473310993));
#78882=CARTESIAN_POINT('Ctrl Pts',(-7.5271296743364,-5.62233240835935,-0.867809121970914));
#78883=CARTESIAN_POINT('Ctrl Pts',(-7.40786370191925,-2.31188865242981,
-5.19796933821563));
#78884=CARTESIAN_POINT('Ctrl Pts',(-7.28859772950208,3.12082856564795,-4.75648435781088));
#78885=CARTESIAN_POINT('Ctrl Pts',(-7.16933175708492,5.68867958966067,0.0513703070056891));
#78886=CARTESIAN_POINT('Ctrl Pts',(-7.05006578466775,3.03442196449068,4.81206792592126));
#78887=CARTESIAN_POINT('Ctrl Pts',(-6.93079981225059,-2.40538210186704,
5.15537111431188));
#78888=CARTESIAN_POINT('Ctrl Pts',(-6.81153383983341,-5.63708735007736,
0.766133532657032));
#78889=CARTESIAN_POINT('Ctrl Pts',(-6.69226786741627,-3.69404472524156,
-4.32640127012959));
#78890=CARTESIAN_POINT('Ctrl Pts',(-6.57300189499908,1.6400665309183,-5.44737516207808));
#78891=CARTESIAN_POINT('Ctrl Pts',(-6.45373592258194,5.46862531548002,-1.56775366086475));
#78892=CARTESIAN_POINT('Ctrl Pts',(-6.33446995016476,4.27708143667285,3.75103835841921));
#78893=CARTESIAN_POINT('Ctrl Pts',(-6.2152039777476,-0.84074860602783,5.62644258512658));
#78894=CARTESIAN_POINT('Ctrl Pts',(-6.09593800533044,-5.18678609157587,
2.33687064736132));
#78895=CARTESIAN_POINT('Ctrl Pts',(-5.97667203291327,-4.77144440584691,
-3.09790778819772));
#78896=CARTESIAN_POINT('Ctrl Pts',(-5.85740606049611,0.0240000274783397,
-5.68886090363832));
#78897=CARTESIAN_POINT('Ctrl Pts',(-5.73814008807894,4.79741285415394,-3.05753892682699));
#78898=CARTESIAN_POINT('Ctrl Pts',(-5.61887411566178,5.16688435059337,2.38055045942261));
#78899=CARTESIAN_POINT('Ctrl Pts',(-5.49960814324461,0.793246126878927,
5.63333604220938));
#78900=CARTESIAN_POINT('Ctrl Pts',(-5.38034217082745,-4.30857820660237,
3.71481738714771));
#78901=CARTESIAN_POINT('Ctrl Pts',(-5.26107619841029,-5.4552028907182,-1.61383884057968));
#78902=CARTESIAN_POINT('Ctrl Pts',(-5.14181022599311,-1.59404646330102,
-5.46101915901246));
#78903=CARTESIAN_POINT('Ctrl Pts',(-5.02254425357596,3.73041681626036,-4.29507913305747));
#78904=CARTESIAN_POINT('Ctrl Pts',(-4.90327828115879,5.63042251929442,0.813668628181062));
#78905=CARTESIAN_POINT('Ctrl Pts',(-4.78401230874162,2.36179854770228,5.17548277963853));
#78906=CARTESIAN_POINT('Ctrl Pts',(-4.66474633632446,-3.07491529943844,
4.78629400304068));
#78907=CARTESIAN_POINT('Ctrl Pts',(-4.54548036390729,-5.68891053013843,
0.00337080760888953));
#78908=CARTESIAN_POINT('Ctrl Pts',(-4.42621439149013,-3.08058511232485,
-4.78264673041885));
#78909=CARTESIAN_POINT('Ctrl Pts',(-4.30694841907297,2.35566371127412,-5.17827798226882));
#78910=CARTESIAN_POINT('Ctrl Pts',(-4.1876824466558,5.62945433217017,-0.8203403587989));
#78911=CARTESIAN_POINT('Ctrl Pts',(-4.06841647423864,3.73550405733429,4.29065540680006));
#78912=CARTESIAN_POINT('Ctrl Pts',(-3.94915050182147,-1.58757379261008,
5.46290434066727));
#78913=CARTESIAN_POINT('Ctrl Pts',(-3.82988452940431,-5.45328658921714,
1.62030236626634));
#78914=CARTESIAN_POINT('Ctrl Pts',(-3.71061855698715,-4.31297740564767,
-3.7097089212816));
#78915=CARTESIAN_POINT('Ctrl Pts',(-3.59135258456998,0.786569815286035,
-5.63427211873411));
#78916=CARTESIAN_POINT('Ctrl Pts',(-3.47208661215282,5.16405966405615,-2.38667177641422));
#78917=CARTESIAN_POINT('Ctrl Pts',(-3.35282063973565,4.80103280564923,3.05185163160719));
#78918=CARTESIAN_POINT('Ctrl Pts',(-3.23355466731848,0.0307415646677118,
5.68882846801215));
#78919=CARTESIAN_POINT('Ctrl Pts',(-3.11428869490132,-4.76776989652671,
3.10355998750428));
#78920=CARTESIAN_POINT('Ctrl Pts',(-2.99502272248416,-5.18955174559502,
-2.33072243350754));
#78921=CARTESIAN_POINT('Ctrl Pts',(-2.87575675006699,-0.84741560123151,
-5.62544230981467));
#78922=CARTESIAN_POINT('Ctrl Pts',(-2.75649077764983,4.27263328560509,-3.75610425694008));
#78923=CARTESIAN_POINT('Ctrl Pts',(-2.63722480523266,5.47047933364981,1.56127199500084));
#78924=CARTESIAN_POINT('Ctrl Pts',(-2.5179588328155,1.64652076198106,5.44542778508989));
#78925=CARTESIAN_POINT('Ctrl Pts',(-2.39869286039833,-3.68891515283567,
4.3307758401288));
#78926=CARTESIAN_POINT('Ctrl Pts',(-2.27942688798117,-5.63799129433396,
-0.759452794634447));
#78927=CARTESIAN_POINT('Ctrl Pts',(-2.16016091556401,-2.41148975772396,
-5.15251700925442));
#78928=CARTESIAN_POINT('Ctrl Pts',(-2.04089494314684,3.02871731858882,-4.81566047249431));
#78929=CARTESIAN_POINT('Ctrl Pts',(-1.92162897072967,5.68861471915913,-0.058111610111389));
#78930=CARTESIAN_POINT('Ctrl Pts',(-1.80236299831251,3.12646302053577,4.75278269685096));
#78931=CARTESIAN_POINT('Ctrl Pts',(-1.68309702589535,-2.30572720347124,
5.20070537960349));
#78932=CARTESIAN_POINT('Ctrl Pts',(-1.56383105347818,-5.62130006801447,
0.874471227430688));
#78933=CARTESIAN_POINT('Ctrl Pts',(-1.44456508106102,-3.77661750910527,
-4.25451226019894));
#78934=CARTESIAN_POINT('Ctrl Pts',(-1.32529910864385,1.53493405659396,-5.47792769431762));
#78935=CARTESIAN_POINT('Ctrl Pts',(-1.20603313622669,5.43744292854874,-1.67270104353375));
#78936=CARTESIAN_POINT('Ctrl Pts',(-1.08676716380952,4.34847402449726,3.66803599226292));
#78937=CARTESIAN_POINT('Ctrl Pts',(-0.967501191392359,-0.73231819393922,
5.64157996000141));
#78938=CARTESIAN_POINT('Ctrl Pts',(-0.848235218975195,-5.14085508242627,
2.43625191713739));
#78939=CARTESIAN_POINT('Ctrl Pts',(-0.728969246558032,-4.83017666497017,
-3.00551289590335));
#78940=CARTESIAN_POINT('Ctrl Pts',(-0.609703274140865,-0.0854803103699123,
-5.68826928852731));
#78941=CARTESIAN_POINT('Ctrl Pts',(-0.490437301723702,4.7376854783199,-3.14929368125304));
#78942=CARTESIAN_POINT('Ctrl Pts',(-0.371171329306535,5.21173862610644,
2.28067859976231));
#78943=CARTESIAN_POINT('Ctrl Pts',(-0.251905356889374,0.901506611104705,
5.61702770265542));
#78944=CARTESIAN_POINT('Ctrl Pts',(-0.132639384472207,-4.23629275005268,
3.79704333898294));
#78945=CARTESIAN_POINT('Ctrl Pts',(-0.0133734120550438,-5.48524925025369,
-1.50856058706799));
#78946=CARTESIAN_POINT('Ctrl Pts',(0.105892560362122,-1.69884260489541,
-5.42933220442958));
#78947=CARTESIAN_POINT('Ctrl Pts',(0.225158532779286,3.64707192288057,-4.36607154907015));
#78948=CARTESIAN_POINT('Ctrl Pts',(0.344424505196449,5.64503803266485,0.705166641320319));
#78949=CARTESIAN_POINT('Ctrl Pts',(0.463690477613616,2.46095768145258,5.12907415352552));
#78950=CARTESIAN_POINT('Ctrl Pts',(0.582956450030778,-2.98223890069384,
4.84458104705164));
#78951=CARTESIAN_POINT('Ctrl Pts',(0.702222422447946,-5.68779218411275,
0.112847031904288));
#78952=CARTESIAN_POINT('Ctrl Pts',(0.821488394865107,-3.17205144116504,
-4.72247859040851));
#78953=CARTESIAN_POINT('Ctrl Pts',(0.940754367282274,2.25557720221346,-5.22265122970302));
#78954=CARTESIAN_POINT('Ctrl Pts',(1.06002033969944,5.61262531263547,-0.928521126430262));
#78955=CARTESIAN_POINT('Ctrl Pts',(1.1792863121166,3.81738127374981,4.21797517691703));
#78956=CARTESIAN_POINT('Ctrl Pts',(1.29855228453377,-1.48215219692403,5.49244383197651));
#78957=CARTESIAN_POINT('Ctrl Pts',(1.41781825695093,-5.42109580048183,1.72494484093319));
#78958=CARTESIAN_POINT('Ctrl Pts',(1.5370842293681,-4.38356800649465,-3.62602342997124));
#78959=CARTESIAN_POINT('Ctrl Pts',(1.65635020178526,0.677998765290155,-5.64836543227584));
#78960=CARTESIAN_POINT('Ctrl Pts',(1.77561617420243,5.1171744952606,-2.48560647877295));
#78961=CARTESIAN_POINT('Ctrl Pts',(1.89488214661959,4.85887328530176,2.95889587171378));
#78962=CARTESIAN_POINT('Ctrl Pts',(2.01414811903676,0.140211141221322,5.68718341695967));
#78963=CARTESIAN_POINT('Ctrl Pts',(2.13341409145392,-4.70716238513036,3.1947357734682));
#78964=CARTESIAN_POINT('Ctrl Pts',(2.25268006387108,-5.23344293778499,-2.23042359187943));
#78965=CARTESIAN_POINT('Ctrl Pts',(2.37194603628825,-0.955514148067151,
-5.60809299986253));
#78966=CARTESIAN_POINT('Ctrl Pts',(2.49121200870541,4.19955996481265,-3.83763084261715));
#78967=CARTESIAN_POINT('Ctrl Pts',(2.61047798112258,5.49951127294373,1.4557094974715));
#78968=CARTESIAN_POINT('Ctrl Pts',(2.72974395353974,1.75100714742461,5.41273390736434));
#78969=CARTESIAN_POINT('Ctrl Pts',(2.84900992595691,-3.60489100077176,4.40096299175742));
#78970=CARTESIAN_POINT('Ctrl Pts',(2.96827589837407,-5.65156208181073,-0.650815194738936));
#78971=CARTESIAN_POINT('Ctrl Pts',(3.08754187079124,-2.51019773852067,-5.1051563830885));
#78972=CARTESIAN_POINT('Ctrl Pts',(3.2068078432084,2.93548434931463,-4.87305304887937));
#78973=CARTESIAN_POINT('Ctrl Pts',(3.32607381562557,5.68644300116001,-0.167572004888354));
#78974=CARTESIAN_POINT('Ctrl Pts',(3.44533978804273,3.21734615305874,4.69173721702972));
#78975=CARTESIAN_POINT('Ctrl Pts',(3.5646057604599,-2.20521835102361,5.24411350054252));
#78976=CARTESIAN_POINT('Ctrl Pts',(3.68387173287706,-5.60343086925195,0.982485051172806));
#78977=CARTESIAN_POINT('Ctrl Pts',(3.80313770529422,-3.85779157684188,-4.18104754002049));
#78978=CARTESIAN_POINT('Ctrl Pts',(3.92240367771139,1.42923310081396,-5.50645140955604));
#78979=CARTESIAN_POINT('Ctrl Pts',(4.04166965012854,5.4042467186407,-1.77702892107158));
#78980=CARTESIAN_POINT('Ctrl Pts',(4.16093562254572,4.41825610219412,3.58367512446205));
#78981=CARTESIAN_POINT('Ctrl Pts',(4.28020159496288,-0.623616558920145,
5.65462790727246));
#78982=CARTESIAN_POINT('Ctrl Pts',(4.39946756738005,-5.09302009520808,2.53473089144989));
#78983=CARTESIAN_POINT('Ctrl Pts',(4.51873353979721,-4.88712000954709,-2.91200487543344));
#78984=CARTESIAN_POINT('Ctrl Pts',(4.63799951221437,-0.194928989547843,
-5.68557095385308));
#78985=CARTESIAN_POINT('Ctrl Pts',(4.75726548463154,4.67620344317297,-3.23988205654479));
#78986=CARTESIAN_POINT('Ctrl Pts',(4.8765314570487,5.25466267097029,2.17996206310455));
#78987=CARTESIAN_POINT('Ctrl Pts',(4.99579742946587,1.00943321141648,5.59863902872416));
#78988=CARTESIAN_POINT('Ctrl Pts',(5.11506340188303,-4.16243833107186,3.8778630097371));
#78989=CARTESIAN_POINT('Ctrl Pts',(5.23432937430019,-5.51326408116101,-1.40272361983516));
#78990=CARTESIAN_POINT('Ctrl Pts',(5.35359534671737,-1.80300955951409,-5.39563443077501));
#78991=CARTESIAN_POINT('Ctrl Pts',(5.47286131913451,3.5623762921537,-4.4354469374985));
#78992=CARTESIAN_POINT('Ctrl Pts',(5.5921272915517,5.65756283769236,0.596403487436154));
#78993=CARTESIAN_POINT('Ctrl Pts',(5.71139326396885,2.55920536965963,5.08076591255386));
#78994=CARTESIAN_POINT('Ctrl Pts',(5.83065923638603,-2.88845799358026,4.90107384167857));
#78995=CARTESIAN_POINT('Ctrl Pts',(5.94992520880318,-5.6845672952253,0.222281461931913));
#78996=CARTESIAN_POINT('Ctrl Pts',(6.06919118122036,-3.26234296225833,-4.66056142314072));
#78997=CARTESIAN_POINT('Ctrl Pts',(6.1884571536375,2.15465531276254,-5.26509020487283));
#78998=CARTESIAN_POINT('Ctrl Pts',(6.30772312605469,5.59371758920206,-1.03635800499401));
#78999=CARTESIAN_POINT('Ctrl Pts',(6.42698909847184,3.89784467668328,4.14373276873832));
#79000=CARTESIAN_POINT('Ctrl Pts',(6.546255070889,-1.3761816681846,5.51994913005693));
#79001=CARTESIAN_POINT('Ctrl Pts',(6.66552104330618,-5.38689724312701,1.82894846134447));
#79002=CARTESIAN_POINT('Ctrl Pts',(6.78478701572333,-4.45253509973197,-3.54099499687852));
#79003=CARTESIAN_POINT('Ctrl Pts',(6.9040529881405,0.569176610223374,-5.66036680513182));
#79004=CARTESIAN_POINT('Ctrl Pts',(7.02331896055767,5.06839411878929,-2.58362060660727));
#79005=CARTESIAN_POINT('Ctrl Pts',(7.14258493297483,4.91491422226634,2.86484424882539));
#79006=CARTESIAN_POINT('Ctrl Pts',(7.26185090539199,0.249628788877266,5.68343204850972));
#79007=CARTESIAN_POINT('Ctrl Pts',(7.38111687780916,-4.64481151901909,3.28472835026752));
#79008=CARTESIAN_POINT('Ctrl Pts',(7.50038285022633,-5.27539586087048,-2.12929868580585));
#79009=CARTESIAN_POINT('Ctrl Pts',(7.61964882264348,-1.0632588086421,-5.58866666460871));
#79010=CARTESIAN_POINT('Ctrl Pts',(7.73891479506065,4.12493128602183,-3.91773611513867));
#79011=CARTESIAN_POINT('Ctrl Pts',(7.85818076747781,5.52650640149627,1.3496078602634));
#79012=CARTESIAN_POINT('Ctrl Pts',(7.97744673989498,1.85484502612115,5.37803535794785));
#79013=CARTESIAN_POINT('Ctrl Pts',(8.09671271231215,-3.51953173357715,4.4695201933325));
#79014=CARTESIAN_POINT('Ctrl Pts',(8.21597868472931,-5.66303974468377,-0.541936557537787));
#79015=CARTESIAN_POINT('Ctrl Pts',(8.33524465714647,-2.60797603712152,-5.05590500030049));
#79016=CARTESIAN_POINT('Ctrl Pts',(8.45451062956364,2.84116418778695,-4.92864083092901));
#79017=CARTESIAN_POINT('Ctrl Pts',(8.5737766019808,5.68216523998536,-0.276970337339723));
#79018=CARTESIAN_POINT('Ctrl Pts',(8.69304257439796,3.30703770238863,4.62895409539172));
#79019=CARTESIAN_POINT('Ctrl Pts',(8.81230854681514,-2.10389276919738,5.28557940040471));
#79020=CARTESIAN_POINT('Ctrl Pts',(8.9315745192323,-5.58348637186443,1.09013499965285));
#79021=CARTESIAN_POINT('Ctrl Pts',(9.05084049164945,-3.93753686465025,-4.10603431814493));
#79022=CARTESIAN_POINT('Ctrl Pts',(9.17010646406663,1.32300281121011,-5.53293574368922));
#79023=CARTESIAN_POINT('Ctrl Pts',(9.28937243648379,5.36904898037513,-1.88069865438264));
#79024=CARTESIAN_POINT('Ctrl Pts',(9.40863840890096,4.48640182512404,3.4979869990878));
#79025=CARTESIAN_POINT('Ctrl Pts',(9.52790438131812,-0.514683959940392,
5.6655815944741));
#79026=CARTESIAN_POINT('Ctrl Pts',(9.64717035373528,-5.0432988461893,2.63227109741554));
#79027=CARTESIAN_POINT('Ctrl Pts',(9.76643632615245,-4.94225334991895,-2.81741835861816));
#79028=CARTESIAN_POINT('Ctrl Pts',(9.88570229856962,-0.304305474408852,
-5.68076689897664));
#79029=CARTESIAN_POINT('Ctrl Pts',(10.0049682709868,4.61298951933098,-3.32927050219805));
#79030=CARTESIAN_POINT('Ctrl Pts',(10.124234243404,5.29564058774396,2.07843815104094));
#79031=CARTESIAN_POINT('Ctrl Pts',(10.2435002158211,1.11698595588803,5.57817683088416));
#79032=CARTESIAN_POINT('Ctrl Pts',(10.3627661882383,-4.08704230254025,3.95724646686431));
#79033=CARTESIAN_POINT('Ctrl Pts',(10.4820321606554,-5.53923700780752,-1.29636713688644));
#79034=CARTESIAN_POINT('Ctrl Pts',(10.6012981330726,-1.90650874766131,-5.3599383184282));
#79035=CARTESIAN_POINT('Ctrl Pts',(10.7205641054898,3.47636129213444,-4.50317960432547));
#79036=CARTESIAN_POINT('Ctrl Pts',(10.8398300779069,5.66799229566339,0.487419448282535));
#79037=CARTESIAN_POINT('Ctrl Pts',(10.9590960503241,2.65650522509982,5.03057594826689));
#79038=CARTESIAN_POINT('Ctrl Pts',(11.0783620227412,-2.79360731099475,4.95575146412935));
#79039=CARTESIAN_POINT('Ctrl Pts',(11.1976279951584,-5.6792370578528,0.331633567322531));
#79040=CARTESIAN_POINT('Ctrl Pts',(11.3168939675756,-3.35142623504413,-4.59691816038984));
#79041=CARTESIAN_POINT('Ctrl Pts',(11.4361599399928,2.05293542056789,-5.30557918998872));
#79042=CARTESIAN_POINT('Ctrl Pts',(11.5554259124099,5.57273816457474,-1.14381105579353));
#79043=CARTESIAN_POINT('Ctrl Pts',(11.6746918848271,3.976864465537,4.06795567884079));
#79044=CARTESIAN_POINT('Ctrl Pts',(11.7939578572443,-1.26970145386314,5.5454100479876));
#79045=CARTESIAN_POINT('Ctrl Pts',(11.9132238296614,-5.35070358300338,1.93227470849723));
#79046=CARTESIAN_POINT('Ctrl Pts',(12.0324898020786,-4.51985314255969,-3.45465511331554));
#79047=CARTESIAN_POINT('Ctrl Pts',(12.1517557744957,0.460143653691493,-5.670271792448));
#79048=CARTESIAN_POINT('Ctrl Pts',(12.2710217469129,5.01773660104659,-2.68067785919545));
#79049=CARTESIAN_POINT('Ctrl Pts',(12.3902877193301,4.96913486110191,2.76973159610198));
#79050=CARTESIAN_POINT('Ctrl Pts',(12.5095536917472,0.358953983481827,5.67757575202713));
#79051=CARTESIAN_POINT('Ctrl Pts',(12.6288196641644,-4.5807403905928,3.37350438805925));
#79052=CARTESIAN_POINT('Ctrl Pts',(12.7480856365816,-5.31539497707732,-2.027385168123));
#79053=CARTESIAN_POINT('Ctrl Pts',(12.8673516089987,-1.17060967841375,-5.56717049883224));
#79054=CARTESIAN_POINT('Ctrl Pts',(12.9866175814159,4.04877488886951,-3.99639040654476));
#79055=CARTESIAN_POINT('Ctrl Pts',(13.1058835538331,5.55145472133397,1.24300637940549));
#79056=CARTESIAN_POINT('Ctrl Pts',(13.2251495262502,1.95799594045214,5.34134498786934));
#79057=CARTESIAN_POINT('Ctrl Pts',(13.3444154986674,-3.43286896509233,4.53642205386241));
#79058=CARTESIAN_POINT('Ctrl Pts',(13.4636814710845,-5.67242003206137,-0.4328572075556));
#79059=CARTESIAN_POINT('Ctrl Pts',(13.5829474435017,-2.70478844014697,-5.00478110173774));
#79060=CARTESIAN_POINT('Ctrl Pts',(13.7022134159189,2.74579176662222,-4.98240323103349));
#79061=CARTESIAN_POINT('Ctrl Pts',(13.8214793883361,5.67578301995597,-0.386266090465443));
#79062=CARTESIAN_POINT('Ctrl Pts',(13.9407453607532,3.39550445017166,4.56445658442803));
#79063=CARTESIAN_POINT('Ctrl Pts',(14.0600113331704,-2.00178798515141,5.32508772179077));
#79064=CARTESIAN_POINT('Ctrl Pts',(14.1792773055875,-5.5614739625385,1.19738120340612));
#79065=CARTESIAN_POINT('Ctrl Pts',(14.2985432780047,-4.0158238378954,-4.02950037662921));
#79066=CARTESIAN_POINT('Ctrl Pts',(14.4178092504218,1.21628253145922,-5.55737088792268));
#79067=CARTESIAN_POINT('Ctrl Pts',(14.537075222839,5.33186274966146,-1.9836718481232));
#79068=CARTESIAN_POINT('Ctrl Pts',(14.6563411952562,4.55288595469166,3.41100335177722));
#79069=CARTESIAN_POINT('Ctrl Pts',(14.7756071676734,-0.405560741509822,
5.67443696477539));
#79070=CARTESIAN_POINT('Ctrl Pts',(14.8948731400905,-4.99170975023798,2.72883640983535));
#79071=CARTESIAN_POINT('Ctrl Pts',(15.0141391125077,-4.99555626678405,-2.72178837672192));
#79072=CARTESIAN_POINT('Ctrl Pts',(15.1334050849249,-0.413569256044401,
-5.67385890313799));
#79073=CARTESIAN_POINT('Ctrl Pts',(15.252671057342,4.54806711883782,-3.41742591211722));
#79074=CARTESIAN_POINT('Ctrl Pts',(15.3719370297592,5.33465719975868,1.97614446418445));
#79075=CARTESIAN_POINT('Ctrl Pts',(15.4912030021763,1.2241250110552,5.55564868755867));
#79076=CARTESIAN_POINT('Ctrl Pts',(15.6104689745935,-4.01013258829202,4.03516430973787));
#79077=CARTESIAN_POINT('Ctrl Pts',(15.7297349470107,-5.56315841080468,-1.18953052863603));
#79078=CARTESIAN_POINT('Ctrl Pts',(15.8490009194279,-2.00930183715662,-5.3222570878775));
#79079=CARTESIAN_POINT('Ctrl Pts',(15.968266891845,3.38905877952192,-4.56924446393595));
#79080=CARTESIAN_POINT('Ctrl Pts',(16.0875328642622,5.67632254390165,0.378254887421002));
#79081=CARTESIAN_POINT('Ctrl Pts',(16.2067988366793,2.75282121159081,4.97852284912694));
#79082=CARTESIAN_POINT('Ctrl Pts',(16.3260648090965,-2.69772198203872,5.00859366388301));
#79083=CARTESIAN_POINT('Ctrl Pts',(16.4453307815137,-5.67180344611339,0.440862848196796));
#79084=CARTESIAN_POINT('Ctrl Pts',(16.5645967539308,-3.43926826645123,-4.53157237321053));
#79085=CARTESIAN_POINT('Ctrl Pts',(16.683862726348,1.95045519882603,-5.34410318946374));
#79086=CARTESIAN_POINT('Ctrl Pts',(16.8031286987652,5.54969480873816,-1.25084048228728));
#79087=CARTESIAN_POINT('Ctrl Pts',(16.9223946711823,4.05441137437299,3.99067197218942));
#79088=CARTESIAN_POINT('Ctrl Pts',(17.0416606435995,-1.16275099019935,5.56881715600848));
#79089=CARTESIAN_POINT('Ctrl Pts',(17.1609266160167,-5.31252822487239,2.03488531426176));
#79090=CARTESIAN_POINT('Ctrl Pts',(17.2801925884338,-4.58549720292351,-3.36703575630613));
#79091=CARTESIAN_POINT('Ctrl Pts',(17.399458560851,0.350940277373286,-5.67807672579202));
#79092=CARTESIAN_POINT('Ctrl Pts',(17.5187245332682,4.96522070365914,-2.77674229020602));
#79093=CARTESIAN_POINT('Ctrl Pts',(17.6379905056853,5.02151512053671,2.67359313966889));
#79094=CARTESIAN_POINT('Ctrl Pts',(17.7572564781025,0.468146235122306,5.66961669646236));
#79095=CARTESIAN_POINT('Ctrl Pts',(17.8765224505196,-4.51497272937164,3.46103100756037));
#79096=CARTESIAN_POINT('Ctrl Pts',(17.9957884229368,-5.35342547224728,-1.92472078373913));
#79097=CARTESIAN_POINT('Ctrl Pts',(18.115054395354,-1.27752699868453,-5.54361246389897));
#79098=CARTESIAN_POINT('Ctrl Pts',(18.2343203677711,3.97111897880176,-4.07356458626403));
#79099=CARTESIAN_POINT('Ctrl Pts',(18.3535863401883,5.57434699254372,1.13594453605012));
#79100=CARTESIAN_POINT('Ctrl Pts',(18.4728523126054,2.06042168722449,5.3026763858526));
#79101=CARTESIAN_POINT('Ctrl Pts',(18.5921182850226,-3.34493479192551,4.60164379543117));
#79102=CARTESIAN_POINT('Ctrl Pts',(18.7113842574398,-5.67969946984019,-0.323617543653628));
#79103=CARTESIAN_POINT('Ctrl Pts',(18.8306502298569,-2.80059909194854,-4.95180362175652));
#79104=CARTESIAN_POINT('Ctrl Pts',(18.9499162022741,2.64940240815424,-5.03432033763551));
#79105=CARTESIAN_POINT('Ctrl Pts',(19.0691821746913,5.66729870480444,-0.495418785256739));
#79106=CARTESIAN_POINT('Ctrl Pts',(19.1884481471084,3.48271363167404,4.4982685715746));
#79107=CARTESIAN_POINT('Ctrl Pts',(19.3077141195256,-1.8989418146318,5.36262383231444));
#79108=CARTESIAN_POINT('Ctrl Pts',(19.4269800919428,-5.5374017938371,1.3041839424993));
#79109=CARTESIAN_POINT('Ctrl Pts',(19.54624606436,-4.09262350204653,-3.95147406074749));
#79110=CARTESIAN_POINT('Ctrl Pts',(19.6655120367771,1.10911178671227,-5.57974779240423));
#79111=CARTESIAN_POINT('Ctrl Pts',(19.7847780091943,5.29270179887156,-2.08591036492105));
#79112=CARTESIAN_POINT('Ctrl Pts',(19.9040439816114,4.61768386769258,3.32275639797979));
#79113=CARTESIAN_POINT('Ctrl Pts',(20.0233099540286,-0.296287318736919,
5.68119073848253));
#79114=CARTESIAN_POINT('Ctrl Pts',(20.1425759264458,-4.93827191400179,2.82439106457381));
#79115=CARTESIAN_POINT('Ctrl Pts',(20.2618418988629,-5.04700901876023,-2.62515034746904));
#79116=CARTESIAN_POINT('Ctrl Pts',(20.3811078712801,-0.522679867286884,
-5.66484952479737));
#79117=CARTESIAN_POINT('Ctrl Pts',(20.5003738436973,4.48146028649235,-3.50431563687621));
#79118=CARTESIAN_POINT('Ctrl Pts',(20.6196398161144,5.37169805673866,1.87311888824337));
#79119=CARTESIAN_POINT('Ctrl Pts',(20.7389057885316,1.33081069666864,5.53106294231917));
#79120=CARTESIAN_POINT('Ctrl Pts',(20.8581717609487,-3.93173767277321,4.11158768053889));
#79121=CARTESIAN_POINT('Ctrl Pts',(20.9774377333659,-5.5850194305705,-1.08225336331834));
#79122=CARTESIAN_POINT('Ctrl Pts',(21.0967037057831,-2.11135075733188,-5.28260469482414));
#79123=CARTESIAN_POINT('Ctrl Pts',(21.2159696782002,3.3005010878612,-4.63361704840726));
#79124=CARTESIAN_POINT('Ctrl Pts',(21.3352356506174,5.68255049719854,0.268950235271458));
#79125=CARTESIAN_POINT('Ctrl Pts',(21.4545016230346,2.84811765733817,4.92462589363116));
#79126=CARTESIAN_POINT('Ctrl Pts',(21.5737675954518,-2.60083751900743,5.05958087018941));
#79127=CARTESIAN_POINT('Ctrl Pts',(21.6930335678689,-5.66226921313533,0.549928850164967));
#79128=CARTESIAN_POINT('Ctrl Pts',(21.8122995402861,-3.52583652311729,-4.46454826320829));
#79129=CARTESIAN_POINT('Ctrl Pts',(21.9315655127032,1.84725260233084,-5.38064793546701));
#79130=CARTESIAN_POINT('Ctrl Pts',(22.0508314851204,5.52459605607864,-1.35740664482838));
#79131=CARTESIAN_POINT('Ctrl Pts',(22.1700974575375,4.1304566827527,3.91191027174289));
#79132=CARTESIAN_POINT('Ctrl Pts',(22.2893634299547,-1.05536988759536,5.59016178501306));
#79133=CARTESIAN_POINT('Ctrl Pts',(22.4086294023719,-5.272385307441,2.13674227555503));
#79134=CARTESIAN_POINT('Ctrl Pts',(22.5278953747891,-4.64944296874926,-3.27816937674247));
#79135=CARTESIAN_POINT('Ctrl Pts',(22.6471613472062,0.241606926064419,-5.68377871451211));
#79136=CARTESIAN_POINT('Ctrl Pts',(22.7664273196234,4.91086587652667,-2.87177832101119));
#79137=CARTESIAN_POINT('Ctrl Pts',(22.8856932920405,5.07203560090617,2.57646448557016));
#79138=CARTESIAN_POINT('Ctrl Pts',(23.0049592644577,0.577165103123198,5.65955782954818));
#79139=CARTESIAN_POINT('Ctrl Pts',(23.1242252368749,-4.44753289320691,3.54727579222515));
#79140=CARTESIAN_POINT('Ctrl Pts',(23.243491209292,-5.38947326132513,-1.82134355565483));
#79141=CARTESIAN_POINT('Ctrl Pts',(23.3627571817092,-1.38397117132737,-5.51800128481301));
#79142=CARTESIAN_POINT('Ctrl Pts',(23.4820231541263,3.8919923166271,-4.14923007190245));
#79143=CARTESIAN_POINT('Ctrl Pts',(23.6012891265436,5.59517473669525,1.02846198185014));
#79144=CARTESIAN_POINT('Ctrl Pts',(23.7205550989607,2.16208433181988,5.26204387328368));
#79145=CARTESIAN_POINT('Ctrl Pts',(23.8398210713778,-3.2557617815647,4.66516126237524));
#79146=CARTESIAN_POINT('Ctrl Pts',(23.9590870437951,-5.68487536199228,-0.214258024066976));
#79147=CARTESIAN_POINT('Ctrl Pts',(24.0783530162122,-2.89537250788858,-4.89699218120943));
#79148=CARTESIAN_POINT('Ctrl Pts',(24.1976189886294,2.55203181135149,-5.08437292260451));
#79149=CARTESIAN_POINT('Ctrl Pts',(24.3168849610465,5.65671543680001,-0.60438799568858));
#79150=CARTESIAN_POINT('Ctrl Pts',(24.4361509334637,3.56863294791704,4.43041457036519));
#79151=CARTESIAN_POINT('Ctrl Pts',(24.5554169058808,-1.79539234796575,5.39817383002159));
#79152=CARTESIAN_POINT('Ctrl Pts',(24.674682878298,-5.51127878118019,1.41050366124196));
#79153=CARTESIAN_POINT('Ctrl Pts',(24.7939488507152,-4.167907413416,-3.87198426849273));
#79154=CARTESIAN_POINT('Ctrl Pts',(24.9132148231323,1.0015302689549,-5.60005816957561));
#79155=CARTESIAN_POINT('Ctrl Pts',(25.0324807955495,5.25158063173888,-2.18737633950104));
#79156=CARTESIAN_POINT('Ctrl Pts',(25.1517467679667,4.68077156543346,3.23327882102573));
#79157=CARTESIAN_POINT('Ctrl Pts',(25.2710127403838,-0.186904162359676,
5.68584041425328));
#79158=CARTESIAN_POINT('Ctrl Pts',(25.390278712801,-4.88300512883198,2.9188996718052));
#79159=CARTESIAN_POINT('Ctrl Pts',(25.5095446852182,-5.09659254969641,-2.52754006192641));
#79160=CARTESIAN_POINT('Ctrl Pts',(25.6288106576353,-0.631596897697456,
-5.65374210068714));
#79161=CARTESIAN_POINT('Ctrl Pts',(25.7480766300525,4.4131936909433,-3.58990749581131));
#79162=CARTESIAN_POINT('Ctrl Pts',(25.8673426024697,5.40674944015302,1.76939957999003));
#79163=CARTESIAN_POINT('Ctrl Pts',(25.9866085748868,1.43700350039011,5.50442870079447));
#79164=CARTESIAN_POINT('Ctrl Pts',(26.105874547304,-3.85188659049215,4.18648827494485));
#79165=CARTESIAN_POINT('Ctrl Pts',(26.2251405197212,-5.60481197061107,-0.974575372333387));
#79166=CARTESIAN_POINT('Ctrl Pts',(26.3444064921383,-2.21261771313111,-5.24099582501282));
#79167=CARTESIAN_POINT('Ctrl Pts',(26.4636724645555,3.21072101556802,-4.69627351657181));
#79168=CARTESIAN_POINT('Ctrl Pts',(26.5829384369726,5.68667384895602,0.159545974138274));
#79169=CARTESIAN_POINT('Ctrl Pts',(26.7022044093899,2.94235926814676,4.86890504317082));
#79170=CARTESIAN_POINT('Ctrl Pts',(26.821470381807,-2.50298980423744,5.10869419931819));
#79171=CARTESIAN_POINT('Ctrl Pts',(26.9407363542241,-5.65063789003752,0.658791179309665));
#79172=CARTESIAN_POINT('Ctrl Pts',(27.0600023266413,-3.61109894343789,-4.39587065357536));
#79173=CARTESIAN_POINT('Ctrl Pts',(27.1792682990585,1.74336585341623,-5.41519989320858));
#79174=CARTESIAN_POINT('Ctrl Pts',(27.2985342714756,5.49745120222388,-1.4634700753453));
#79175=CARTESIAN_POINT('Ctrl Pts',(27.4178002438928,4.2049722263732,3.83169974785256));
#79176=CARTESIAN_POINT('Ctrl Pts',(27.53706621631,-0.947597915945529,5.60943602975911));
#79177=CARTESIAN_POINT('Ctrl Pts',(27.6563321887271,-5.23028969812594,2.23780786841534));
#79178=CARTESIAN_POINT('Ctrl Pts',(27.7755981611443,-4.71166675694639,-3.18808888736647));
#79179=CARTESIAN_POINT('Ctrl Pts',(27.8948641335614,0.132184092698237,-5.68737564680772));
#79180=CARTESIAN_POINT('Ctrl Pts',(28.0141301059787,4.8546922506191,-2.96575075386364));
#79181=CARTESIAN_POINT('Ctrl Pts',(28.1333960783957,5.12067759133716,2.47838160658135));
#79182=CARTESIAN_POINT('Ctrl Pts',(28.252662050813,0.685970211023877,5.64740287670818));
#79183=CARTESIAN_POINT('Ctrl Pts',(28.3719280232301,-4.37844585926038,3.63220680025098));
#79184=CARTESIAN_POINT('Ctrl Pts',(28.4911939956473,-5.42352499357456,-1.71729177088093));
#79185=CARTESIAN_POINT('Ctrl Pts',(28.6104599680644,-1.48990277345135,-5.49034644698546));
#79186=CARTESIAN_POINT('Ctrl Pts',(28.7297259404816,3.81142420786515,-4.22335883982919));
#79187=CARTESIAN_POINT('Ctrl Pts',(28.8489919128988,5.61393023998058,0.920598524273739));
#79188=CARTESIAN_POINT('Ctrl Pts',(28.9682578853159,2.26294622224433,5.21946249890676));
#79189=CARTESIAN_POINT('Ctrl Pts',(29.0875238577331,-3.16538296031649,4.72695093022996));
#79190=CARTESIAN_POINT('Ctrl Pts',(29.2067898301503,-5.68794579156296,-0.104819151420763));
#79191=CARTESIAN_POINT('Ctrl Pts',(29.3260558025674,-2.9890735874826,-4.84036708017872));
#79192=CARTESIAN_POINT('Ctrl Pts',(29.4453217749846,2.45371603859621,-5.13254244835828));
#79193=CARTESIAN_POINT('Ctrl Pts',(29.5645877474018,5.64403713558418,-0.71313336369156));
#79194=CARTESIAN_POINT('Ctrl Pts',(29.6838537198189,3.65323057763945,4.36091971135265));
#79195=CARTESIAN_POINT('Ctrl Pts',(29.8031196922361,-1.69117793595491,5.43172454853918));
#79196=CARTESIAN_POINT('Ctrl Pts',(29.9223856646532,-5.48311459954228,1.51630098283608));
#79197=CARTESIAN_POINT('Ctrl Pts',(30.0416516370704,-4.24164768969385,-3.79106043987415));
#79198=CARTESIAN_POINT('Ctrl Pts',(30.1609176094876,0.89357782230812,-5.61829449724229));
#79199=CARTESIAN_POINT('Ctrl Pts',(30.2801835819047,5.20851447798661,-2.28803219270779));
#79200=CARTESIAN_POINT('Ctrl Pts',(30.3994495543219,4.74212568261973,3.14260376002165));
#79201=CARTESIAN_POINT('Ctrl Pts',(30.5187155267391,-0.0774517837577881,
5.68838427002401));
#79202=CARTESIAN_POINT('Ctrl Pts',(30.6379814991563,-4.8259298634531,3.01232722911953));
#79203=CARTESIAN_POINT('Ctrl Pts',(30.7572474715734,-5.14428849573012,-2.42899367124797));
#79204=CARTESIAN_POINT('Ctrl Pts',(30.8765134439906,-0.740280008531856,
-5.64054074457688));
#79205=CARTESIAN_POINT('Ctrl Pts',(30.9957794164077,4.34329261555279,-3.67416978893845));
#79206=CARTESIAN_POINT('Ctrl Pts',(31.1150453888249,5.43979836829653,1.66502495312906));
#79207=CARTESIAN_POINT('Ctrl Pts',(31.2343113612421,1.5426640924258,5.47575582729946));
#79208=CARTESIAN_POINT('Ctrl Pts',(31.3535773336592,-3.77060891526627,4.25983835261126));
#79209=CARTESIAN_POINT('Ctrl Pts',(31.4728433060765,-5.62252870051896,-0.866536435532014));
#79210=CARTESIAN_POINT('Ctrl Pts',(31.5921092784935,-2.31306519910814,-5.19744588879372));
#79211=CARTESIAN_POINT('Ctrl Pts',(31.7113752509108,3.11975181378185,-4.7571906628459));
#79212=CARTESIAN_POINT('Ctrl Pts',(31.8306412233278,5.6886910720407,0.0500826232173974));
#79213=CARTESIAN_POINT('Ctrl Pts',(31.9499071957451,3.03551114049219,4.81138093463942));
#79214=CARTESIAN_POINT('Ctrl Pts',(32.0691731681622,-2.40421507681752,5.15591546155158));
#79215=CARTESIAN_POINT('Ctrl Pts',(32.1884391405794,-5.63691378462165,0.767409517146029));
#79216=CARTESIAN_POINT('Ctrl Pts',(32.3077051129966,-3.69502394944088,-4.32556497989826));
#79217=CARTESIAN_POINT('Ctrl Pts',(32.4269710854137,1.63883342780062,-5.44774626595132));
#79218=CARTESIAN_POINT('Ctrl Pts',(32.5462370578309,5.46827030059994,-1.56899149195925));
#79219=CARTESIAN_POINT('Ctrl Pts',(32.665503030248,4.27793040749859,3.7500701074597));
#79220=CARTESIAN_POINT('Ctrl Pts',(32.7847690026652,-0.839474989907709,
5.62663275179595));
#79221=CARTESIAN_POINT('Ctrl Pts',(32.9040349750823,-5.18625698754698,2.33804466197375));
#79222=CARTESIAN_POINT('Ctrl Pts',(33.0233009474996,-4.77214552217987,-3.09682765058092));
#79223=CARTESIAN_POINT('Ctrl Pts',(33.1425669199166,0.0227123033492882,
-5.68886619051107));
#79224=CARTESIAN_POINT('Ctrl Pts',(33.2618328923339,4.79672063052055,-3.05862478493235));
#79225=CARTESIAN_POINT('Ctrl Pts',(33.381098864751,5.16742307667829,2.37938082888736));
#79226=CARTESIAN_POINT('Ctrl Pts',(33.5003648371682,0.794521261531888,5.63315633967645));
#79227=CARTESIAN_POINT('Ctrl Pts',(33.6196308095853,-4.30773721475356,3.71579257640827));
#79228=CARTESIAN_POINT('Ctrl Pts',(33.7388967820025,-5.45556805752349,-1.61260396625899));
#79229=CARTESIAN_POINT('Ctrl Pts',(33.8581627544197,-1.59528257200157,-5.46065819272098));
#79230=CARTESIAN_POINT('Ctrl Pts',(33.9774287268369,3.72944449189255,-4.29592343555539));
#79231=CARTESIAN_POINT('Ctrl Pts',(34.096694699254,5.63060655607218,0.812394111861771));
#79232=CARTESIAN_POINT('Ctrl Pts',(34.2159606716712,2.36297000307123,5.17494803325048));
#79233=CARTESIAN_POINT('Ctrl Pts',(34.3352266440884,-3.07383180107209,4.78698991444201));
#79234=CARTESIAN_POINT('Ctrl Pts',(34.4544926165055,-5.68890962138567,0.00465854226991125));
#79235=CARTESIAN_POINT('Ctrl Pts',(34.5737585889227,-3.08166762739048,-4.78194929045732));
#79236=CARTESIAN_POINT('Ctrl Pts',(34.6930245613398,2.35449150231328,-5.17881107472906));
#79237=CARTESIAN_POINT('Ctrl Pts',(34.812290533757,5.629268496748,-0.82161461409729));
#79238=CARTESIAN_POINT('Ctrl Pts',(34.9315565061742,3.73647518902874,4.28980973279877));
#79239=CARTESIAN_POINT('Ctrl Pts',(35.0508224785913,-1.58633717557033,5.4632635619564));
#79240=CARTESIAN_POINT('Ctrl Pts',(35.1700884510085,-5.45291968006245,1.62153672395));
#79241=CARTESIAN_POINT('Ctrl Pts',(35.2893544234257,-4.31381701990819,-3.70873254599588));
#79242=CARTESIAN_POINT('Ctrl Pts',(35.4086203958428,0.785294427576647,-5.63445002139296));
#79243=CARTESIAN_POINT('Ctrl Pts',(35.52788636826,5.16351928900528,-2.38784064536003));
#79244=CARTESIAN_POINT('Ctrl Pts',(35.6471523406771,4.80172349350685,3.05076479745392));
#79245=CARTESIAN_POINT('Ctrl Pts',(35.7664183130943,0.0320292848053549,
5.68882136388004));
#79246=CARTESIAN_POINT('Ctrl Pts',(35.8856842855114,-4.76706726540989,3.10463913404421));
#79247=CARTESIAN_POINT('Ctrl Pts',(36.0049502579287,-5.19007917494346,-2.32954767244375));
#79248=CARTESIAN_POINT('Ctrl Pts',(36.1242162303458,-0.84868898024466,-5.62525034734734));
#79249=CARTESIAN_POINT('Ctrl Pts',(36.243482202763,4.27178301087878,-3.7570713056591));
#79250=CARTESIAN_POINT('Ctrl Pts',(36.3627481751801,5.47083248363574,1.56003365830421));
#79251=CARTESIAN_POINT('Ctrl Pts',(36.4820141475973,1.64775356318288,5.44505495213162));
#79252=CARTESIAN_POINT('Ctrl Pts',(36.6012801200144,-3.68793517297259,4.33161072664821));
#79253=CARTESIAN_POINT('Ctrl Pts',(36.7205460924317,-5.63816225396792,-0.758176526943501));
#79254=CARTESIAN_POINT('Ctrl Pts',(36.8398120648488,-2.41265754168496,-5.15197109043847));
#79255=CARTESIAN_POINT('Ctrl Pts',(36.959078037266,3.02763007680679,-4.81634578333499));
#79256=CARTESIAN_POINT('Ctrl Pts',(37.0783440096831,5.68859590628108,-0.0593995470360426));
#79257=CARTESIAN_POINT('Ctrl Pts',(37.1976099821003,3.12754924515988,4.75207538677428));
#79258=CARTESIAN_POINT('Ctrl Pts',(37.3168759545174,-2.30456980569776,5.20122619173273));
#79259=CARTESIAN_POINT('Ctrl Pts',(37.4361419269346,-5.6210642102154,0.875745489588154));
#79260=CARTESIAN_POINT('Ctrl Pts',(37.5554078993518,-3.7776521925,-4.25366080203663));
#79261=CARTESIAN_POINT('Ctrl Pts',(37.674673871769,1.53383028195009,-5.47826831172611));
#79262=CARTESIAN_POINT('Ctrl Pts',(37.7939398441861,5.43680539659932,-1.67394451735641));
#79263=CARTESIAN_POINT('Ctrl Pts',(37.9132058166033,4.34979570085314,3.66707572422626));
#79264=CARTESIAN_POINT('Ctrl Pts',(38.0324717890204,-0.731974977049794,
5.64169961840002));
#79265=CARTESIAN_POINT('Ctrl Pts',(38.1517377614376,-5.13852695641803,2.43750379477149));
#79266=CARTESIAN_POINT('Ctrl Pts',(38.2710037338548,-4.83425611667699,-3.00459531183657));
#79267=CARTESIAN_POINT('Ctrl Pts',(38.3902697062719,-0.0800979232670034,
-5.68784572485145));
#79268=CARTESIAN_POINT('Ctrl Pts',(38.4896580166196,3.92206602589366,-3.57444125581233));
#79269=CARTESIAN_POINT('Ctrl Pts',(38.5691686648977,4.98803046896621,-0.430338849328192));
#79270=CARTESIAN_POINT('Ctrl Pts',(38.6089239890367,4.72850927687308,1.19359047334112));
#79271=CARTESIAN_POINT('Ctrl Pts',(38.6288016511063,4.40751902618983,1.92756012635639));
#79272=CARTESIAN_POINT('Ctrl Pts',(-17.7012016511063,2.70858201811927,-3.80079309428511));
#79273=CARTESIAN_POINT('Ctrl Pts',(-17.6813239890368,3.34151559640192,-3.34974183569964));
#79274=CARTESIAN_POINT('Ctrl Pts',(-17.6415686648977,4.36673052904853,-2.12721215393368));
#79275=CARTESIAN_POINT('Ctrl Pts',(-17.5620580166196,5.04601701997133,1.0212564078875));
#79276=CARTESIAN_POINT('Ctrl Pts',(-17.462669706272,2.76747699723466,4.77477475904616));
#79277=CARTESIAN_POINT('Ctrl Pts',(-17.3434037338548,-2.52715259554554,
4.91000977934608));
#79278=CARTESIAN_POINT('Ctrl Pts',(-17.2241377614376,-5.49214719115606,
0.531331770882378));
#79279=CARTESIAN_POINT('Ctrl Pts',(-17.1048717890205,-3.42049558996118,
-4.33171847885584));
#79280=CARTESIAN_POINT('Ctrl Pts',(-16.9856058166033,1.79375966025411,-5.22009527196343));
#79281=CARTESIAN_POINT('Ctrl Pts',(-16.8663398441861,5.35998160039607,-1.31558583001987));
#79282=CARTESIAN_POINT('Ctrl Pts',(-16.747073871769,4.00656733798903,3.79611905041868));
#79283=CARTESIAN_POINT('Ctrl Pts',(-16.6278078993518,-1.02519201225003,
5.42331051522014));
#79284=CARTESIAN_POINT('Ctrl Pts',(-16.5085419269346,-5.11563966113103,
2.07186184819784));
#79285=CARTESIAN_POINT('Ctrl Pts',(-16.3892759545175,-4.51012637032802,
-3.18144843056949));
#79286=CARTESIAN_POINT('Ctrl Pts',(-16.2700099821003,0.235660632876478,
-5.51428214619193));
#79287=CARTESIAN_POINT('Ctrl Pts',(-16.1507440096831,4.76508560831362,-2.78508122179041));
#79288=CARTESIAN_POINT('Ctrl Pts',(-16.031478037266,4.9202607269294,2.50076526427245));
#79289=CARTESIAN_POINT('Ctrl Pts',(-15.9122120648488,0.558714083441273,
5.49095834237153));
#79290=CARTESIAN_POINT('Ctrl Pts',(-15.7929460924317,-4.31571801251304,
3.4405445374493));
#79291=CARTESIAN_POINT('Ctrl Pts',(-15.6736801200144,-5.22839852259545,
-1.76822762570804));
#79292=CARTESIAN_POINT('Ctrl Pts',(-15.5544141475974,-1.34149917458011,
-5.35379846877344));
#79293=CARTESIAN_POINT('Ctrl Pts',(-15.4351481751801,3.77687238681933,-4.02467526918476));
#79294=CARTESIAN_POINT('Ctrl Pts',(-15.315882202763,5.42814130105117,0.999029412519419));
#79295=CARTESIAN_POINT('Ctrl Pts',(-15.1966162303458,2.09647099580402,5.10564263419233));
#79296=CARTESIAN_POINT('Ctrl Pts',(-15.0773502579287,-3.15972302753357,
4.52536490168926));
#79297=CARTESIAN_POINT('Ctrl Pts',(-14.9580842855115,-5.51534646773363,
-0.209118852948021));
#79298=CARTESIAN_POINT('Ctrl Pts',(-14.8388183130943,-2.80797801605581,
-4.75163516481528));
#79299=CARTESIAN_POINT('Ctrl Pts',(-14.7195523406772,2.47706526799874,-4.93223325787853));
#79300=CARTESIAN_POINT('Ctrl Pts',(-14.60028636826,5.48820584468934,-0.585127246171516));
#79301=CARTESIAN_POINT('Ctrl Pts',(-14.4810203958428,3.46126916995884,4.29911537502828));
#79302=CARTESIAN_POINT('Ctrl Pts',(-14.3617544234257,-1.74305223413087,
5.23684505989782));
#79303=CARTESIAN_POINT('Ctrl Pts',(-14.2424884510085,-5.34728208824364,
1.36724231432135));
#79304=CARTESIAN_POINT('Ctrl Pts',(-14.1232224785913,-4.04280024474373,
-3.75746503060578));
#79305=CARTESIAN_POINT('Ctrl Pts',(-14.0039565061742,0.972901714182095,
-5.43288500978274));
#79306=CARTESIAN_POINT('Ctrl Pts',(-13.884690533757,5.09549686765353,-2.12101130298848));
#79307=CARTESIAN_POINT('Ctrl Pts',(-13.7654245613399,4.54051476518803,3.13791378824016));
#79308=CARTESIAN_POINT('Ctrl Pts',(-13.6461585889227,-0.182580702264231,
5.51628874901311));
#79309=CARTESIAN_POINT('Ctrl Pts',(-13.5268926165055,-4.73807026938147,
2.83080684572858));
#79310=CARTESIAN_POINT('Ctrl Pts',(-13.4076266440883,-4.94409396410031,
-2.45330637090273));
#79311=CARTESIAN_POINT('Ctrl Pts',(-13.2883606716712,-0.611525627868499,
-5.48532712623696));
#79312=CARTESIAN_POINT('Ctrl Pts',(-13.169094699254,4.28241256936083,-3.48191324721959));
#79313=CARTESIAN_POINT('Ctrl Pts',(-13.0498287268369,5.24517071586569,1.71783626600429));
#79314=CARTESIAN_POINT('Ctrl Pts',(-12.9305627544197,1.39295362426069,5.34064204717326));
#79315=CARTESIAN_POINT('Ctrl Pts',(-12.8112967820026,-3.73797060043469,
4.0608315731711));
#79316=CARTESIAN_POINT('Ctrl Pts',(-12.6920308095854,-5.43750300647318,
-0.946751461562825));
#79317=CARTESIAN_POINT('Ctrl Pts',(-12.5727648371682,-2.14550248601868,
-5.08523316651894));
#79318=CARTESIAN_POINT('Ctrl Pts',(-12.453498864751,3.11603189769737,-4.55555951425388));
#79319=CARTESIAN_POINT('Ctrl Pts',(-12.3342328923339,5.51710334487009,0.156038320292407));
#79320=CARTESIAN_POINT('Ctrl Pts',(-12.2149669199167,2.85357014318101,4.72439569821608));
#79321=CARTESIAN_POINT('Ctrl Pts',(-12.0957009474996,-2.42949068190233,
4.95584022158971));
#79322=CARTESIAN_POINT('Ctrl Pts',(-11.9764349750824,-5.48232143283452,
0.637909854493391));
#79323=CARTESIAN_POINT('Ctrl Pts',(-11.8571690026652,-3.50247672353525,
-4.26561063348149));
#79324=CARTESIAN_POINT('Ctrl Pts',(-11.737903030248,1.69258053258732,-5.25337495483456));
#79325=CARTESIAN_POINT('Ctrl Pts',(-11.6186370578309,5.33387837945656,-1.41863268979052));
#79326=CARTESIAN_POINT('Ctrl Pts',(-11.4993710854137,4.07876890015574,3.71838964264088));
#79327=CARTESIAN_POINT('Ctrl Pts',(-11.3801051129966,-0.920579293210441,
5.44199513416622));
#79328=CARTESIAN_POINT('Ctrl Pts',(-11.2608391405794,-5.07485175088737,
2.16994400432173));
#79329=CARTESIAN_POINT('Ctrl Pts',(-11.1415731681622,-4.57049880983454,
-3.09407787631109));
#79330=CARTESIAN_POINT('Ctrl Pts',(-11.0223071957451,0.129492326291972,
-5.51779022914138));
#79331=CARTESIAN_POINT('Ctrl Pts',(-10.9030412233279,4.71061176530949,-2.87626738532846));
#79332=CARTESIAN_POINT('Ctrl Pts',(-10.7837752509108,4.96747175978485,2.40561875431596));
#79333=CARTESIAN_POINT('Ctrl Pts',(-10.6645092784936,0.664279314588377,
5.47918883299221));
#79334=CARTESIAN_POINT('Ctrl Pts',(-10.5452433060764,-4.24870995595397,
3.52295912345773));
#79335=CARTESIAN_POINT('Ctrl Pts',(-10.4259773336592,-5.26145758708642,
-1.66728561880302));
#79336=CARTESIAN_POINT('Ctrl Pts',(-10.3067113612421,-1.44427891638068,
-5.32699124150536));
#79337=CARTESIAN_POINT('Ctrl Pts',(-10.1874453888249,3.69872261043595,-4.09661181056081));
#79338=CARTESIAN_POINT('Ctrl Pts',(-10.0681794164077,5.44636128890534,0.894385815009405));
#79339=CARTESIAN_POINT('Ctrl Pts',(-9.94891344399059,2.19433529210285,5.06435286104834));
#79340=CARTESIAN_POINT('Ctrl Pts',(-9.82964747157342,-3.07205223227173,
4.58533230612251));
#79341=CARTESIAN_POINT('Ctrl Pts',(-9.71038149915626,-5.51834938593094,
-0.102943334763881));
#79342=CARTESIAN_POINT('Ctrl Pts',(-9.59111552673909,-2.89889804676615,
-4.6967187897331));
#79343=CARTESIAN_POINT('Ctrl Pts',(-9.47184955432193,2.38169114073705,-4.97898830943708));
#79344=CARTESIAN_POINT('Ctrl Pts',(-9.35258358190476,5.47592939922501,-0.690633397744341));
#79345=CARTESIAN_POINT('Ctrl Pts',(-9.23331760948761,3.54335997285394,4.23171092799982));
#79346=CARTESIAN_POINT('Ctrl Pts',(-9.11405163707043,-1.64195211018554,
5.26941842552227));
#79347=CARTESIAN_POINT('Ctrl Pts',(-8.99478566465327,-5.31998079274526,
1.46989171036448));
#79348=CARTESIAN_POINT('Ctrl Pts',(-8.87551969223611,-4.11435989135324,
-3.67896995907826));
#79349=CARTESIAN_POINT('Ctrl Pts',(-8.75625371981893,0.868171633294266,
-5.45060136962148));
#79350=CARTESIAN_POINT('Ctrl Pts',(-8.63698774740178,5.05373674003329,-2.21867578474511));
#79351=CARTESIAN_POINT('Ctrl Pts',(-8.51772177498461,4.60005965974758,3.0499554754356));
#79352=CARTESIAN_POINT('Ctrl Pts',(-8.39845580256745,-0.0763919602722595,
5.51878080229521));
#79353=CARTESIAN_POINT('Ctrl Pts',(-8.27918983015028,-4.68271709308568,
2.92146160363265));
#79354=CARTESIAN_POINT('Ctrl Pts',(-8.15992385773312,-4.99038960395785,
-2.3577083950493));
#79355=CARTESIAN_POINT('Ctrl Pts',(-8.04065788531595,-0.716971493908937,
-5.47254320698324));
#79356=CARTESIAN_POINT('Ctrl Pts',(-7.92139191289879,4.21461394311765,-3.56367879947885));
#79357=CARTESIAN_POINT('Ctrl Pts',(-7.80212594048163,5.27725728586228,1.61658059316265));
#79358=CARTESIAN_POINT('Ctrl Pts',(-7.68285996806445,1.49547047884913,5.31284719545623));
#79359=CARTESIAN_POINT('Ctrl Pts',(-7.5635939956473,-3.65913214580814,4.13201273169507));
#79360=CARTESIAN_POINT('Ctrl Pts',(-7.44432802323013,-5.45471527816404,
-0.841937354878873));
#79361=CARTESIAN_POINT('Ctrl Pts',(-7.32506205081297,-2.24296491880738,
-5.04300363358741));
#79362=CARTESIAN_POINT('Ctrl Pts',(-7.2057960783958,3.02778811730507,-4.61468052979649));
#79363=CARTESIAN_POINT('Ctrl Pts',(-7.08653010597863,5.51908446824771,0.0498388174363854));
#79364=CARTESIAN_POINT('Ctrl Pts',(-6.96726413356148,2.94395753361986,4.66860699948275));
#79365=CARTESIAN_POINT('Ctrl Pts',(-6.8479981611443,-2.33367107241249,5.00167537942653));
#79366=CARTESIAN_POINT('Ctrl Pts',(-6.72873218872715,-5.46903033465158,
0.743292993399969));
#79367=CARTESIAN_POINT('Ctrl Pts',(-6.60946621630998,-3.58391513298606,
-4.19741939707365));
#79368=CARTESIAN_POINT('Ctrl Pts',(-6.49020024389281,1.59117165504184,-5.28497398665006));
#79369=CARTESIAN_POINT('Ctrl Pts',(-6.37093427147565,5.30559061476902,-1.52101462972962));
#79370=CARTESIAN_POINT('Ctrl Pts',(-6.25166829905848,4.14956992295298,3.63920962983732));
#79371=CARTESIAN_POINT('Ctrl Pts',(-6.13240232664132,-0.815683587042184,
5.45870291930293));
#79372=CARTESIAN_POINT('Ctrl Pts',(-6.01313635422416,-5.03215379016394,
2.26720213203748));
#79373=CARTESIAN_POINT('Ctrl Pts',(-5.89387038180699,-4.62919457782091,
-3.0055506710169));
#79374=CARTESIAN_POINT('Ctrl Pts',(-5.77460440938983,0.0232845209164049,
-5.51926037675902));
#79375=CARTESIAN_POINT('Ctrl Pts',(-5.65533843697266,4.65438883554905,-2.96638531598526));
#79376=CARTESIAN_POINT('Ctrl Pts',(-5.5360724645555,5.01284537459657,2.30957972924997));
#79377=CARTESIAN_POINT('Ctrl Pts',(-5.41680649213833,0.76959728691932,5.46539086354699));
#79378=CARTESIAN_POINT('Ctrl Pts',(-5.29754051972117,-4.18012768789241,
3.60406850493881));
#79379=CARTESIAN_POINT('Ctrl Pts',(-5.17827454730401,-5.29256834925714,
-1.56572588399702));
#79380=CARTESIAN_POINT('Ctrl Pts',(-5.05900857488683,-1.5465235717021,-5.29821121866109));
#79381=CARTESIAN_POINT('Ctrl Pts',(-4.93974260246968,3.61920287233824,-4.16703105870777));
#79382=CARTESIAN_POINT('Ctrl Pts',(-4.82047663005251,5.46256420073112,0.789410937514474));
#79383=CARTESIAN_POINT('Ctrl Pts',(-4.70121065763534,2.29138686338495,5.02118746091831));
#79384=CARTESIAN_POINT('Ctrl Pts',(-4.58194468521818,-2.98324365133024,
4.64360146784524));
#79385=CARTESIAN_POINT('Ctrl Pts',(-4.46267871280103,-5.51930852375722,
0.00327031460068596));
#79386=CARTESIAN_POINT('Ctrl Pts',(-4.34341274038385,-2.98874443156363,
-4.64006293041094));
#79387=CARTESIAN_POINT('Ctrl Pts',(-4.22414676796669,2.28543492323537,-5.02389933090152));
#79388=CARTESIAN_POINT('Ctrl Pts',(-4.10488079554952,5.46162487791711,-0.795883765567264));
#79389=CARTESIAN_POINT('Ctrl Pts',(-3.98561482313236,3.62413844882069,4.16273921584765));
#79390=CARTESIAN_POINT('Ctrl Pts',(-3.86634885071519,-1.54024386905451,
5.30004019788685));
#79391=CARTESIAN_POINT('Ctrl Pts',(-3.74708287829803,-5.29070917795299,
1.57199671427794));
#79392=CARTESIAN_POINT('Ctrl Pts',(-3.62781690588086,-4.18439573476381,
-3.59911233643337));
#79393=CARTESIAN_POINT('Ctrl Pts',(-3.5085509334637,0.76312001446289,-5.4662990330664));
#79394=CARTESIAN_POINT('Ctrl Pts',(-3.38928496104654,5.01010489970247,-2.31551855301444));
#79395=CARTESIAN_POINT('Ctrl Pts',(-3.27001898862937,4.65790086637442,2.96086757461472));
#79396=CARTESIAN_POINT('Ctrl Pts',(-3.1507530162122,0.0298250744156161,
5.5192289081277));
#79397=CARTESIAN_POINT('Ctrl Pts',(-3.03148704379505,-4.62562961568883,
3.01103436277953));
#79398=CARTESIAN_POINT('Ctrl Pts',(-2.91222107137787,-5.03483699246105,
-2.26123721327999));
#79399=CARTESIAN_POINT('Ctrl Pts',(-2.79295509896072,-0.822151820856484,
-5.45773246493805));
#79400=CARTESIAN_POINT('Ctrl Pts',(-2.67368912654355,4.145254383453,-3.64412450004667));
#79401=CARTESIAN_POINT('Ctrl Pts',(-2.55442315412639,5.30738935957861,1.5147262000798));
#79402=CARTESIAN_POINT('Ctrl Pts',(-2.43515718170922,1.59743346779706,5.28308466630418));
#79403=CARTESIAN_POINT('Ctrl Pts',(-2.31589120929206,-3.57893848718462,
4.20166354915829));
#79404=CARTESIAN_POINT('Ctrl Pts',(-2.19662523687489,-5.46990732985377,
-0.736811426477842));
#79405=CARTESIAN_POINT('Ctrl Pts',(-2.07735926445773,-2.33959664231811,
-4.99890636305885));
#79406=CARTESIAN_POINT('Ctrl Pts',(-1.95809329204056,2.93842295883862,-4.67209244240168));
#79407=CARTESIAN_POINT('Ctrl Pts',(-1.8388273196234,5.51902153171351,-0.056379143830598));
#79408=CARTESIAN_POINT('Ctrl Pts',(-1.71956134720623,3.0332545936587,4.61108922548945));
#79409=CARTESIAN_POINT('Ctrl Pts',(-1.60029537478907,-2.23698715951982,
5.04565810608688));
#79410=CARTESIAN_POINT('Ctrl Pts',(-1.4810294023719,-5.45371371471264,0.848400844725927));
#79411=CARTESIAN_POINT('Ctrl Pts',(-1.36176342995474,-3.66402619597342,
-4.12767359545265));
#79412=CARTESIAN_POINT('Ctrl Pts',(-1.24249745753757,1.48917346776363,-5.31461566421181));
#79413=CARTESIAN_POINT('Ctrl Pts',(-1.12323148512041,5.27533786020922,-1.62283324344174));
#79414=CARTESIAN_POINT('Ctrl Pts',(-1.00396551270325,4.21883410217057,3.55868179158226));
#79415=CARTESIAN_POINT('Ctrl Pts',(-0.884699540286082,-0.710485782558413,
5.47338900756735));
#79416=CARTESIAN_POINT('Ctrl Pts',(-0.765433567868916,-4.98759211021465,
2.36362057392911));
#79417=CARTESIAN_POINT('Ctrl Pts',(-0.646167595451754,-4.68617586741602,
-2.91591032355664));
#79418=CARTESIAN_POINT('Ctrl Pts',(-0.526901623034587,-0.0829319081640793,
-5.51868639931506));
#79419=CARTESIAN_POINT('Ctrl Pts',(-0.407635650617423,4.5964420963982,-3.05540460984056));
#79420=CARTESIAN_POINT('Ctrl Pts',(-0.288369678200257,5.05636242128851,
2.21268532330241));
#79421=CARTESIAN_POINT('Ctrl Pts',(-0.169103705783095,0.874630229555327,
5.44956872026812));
#79422=CARTESIAN_POINT('Ctrl Pts',(-0.0498377333659291,-4.10999725881205,
3.68384307591051));
#79423=CARTESIAN_POINT('Ctrl Pts',(0.0694282390512345,-5.3217189445097,
-1.46358626360836));
#79424=CARTESIAN_POINT('Ctrl Pts',(0.188694211468401,-1.64819545325033,
-5.26746893899353));
#79425=CARTESIAN_POINT('Ctrl Pts',(0.307960183885564,3.5383427185345,-4.23590699633152));
#79426=CARTESIAN_POINT('Ctrl Pts',(0.427226156302729,5.47674398561209,0.684143692098591));
#79427=CARTESIAN_POINT('Ctrl Pts',(0.546492128719893,2.38758979173424,4.97616240307561));
#79428=CARTESIAN_POINT('Ctrl Pts',(0.665758101137058,-2.89333018989815,
4.70015081541011));
#79429=CARTESIAN_POINT('Ctrl Pts',(0.785024073554225,-5.51822351869001,
0.109482752764602));
#79430=CARTESIAN_POINT('Ctrl Pts',(0.904290045971388,-3.07748389858988,
-4.58168856747125));
#79431=CARTESIAN_POINT('Ctrl Pts',(1.02355601838855,2.18833226717407,-5.06694969027927));
#79432=CARTESIAN_POINT('Ctrl Pts',(1.14282199080572,5.445297577554,-0.9008393681789));
#79433=CARTESIAN_POINT('Ctrl Pts',(1.26208796322288,3.70357468113084,4.09222578270839));
#79434=CARTESIAN_POINT('Ctrl Pts',(1.38135393564004,-1.43796517991438,5.32869903604344));
#79435=CARTESIAN_POINT('Ctrl Pts',(1.50061990805721,-5.25947808480922,1.67351951013068));
#79436=CARTESIAN_POINT('Ctrl Pts',(1.61988588047437,-4.25288183643263,-3.51792173885636));
#79437=CARTESIAN_POINT('Ctrl Pts',(1.73915185289153,0.657785764873116,-5.47997218632601));
#79438=CARTESIAN_POINT('Ctrl Pts',(1.8584178253087,4.96461750621998,-2.41150374088671));
#79439=CARTESIAN_POINT('Ctrl Pts',(1.97768379772586,4.71401696288765,2.87068308055491));
#79440=CARTESIAN_POINT('Ctrl Pts',(2.09694977014304,0.136031063025135,5.51763290055334));
#79441=CARTESIAN_POINT('Ctrl Pts',(2.21621574256019,-4.56682898022772,3.09949194880851));
#79442=CARTESIAN_POINT('Ctrl Pts',(2.33548171497737,-5.07741966798188,-2.1639285548667));
#79443=CARTESIAN_POINT('Ctrl Pts',(2.45474768739452,-0.927027653899548,
-5.44090038544007));
#79444=CARTESIAN_POINT('Ctrl Pts',(2.57401365981169,4.07435957852114,-3.72322055488116));
#79445=CARTESIAN_POINT('Ctrl Pts',(2.69327963222886,5.33555577723577,1.4123108097663));
#79446=CARTESIAN_POINT('Ctrl Pts',(2.81254560464602,1.69880482787383,5.25136548263106));
#79447=CARTESIAN_POINT('Ctrl Pts',(2.93181157706318,-3.49741932525881,4.2697582295351));
#79448=CARTESIAN_POINT('Ctrl Pts',(3.05107754948035,-5.48307353498178,-0.631412611023234));
#79449=CARTESIAN_POINT('Ctrl Pts',(3.17034352189751,-2.43536186781919,-4.95295768689262));
#79450=CARTESIAN_POINT('Ctrl Pts',(3.28960949431468,2.84796951976903,-4.72777398887077));
#79451=CARTESIAN_POINT('Ctrl Pts',(3.40887546673184,5.51691455857687,-0.162576224397382));
#79452=CARTESIAN_POINT('Ctrl Pts',(3.528141439149,3.12142825104746,4.55186367864189));
#79453=CARTESIAN_POINT('Ctrl Pts',(3.64740741156617,-2.13947475128482,5.08777211203403));
#79454=CARTESIAN_POINT('Ctrl Pts',(3.76667338398333,-5.43637724571383,0.953194480502964));
#79455=CARTESIAN_POINT('Ctrl Pts',(3.88593935640051,-3.74278024239289,-4.05639905982263));
#79456=CARTESIAN_POINT('Ctrl Pts',(4.00520532881766,1.38662374701919,-5.34228900936473));
#79457=CARTESIAN_POINT('Ctrl Pts',(4.12447130123482,5.24313132025201,-1.72405082116765));
#79458=CARTESIAN_POINT('Ctrl Pts',(4.24373727365199,4.28653578497914,3.47683595233796));
#79459=CARTESIAN_POINT('Ctrl Pts',(4.36300324606916,-0.605024841042691,
5.48604795978835));
#79460=CARTESIAN_POINT('Ctrl Pts',(4.48226921848632,-4.9411832149985,2.45916362025659));
#79461=CARTESIAN_POINT('Ctrl Pts',(4.60153519090348,-4.74142157490775,-2.82519003332091));
#79462=CARTESIAN_POINT('Ctrl Pts',(4.72080116332065,-0.189117622405927,
-5.51606850938893));
#79463=CARTESIAN_POINT('Ctrl Pts',(4.84006713573782,4.53679300913506,-3.1432922975186));
#79464=CARTESIAN_POINT('Ctrl Pts',(4.95933310815498,5.09800678279429,2.11497142249248));
#79465=CARTESIAN_POINT('Ctrl Pts',(5.07859908057215,0.979339242271404,5.43172826307833));
#79466=CARTESIAN_POINT('Ctrl Pts',(5.1978650529893,-4.03834464236845,3.76225329089237));
#79467=CARTESIAN_POINT('Ctrl Pts',(5.31713102540649,-5.3488985765674,-1.36090458628507));
#79468=CARTESIAN_POINT('Ctrl Pts',(5.43639699782363,-1.74925690561014,-5.234775788279));
#79469=CARTESIAN_POINT('Ctrl Pts',(5.55566297024081,3.45617209656404,-4.3032141143927));
#79470=CARTESIAN_POINT('Ctrl Pts',(5.67492894265797,5.48889539189286,0.578623065763662));
#79471=CARTESIAN_POINT('Ctrl Pts',(5.79419491507513,2.48290844722863,4.92929436309676));
#79472=CARTESIAN_POINT('Ctrl Pts',(5.9134608874923,-2.8023451485171,4.75495940508004));
#79473=CARTESIAN_POINT('Ctrl Pts',(6.03272685990946,-5.51509477257414,0.215654642662343));
#79474=CARTESIAN_POINT('Ctrl Pts',(6.15199283232664,-3.16508358210627,-4.52161732056773));
#79475=CARTESIAN_POINT('Ctrl Pts',(6.27125880474377,2.09041913570026,-5.10812344334733));
#79476=CARTESIAN_POINT('Ctrl Pts',(6.39052477716097,5.42695354514956,-1.00546133399804));
#79477=CARTESIAN_POINT('Ctrl Pts',(6.50979074957811,3.78163924961165,4.0201967440877));
#79478=CARTESIAN_POINT('Ctrl Pts',(6.62905672199529,-1.33515392291886,5.35538432584356));
#79479=CARTESIAN_POINT('Ctrl Pts',(6.74832269441244,-5.22629908012832,1.77442249772322));
#79480=CARTESIAN_POINT('Ctrl Pts',(6.86758866682961,-4.31979283170086,-3.4354282362702));
#79481=CARTESIAN_POINT('Ctrl Pts',(6.98685463924679,0.552207896342436,-5.49161576538213));
#79482=CARTESIAN_POINT('Ctrl Pts',(7.10612061166394,4.91729140639404,-2.50659579908286));
#79483=CARTESIAN_POINT('Ctrl Pts',(7.22538658408111,4.76838716600991,2.77943539417787));
#79484=CARTESIAN_POINT('Ctrl Pts',(7.34465255649827,0.242186670879671,5.5139933706729));
#79485=CARTESIAN_POINT('Ctrl Pts',(7.46391852891544,-4.50633696423125,3.18680160037922));
#79486=CARTESIAN_POINT('Ctrl Pts',(7.5831845013326,-5.11812185950969,-2.06581845925188));
#79487=CARTESIAN_POINT('Ctrl Pts',(7.70245047374978,-1.03156015100075,-5.42205320245419));
#79488=CARTESIAN_POINT('Ctrl Pts',(7.82171644616692,4.0019557850734,-3.80093766979861));
#79489=CARTESIAN_POINT('Ctrl Pts',(7.94098241858411,5.36174610705912,1.30937235300469));
#79490=CARTESIAN_POINT('Ctrl Pts',(8.06024839100124,1.79954701496616,5.21770139202147));
#79491=CARTESIAN_POINT('Ctrl Pts',(8.17951436341844,-3.41460485164159,4.33627155313435));
#79492=CARTESIAN_POINT('Ctrl Pts',(8.29878033583558,-5.49420901728412,-0.525779944245337));
#79493=CARTESIAN_POINT('Ctrl Pts',(8.41804630825275,-2.53022512749731,-4.90517462273849));
#79494=CARTESIAN_POINT('Ctrl Pts',(8.53731228066992,2.75646130062513,-4.78170454686741));
#79495=CARTESIAN_POINT('Ctrl Pts',(8.65657825308707,5.51276432918079,-0.268713092886506));
#79496=CARTESIAN_POINT('Ctrl Pts',(8.77584422550425,3.2084458496022,4.49095229384002));
#79497=CARTESIAN_POINT('Ctrl Pts',(8.8951101979214,-2.04116996261123,5.12800179983491));
#79498=CARTESIAN_POINT('Ctrl Pts',(9.01437617033858,-5.41702734842686,1.05763508913624));
#79499=CARTESIAN_POINT('Ctrl Pts',(9.13364214275574,-3.82014810472759,-3.98362218757285));
#79500=CARTESIAN_POINT('Ctrl Pts',(9.2529081151729,1.28356047334216,-5.36798377294959));
#79501=CARTESIAN_POINT('Ctrl Pts',(9.37217408759007,5.20898292298034,-1.82462987574903));
#79502=CARTESIAN_POINT('Ctrl Pts',(9.49144006000723,4.35264989723879,3.39370242470428));
#79503=CARTESIAN_POINT('Ctrl Pts',(9.61070603242441,-0.499339821234622,
5.49667508756937));
#79504=CARTESIAN_POINT('Ctrl Pts',(9.72997200484156,-4.89294429261305,2.55379588549317));
#79505=CARTESIAN_POINT('Ctrl Pts',(9.84923797725873,-4.79491123937786,-2.73342339967016));
#79506=CARTESIAN_POINT('Ctrl Pts',(9.96850394967589,-0.295233294641205,
-5.51140767654798));
#79507=CARTESIAN_POINT('Ctrl Pts',(10.0877699220931,4.47546366552298,-3.2300158287476));
#79508=CARTESIAN_POINT('Ctrl Pts',(10.2070358945102,5.13776303561924,2.01647421634918));
#79509=CARTESIAN_POINT('Ctrl Pts',(10.3263018669274,1.08368554481396,5.41187609940749));
#79510=CARTESIAN_POINT('Ctrl Pts',(10.4455678393446,-3.96519637597766,3.83927010970967));
#79511=CARTESIAN_POINT('Ctrl Pts',(10.5648338117617,-5.37409717912364,-1.25771888143246));
#79512=CARTESIAN_POINT('Ctrl Pts',(10.6840997841789,-1.84967049944617,-5.20014387482263));
#79513=CARTESIAN_POINT('Ctrl Pts',(10.803365756596,3.3727214393139,-4.36892748488331));
#79514=CARTESIAN_POINT('Ctrl Pts',(10.9226317290132,5.49901391915264,0.472888139354224));
#79515=CARTESIAN_POINT('Ctrl Pts',(11.0418977014304,2.57730752744729,4.88060069912919));
#79516=CARTESIAN_POINT('Ctrl Pts',(11.1611636738475,-2.71032222460136,4.80800693782864));
#79517=CARTESIAN_POINT('Ctrl Pts',(11.2804296462647,-5.5099234441787,0.321746662246017));
#79518=CARTESIAN_POINT('Ctrl Pts',(11.3996956186819,-3.25151103850694,-4.4598714378157));
#79519=CARTESIAN_POINT('Ctrl Pts',(11.518961591099,1.99173179213046,-5.14740534090655));
#79520=CARTESIAN_POINT('Ctrl Pts',(11.6382275635162,5.40659957463875,-1.10971091501));
#79521=CARTESIAN_POINT('Ctrl Pts',(11.7574935359333,3.85830324210287,3.94667877681414));
#79522=CARTESIAN_POINT('Ctrl Pts',(11.8767595083505,-1.23184817546466,5.38008618406631));
#79523=CARTESIAN_POINT('Ctrl Pts',(11.9960254807677,-5.1911844521573,1.87466830640958));
#79524=CARTESIAN_POINT('Ctrl Pts',(12.1152914531849,-4.38510393926939,-3.35166238114473));
#79525=CARTESIAN_POINT('Ctrl Pts',(12.234557425602,0.446425510915778,-5.50122545789394));
#79526=CARTESIAN_POINT('Ctrl Pts',(12.3538233980192,4.86814412802,-2.6007595091051));
#79527=CARTESIAN_POINT('Ctrl Pts',(12.4730893704363,4.82099133907667,2.68715831017164));
#79528=CARTESIAN_POINT('Ctrl Pts',(12.5923553428535,0.348252581961536,5.50831166643045));
#79529=CARTESIAN_POINT('Ctrl Pts',(12.7116213152707,-4.44417597165164,3.2729309813026));
#79530=CARTESIAN_POINT('Ctrl Pts',(12.8308872876878,-5.15692849249391,-1.96694326270007));
#79531=CARTESIAN_POINT('Ctrl Pts',(12.950153260105,-1.13571059728118,-5.40119789626338));
#79532=CARTESIAN_POINT('Ctrl Pts',(13.0694192325222,3.92806981873332,-3.87724706132231));
#79533=CARTESIAN_POINT('Ctrl Pts',(13.1886852049393,5.38595064914221,1.20594895430169));
#79534=CARTESIAN_POINT('Ctrl Pts',(13.3079511773565,1.89962271798245,5.18210486237994));
#79535=CARTESIAN_POINT('Ctrl Pts',(13.4272171497737,-3.33052573767825,4.40117888593941));
#79536=CARTESIAN_POINT('Ctrl Pts',(13.5464831221908,-5.50330965259982,-0.419952548484216));
#79537=CARTESIAN_POINT('Ctrl Pts',(13.665749094608,-2.62415128759299,-4.85557486763419));
#79538=CARTESIAN_POINT('Ctrl Pts',(13.7850150670251,2.66393219258639,-4.8338641425549));
#79539=CARTESIAN_POINT('Ctrl Pts',(13.9042810394423,5.50657238061311,-0.374750440220661));
#79540=CARTESIAN_POINT('Ctrl Pts',(14.0235470118595,3.29427516129926,4.42837763035443));
#79541=CARTESIAN_POINT('Ctrl Pts',(14.1428129842767,-1.94210920187053,5.16633226993638));
#79542=CARTESIAN_POINT('Ctrl Pts',(14.2620789566938,-5.39567118932092,1.16168398977903));
#79543=CARTESIAN_POINT('Ctrl Pts',(14.381344929111,-3.89610112885092,-3.90936993250106));
#79544=CARTESIAN_POINT('Ctrl Pts',(14.5006109015281,1.1800218174666,-5.39169043859891));
#79545=CARTESIAN_POINT('Ctrl Pts',(14.6198768739453,5.17290531566747,-1.92453315651251));
#79546=CARTESIAN_POINT('Ctrl Pts',(14.7391428463625,4.41715195278582,3.30931199819195));
#79547=CARTESIAN_POINT('Ctrl Pts',(14.8584088187797,-0.393469864863733,
5.5052664550247));
#79548=CARTESIAN_POINT('Ctrl Pts',(14.9776747911968,-4.84289320892863,2.64748232143101));
#79549=CARTESIAN_POINT('Ctrl Pts',(15.096940763614,-4.84662505027999,-2.64064440949086));
#79550=CARTESIAN_POINT('Ctrl Pts',(15.2162067360311,-0.401239623642889,
-5.50470562698815));
#79551=CARTESIAN_POINT('Ctrl Pts',(15.3354727084483,4.41247677962867,-3.31554308441536));
#79552=CARTESIAN_POINT('Ctrl Pts',(15.4547386808655,5.17561645555266,1.91723018450819));
#79553=CARTESIAN_POINT('Ctrl Pts',(15.5740046532826,1.18763049126349,5.39001958174527));
#79554=CARTESIAN_POINT('Ctrl Pts',(15.6932706256998,-3.89057955098784,3.91486500824893));
#79555=CARTESIAN_POINT('Ctrl Pts',(15.812536598117,-5.39730541957021,-1.15406736512861));
#79556=CARTESIAN_POINT('Ctrl Pts',(15.9318025705341,-1.94939904536532,-5.16358602497382));
#79557=CARTESIAN_POINT('Ctrl Pts',(16.0510685429513,3.28802165374775,-4.43302277005912));
#79558=CARTESIAN_POINT('Ctrl Pts',(16.1703345153684,5.50709581987209,0.366978073083481));
#79559=CARTESIAN_POINT('Ctrl Pts',(16.2896004877856,2.67075207054522,4.83009944546223));
#79560=CARTESIAN_POINT('Ctrl Pts',(16.4088664602028,-2.61729549995758,4.85927376685843));
#79561=CARTESIAN_POINT('Ctrl Pts',(16.5281324326199,-5.50271144876792,0.42771951904863));
#79562=CARTESIAN_POINT('Ctrl Pts',(16.6473984050371,-3.3367342583345,-4.39647378755214));
#79563=CARTESIAN_POINT('Ctrl Pts',(16.7666643774543,1.89230678652,-5.18478083442946));
#79564=CARTESIAN_POINT('Ctrl Pts',(16.8859303498714,5.38424320436169,-1.21354950111718));
#79565=CARTESIAN_POINT('Ctrl Pts',(17.0051963222886,3.93353826516432,3.87169910915921));
#79566=CARTESIAN_POINT('Ctrl Pts',(17.1244622947058,-1.12808619808918,5.40279546207863));
#79567=CARTESIAN_POINT('Ctrl Pts',(17.2437282671229,-5.1541472060249,1.97421980893783));
#79568=CARTESIAN_POINT('Ctrl Pts',(17.3629942395401,-4.44879097037678,-3.26665519718109));
#79569=CARTESIAN_POINT('Ctrl Pts',(17.4822602119573,0.340477786383454,-5.50879770479514));
#79570=CARTESIAN_POINT('Ctrl Pts',(17.6015261843744,4.81719387338903,-2.69395999628055));
#79571=CARTESIAN_POINT('Ctrl Pts',(17.7207921567916,4.87180999949389,2.59388600447428));
#79572=CARTESIAN_POINT('Ctrl Pts',(17.8400581292088,0.454189513473253,5.50058989211409));
#79573=CARTESIAN_POINT('Ctrl Pts',(17.9593241016259,-4.38036902456705,3.35784819251709));
#79574=CARTESIAN_POINT('Ctrl Pts',(18.0785900740431,-5.19382519442694,-1.86733958484043));
#79575=CARTESIAN_POINT('Ctrl Pts',(18.1978560464602,-1.23944041935899,-5.37834219088336));
#79576=CARTESIAN_POINT('Ctrl Pts',(18.3171220188774,3.85272904406541,-3.95212046734302));
#79577=CARTESIAN_POINT('Ctrl Pts',(18.4363879912946,5.40816043903902,1.10207891776834));
#79578=CARTESIAN_POINT('Ctrl Pts',(18.5556539637117,1.99899487267145,5.14458907731317));
#79579=CARTESIAN_POINT('Ctrl Pts',(18.6749199361289,-3.24521312308923,4.46445618873186));
#79580=CARTESIAN_POINT('Ctrl Pts',(18.7941859085461,-5.51037207039808,-0.313969618200402));
#79581=CARTESIAN_POINT('Ctrl Pts',(18.9134518809632,-2.71710556141284,-4.80417679145097));
#79582=CARTESIAN_POINT('Ctrl Pts',(19.0327178533804,2.5704164649311,-4.88423345799399));
#79583=CARTESIAN_POINT('Ctrl Pts',(19.1519838257976,5.49834100613709,-0.480648994181217));
#79584=CARTESIAN_POINT('Ctrl Pts',(19.2712497982147,3.37888439821132,4.36416286347117));
#79585=CARTESIAN_POINT('Ctrl Pts',(19.3905157706319,-1.84232915741783,5.2027493261837));
#79586=CARTESIAN_POINT('Ctrl Pts',(19.5097817430491,-5.37231667790874,1.26530264665799));
#79587=CARTESIAN_POINT('Ctrl Pts',(19.6290477154662,-3.97061118463848,-3.83366979483112));
#79588=CARTESIAN_POINT('Ctrl Pts',(19.7483136878834,1.07604612619046,-5.41340022626143));
#79589=CARTESIAN_POINT('Ctrl Pts',(19.8675796603005,5.13491186009314,-2.02372366306542));
#79590=CARTESIAN_POINT('Ctrl Pts',(19.9868456327177,4.48001806250103,3.22369592781969));
#79591=CARTESIAN_POINT('Ctrl Pts',(20.1061116051349,-0.287454182153403,
5.51181888023721));
#79592=CARTESIAN_POINT('Ctrl Pts',(20.2253775775521,-4.79104850097146,2.74018823016145));
#79593=CARTESIAN_POINT('Ctrl Pts',(20.3446435499692,-4.89654385477662,-2.54688742460792));
#79594=CARTESIAN_POINT('Ctrl Pts',(20.4639095223864,-0.507097348680508,
-5.49596484289502));
#79595=CARTESIAN_POINT('Ctrl Pts',(20.5831754948035,4.34785567940971,-3.39984238846463));
#79596=CARTESIAN_POINT('Ctrl Pts',(20.7024414672207,5.21155302312105,1.81727608320107));
#79597=CARTESIAN_POINT('Ctrl Pts',(20.8217074396379,1.29113558434761,5.3661668049184));
#79598=CARTESIAN_POINT('Ctrl Pts',(20.940973412055,-3.81452180264571,3.98900998902192));
#79599=CARTESIAN_POINT('Ctrl Pts',(21.0602393844722,-5.41851470245351,-1.04998842597045));
#79600=CARTESIAN_POINT('Ctrl Pts',(21.1795053568893,-2.04840560769031,-5.1251157783761));
#79601=CARTESIAN_POINT('Ctrl Pts',(21.2987713293066,3.2021041094591,-4.49547623145327));
#79602=CARTESIAN_POINT('Ctrl Pts',(21.4180373017236,5.51313810082114,0.260932092029769));
#79603=CARTESIAN_POINT('Ctrl Pts',(21.5373032741409,2.76320746820189,4.77780930584825));
#79604=CARTESIAN_POINT('Ctrl Pts',(21.656569246558,-2.52329942816223,4.90874090487696));
#79605=CARTESIAN_POINT('Ctrl Pts',(21.7758352189752,-5.49346145739179,0.533533964736603));
#79606=CARTESIAN_POINT('Ctrl Pts',(21.8951011913923,-3.42072167813528,-4.33144784986639));
#79607=CARTESIAN_POINT('Ctrl Pts',(22.0143671638096,1.79218094212641,-5.22023608144834));
#79608=CARTESIAN_POINT('Ctrl Pts',(22.1336331362266,5.35989271427127,-1.31693863443915));
#79609=CARTESIAN_POINT('Ctrl Pts',(22.2528991086439,4.00731645459238,3.79528551075277));
#79610=CARTESIAN_POINT('Ctrl Pts',(22.372165081061,-1.02390642029995,5.42350374922381));
#79611=CARTESIAN_POINT('Ctrl Pts',(22.4914310534782,-5.11520105892454,2.07304013520094));
#79612=CARTESIAN_POINT('Ctrl Pts',(22.6106970258953,-4.51083033775836,-3.18043816782147));
#79613=CARTESIAN_POINT('Ctrl Pts',(22.7299629983125,0.234403961770981,-5.51432970161217));
#79614=CARTESIAN_POINT('Ctrl Pts',(22.8492289707297,4.76445951254608,-2.7861627426778));
#79615=CARTESIAN_POINT('Ctrl Pts',(22.9684949431468,4.92082432595416,2.49965302161611));
#79616=CARTESIAN_POINT('Ctrl Pts',(23.087760915564,0.559958230386614,5.4908309075766));
#79617=CARTESIAN_POINT('Ctrl Pts',(23.2070268879812,-4.31493975465448,3.44152178390302));
#79618=CARTESIAN_POINT('Ctrl Pts',(23.3262928603983,-5.22879830016766,-1.76704431510376));
#79619=CARTESIAN_POINT('Ctrl Pts',(23.4455588328155,-1.34271119963572,-5.35349455120195));
#79620=CARTESIAN_POINT('Ctrl Pts',(23.5648248052326,3.77596136443968,-4.02553015758615));
#79621=CARTESIAN_POINT('Ctrl Pts',(23.6840907776498,5.42836725108453,0.997800712933093));
#79622=CARTESIAN_POINT('Ctrl Pts',(23.803356750067,2.09762667534973,5.10516793124745));
#79623=CARTESIAN_POINT('Ctrl Pts',(23.9226227224841,-3.15869860443647,4.52608002599466));
#79624=CARTESIAN_POINT('Ctrl Pts',(24.0418886949013,-5.51539365502694,-0.207870405458184));
#79625=CARTESIAN_POINT('Ctrl Pts',(24.1611546673185,-2.80905352221347,-4.75099943009008));
#79626=CARTESIAN_POINT('Ctrl Pts',(24.2804206397356,2.47594875234367,-4.93279383829738));
#79627=CARTESIAN_POINT('Ctrl Pts',(24.3996866121528,5.48807325434234,-0.586369533953697));
#79628=CARTESIAN_POINT('Ctrl Pts',(24.51895258457,3.46224222428067,4.29833177590844));
#79629=CARTESIAN_POINT('Ctrl Pts',(24.6382185569871,-1.74186678400333,5.23723948107804));
#79630=CARTESIAN_POINT('Ctrl Pts',(24.7574845294043,-5.34697246381719,1.36845268334623));
#79631=CARTESIAN_POINT('Ctrl Pts',(24.8767505018215,-4.04365067638685,-3.75654981102771));
#79632=CARTESIAN_POINT('Ctrl Pts',(24.9960164742386,0.971671908172561,-5.43310509545365));
#79633=CARTESIAN_POINT('Ctrl Pts',(25.1152824466558,5.09501662759478,-2.12216465900021));
#79634=CARTESIAN_POINT('Ctrl Pts',(25.234548419073,4.54122494315783,3.13688592253812));
#79635=CARTESIAN_POINT('Ctrl Pts',(25.3538143914901,-0.181332037298062,
5.5163299364365));
#79636=CARTESIAN_POINT('Ctrl Pts',(25.4730803639073,-4.73742937005836,2.8318792769264));
#79637=CARTESIAN_POINT('Ctrl Pts',(25.5923463363244,-4.94464916483277,-2.45218716905851));
#79638=CARTESIAN_POINT('Ctrl Pts',(25.7116123087416,-0.612767264061086,
-5.48518856152378));
#79639=CARTESIAN_POINT('Ctrl Pts',(25.8308782811588,4.2816242980748,-3.48288251962541));
#79640=CARTESIAN_POINT('Ctrl Pts',(25.9501442535759,5.24555942878053,1.71664893164223));
#79641=CARTESIAN_POINT('Ctrl Pts',(26.0694102259931,1.39416248969908,5.34032660309201));
#79642=CARTESIAN_POINT('Ctrl Pts',(26.1886761984103,-3.73705129986135,4.06167759153547));
#79643=CARTESIAN_POINT('Ctrl Pts',(26.3079421708274,-5.43771717265829,-0.945520610856157));
#79644=CARTESIAN_POINT('Ctrl Pts',(26.4272081432446,-2.14665351813937,-5.08474738295189));
#79645=CARTESIAN_POINT('Ctrl Pts',(26.5464741156617,3.1150006270531,-4.55626473866868));
#79646=CARTESIAN_POINT('Ctrl Pts',(26.6657400880789,5.51713852416773,0.154789471609084));
#79647=CARTESIAN_POINT('Ctrl Pts',(26.7850060604961,2.8546394784388,4.72374964657473));
#79648=CARTESIAN_POINT('Ctrl Pts',(26.9042720329133,-2.42836882180111,4.95639003112961));
#79649=CARTESIAN_POINT('Ctrl Pts',(27.0235380053304,-5.4821768958969,0.639150809645876));
#79650=CARTESIAN_POINT('Ctrl Pts',(27.1428039777476,-3.50344219214909,-4.26481770790332));
#79651=CARTESIAN_POINT('Ctrl Pts',(27.2620699501647,1.69139134177108,-5.2537579506824));
#79652=CARTESIAN_POINT('Ctrl Pts',(27.3813359225819,5.33355712286708,-1.41984002355569));
#79653=CARTESIAN_POINT('Ctrl Pts',(27.5006018949991,4.07961048573915,3.7174662822981));
#79654=CARTESIAN_POINT('Ctrl Pts',(27.6198678674162,-0.919347426341828,
5.44220337593657));
#79655=CARTESIAN_POINT('Ctrl Pts',(27.7391338398334,-5.07436043503451,2.17109268589186));
#79656=CARTESIAN_POINT('Ctrl Pts',(27.8583998122506,-4.57119906438141,-3.0930432245888));
#79657=CARTESIAN_POINT('Ctrl Pts',(27.9776657846677,0.128243322806431,-5.51781939950306));
#79658=CARTESIAN_POINT('Ctrl Pts',(28.0969317570849,4.7099605763017,-2.8773335998908));
#79659=CARTESIAN_POINT('Ctrl Pts',(28.2161977295021,4.96801616540672,2.40449426192572));
#79660=CARTESIAN_POINT('Ctrl Pts',(28.3354637019192,0.665519559973907,5.47903832717648));
#79661=CARTESIAN_POINT('Ctrl Pts',(28.4547296743364,-4.24791239443814,3.52392076593041));
#79662=CARTESIAN_POINT('Ctrl Pts',(28.5739956467536,-5.26183485700175,-1.66609459906019));
#79663=CARTESIAN_POINT('Ctrl Pts',(28.6932616191707,-1.44548469052482,-5.32666417984418));
#79664=CARTESIAN_POINT('Ctrl Pts',(28.8125275915879,3.69779521169796,-4.09744894388208));
#79665=CARTESIAN_POINT('Ctrl Pts',(28.931793564005,5.44656360144046,0.893152960494481));
#79666=CARTESIAN_POINT('Ctrl Pts',(29.0510595364223,2.1954815965324,5.06385602428271));
#79667=CARTESIAN_POINT('Ctrl Pts',(29.1703255088393,-3.07101422342191,4.58602757459188));
#79668=CARTESIAN_POINT('Ctrl Pts',(29.2895914812566,-5.51837254668137,-0.10169420538848));
#79669=CARTESIAN_POINT('Ctrl Pts',(29.4088574536737,-2.89996111595197,-4.69606247843269));
#79670=CARTESIAN_POINT('Ctrl Pts',(29.5281234260909,2.38056404208793,-4.97952729853896));
#79671=CARTESIAN_POINT('Ctrl Pts',(29.6473893985081,5.47577292801507,-0.691872904653279));
#79672=CARTESIAN_POINT('Ctrl Pts',(29.7666553709252,3.54431776692506,4.23090874900843));
#79673=CARTESIAN_POINT('Ctrl Pts',(29.8859213433424,-1.64075928908623,5.26978996077206));
#79674=CARTESIAN_POINT('Ctrl Pts',(30.0051873157595,-5.31964793358328,1.4710958969759));
#79675=CARTESIAN_POINT('Ctrl Pts',(30.1244532881768,-4.11519255303412,-3.67803854341268));
#79676=CARTESIAN_POINT('Ctrl Pts',(30.2437192605938,0.866937819671528,-5.45079774823832));
#79677=CARTESIAN_POINT('Ctrl Pts',(30.3629852330111,5.0532343938558,-2.21981968549902));
#79678=CARTESIAN_POINT('Ctrl Pts',(30.4822512054281,4.60074992604512,3.0489141334863));
#79679=CARTESIAN_POINT('Ctrl Pts',(30.6015171778454,-0.0751427339222241,
5.51879795289839));
#79680=CARTESIAN_POINT('Ctrl Pts',(30.7207831502625,-4.68205567468513,2.92252150283363));
#79681=CARTESIAN_POINT('Ctrl Pts',(30.8400491226797,-4.99092316406302,-2.35657871623164));
#79682=CARTESIAN_POINT('Ctrl Pts',(30.9593150950968,-0.718210233648821,
-5.47238077400128));
#79683=CARTESIAN_POINT('Ctrl Pts',(31.078581067514,4.21380716521979,-3.56463272297702));
#79684=CARTESIAN_POINT('Ctrl Pts',(31.1978470399312,5.27762307784604,1.61538599831857));
#79685=CARTESIAN_POINT('Ctrl Pts',(31.3171130123484,1.496673050053,5.31250854649871));
#79686=CARTESIAN_POINT('Ctrl Pts',(31.4363789847655,-3.65819673477567,4.13284090246077));
#79687=CARTESIAN_POINT('Ctrl Pts',(31.5556449571827,-5.45490571831667,-0.840702610708948));
#79688=CARTESIAN_POINT('Ctrl Pts',(31.6749109295998,-2.24410638940634,-5.04249578962663));
#79689=CARTESIAN_POINT('Ctrl Pts',(31.794176902017,3.02674346636162,-4.61536577794365));
#79690=CARTESIAN_POINT('Ctrl Pts',(31.9134428744342,5.51909560830654,0.0485895230291355));
#79691=CARTESIAN_POINT('Ctrl Pts',(32.0327088468513,2.94501423830122,4.66794048929288));
#79692=CARTESIAN_POINT('Ctrl Pts',(32.1519748192685,-2.3325388395765,5.0022034981839));
#79693=CARTESIAN_POINT('Ctrl Pts',(32.2712407916856,-5.46886194365754,0.744530937296086));
#79694=CARTESIAN_POINT('Ctrl Pts',(32.3905067641028,-3.58486516382964,-4.19660803894495));
#79695=CARTESIAN_POINT('Ctrl Pts',(32.50977273652,1.5899753141059,-5.28533402690029));
#79696=CARTESIAN_POINT('Ctrl Pts',(32.6290387089371,5.305246183855,-1.52221555768843));
#79697=CARTESIAN_POINT('Ctrl Pts',(32.7483046813544,4.15039358363284,3.63827024509121));
#79698=CARTESIAN_POINT('Ctrl Pts',(32.8675706537714,-0.814447940907383,
5.45888741658297));
#79699=CARTESIAN_POINT('Ctrl Pts',(32.9868366261887,-5.03164046017552,2.26834114605837));
#79700=CARTESIAN_POINT('Ctrl Pts',(33.1061025986057,-4.62987479195544,-3.00450273526126));
#79701=CARTESIAN_POINT('Ctrl Pts',(33.2253685710231,0.0220351873710713,
-5.5192655060156));
#79702=CARTESIAN_POINT('Ctrl Pts',(33.34463454344,4.65371724899836,-2.96743880168604));
#79703=CARTESIAN_POINT('Ctrl Pts',(33.4639005158574,5.01336803978119,2.30844496860492));
#79704=CARTESIAN_POINT('Ctrl Pts',(33.5831664882744,0.770834406315328,5.46521651843883));
#79705=CARTESIAN_POINT('Ctrl Pts',(33.7024324606917,-4.17931176831432,3.6050146211362));
#79706=CARTESIAN_POINT('Ctrl Pts',(33.8216984331088,-5.29292262943967,-1.56452782466247));
#79707=CARTESIAN_POINT('Ctrl Pts',(33.9409644055259,-1.54772282861625,-5.29786101376356));
#79708=CARTESIAN_POINT('Ctrl Pts',(34.0602303779431,3.6182595356233,-4.16785019023544));
#79709=CARTESIAN_POINT('Ctrl Pts',(34.1794963503603,5.4627427508684,0.788174418017909));
#79710=CARTESIAN_POINT('Ctrl Pts',(34.2987623227774,2.29252339446042,5.0206686567849));
#79711=CARTESIAN_POINT('Ctrl Pts',(34.4180282951946,-2.98219245501818,4.64427663222141));
#79712=CARTESIAN_POINT('Ctrl Pts',(34.5372942676118,-5.51930764209687,0.00451965836400682));
#79713=CARTESIAN_POINT('Ctrl Pts',(34.656560240029,-2.98979467388986,-4.63938628304514));
#79714=CARTESIAN_POINT('Ctrl Pts',(34.7758262124461,2.28429766103466,-5.02441653041523));
#79715=CARTESIAN_POINT('Ctrl Pts',(34.8950921848632,5.46144458275793,-0.797120031824677));
#79716=CARTESIAN_POINT('Ctrl Pts',(35.0143581572805,3.62508062841914,4.16191875370487));
#79717=CARTESIAN_POINT('Ctrl Pts',(35.1336241296976,-1.53904411895615,5.30038870980534));
#79718=CARTESIAN_POINT('Ctrl Pts',(35.2528901021148,-5.29035320736527,1.57319427237781));
#79719=CARTESIAN_POINT('Ctrl Pts',(35.3721560745319,-4.18521031782329,-3.59816506956947));
#79720=CARTESIAN_POINT('Ctrl Pts',(35.4914220469491,0.76188264955475,-5.46647163195967));
#79721=CARTESIAN_POINT('Ctrl Pts',(35.6106880193662,5.0095806347121,-2.31665257477511));
#79722=CARTESIAN_POINT('Ctrl Pts',(35.7299539917834,4.65857096293502,2.95981314196468));
#79723=CARTESIAN_POINT('Ctrl Pts',(35.8492199642006,0.0310744040885409,
5.51922201578924));
#79724=CARTESIAN_POINT('Ctrl Pts',(35.9684859366178,-4.6249479319303,3.01208133700502));
#79725=CARTESIAN_POINT('Ctrl Pts',(36.0877519090349,-5.03534869769585,-2.2600974750615));
#79726=CARTESIAN_POINT('Ctrl Pts',(36.2070178814521,-0.82338723695312,-5.45754622539771));
#79727=CARTESIAN_POINT('Ctrl Pts',(36.3262838538693,4.14442945774543,-3.64506271839436));
#79728=CARTESIAN_POINT('Ctrl Pts',(36.4455498262864,5.30773198119607,1.51352478159224));
#79729=CARTESIAN_POINT('Ctrl Pts',(36.5648157987036,1.59862951581808,5.28272294851769));
#79730=CARTESIAN_POINT('Ctrl Pts',(36.6840817711207,-3.57798772320569,4.20247354542357));
#79731=CARTESIAN_POINT('Ctrl Pts',(36.803347743538,-5.47007319271275,-0.735573207822807));
#79732=CARTESIAN_POINT('Ctrl Pts',(36.922613715955,-2.34072961144035,-4.99837671957824));
#79733=CARTESIAN_POINT('Ctrl Pts',(37.0418796883723,2.93736813071235,-4.67275732224894));
#79734=CARTESIAN_POINT('Ctrl Pts',(37.1611456607894,5.51900327969889,-0.057628683827517));
#79735=CARTESIAN_POINT('Ctrl Pts',(37.2804116332065,3.03430843495129,4.61040300226366));
#79736=CARTESIAN_POINT('Ctrl Pts',(37.3996776056238,-2.2358642669444,5.0461633913799));
#79737=CARTESIAN_POINT('Ctrl Pts',(37.5189435780408,-5.45348488848064,0.849637117637928));
#79738=CARTESIAN_POINT('Ctrl Pts',(37.6382095504581,-3.66503003262188,-4.12684752159054));
#79739=CARTESIAN_POINT('Ctrl Pts',(37.7574755228752,1.48810259966544,-5.31494612688231));
#79740=CARTESIAN_POINT('Ctrl Pts',(37.8767414952924,5.27471933483358,-1.62403964590353));
#79741=CARTESIAN_POINT('Ctrl Pts',(37.9960074677095,4.22011637573384,3.55775015176621));
#79742=CARTESIAN_POINT('Ctrl Pts',(38.1152734401267,-0.710152797904622,
5.47350509862131));
#79743=CARTESIAN_POINT('Ctrl Pts',(38.2345394125439,-4.9853333920201,2.36483512966171));
#79744=CARTESIAN_POINT('Ctrl Pts',(38.353805384961,-4.69013369949273,-2.91502009518441));
#79745=CARTESIAN_POINT('Ctrl Pts',(38.4730713573783,-0.077709984764535,
-5.51827546323263));
#79746=CARTESIAN_POINT('Ctrl Pts',(38.5724596677258,3.80513849405293,-3.46787737060704));
#79747=CARTESIAN_POINT('Ctrl Pts',(38.651970316004,4.8393236171102,-0.417509269414375));
#79748=CARTESIAN_POINT('Ctrl Pts',(38.691725640143,4.58753946265277,1.15800627176077));
#79749=CARTESIAN_POINT('Ctrl Pts',(38.7116033022125,4.27611881062226,1.87009427887657));
#79750=CARTESIAN_POINT('Ctrl Pts',(-17.6184,2.62535040627071,-3.68399909158434));
#79751=CARTESIAN_POINT('Ctrl Pts',(-17.5985223379305,3.23883466326236,-3.24680811968291));
#79752=CARTESIAN_POINT('Ctrl Pts',(-17.5587670137914,4.23254591953354,-2.06184536971571));
#79753=CARTESIAN_POINT('Ctrl Pts',(-17.4792563655133,4.8909587174436,0.989874372427294));
#79754=CARTESIAN_POINT('Ctrl Pts',(-17.3798680551657,2.68243561037911,4.62805141939821));
#79755=CARTESIAN_POINT('Ctrl Pts',(-17.2606020827485,-2.44949610129593,
4.7591308229798));
#79756=CARTESIAN_POINT('Ctrl Pts',(-17.1413361103314,-5.32337982130319,
0.515004556339686));
#79757=CARTESIAN_POINT('Ctrl Pts',(-17.0220701379142,-3.31538769240887,
-4.19860974939619));
#79758=CARTESIAN_POINT('Ctrl Pts',(-16.902804165497,1.73863948785637,-5.05968774485838));
#79759=CARTESIAN_POINT('Ctrl Pts',(-16.7835381930798,5.19527552722027,-1.27515938975536));
#79760=CARTESIAN_POINT('Ctrl Pts',(-16.6642722206627,3.88345012932081,3.67946867571279));
#79761=CARTESIAN_POINT('Ctrl Pts',(-16.5450062482455,-0.993689040191803,
5.25665841728971));
#79762=CARTESIAN_POINT('Ctrl Pts',(-16.4257402758284,-4.95844193487295,
2.00819591524889));
#79763=CARTESIAN_POINT('Ctrl Pts',(-16.3064743034112,-4.37153537144703,
-3.08368617743557));
#79764=CARTESIAN_POINT('Ctrl Pts',(-16.187208330994,0.228419052524531,-5.34483459461538));
#79765=CARTESIAN_POINT('Ctrl Pts',(-16.0679423585769,4.61866000512981,-2.69949887735067));
#79766=CARTESIAN_POINT('Ctrl Pts',(-15.9486763861597,4.76906677072755,2.42391962238011));
#79767=CARTESIAN_POINT('Ctrl Pts',(-15.8294104137425,0.541545441910157,
5.32222750447519));
#79768=CARTESIAN_POINT('Ctrl Pts',(-15.7101444413254,-4.18310095899125,
3.33482055878733));
#79769=CARTESIAN_POINT('Ctrl Pts',(-15.5908784689082,-5.06773584614322,
-1.71389202338234));
#79770=CARTESIAN_POINT('Ctrl Pts',(-15.4716124964911,-1.30027644702517,
-5.18928239612476));
#79771=CARTESIAN_POINT('Ctrl Pts',(-15.3523465240739,3.66081343996144,-3.90100162460633));
#79772=CARTESIAN_POINT('Ctrl Pts',(-15.2330805516567,5.26134075862523,0.968330387076498));
#79773=CARTESIAN_POINT('Ctrl Pts',(-15.1138145792395,2.03204885203783,4.94875210508029));
#79774=CARTESIAN_POINT('Ctrl Pts',(-14.9945486068224,-3.06262837106116,
4.38630564025653));
#79775=CARTESIAN_POINT('Ctrl Pts',(-14.8752826344052,-5.34586621077957,
-0.202692870982978));
#79776=CARTESIAN_POINT('Ctrl Pts',(-14.7560166619881,-2.72169207944861,
-4.60562287829862));
#79777=CARTESIAN_POINT('Ctrl Pts',(-14.6367506895709,2.40094789974828,-4.78067139956327));
#79778=CARTESIAN_POINT('Ctrl Pts',(-14.5174847171537,5.31955958788271,-0.56714695851215));
#79779=CARTESIAN_POINT('Ctrl Pts',(-14.3982187447365,3.35490834716323,4.16700850147134));
#79780=CARTESIAN_POINT('Ctrl Pts',(-14.2789527723194,-1.68949024264872,
5.07592283106375));
#79781=CARTESIAN_POINT('Ctrl Pts',(-14.1596867999022,-5.18296625647794,
1.32522852967441));
#79782=CARTESIAN_POINT('Ctrl Pts',(-14.0404208274851,-3.91856964050138,
-3.6420024494952));
#79783=CARTESIAN_POINT('Ctrl Pts',(-13.9211548550679,0.943005562874773,
-5.26593869864046));
#79784=CARTESIAN_POINT('Ctrl Pts',(-13.8018888826508,4.93891810628447,-2.05583506379208));
#79785=CARTESIAN_POINT('Ctrl Pts',(-13.6826229102336,4.40098996586505,3.04148930462108));
#79786=CARTESIAN_POINT('Ctrl Pts',(-13.5633569378164,-0.176970207163579,
5.34677953683851));
#79787=CARTESIAN_POINT('Ctrl Pts',(-13.4440909653992,-4.59247481650836,
2.74381940542772));
#79788=CARTESIAN_POINT('Ctrl Pts',(-13.3248249929821,-4.79216763991698,
-2.37791908624871));
#79789=CARTESIAN_POINT('Ctrl Pts',(-13.2055590205649,-0.592734148285034,
-5.31676932913924));
#79790=CARTESIAN_POINT('Ctrl Pts',(-13.0862930481478,4.15081895382183,-3.37491805566053));
#79791=CARTESIAN_POINT('Ctrl Pts',(-12.9670270757306,5.08399264919423,1.66504913223642));
#79792=CARTESIAN_POINT('Ctrl Pts',(-12.8477611033134,1.35014976061496,5.17653025623679));
#79793=CARTESIAN_POINT('Ctrl Pts',(-12.7284951308963,-3.62310706075401,
3.93604688693356));
#79794=CARTESIAN_POINT('Ctrl Pts',(-12.6092291584791,-5.27041478960109,
-0.917658877458269));
#79795=CARTESIAN_POINT('Ctrl Pts',(-12.4899631860619,-2.07957366092086,
-4.92896979688741));
#79796=CARTESIAN_POINT('Ctrl Pts',(-12.3706972136447,3.02027981942101,-4.41557240708635));
#79797=CARTESIAN_POINT('Ctrl Pts',(-12.2514312412276,5.34756910110119,0.151243442078761));
#79798=CARTESIAN_POINT('Ctrl Pts',(-12.1321652688104,2.76588321291629,4.57922044919569));
#79799=CARTESIAN_POINT('Ctrl Pts',(-12.0128992963933,-2.35483522599469,
4.80355294841628));
#79800=CARTESIAN_POINT('Ctrl Pts',(-11.8936333239761,-5.31385599723994,
0.618307617954934));
#79801=CARTESIAN_POINT('Ctrl Pts',(-11.7743673515589,-3.39484963998713,
-4.13453332211792));
#79802=CARTESIAN_POINT('Ctrl Pts',(-11.6551013791418,1.64056947847539,-5.09194478133052));
#79803=CARTESIAN_POINT('Ctrl Pts',(-11.5358354067246,5.16997442825406,-1.37503973797965));
#79804=CARTESIAN_POINT('Ctrl Pts',(-11.4165694343074,3.95343302047925,3.60412780328452));
#79805=CARTESIAN_POINT('Ctrl Pts',(-11.2973034618903,-0.892290949753927,
5.2747688793739));
#79806=CARTESIAN_POINT('Ctrl Pts',(-11.1780374894731,-4.91890739022456,
2.10326411946247));
#79807=CARTESIAN_POINT('Ctrl Pts',(-11.058771517056,-4.43005263528682,-2.99900041987535));
#79808=CARTESIAN_POINT('Ctrl Pts',(-10.9395055446388,0.125513175958816,
-5.3482348782084));
#79809=CARTESIAN_POINT('Ctrl Pts',(-10.8202395722216,4.56586008070243,-2.78788299490349));
#79810=CARTESIAN_POINT('Ctrl Pts',(-10.7009735998044,4.81482706281336,2.3316968553018));
#79811=CARTESIAN_POINT('Ctrl Pts',(-10.5817076273873,0.643866774853417,
5.31081965858981));
#79812=CARTESIAN_POINT('Ctrl Pts',(-10.4624416549701,-4.11815198298316,
3.41470263930491));
#79813=CARTESIAN_POINT('Ctrl Pts',(-10.343175682553,-5.09977904358443,-1.61605184831468));
#79814=CARTESIAN_POINT('Ctrl Pts',(-10.2239097101358,-1.39989788550755,
-5.1632989241352));
#79815=CARTESIAN_POINT('Ctrl Pts',(-10.1046437377186,3.5850651163716,-3.97072763875836));
#79816=CARTESIAN_POINT('Ctrl Pts',(-9.98537776530147,5.27900086719687,0.866902367028086));
#79817=CARTESIAN_POINT('Ctrl Pts',(-9.86611179288431,2.12690589100833,4.90873111920161));
#79818=CARTESIAN_POINT('Ctrl Pts',(-9.74684582046714,-2.97765159855841,
4.44443031528525));
#79819=CARTESIAN_POINT('Ctrl Pts',(-9.62757984804998,-5.34877685275258,
-0.0997800044217893));
#79820=CARTESIAN_POINT('Ctrl Pts',(-9.50831387563282,-2.80981824212958,
-4.55239402029525));
#79821=CARTESIAN_POINT('Ctrl Pts',(-9.38904790321564,2.30850450978291,-4.82598972213328));
#79822=CARTESIAN_POINT('Ctrl Pts',(-9.26978193079849,5.30766038347549,-0.669411027328533));
#79823=CARTESIAN_POINT('Ctrl Pts',(-9.15051595838132,3.43447659405036,4.10167531561732));
#79824=CARTESIAN_POINT('Ctrl Pts',(-9.03124998596416,-1.59149680929566,
5.10749525460629));
#79825=CARTESIAN_POINT('Ctrl Pts',(-8.91198401354699,-5.15650389840683,
1.42472362777463));
#79826=CARTESIAN_POINT('Ctrl Pts',(-8.79271804112983,-3.98793034142981,
-3.56591944128407));
#79827=CARTESIAN_POINT('Ctrl Pts',(-8.67345206871266,0.841493716983345,
-5.28311065510666));
#79828=CARTESIAN_POINT('Ctrl Pts',(-8.55418609629549,4.8984412193819,-2.15049842829157));
#79829=CARTESIAN_POINT('Ctrl Pts',(-8.43492012387834,4.45870511426281,2.9562338496592));
#79830=CARTESIAN_POINT('Ctrl Pts',(-8.31565415146116,-0.0740445231469701,
5.3491950121879));
#79831=CARTESIAN_POINT('Ctrl Pts',(-8.19638817904401,-4.53882257969058,
2.83168844683082));
#79832=CARTESIAN_POINT('Ctrl Pts',(-8.07712220662684,-4.83704066797944,
-2.2852587263015));
#79833=CARTESIAN_POINT('Ctrl Pts',(-7.95785623420967,-0.694939784074152,
-5.30437824502882));
#79834=CARTESIAN_POINT('Ctrl Pts',(-7.83859026179251,4.08510370142725,-3.45417104648997));
#79835=CARTESIAN_POINT('Ctrl Pts',(-7.71932428937535,5.11509323577896,1.56690492982581));
#79836=CARTESIAN_POINT('Ctrl Pts',(-7.60005831695818,1.44951639010705,5.1495895083623));
#79837=CARTESIAN_POINT('Ctrl Pts',(-7.48079234454102,-3.54669122121178,
4.00504073028022));
#79838=CARTESIAN_POINT('Ctrl Pts',(-7.36152637212386,-5.28709814796872,
-0.816065587786831));
#79839=CARTESIAN_POINT('Ctrl Pts',(-7.24226039970668,-2.17404118518495,
-4.88803792895919));
#79840=CARTESIAN_POINT('Ctrl Pts',(-7.12299442728953,2.93474766896221,-4.4728767017821));
#79841=CARTESIAN_POINT('Ctrl Pts',(-7.00372845487236,5.34948934683475,0.0483073278670784));
#79842=CARTESIAN_POINT('Ctrl Pts',(-6.8844624824552,2.85349310274905,4.52514607304423));
#79843=CARTESIAN_POINT('Ctrl Pts',(-6.76519651003803,-2.26196004295795,
4.84797964454119));
#79844=CARTESIAN_POINT('Ctrl Pts',(-6.64593053762087,-5.30097331922578,
0.720452454142903));
#79845=CARTESIAN_POINT('Ctrl Pts',(-6.5266645652037,-3.47378554073058,-4.06843752401771));
#79846=CARTESIAN_POINT('Ctrl Pts',(-6.40739859278654,1.54227677916538,-5.12257281122204));
#79847=CARTESIAN_POINT('Ctrl Pts',(-6.28813262036938,5.14255591405802,-1.47427559859448));
#79848=CARTESIAN_POINT('Ctrl Pts',(-6.16886664795221,4.0220584092331,3.52738090125541));
#79849=CARTESIAN_POINT('Ctrl Pts',(-6.04960067553505,-0.790618568056538,
5.2909632534793));
#79850=CARTESIAN_POINT('Ctrl Pts',(-5.93033470311788,-4.87752148875202,
2.19753361671364));
#79851=CARTESIAN_POINT('Ctrl Pts',(-5.81106873070072,-4.48694474979491,
-2.91319355383608));
#79852=CARTESIAN_POINT('Ctrl Pts',(-5.69180275828355,0.0225690143544715,
-5.34965984987971));
#79853=CARTESIAN_POINT('Ctrl Pts',(-5.57253678586638,4.51136481694416,-2.87523170514354));
#79854=CARTESIAN_POINT('Ctrl Pts',(-5.45327081344922,4.85880639859978,2.23860899907733));
#79855=CARTESIAN_POINT('Ctrl Pts',(-5.33400484103205,0.745948446959714,
5.29744568488459));
#79856=CARTESIAN_POINT('Ctrl Pts',(-5.21473886861489,-4.05167716918246,
3.49331962272991));
#79857=CARTESIAN_POINT('Ctrl Pts',(-5.09547289619773,-5.12993380779606,
-1.51761292741435));
#79858=CARTESIAN_POINT('Ctrl Pts',(-4.97620692378056,-1.49900068010318,
-5.13540327830972));
#79859=CARTESIAN_POINT('Ctrl Pts',(-4.8569409513634,3.50798892841612,-4.03898298435808));
#79860=CARTESIAN_POINT('Ctrl Pts',(-4.73767497894623,5.29470588216781,0.765153246847895));
#79861=CARTESIAN_POINT('Ctrl Pts',(-4.61840900652908,2.22097517906763,4.86689214219808));
#79862=CARTESIAN_POINT('Ctrl Pts',(-4.4991430341119,-2.89157200322203,4.50090893264979));
#79863=CARTESIAN_POINT('Ctrl Pts',(-4.37987706169475,-5.34970651737601,
0.00316982159248442));
#79864=CARTESIAN_POINT('Ctrl Pts',(-4.26061108927757,-2.89690375080243,
-4.49747913040303));
#79865=CARTESIAN_POINT('Ctrl Pts',(-4.14134511686041,2.21520613519663,-4.86952067953422));
#79866=CARTESIAN_POINT('Ctrl Pts',(-4.02207914444325,5.29379542366406,-0.771427172335632));
#79867=CARTESIAN_POINT('Ctrl Pts',(-3.90281317202608,3.51277284030709,4.03482302489525));
#79868=CARTESIAN_POINT('Ctrl Pts',(-3.78354719960892,-1.49291394549895,
5.13717605510642));
#79869=CARTESIAN_POINT('Ctrl Pts',(-3.66428122719175,-5.12813176668884,
1.52369106228954));
#79870=CARTESIAN_POINT('Ctrl Pts',(-3.54501525477459,-4.05581406387994,
-3.48851575158515));
#79871=CARTESIAN_POINT('Ctrl Pts',(-3.42574928235742,0.73967021363975,-5.29832594739868));
#79872=CARTESIAN_POINT('Ctrl Pts',(-3.30648330994026,4.85615013534878,-2.24436532961465));
#79873=CARTESIAN_POINT('Ctrl Pts',(-3.18721733752309,4.51476892709962,2.86988351762224));
#79874=CARTESIAN_POINT('Ctrl Pts',(-3.06795136510593,0.0289085841635225,
5.34962934824326));
#79875=CARTESIAN_POINT('Ctrl Pts',(-2.94868539268877,-4.48348933485096,
2.91850873805477));
#79876=CARTESIAN_POINT('Ctrl Pts',(-2.8294194202716,-4.88012223932707,-2.19175199305243));
#79877=CARTESIAN_POINT('Ctrl Pts',(-2.71015344785444,-0.796888040481462,
-5.29002262006144));
#79878=CARTESIAN_POINT('Ctrl Pts',(-2.59088747543727,4.01787548130092,-3.53214474315326));
#79879=CARTESIAN_POINT('Ctrl Pts',(-2.4716215030201,5.1442993855074,1.46818040515877));
#79880=CARTESIAN_POINT('Ctrl Pts',(-2.35235553060294,1.54834617361307,5.12074154751847));
#79881=CARTESIAN_POINT('Ctrl Pts',(-2.23308955818578,-3.46896182153357,
4.07255125818778));
#79882=CARTESIAN_POINT('Ctrl Pts',(-2.11382358576862,-5.3018233653736,-0.714170058321242));
#79883=CARTESIAN_POINT('Ctrl Pts',(-1.99455761335145,-2.26770352691226,
-4.84529571686329));
#79884=CARTESIAN_POINT('Ctrl Pts',(-1.87529164093429,2.84812859908841,-4.52852441230905));
#79885=CARTESIAN_POINT('Ctrl Pts',(-1.75602566851712,5.3494283442679,-0.0546466775498073));
#79886=CARTESIAN_POINT('Ctrl Pts',(-1.63675969609995,2.94004616678162,4.46939575412793));
#79887=CARTESIAN_POINT('Ctrl Pts',(-1.51749372368279,-2.1682471155684,4.89061083257026));
#79888=CARTESIAN_POINT('Ctrl Pts',(-1.39822775126562,-5.28612736141081,
0.822330462021165));
#79889=CARTESIAN_POINT('Ctrl Pts',(-1.27896177884846,-3.55143488284157,
-4.00083493070636));
#79890=CARTESIAN_POINT('Ctrl Pts',(-1.1596958064313,1.4434128789333,-5.15130363410601));
#79891=CARTESIAN_POINT('Ctrl Pts',(-1.04042983401413,5.1132327918697,-1.57296544334973));
#79892=CARTESIAN_POINT('Ctrl Pts',(-0.921163861596969,4.08919417984387,
3.4493275909016));
#79893=CARTESIAN_POINT('Ctrl Pts',(-0.801897889179802,-0.688653371177603,
5.30519805513329));
#79894=CARTESIAN_POINT('Ctrl Pts',(-0.682631916762638,-4.83432913800304,
2.29098923072084));
#79895=CARTESIAN_POINT('Ctrl Pts',(-0.563365944345475,-4.54217506986187,
-2.82630775120993));
#79896=CARTESIAN_POINT('Ctrl Pts',(-0.444099971928309,-0.0803835059582494,
-5.3491035101028));
#79897=CARTESIAN_POINT('Ctrl Pts',(-0.324833999511145,4.45519871447649,
-2.9615155384281));
#79898=CARTESIAN_POINT('Ctrl Pts',(-0.205568027093979,4.90098621647057,
2.14469204684251));
#79899=CARTESIAN_POINT('Ctrl Pts',(-0.0863020546768169,0.847753848005954,
5.28210973788082));
#79900=CARTESIAN_POINT('Ctrl Pts',(0.0329639177403491,-3.98370176757143,
3.57064281283809));
#79901=CARTESIAN_POINT('Ctrl Pts',(0.152229890157513,-5.1581886387657,-1.41861194014872));
#79902=CARTESIAN_POINT('Ctrl Pts',(0.271495862574679,-1.59754830160526,
-5.10560567355749));
#79903=CARTESIAN_POINT('Ctrl Pts',(0.390761834991842,3.42961351418844,-4.10574244359289));
#79904=CARTESIAN_POINT('Ctrl Pts',(0.510027807409007,5.30844993855932,0.663120742876867));
#79905=CARTESIAN_POINT('Ctrl Pts',(0.629293779826171,2.3142219020159,4.82325065262569));
#79906=CARTESIAN_POINT('Ctrl Pts',(0.748559752243337,-2.80442147910245,
4.55572058376859));
#79907=CARTESIAN_POINT('Ctrl Pts',(0.867825724660504,-5.34865485326728,
0.106118473624908));
#79908=CARTESIAN_POINT('Ctrl Pts',(0.987091697077666,-2.98291635601472,
-4.44089854453399));
#79909=CARTESIAN_POINT('Ctrl Pts',(1.10635766949483,2.12108733213468,-4.91124815085553));
#79910=CARTESIAN_POINT('Ctrl Pts',(1.22562364191199,5.27796984247255,-0.873157609927544));
#79911=CARTESIAN_POINT('Ctrl Pts',(1.34488961432916,3.58976808851186,3.96647638849978));
#79912=CARTESIAN_POINT('Ctrl Pts',(1.46415558674632,-1.39377816290472,5.16495424011036));
#79913=CARTESIAN_POINT('Ctrl Pts',(1.58342155916349,-5.09786036913662,1.62209417932818));
#79914=CARTESIAN_POINT('Ctrl Pts',(1.70268753158065,-4.12219566637061,-3.40982004774148));
#79915=CARTESIAN_POINT('Ctrl Pts',(1.82195350399781,0.637572764456073,-5.31157894037619));
#79916=CARTESIAN_POINT('Ctrl Pts',(1.94121947641498,4.81206051717935,-2.33740100300047));
#79917=CARTESIAN_POINT('Ctrl Pts',(2.06048544883214,4.56916064047356,2.78247028939603));
#79918=CARTESIAN_POINT('Ctrl Pts',(2.17975142124932,0.13185098482894,5.34808238414702));
#79919=CARTESIAN_POINT('Ctrl Pts',(2.29901739366647,-4.42649557532506,3.00424812414882));
#79920=CARTESIAN_POINT('Ctrl Pts',(2.41828336608365,-4.92139639817879,-2.09743351785397));
#79921=CARTESIAN_POINT('Ctrl Pts',(2.5375493385008,-0.898541159731936,-5.27370777101761));
#79922=CARTESIAN_POINT('Ctrl Pts',(2.65681531091797,3.94915919222963,-3.60881026714515));
#79923=CARTESIAN_POINT('Ctrl Pts',(2.77608128333514,5.17160028152781,1.36891212206108));
#79924=CARTESIAN_POINT('Ctrl Pts',(2.8953472557523,1.64660250832305,5.0899970578978));
#79925=CARTESIAN_POINT('Ctrl Pts',(3.01461322816947,-3.38994764974585,4.13855346731278));
#79926=CARTESIAN_POINT('Ctrl Pts',(3.13387920058662,-5.31458498815282,-0.61201002730754));
#79927=CARTESIAN_POINT('Ctrl Pts',(3.25314517300379,-2.3605259971177,-4.80075899069673));
#79928=CARTESIAN_POINT('Ctrl Pts',(3.37241114542096,2.76045469022341,-4.58249492886218));
#79929=CARTESIAN_POINT('Ctrl Pts',(3.49167711783813,5.34738611599374,-0.157580443906409));
#79930=CARTESIAN_POINT('Ctrl Pts',(3.61094309025528,3.02551034903617,4.41199014025406));
#79931=CARTESIAN_POINT('Ctrl Pts',(3.73020906267246,-2.07373115154603,4.93143072352554));
#79932=CARTESIAN_POINT('Ctrl Pts',(3.84947503508961,-5.26932362217573,0.923903909833121));
#79933=CARTESIAN_POINT('Ctrl Pts',(3.96874100750679,-3.62776890794389,-3.93175057962476));
#79934=CARTESIAN_POINT('Ctrl Pts',(4.08800697992394,1.34401439322441,-5.17812660917343));
#79935=CARTESIAN_POINT('Ctrl Pts',(4.2072729523411,5.08201592186332,-1.67107272126372));
#79936=CARTESIAN_POINT('Ctrl Pts',(4.32653892475827,4.15481546776415,3.36999678021387));
#79937=CARTESIAN_POINT('Ctrl Pts',(4.44580489717544,-0.586433123165232,
5.31746801230425));
#79938=CARTESIAN_POINT('Ctrl Pts',(4.56507086959259,-4.78934633478894,2.38359634906328));
#79939=CARTESIAN_POINT('Ctrl Pts',(4.68433684200976,-4.5957231402684,-2.73837519120838));
#79940=CARTESIAN_POINT('Ctrl Pts',(4.80360281442692,-0.183306255264012,
-5.34656606492479));
#79941=CARTESIAN_POINT('Ctrl Pts',(4.9228687868441,4.39738257509714,-3.04670253849241));
#79942=CARTESIAN_POINT('Ctrl Pts',(5.04213475926125,4.94135089461829,2.04998078188042));
#79943=CARTESIAN_POINT('Ctrl Pts',(5.16140073167843,0.949245273126337,5.26481749743252));
#79944=CARTESIAN_POINT('Ctrl Pts',(5.28066670409559,-3.91425095366504,3.64664357204764));
#79945=CARTESIAN_POINT('Ctrl Pts',(5.39993267651275,-5.18453307197378,-1.31908555273497));
#79946=CARTESIAN_POINT('Ctrl Pts',(5.51919864892993,-1.69550425170618,-5.07391714578299));
#79947=CARTESIAN_POINT('Ctrl Pts',(5.63846462134707,3.34996790097437,-4.17098129128691));
#79948=CARTESIAN_POINT('Ctrl Pts',(5.75773059376426,5.32022794609337,0.560842644091171));
#79949=CARTESIAN_POINT('Ctrl Pts',(5.8769965661814,2.40661152479762,4.77782281363966));
#79950=CARTESIAN_POINT('Ctrl Pts',(5.99626253859857,-2.71623230345395,4.6088449684815));
#79951=CARTESIAN_POINT('Ctrl Pts',(6.11552851101574,-5.34562224992299,0.209027823392774));
#79952=CARTESIAN_POINT('Ctrl Pts',(6.23479448343291,-3.06782420195421,-4.38267321799473));
#79953=CARTESIAN_POINT('Ctrl Pts',(6.35406045585007,2.02618295863798,-4.95115668182184));
#79954=CARTESIAN_POINT('Ctrl Pts',(6.47332642826723,5.26018950109706,-0.974564663002068));
#79955=CARTESIAN_POINT('Ctrl Pts',(6.59259240068441,3.66543382254001,3.89666071943709));
#79956=CARTESIAN_POINT('Ctrl Pts',(6.71185837310155,-1.29412617765311,5.19081952163018));
#79957=CARTESIAN_POINT('Ctrl Pts',(6.83112434551873,-5.06570091712964,1.71989653410197));
#79958=CARTESIAN_POINT('Ctrl Pts',(6.95039031793588,-4.18705056366974,-3.32986147566189));
#79959=CARTESIAN_POINT('Ctrl Pts',(7.06965629035308,0.535239182461503,-5.32286472563243));
#79960=CARTESIAN_POINT('Ctrl Pts',(7.18892226277021,4.76618869399877,-2.42957099155845));
#79961=CARTESIAN_POINT('Ctrl Pts',(7.3081882351874,4.62186010975348,2.69402653953035));
#79962=CARTESIAN_POINT('Ctrl Pts',(7.42745420760454,0.234744552882073,5.34455469283609));
#79963=CARTESIAN_POINT('Ctrl Pts',(7.54672018002173,-4.36786240944341,3.08887485049092));
#79964=CARTESIAN_POINT('Ctrl Pts',(7.66598615243887,-4.9608478581489,-2.0023382326979));
#79965=CARTESIAN_POINT('Ctrl Pts',(7.78525212485605,-0.999861493359396,
-5.25543974029968));
#79966=CARTESIAN_POINT('Ctrl Pts',(7.90451809727322,3.87898028412496,-3.68413922445854));
#79967=CARTESIAN_POINT('Ctrl Pts',(8.02378406969037,5.19698581262198,1.26913684574598));
#79968=CARTESIAN_POINT('Ctrl Pts',(8.14305004210754,1.74424900381116,5.05736742609511));
#79969=CARTESIAN_POINT('Ctrl Pts',(8.2623160145247,-3.30967796970602,4.2030229129362));
#79970=CARTESIAN_POINT('Ctrl Pts',(8.38158198694187,-5.32537828988446,-0.509623330952893));
#79971=CARTESIAN_POINT('Ctrl Pts',(8.50084795935902,-2.4524742178731,-4.75444424517648));
#79972=CARTESIAN_POINT('Ctrl Pts',(8.6201139317762,2.67175841346331,-4.63476826280582));
#79973=CARTESIAN_POINT('Ctrl Pts',(8.73937990419336,5.34336341837622,-0.260455848433275));
#79974=CARTESIAN_POINT('Ctrl Pts',(8.85864587661052,3.10985399681577,4.35295049228831));
#79975=CARTESIAN_POINT('Ctrl Pts',(8.97791184902769,-1.97844715602509,4.97042419926512));
#79976=CARTESIAN_POINT('Ctrl Pts',(9.09717782144485,-5.25056832498928,1.02513517861963));
#79977=CARTESIAN_POINT('Ctrl Pts',(9.21644379386203,-3.70275934480493,-3.86121005700076));
#79978=CARTESIAN_POINT('Ctrl Pts',(9.33570976627918,1.24411813547422,-5.20303180220995));
#79979=CARTESIAN_POINT('Ctrl Pts',(9.45497573869635,5.04891686558556,-1.76856109711541));
#79980=CARTESIAN_POINT('Ctrl Pts',(9.57424171111352,4.21889796935353,3.28941785032073));
#79981=CARTESIAN_POINT('Ctrl Pts',(9.69350768353068,-0.483995682528848,
5.32776858066465));
#79982=CARTESIAN_POINT('Ctrl Pts',(9.81277365594783,-4.7425897390368,2.47532067357079));
#79983=CARTESIAN_POINT('Ctrl Pts',(9.932039628365,-4.64756912883677,-2.64942844072216));
#79984=CARTESIAN_POINT('Ctrl Pts',(10.0513056007822,-0.286161114873556,
-5.34204845411932));
#79985=CARTESIAN_POINT('Ctrl Pts',(10.1705715731993,4.33793781171498,-3.13076115529714));
#79986=CARTESIAN_POINT('Ctrl Pts',(10.2898375456165,4.97988548349452,1.95451028165742));
#79987=CARTESIAN_POINT('Ctrl Pts',(10.4091035180337,1.05038513373988,5.24557536793082));
#79988=CARTESIAN_POINT('Ctrl Pts',(10.5283694904508,-3.84335044941505,3.72129375255503));
#79989=CARTESIAN_POINT('Ctrl Pts',(10.647635462868,-5.20895735043977,-1.21907062597848));
#79990=CARTESIAN_POINT('Ctrl Pts',(10.7669014352852,-1.79283225123103,-5.04034943121707));
#79991=CARTESIAN_POINT('Ctrl Pts',(10.8861674077023,3.26908158649335,-4.23467536544114));
#79992=CARTESIAN_POINT('Ctrl Pts',(11.0054333801195,5.3300355426419,0.458356830425908));
#79993=CARTESIAN_POINT('Ctrl Pts',(11.1246993525366,2.49810982979476,4.73062544999149));
#79994=CARTESIAN_POINT('Ctrl Pts',(11.2439653249538,-2.62703713820798,4.66026241152792));
#79995=CARTESIAN_POINT('Ctrl Pts',(11.363231297371,-5.34060983050459,0.311859757169513));
#79996=CARTESIAN_POINT('Ctrl Pts',(11.4824972697881,-3.15159584196975,-4.32282471524157));
#79997=CARTESIAN_POINT('Ctrl Pts',(11.6017632422053,1.93052816369304,-4.98923149182437));
#79998=CARTESIAN_POINT('Ctrl Pts',(11.7210292146225,5.24046098470274,-1.07561077422649));
#79999=CARTESIAN_POINT('Ctrl Pts',(11.8402951870396,3.73974201866875,3.8254018747875));
#80000=CARTESIAN_POINT('Ctrl Pts',(11.9595611594568,-1.1939948970662,5.21476232014501));
#80001=CARTESIAN_POINT('Ctrl Pts',(12.078827131874,-5.0316653213112,1.81706190432193));
#80002=CARTESIAN_POINT('Ctrl Pts',(12.1980931042911,-4.2503547359791,-3.24866964897392));
#80003=CARTESIAN_POINT('Ctrl Pts',(12.3173590767083,0.432707368140066,-5.33217912333988));
#80004=CARTESIAN_POINT('Ctrl Pts',(12.4366250491255,4.71855165499341,-2.52084115901474));
#80005=CARTESIAN_POINT('Ctrl Pts',(12.5558910215426,4.67284781705142,2.6045850242413));
#80006=CARTESIAN_POINT('Ctrl Pts',(12.6751569939598,0.337551180441248,5.33904758083378));
#80007=CARTESIAN_POINT('Ctrl Pts',(12.7944229663769,-4.30761155271047,3.17235757454594));
#80008=CARTESIAN_POINT('Ctrl Pts',(12.9136889387941,-4.99846200791051,-1.90650135727714));
#80009=CARTESIAN_POINT('Ctrl Pts',(13.0329549112113,-1.10081151614861,-5.23522529369453));
#80010=CARTESIAN_POINT('Ctrl Pts',(13.1522208836285,3.80736474859714,-3.75810371609987));
#80011=CARTESIAN_POINT('Ctrl Pts',(13.2714868560456,5.22044657695045,1.16889152919789));
#80012=CARTESIAN_POINT('Ctrl Pts',(13.3907528284628,1.84124949551275,5.02286473689053));
#80013=CARTESIAN_POINT('Ctrl Pts',(13.5100188008799,-3.22818251026418,4.26593571801641));
#80014=CARTESIAN_POINT('Ctrl Pts',(13.6292847732971,-5.33419927313827,-0.407047889412836));
#80015=CARTESIAN_POINT('Ctrl Pts',(13.7485507457143,-2.54351413503901,-4.70636863353064));
#80016=CARTESIAN_POINT('Ctrl Pts',(13.8678167181314,2.58207261855057,-4.68532505407631));
#80017=CARTESIAN_POINT('Ctrl Pts',(13.9870826905486,5.33736174127025,-0.363234789975878));
#80018=CARTESIAN_POINT('Ctrl Pts',(14.1063486629658,3.19304587242686,4.29229867628082));
#80019=CARTESIAN_POINT('Ctrl Pts',(14.2256146353829,-1.88243041858965,5.00757681808199));
#80020=CARTESIAN_POINT('Ctrl Pts',(14.3448806078001,-5.22986841610334,1.12598677615193));
#80021=CARTESIAN_POINT('Ctrl Pts',(14.4641465802173,-3.77637841980645,-3.7892394883729));
#80022=CARTESIAN_POINT('Ctrl Pts',(14.5834125526344,1.14376110347399,-5.22600998927515));
#80023=CARTESIAN_POINT('Ctrl Pts',(14.7026785250516,5.01394788167348,-1.86539446490182));
#80024=CARTESIAN_POINT('Ctrl Pts',(14.8219444974688,4.28141795087999,3.20762064460667));
#80025=CARTESIAN_POINT('Ctrl Pts',(14.9412104698859,-0.381378988217642,
5.33609594527402));
#80026=CARTESIAN_POINT('Ctrl Pts',(15.0604764423031,-4.69407666761928,2.56612823302666));
#80027=CARTESIAN_POINT('Ctrl Pts',(15.1797424147203,-4.69769383377592,-2.55950044225979));
#80028=CARTESIAN_POINT('Ctrl Pts',(15.2990083871374,-0.388909991241378,
-5.33555235083833));
#80029=CARTESIAN_POINT('Ctrl Pts',(15.4182743595546,4.27688644041953,-3.21366025671349));
#80030=CARTESIAN_POINT('Ctrl Pts',(15.5375403319717,5.01657571134664,1.85831590483193));
#80031=CARTESIAN_POINT('Ctrl Pts',(15.6568063043889,1.15113597147179,5.22439047593186));
#80032=CARTESIAN_POINT('Ctrl Pts',(15.7760722768061,-3.77102651368367,3.79456570676));
#80033=CARTESIAN_POINT('Ctrl Pts',(15.8953382492232,-5.23145242833573,-1.11860420162119));
#80034=CARTESIAN_POINT('Ctrl Pts',(16.0146042216404,-1.88949625357401,-5.00491496207014));
#80035=CARTESIAN_POINT('Ctrl Pts',(16.1338701940576,3.18698452797358,-4.2968010761823));
#80036=CARTESIAN_POINT('Ctrl Pts',(16.2531361664747,5.33786909584254,0.355701258745961));
#80037=CARTESIAN_POINT('Ctrl Pts',(16.3724021388919,2.58868292949964,4.68167604179753));
#80038=CARTESIAN_POINT('Ctrl Pts',(16.4916681113091,-2.53686901787644,4.70995386983385));
#80039=CARTESIAN_POINT('Ctrl Pts',(16.6109340837262,-5.33361945142245,0.414576189900464));
#80040=CARTESIAN_POINT('Ctrl Pts',(16.7302000561434,-3.23420025021777,-4.26137520189376));
#80041=CARTESIAN_POINT('Ctrl Pts',(16.8494660285605,1.83415837421399,-5.02545847939519));
#80042=CARTESIAN_POINT('Ctrl Pts',(16.9687320009777,5.21879159998521,-1.17625851994709));
#80043=CARTESIAN_POINT('Ctrl Pts',(17.0879979733949,3.81266515595566,3.75272624612899));
#80044=CARTESIAN_POINT('Ctrl Pts',(17.2072639458121,-1.09342140597902,5.23677376814878));
#80045=CARTESIAN_POINT('Ctrl Pts',(17.3265299182292,-4.99576618717741,1.91355430361389));
#80046=CARTESIAN_POINT('Ctrl Pts',(17.4457958906464,-4.31208473783005,-3.16627463805604));
#80047=CARTESIAN_POINT('Ctrl Pts',(17.5650618630635,0.330015295393627,-5.33951868379825));
#80048=CARTESIAN_POINT('Ctrl Pts',(17.6843278354807,4.66916704311892,-2.61117770235508));
#80049=CARTESIAN_POINT('Ctrl Pts',(17.8035938078979,4.72210487845107,2.51417886927967));
#80050=CARTESIAN_POINT('Ctrl Pts',(17.922859780315,0.440232791824194,5.33156308776582));
#80051=CARTESIAN_POINT('Ctrl Pts',(18.0421257527322,-4.24576531976245,3.25466537747382));
#80052=CARTESIAN_POINT('Ctrl Pts',(18.1613917251494,-5.03422491660662,-1.80995838594174));
#80053=CARTESIAN_POINT('Ctrl Pts',(18.2806576975665,-1.20135384003343,-5.21307191786773));
#80054=CARTESIAN_POINT('Ctrl Pts',(18.3999236699837,3.73433910932905,-3.83067634842202));
#80055=CARTESIAN_POINT('Ctrl Pts',(18.5191896424009,5.24197388553433,1.06821329948656));
#80056=CARTESIAN_POINT('Ctrl Pts',(18.638455614818,1.9375680581184,4.98650176877373));
#80057=CARTESIAN_POINT('Ctrl Pts',(18.7577215872352,-3.14549145425294,4.32726858203256));
#80058=CARTESIAN_POINT('Ctrl Pts',(18.8769875596524,-5.34104467095598,-0.304321692747175));
#80059=CARTESIAN_POINT('Ctrl Pts',(18.9962535320695,-2.63361203087714,-4.65654996114543));
#80060=CARTESIAN_POINT('Ctrl Pts',(19.1155195044867,2.49143052170795,-4.73414657835247));
#80061=CARTESIAN_POINT('Ctrl Pts',(19.2347854769038,5.32938330746976,-0.465879203105705));
#80062=CARTESIAN_POINT('Ctrl Pts',(19.354051449321,3.27505516474859,4.23005715536775));
#80063=CARTESIAN_POINT('Ctrl Pts',(19.4733174217382,-1.78571650020385,5.04287482005294));
#80064=CARTESIAN_POINT('Ctrl Pts',(19.5925833941553,-5.20723156198039,1.22642135081669));
#80065=CARTESIAN_POINT('Ctrl Pts',(19.7118493665725,-3.84859886723042,-3.71586552891477));
#80066=CARTESIAN_POINT('Ctrl Pts',(19.8311153389897,1.04298046566866,-5.24705266011862));
#80067=CARTESIAN_POINT('Ctrl Pts',(19.9503813114068,4.97712192131473,-1.9615369612098));
#80068=CARTESIAN_POINT('Ctrl Pts',(20.069647283824,4.34235225730947,3.12463545765959));
#80069=CARTESIAN_POINT('Ctrl Pts',(20.1889132562412,-0.278621045569882,
5.34244702199188));
#80070=CARTESIAN_POINT('Ctrl Pts',(20.3081792286583,-4.64382508794112,2.65598539574908));
#80071=CARTESIAN_POINT('Ctrl Pts',(20.4274452010755,-4.74607869079302,-2.46862450174681));
#80072=CARTESIAN_POINT('Ctrl Pts',(20.5467111734927,-0.491514830074133,
-5.32708016099266));
#80073=CARTESIAN_POINT('Ctrl Pts',(20.6659771459098,4.21425107232707,-3.29536914005304));
#80074=CARTESIAN_POINT('Ctrl Pts',(20.785243118327,5.05140798950344,1.76143327815877));
#80075=CARTESIAN_POINT('Ctrl Pts',(20.9045090907442,1.25146047202657,5.20127066751764));
#80076=CARTESIAN_POINT('Ctrl Pts',(21.0237750631613,-3.69730593251821,3.86643229750494));
#80077=CARTESIAN_POINT('Ctrl Pts',(21.1430410355785,-5.25200997433651,-1.01772348862257));
#80078=CARTESIAN_POINT('Ctrl Pts',(21.2623070079956,-1.98546045804875,-4.96762686192806));
#80079=CARTESIAN_POINT('Ctrl Pts',(21.3815729804128,3.10370713105701,-4.35733541449928));
#80080=CARTESIAN_POINT('Ctrl Pts',(21.50083895283,5.34372570444373,0.252913948788086));
#80081=CARTESIAN_POINT('Ctrl Pts',(21.6201049252471,2.67829727906562,4.63099271806533));
#80082=CARTESIAN_POINT('Ctrl Pts',(21.7393708976643,-2.44576133731702,4.75790093956452));
#80083=CARTESIAN_POINT('Ctrl Pts',(21.8586368700814,-5.32465370164826,0.517139079308235));
#80084=CARTESIAN_POINT('Ctrl Pts',(21.9779028424986,-3.31560683315326,-4.19834743652449));
#80085=CARTESIAN_POINT('Ctrl Pts',(22.0971688149158,1.73710928192197,-5.05982422742967));
#80086=CARTESIAN_POINT('Ctrl Pts',(22.2164347873329,5.19518937246391,-1.27647062404992));
#80087=CARTESIAN_POINT('Ctrl Pts',(22.3357007597501,3.88417622643207,3.67866074976264));
#80088=CARTESIAN_POINT('Ctrl Pts',(22.4549667321673,-0.992442953004545,
5.25684571343457));
#80089=CARTESIAN_POINT('Ctrl Pts',(22.5742327045844,-4.95801681040808,2.00933799484685));
#80090=CARTESIAN_POINT('Ctrl Pts',(22.6934986770016,-4.37221770676746,-3.08270695890047));
#80091=CARTESIAN_POINT('Ctrl Pts',(22.8127646494188,0.227200997477541,-5.34488068871223));
#80092=CARTESIAN_POINT('Ctrl Pts',(22.9320306218359,4.61805314856548,-2.70054716434442));
#80093=CARTESIAN_POINT('Ctrl Pts',(23.0512965942531,4.76961305100215,2.42284155766206));
#80094=CARTESIAN_POINT('Ctrl Pts',(23.1705625666702,0.542751357650036,5.32210398560502));
#80095=CARTESIAN_POINT('Ctrl Pts',(23.2898285390875,-4.18234661610206,3.33576777558089));
#80096=CARTESIAN_POINT('Ctrl Pts',(23.4090945115045,-5.06812333901019,-1.71274507455268));
#80097=CARTESIAN_POINT('Ctrl Pts',(23.5283604839218,-1.30145122794406,-5.1889878175909));
#80098=CARTESIAN_POINT('Ctrl Pts',(23.6476264563389,3.65993041225227,-3.90183024326985));
#80099=CARTESIAN_POINT('Ctrl Pts',(23.7668924287561,5.26155976547379,0.967139444016044));
#80100=CARTESIAN_POINT('Ctrl Pts',(23.8861584011732,2.03316901887958,4.94829198921123));
#80101=CARTESIAN_POINT('Ctrl Pts',(24.0054243735904,-3.06163542730824,4.38699878961408));
#80102=CARTESIAN_POINT('Ctrl Pts',(24.1246903460076,-5.34591194806159,-0.201482786849391));
#80103=CARTESIAN_POINT('Ctrl Pts',(24.2439563184247,-2.72273453653836,-4.60500667897073));
#80104=CARTESIAN_POINT('Ctrl Pts',(24.3632222908419,2.39986569333583,-4.78121475399025));
#80105=CARTESIAN_POINT('Ctrl Pts',(24.4824882632591,5.31943107188467,-0.568351072218813));
#80106=CARTESIAN_POINT('Ctrl Pts',(24.6017542356763,3.35585150064429,4.16624898145168));
#80107=CARTESIAN_POINT('Ctrl Pts',(24.7210202080934,-1.6883412200409,5.0763051321345));
#80108=CARTESIAN_POINT('Ctrl Pts',(24.8402861805106,-5.1826661464542,1.32640170545049));
#80109=CARTESIAN_POINT('Ctrl Pts',(24.9595521529277,-3.9193939393577,-3.64111535356268));
#80110=CARTESIAN_POINT('Ctrl Pts',(25.0788181253449,0.941813547390232,-5.2661520213317));
#80111=CARTESIAN_POINT('Ctrl Pts',(25.1980840977621,4.93845262345068,-2.05695297849937));
#80112=CARTESIAN_POINT('Ctrl Pts',(25.3173500701792,4.40167832088221,3.04049302405052));
#80113=CARTESIAN_POINT('Ctrl Pts',(25.4366160425964,-0.175759912236459,
5.34681945861972));
#80114=CARTESIAN_POINT('Ctrl Pts',(25.5558820150136,-4.59185361128473,2.74485888204762));
#80115=CARTESIAN_POINT('Ctrl Pts',(25.6751479874307,-4.79270577996915,-2.37683427619063));
#80116=CARTESIAN_POINT('Ctrl Pts',(25.7944139598479,-0.593937630424711,
-5.31663502236041));
#80117=CARTESIAN_POINT('Ctrl Pts',(25.9136799322651,4.15005490520629,-3.37585754343952));
#80118=CARTESIAN_POINT('Ctrl Pts',(26.0329459046822,5.08436941740803,1.66389828329445));
#80119=CARTESIAN_POINT('Ctrl Pts',(26.1522118770994,1.35132147900805,5.17622450538955));
#80120=CARTESIAN_POINT('Ctrl Pts',(26.2714778495166,-3.62221600923054,3.93686690812609));
#80121=CARTESIAN_POINT('Ctrl Pts',(26.3907438219337,-5.27062237470552,-0.916465849378926));
#80122=CARTESIAN_POINT('Ctrl Pts',(26.5100097943509,-2.08068932314761,-4.92849894089096));
#80123=CARTESIAN_POINT('Ctrl Pts',(26.629275766768,3.01928023853817,-4.41625596076554));
#80124=CARTESIAN_POINT('Ctrl Pts',(26.7485417391852,5.34760319937945,0.1500329690799));
#80125=CARTESIAN_POINT('Ctrl Pts',(26.8678077116024,2.76691968873083,4.57859424997864));
#80126=CARTESIAN_POINT('Ctrl Pts',(26.9870736840195,-2.35374783936478,4.80408586294104));
#80127=CARTESIAN_POINT('Ctrl Pts',(27.1063396564367,-5.31371590175628,0.619510439982084));
#80128=CARTESIAN_POINT('Ctrl Pts',(27.2256056288538,-3.39578544086029,-4.13376476223128));
#80129=CARTESIAN_POINT('Ctrl Pts',(27.344871601271,1.63941683012594,-5.09231600815622));
#80130=CARTESIAN_POINT('Ctrl Pts',(27.4641375736882,5.16966304351028,-1.37620997176607));
#80131=CARTESIAN_POINT('Ctrl Pts',(27.5834035461054,3.95424874510512,3.60323281674365));
#80132=CARTESIAN_POINT('Ctrl Pts',(27.7026695185225,-0.891096936738138,
5.27497072211403));
#80133=CARTESIAN_POINT('Ctrl Pts',(27.8219354909397,-4.91843117194308,2.10437750336837));
#80134=CARTESIAN_POINT('Ctrl Pts',(27.9412014633568,-4.43073137181643,-2.99799756181113));
#80135=CARTESIAN_POINT('Ctrl Pts',(28.060467435774,0.124302552914632,-5.34826315219841));
#80136=CARTESIAN_POINT('Ctrl Pts',(28.1797334081912,4.56522890198429,-2.78891644591795));
#80137=CARTESIAN_POINT('Ctrl Pts',(28.2989993806083,4.81535473947628,2.33060691727008));
#80138=CARTESIAN_POINT('Ctrl Pts',(28.4182653530255,0.645068908923938,5.31067377764479));
#80139=CARTESIAN_POINT('Ctrl Pts',(28.5375313254427,-4.11737892961589,3.41563473160984));
#80140=CARTESIAN_POINT('Ctrl Pts',(28.6567972978598,-5.10014472042894,-1.61489742723945));
#80141=CARTESIAN_POINT('Ctrl Pts',(28.7760632702771,-1.4010666075983,-5.1629819127029));
#80142=CARTESIAN_POINT('Ctrl Pts',(28.8953292426941,3.58416621553077,-3.97153904793497));
#80143=CARTESIAN_POINT('Ctrl Pts',(29.0145952151114,5.27919696290035,0.865707396715219));
#80144=CARTESIAN_POINT('Ctrl Pts',(29.1338611875285,2.12801697082046,4.90824954965865));
#80145=CARTESIAN_POINT('Ctrl Pts',(29.2531271599457,-2.97664548652733,4.44510421895379));
#80146=CARTESIAN_POINT('Ctrl Pts',(29.3723931323628,-5.34879930179978,-0.0985692593562008));
#80147=CARTESIAN_POINT('Ctrl Pts',(29.49165910478,-2.81084864442134,-4.55175787668666));
#80148=CARTESIAN_POINT('Ctrl Pts',(29.6109250771972,2.30741204557965,-4.82651214871964));
#80149=CARTESIAN_POINT('Ctrl Pts',(29.7301910496143,5.30750872044597,-0.670612445614996));
#80150=CARTESIAN_POINT('Ctrl Pts',(29.8494570220315,3.43540495621067,4.10089778666421));
#80151=CARTESIAN_POINT('Ctrl Pts',(29.9687229944486,-1.59034064221755,5.10785537300494));
#80152=CARTESIAN_POINT('Ctrl Pts',(30.0879889668658,-5.15618126762428,1.42589081111571));
#80153=CARTESIAN_POINT('Ctrl Pts',(30.207254939283,-3.9887374163744,-3.56501664695121));
#80154=CARTESIAN_POINT('Ctrl Pts',(30.3265209117001,0.840297817034937,-5.28330099923434));
#80155=CARTESIAN_POINT('Ctrl Pts',(30.4457868841173,4.89795430972499,-2.15160717829025));
#80156=CARTESIAN_POINT('Ctrl Pts',(30.5650528565345,4.45937416947051,2.95522450695096));
#80157=CARTESIAN_POINT('Ctrl Pts',(30.6843188289516,-0.0728336840866598,
5.34921163577276));
#80158=CARTESIAN_POINT('Ctrl Pts',(30.8035848013688,-4.53818148591717,2.83271577654773));
#80159=CARTESIAN_POINT('Ctrl Pts',(30.922850773786,-4.83755783239591,-2.28416376121532));
#80160=CARTESIAN_POINT('Ctrl Pts',(31.0421167462031,-0.696140458765788,
-5.30422080342567));
#80161=CARTESIAN_POINT('Ctrl Pts',(31.1613827186203,4.08432171488679,-3.45509565701559));
#80162=CARTESIAN_POINT('Ctrl Pts',(31.2806486910375,5.11544778739555,1.56574704350808));
#80163=CARTESIAN_POINT('Ctrl Pts',(31.3999146634546,1.45068200768019,5.14926126569795));
#80164=CARTESIAN_POINT('Ctrl Pts',(31.5191806358718,-3.54578455428506,4.00584345231029));
#80165=CARTESIAN_POINT('Ctrl Pts',(31.638446608289,-5.28728273611438,-0.814868785885891));
#80166=CARTESIAN_POINT('Ctrl Pts',(31.7577125807061,-2.17514757970455,-4.88754569045954));
#80167=CARTESIAN_POINT('Ctrl Pts',(31.8769785531233,2.9337351189414,-4.47354089304141));
#80168=CARTESIAN_POINT('Ctrl Pts',(31.9962445255404,5.34950014457238,0.047096422840884));
#80169=CARTESIAN_POINT('Ctrl Pts',(32.1155104979576,2.85451733611025,4.52450004394633));
#80170=CARTESIAN_POINT('Ctrl Pts',(32.2347764703748,-2.26086260233548,4.84849153481623));
#80171=CARTESIAN_POINT('Ctrl Pts',(32.3540424427919,-5.30081010269343,0.721652357446135));
#80172=CARTESIAN_POINT('Ctrl Pts',(32.4733084152091,-3.47470637821841,-4.06765109799164));
#80173=CARTESIAN_POINT('Ctrl Pts',(32.5925743876263,1.54111720041119,-5.12292178784925));
#80174=CARTESIAN_POINT('Ctrl Pts',(32.7118403600434,5.14222206711005,-1.47543962341761));
#80175=CARTESIAN_POINT('Ctrl Pts',(32.8311063324606,4.02285675976709,3.52647038272272));
#80176=CARTESIAN_POINT('Ctrl Pts',(32.9503723048777,-0.789420891907063,
5.29114208137));
#80177=CARTESIAN_POINT('Ctrl Pts',(33.0696382772949,-4.87702393280405,2.19863763014299));
#80178=CARTESIAN_POINT('Ctrl Pts',(33.1889042497121,-4.487604061731,-2.91217781994159));
#80179=CARTESIAN_POINT('Ctrl Pts',(33.3081702221293,0.0213580713928514,
-5.34966482152014));
#80180=CARTESIAN_POINT('Ctrl Pts',(33.4274361945464,4.51071386747616,-2.87625281843973));
#80181=CARTESIAN_POINT('Ctrl Pts',(33.5467021669636,4.85931300288409,2.23750910832247));
#80182=CARTESIAN_POINT('Ctrl Pts',(33.6659681393807,0.747147551098779,5.29727669720119));
#80183=CARTESIAN_POINT('Ctrl Pts',(33.785234111798,-4.05088632187509,3.49423666586414));
#80184=CARTESIAN_POINT('Ctrl Pts',(33.904500084215,-5.13027720135584,-1.51645168306597));
#80185=CARTESIAN_POINT('Ctrl Pts',(34.0237660566323,-1.50016308523093,-5.13506383480611));
#80186=CARTESIAN_POINT('Ctrl Pts',(34.1430320290494,3.50707457935405,-4.03977694491552));
#80187=CARTESIAN_POINT('Ctrl Pts',(34.2622980014666,5.29487894566462,0.763954724174054));
#80188=CARTESIAN_POINT('Ctrl Pts',(34.3815639738838,2.22207678584961,4.86638928031932));
#80189=CARTESIAN_POINT('Ctrl Pts',(34.5008299463009,-2.89055310896428,4.5015633500008));
#80190=CARTESIAN_POINT('Ctrl Pts',(34.6200959187181,-5.34970566280806,0.00438077445810644));
#80191=CARTESIAN_POINT('Ctrl Pts',(34.7393618911352,-2.89792172038924,-4.49682327563297));
#80192=CARTESIAN_POINT('Ctrl Pts',(34.8586278635524,2.21410381975605,-4.8700219861014));
#80193=CARTESIAN_POINT('Ctrl Pts',(34.9778938359695,5.29362066876786,-0.772625449552068));
#80194=CARTESIAN_POINT('Ctrl Pts',(35.0971598083868,3.51368606780953,4.03402777461097));
#80195=CARTESIAN_POINT('Ctrl Pts',(35.2164257808038,-1.49175106234197,5.13751385765428));
#80196=CARTESIAN_POINT('Ctrl Pts',(35.3356917532211,-5.12778673466809,1.52485182080563));
#80197=CARTESIAN_POINT('Ctrl Pts',(35.4549577256382,-4.05660361573838,-3.48759759314308));
#80198=CARTESIAN_POINT('Ctrl Pts',(35.5742236980554,0.738470871532858,-5.29849324252636));
#80199=CARTESIAN_POINT('Ctrl Pts',(35.6934896704726,4.85564198041892,-2.24546450419021));
#80200=CARTESIAN_POINT('Ctrl Pts',(35.8127556428897,4.5154184323632,2.86886148647546));
#80201=CARTESIAN_POINT('Ctrl Pts',(35.9320216153069,0.0301195233717248,
5.34962266769844));
#80202=CARTESIAN_POINT('Ctrl Pts',(36.051287587724,-4.48282859845072,2.91952353996583));
#80203=CARTESIAN_POINT('Ctrl Pts',(36.1705535601412,-4.88061822044823,-2.19064727767925));
#80204=CARTESIAN_POINT('Ctrl Pts',(36.2898195325583,-0.79808549366158,-5.28984210344808));
#80205=CARTESIAN_POINT('Ctrl Pts',(36.4090855049755,4.01707590461207,-3.53305413112963));
#80206=CARTESIAN_POINT('Ctrl Pts',(36.5283514773927,5.14463147875642,1.46701590488028));
#80207=CARTESIAN_POINT('Ctrl Pts',(36.6476174498098,1.54950546845328,5.12039094490375));
#80208=CARTESIAN_POINT('Ctrl Pts',(36.7668834222271,-3.46804027343879,4.07333636419893));
#80209=CARTESIAN_POINT('Ctrl Pts',(36.8861493946441,-5.30198413145758,-0.712969888702118));
#80210=CARTESIAN_POINT('Ctrl Pts',(37.0054153670614,-2.26880168119574,-4.84478234871799));
#80211=CARTESIAN_POINT('Ctrl Pts',(37.1246813394785,2.84710618461792,-4.5291688611629));
#80212=CARTESIAN_POINT('Ctrl Pts',(37.2439473118957,5.34941065311671,-0.0558578206189876));
#80213=CARTESIAN_POINT('Ctrl Pts',(37.3632132843128,2.9410676247427,4.46873061775304));
#80214=CARTESIAN_POINT('Ctrl Pts',(37.48247925673,-2.16715872819103,4.89110059102707));
#80215=CARTESIAN_POINT('Ctrl Pts',(37.6017452291471,-5.28590556674589,0.823528745687691));
#80216=CARTESIAN_POINT('Ctrl Pts',(37.7210112015644,-3.55240787274374,-4.00003424114442));
#80217=CARTESIAN_POINT('Ctrl Pts',(37.8402771739814,1.44237491738078,-5.15162394203852));
#80218=CARTESIAN_POINT('Ctrl Pts',(37.9595431463987,5.11263327306786,-1.57413477445065));
#80219=CARTESIAN_POINT('Ctrl Pts',(38.0788091188158,4.09043705061455,3.44842457930616));
#80220=CARTESIAN_POINT('Ctrl Pts',(38.198075091233,-0.688330618759455,5.30531057884261));
#80221=CARTESIAN_POINT('Ctrl Pts',(38.3173410636501,-4.83213982762216,2.29216646455193));
#80222=CARTESIAN_POINT('Ctrl Pts',(38.4366070360674,-4.54601128230848,-2.82544487853224));
#80223=CARTESIAN_POINT('Ctrl Pts',(38.5558730084845,-0.0753220462620636,
-5.34870520161382));
#80224=CARTESIAN_POINT('Ctrl Pts',(38.6552613188321,3.68821096221221,-3.36131348540175));
#80225=CARTESIAN_POINT('Ctrl Pts',(38.7347719671102,4.6906167652542,-0.404679689500564));
#80226=CARTESIAN_POINT('Ctrl Pts',(38.7745272912493,4.44656964843245,1.12242207018042));
#80227=CARTESIAN_POINT('Ctrl Pts',(38.7944049533188,4.14471859505469,1.81262843139675));
#80228=CARTESIAN_POINT('Ctrl Pts',(38.546,4.53891924175751,1.98502597383594));
#80229=CARTESIAN_POINT('Ctrl Pts',(38.5261223379305,4.86947909109343,1.22917467492126));
#80230=CARTESIAN_POINT('Ctrl Pts',(38.5062446758609,5.0031082059578,0.393003122839607));
#80231=CARTESIAN_POINT('Ctrl Pts',(38.4863670137914,4.93270479300402,-0.429812242173168));
#80232=CARTESIAN_POINT('Ctrl Pts',(38.4664893517219,4.86230138005024,-1.25262760718594));
#80233=CARTESIAN_POINT('Ctrl Pts',(38.4466116896524,4.58786543927832,-2.06208678512975));
#80234=CARTESIAN_POINT('Ctrl Pts',(38.4267340275828,4.1301428507968,-2.74682029345583));
#80235=CARTESIAN_POINT('Ctrl Pts',(38.3869787034438,3.21469767383359,-4.11628731010823));
#80236=CARTESIAN_POINT('Ctrl Pts',(38.3472233793047,1.56610590603186,-4.98685164828932));
#80237=CARTESIAN_POINT('Ctrl Pts',(38.3074680551656,-0.0741720898843624,
-4.96159290771613));
#80238=CARTESIAN_POINT('Ctrl Pts',(38.2677127310266,-1.71445008580022,-4.93633416714295));
#80239=CARTESIAN_POINT('Ctrl Pts',(38.2279574068875,-3.34641430983077,-4.01525234781577));
#80240=CARTESIAN_POINT('Ctrl Pts',(38.1882020827485,-4.21462008633842,-2.620654273424));
#80241=CARTESIAN_POINT('Ctrl Pts',(38.166064292547,-4.69808130186775,-1.84407100426816));
#80242=CARTESIAN_POINT('Ctrl Pts',(38.1439265023456,-4.94471401759233,-0.920658400937587));
#80243=CARTESIAN_POINT('Ctrl Pts',(38.1217887121441,-4.94678507297176,0.00149831882859774));
#80244=CARTESIAN_POINT('Origin',(-20.5573438024112,0.,0.));
#80245=CARTESIAN_POINT('',(-18.6,-2.5,-3.06161699786838E-16));
#80246=CARTESIAN_POINT('Origin',(-18.6,0.,0.));
#80247=CARTESIAN_POINT('',(-22.5146876048223,-2.5,-3.06161699786838E-16));
#80248=CARTESIAN_POINT('',(-20.5573438024112,-2.5,-3.06161699786838E-16));
#80249=CARTESIAN_POINT('Origin',(-22.5146876048223,0.,0.));
#80250=CARTESIAN_POINT('Origin',(-18.1,0.,0.));
#80251=CARTESIAN_POINT('',(-18.1,-3.75,-4.59242549680257E-16));
#80252=CARTESIAN_POINT('Origin',(10.45,0.,0.));
#80253=CARTESIAN_POINT('Origin',(38.546,0.,0.));
#80254=CARTESIAN_POINT('Origin',(38.75,0.,0.));
#80255=CARTESIAN_POINT('',(39.,-4.5,-5.51091059616309E-16));
#80256=CARTESIAN_POINT('Origin',(39.,0.,0.));
#80257=CARTESIAN_POINT('',(38.75,-4.75,-5.81707229594993E-16));
#80258=CARTESIAN_POINT('Origin',(39.,0.,0.));
#80259=CARTESIAN_POINT('Origin',(-24.173,-3.33066907387547E-15,0.));
#80260=CARTESIAN_POINT('',(-24.173,-3.33066907387547E-15,3.00000000000001));
#80261=CARTESIAN_POINT('',(-24.173,-3.33066907387547E-15,-3.00000000000001));
#80262=CARTESIAN_POINT('Origin',(-24.173,-3.33066907387547E-15,0.));
#80263=CARTESIAN_POINT('',(0.,0.,0.));
#80264=CARTESIAN_POINT('Origin',(27.25,0.,0.));
#80265=CARTESIAN_POINT('',(27.,5.55,-6.79678973526781E-16));
#80266=CARTESIAN_POINT('Origin',(27.,0.,0.));
#80267=CARTESIAN_POINT('',(27.5,5.05,6.18446633569413E-16));
#80268=CARTESIAN_POINT('',(27.25,5.3,-6.49062803548097E-16));
#80269=CARTESIAN_POINT('',(27.5,-5.05,-6.18446633569413E-16));
#80270=CARTESIAN_POINT('Origin',(27.5,0.,0.));
#80271=CARTESIAN_POINT('Origin',(27.5,0.,0.));
#80272=CARTESIAN_POINT('Origin',(38.,0.,0.));
#80273=CARTESIAN_POINT('',(49.,-5.05,-6.18446633569413E-16));
#80274=CARTESIAN_POINT('Origin',(49.,0.,0.));
#80275=CARTESIAN_POINT('',(38.,-5.05,-6.18446633569413E-16));
#80276=CARTESIAN_POINT('Origin',(27.,7.6,0.));
#80277=CARTESIAN_POINT('',(27.,-7.6,-9.30731567351989E-16));
#80278=CARTESIAN_POINT('Origin',(27.,0.,0.));
#80279=CARTESIAN_POINT('Origin',(41.725,9.16562810019684,-1.42563428843676));
#80280=CARTESIAN_POINT('',(54.3836840636427,9.00782597316669,-1.02818086692503));
#80281=CARTESIAN_POINT('',(53.95,9.32343022722099,-1.82308770994211));
#80282=CARTESIAN_POINT('Ctrl Pts',(54.3836840636427,9.00782597316669,-1.02818086692503));
#80283=CARTESIAN_POINT('Ctrl Pts',(54.1865412262364,9.16194205564155,-1.41635031333084));
#80284=CARTESIAN_POINT('Ctrl Pts',(53.95,9.32343022722099,-1.82308770994211));
#80285=CARTESIAN_POINT('',(30.5,9.32343022722099,-1.82308770994211));
#80286=CARTESIAN_POINT('',(41.725,9.32343022722099,-1.82308770994211));
#80287=CARTESIAN_POINT('',(30.5,9.00782597317269,-1.0281808669314));
#80288=CARTESIAN_POINT('',(30.5,8.98477062633365,-0.970111773326804));
#80289=CARTESIAN_POINT('',(41.725,9.00782597317269,-1.02818086693141));
#80290=CARTESIAN_POINT('Origin',(30.5,10.1,0.));
#80291=CARTESIAN_POINT('',(30.5,9.00782597317269,1.0281808669314));
#80292=CARTESIAN_POINT('Origin',(30.5,10.1,0.));
#80293=CARTESIAN_POINT('',(54.3836840636427,9.00782597316669,1.02818086692503));
#80294=CARTESIAN_POINT('',(41.725,9.00782597317269,1.02818086693141));
#80295=CARTESIAN_POINT('',(54.75,8.68564356435644,0.499595709502806));
#80296=CARTESIAN_POINT('Ctrl Pts',(54.75,8.68564356435643,0.499595709502812));
#80297=CARTESIAN_POINT('Ctrl Pts',(54.687196533521,8.73974159983834,0.652747354291056));
#80298=CARTESIAN_POINT('Ctrl Pts',(54.5981025051697,8.81720407288878,0.789394637203874));
#80299=CARTESIAN_POINT('Ctrl Pts',(54.4672398095032,8.93309472235716,0.944212036355286));
#80300=CARTESIAN_POINT('Ctrl Pts',(54.4264645321808,8.9694238698269,0.987388647197093));
#80301=CARTESIAN_POINT('Ctrl Pts',(54.3836840636385,9.00782597316448,1.02818086692269));
#80302=CARTESIAN_POINT('',(54.75,8.68564356435644,-0.499595709502806));
#80303=CARTESIAN_POINT('Origin',(54.75,10.1,0.));
#80304=CARTESIAN_POINT('Ctrl Pts',(54.3836840636385,9.00782597316448,-1.02818086692269));
#80305=CARTESIAN_POINT('Ctrl Pts',(54.4264645321807,8.9694238698269,-0.987388647197093));
#80306=CARTESIAN_POINT('Ctrl Pts',(54.4672398095032,8.93309472235716,-0.944212036355286));
#80307=CARTESIAN_POINT('Ctrl Pts',(54.5981025051697,8.81720407288878,-0.789394637203873));
#80308=CARTESIAN_POINT('Ctrl Pts',(54.687196533521,8.73974159983834,-0.65274735429106));
#80309=CARTESIAN_POINT('Ctrl Pts',(54.75,8.68564356435643,-0.499595709502813));
#80310=CARTESIAN_POINT('Origin',(41.725,9.16562810019684,1.42563428843676));
#80311=CARTESIAN_POINT('',(53.95,9.32343022722099,1.82308770994211));
#80312=CARTESIAN_POINT('Ctrl Pts',(53.95,9.32343022722099,1.82308770994211));
#80313=CARTESIAN_POINT('Ctrl Pts',(54.1865412262364,9.16194205564153,1.41635031333086));
#80314=CARTESIAN_POINT('Ctrl Pts',(54.3836840636427,9.00782597316669,1.02818086692503));
#80315=CARTESIAN_POINT('',(30.5,9.32343022722099,1.82308770994211));
#80316=CARTESIAN_POINT('',(30.5,8.98477062633365,0.970111773326804));
#80317=CARTESIAN_POINT('',(41.725,9.32343022722099,1.82308770994211));
#80318=CARTESIAN_POINT('Origin',(54.35,0.,0.));
#80319=CARTESIAN_POINT('',(53.95,9.25889390890006,2.12670721626964));
#80320=CARTESIAN_POINT('Origin',(53.95,0.,0.));
#80321=CARTESIAN_POINT('',(54.3836840636427,8.64725733530933,2.72452293712243));
#80322=CARTESIAN_POINT('Ctrl Pts',(54.3836840636427,8.64725733530933,2.72452293712243));
#80323=CARTESIAN_POINT('Ctrl Pts',(54.1865412262364,8.94593211997956,2.4325971605926));
#80324=CARTESIAN_POINT('Ctrl Pts',(53.95,9.25889390890006,2.12670721626964));
#80325=CARTESIAN_POINT('',(54.75,8.13793410669876,3.07636611524524));
#80326=CARTESIAN_POINT('Ctrl Pts',(54.3836840636385,8.64725733530636,2.72452293712367));
#80327=CARTESIAN_POINT('Ctrl Pts',(54.4264645321807,8.59558357772359,2.74616894156256));
#80328=CARTESIAN_POINT('Ctrl Pts',(54.4672398095032,8.5448337403194,2.77083634278586));
#80329=CARTESIAN_POINT('Ctrl Pts',(54.5981025051697,8.37599245469372,2.86513210081603));
#80330=CARTESIAN_POINT('Ctrl Pts',(54.687196533521,8.24964750716334,2.95845877916735));
#80331=CARTESIAN_POINT('Ctrl Pts',(54.75,8.13793410669875,3.07636611524524));
#80332=CARTESIAN_POINT('Origin',(54.75,0.,0.));
#80333=CARTESIAN_POINT('Origin',(41.725,0.,0.));
#80334=CARTESIAN_POINT('',(53.95,9.25889390890006,-2.12670721626965));
#80335=CARTESIAN_POINT('Origin',(53.95,0.,0.));
#80336=CARTESIAN_POINT('',(30.5,9.25889390890006,-2.12670721626965));
#80337=CARTESIAN_POINT('',(41.725,9.25889390890006,-2.12670721626965));
#80338=CARTESIAN_POINT('',(30.5,7.77586075855085,-5.45765420887298));
#80339=CARTESIAN_POINT('Origin',(30.5,0.,0.));
#80340=CARTESIAN_POINT('',(53.95,7.77586075855085,-5.45765420887298));
#80341=CARTESIAN_POINT('',(41.725,7.77586075855085,-5.45765420887298));
#80342=CARTESIAN_POINT('',(53.95,7.59341071931979,-5.70877514425986));
#80343=CARTESIAN_POINT('Origin',(53.95,0.,0.));
#80344=CARTESIAN_POINT('',(30.5,7.59341071931979,-5.70877514425986));
#80345=CARTESIAN_POINT('',(41.725,7.59341071931979,-5.70877514425986));
#80346=CARTESIAN_POINT('',(30.5,4.88377432324997,-8.14854271385775));
#80347=CARTESIAN_POINT('Origin',(30.5,0.,0.));
#80348=CARTESIAN_POINT('',(53.95,4.88377432324997,-8.14854271385775));
#80349=CARTESIAN_POINT('',(41.725,4.88377432324997,-8.14854271385775));
#80350=CARTESIAN_POINT('',(53.95,4.61495783239841,-8.30374398721351));
#80351=CARTESIAN_POINT('Origin',(53.95,0.,0.));
#80352=CARTESIAN_POINT('',(30.5,4.61495783239841,-8.30374398721351));
#80353=CARTESIAN_POINT('',(41.725,4.61495783239841,-8.30374398721351));
#80354=CARTESIAN_POINT('',(30.5,1.14723893976231,-9.43047415642994));
#80355=CARTESIAN_POINT('Origin',(30.5,0.,0.));
#80356=CARTESIAN_POINT('',(53.95,1.14723893976231,-9.43047415642994));
#80357=CARTESIAN_POINT('',(41.725,1.14723893976231,-9.43047415642994));
#80358=CARTESIAN_POINT('',(53.95,0.838536810679625,-9.46292005763206));
#80359=CARTESIAN_POINT('Origin',(53.95,0.,0.));
#80360=CARTESIAN_POINT('',(30.5,0.838536810679625,-9.46292005763206));
#80361=CARTESIAN_POINT('',(41.725,0.838536810679625,-9.46292005763206));
#80362=CARTESIAN_POINT('',(30.5,-2.78766447874883,-9.08179094418727));
#80363=CARTESIAN_POINT('Origin',(30.5,0.,0.));
#80364=CARTESIAN_POINT('',(53.95,-2.78766447874883,-9.08179094418727));
#80365=CARTESIAN_POINT('',(41.725,-2.78766447874883,-9.08179094418727));
#80366=CARTESIAN_POINT('',(53.95,-3.08287484347344,-8.98587128215615));
#80367=CARTESIAN_POINT('Origin',(53.95,0.,0.));
#80368=CARTESIAN_POINT('',(30.5,-3.08287484347344,-8.98587128215615));
#80369=CARTESIAN_POINT('',(41.725,-3.08287484347344,-8.98587128215615));
#80370=CARTESIAN_POINT('',(30.5,-6.24055538374756,-7.16278357221404));
#80371=CARTESIAN_POINT('Origin',(30.5,0.,0.));
#80372=CARTESIAN_POINT('',(53.95,-6.24055538374756,-7.16278357221404));
#80373=CARTESIAN_POINT('',(41.725,-6.24055538374756,-7.16278357221404));
#80374=CARTESIAN_POINT('',(53.95,-6.47122943015123,-6.95508372791763));
#80375=CARTESIAN_POINT('Origin',(53.95,0.,0.));
#80376=CARTESIAN_POINT('',(30.5,-6.47122943015123,-6.95508372791763));
#80377=CARTESIAN_POINT('',(41.725,-6.47122943015123,-6.95508372791763));
#80378=CARTESIAN_POINT('',(30.5,-8.61439756923049,-4.00526584875909));
#80379=CARTESIAN_POINT('Origin',(30.5,0.,0.));
#80380=CARTESIAN_POINT('',(53.95,-8.61439756923049,-4.00526584875909));
#80381=CARTESIAN_POINT('',(41.725,-8.61439756923049,-4.00526584875909));
#80382=CARTESIAN_POINT('',(53.95,-8.74064965908211,-3.72169901217008));
#80383=CARTESIAN_POINT('Origin',(53.95,0.,0.));
#80384=CARTESIAN_POINT('',(30.5,-8.74064965908211,-3.72169901217008));
#80385=CARTESIAN_POINT('',(41.725,-8.74064965908211,-3.72169901217008));
#80386=CARTESIAN_POINT('',(30.5,-9.49873215564839,-0.155201273355761));
#80387=CARTESIAN_POINT('Origin',(30.5,0.,0.));
#80388=CARTESIAN_POINT('',(53.95,-9.49873215564839,-0.155201273355761));
#80389=CARTESIAN_POINT('',(41.725,-9.49873215564839,-0.155201273355761));
#80390=CARTESIAN_POINT('',(53.95,-9.5,-1.16341445918999E-15));
#80391=CARTESIAN_POINT('Origin',(53.95,0.,0.));
#80392=CARTESIAN_POINT('',(29.5,-9.5,-1.16341445918999E-15));
#80393=CARTESIAN_POINT('',(41.725,-9.5,-1.16341445918999E-15));
#80394=CARTESIAN_POINT('Origin',(29.5,0.,0.));
#80395=CARTESIAN_POINT('',(53.95,-9.49873215564839,0.155201273355763));
#80396=CARTESIAN_POINT('Origin',(53.95,0.,0.));
#80397=CARTESIAN_POINT('',(30.5,-9.49873215564839,0.155201273355763));
#80398=CARTESIAN_POINT('',(41.725,-9.49873215564839,0.155201273355763));
#80399=CARTESIAN_POINT('',(30.5,-8.74064965908211,3.72169901217009));
#80400=CARTESIAN_POINT('Origin',(30.5,0.,0.));
#80401=CARTESIAN_POINT('',(53.95,-8.74064965908211,3.72169901217008));
#80402=CARTESIAN_POINT('',(41.725,-8.74064965908211,3.72169901217009));
#80403=CARTESIAN_POINT('',(53.95,-8.61439756923049,4.00526584875909));
#80404=CARTESIAN_POINT('Origin',(53.95,0.,0.));
#80405=CARTESIAN_POINT('',(30.5,-8.61439756923049,4.00526584875909));
#80406=CARTESIAN_POINT('',(41.725,-8.61439756923049,4.00526584875909));
#80407=CARTESIAN_POINT('',(30.5,-6.47122943015123,6.95508372791763));
#80408=CARTESIAN_POINT('Origin',(30.5,0.,0.));
#80409=CARTESIAN_POINT('',(53.95,-6.47122943015123,6.95508372791763));
#80410=CARTESIAN_POINT('',(41.725,-6.47122943015123,6.95508372791763));
#80411=CARTESIAN_POINT('',(53.95,-6.24055538374755,7.16278357221405));
#80412=CARTESIAN_POINT('Origin',(53.95,0.,0.));
#80413=CARTESIAN_POINT('',(30.5,-6.24055538374755,7.16278357221405));
#80414=CARTESIAN_POINT('',(41.725,-6.24055538374755,7.16278357221405));
#80415=CARTESIAN_POINT('',(30.5,-3.08287484347343,8.98587128215615));
#80416=CARTESIAN_POINT('Origin',(30.5,0.,0.));
#80417=CARTESIAN_POINT('',(53.95,-3.08287484347343,8.98587128215615));
#80418=CARTESIAN_POINT('',(41.725,-3.08287484347343,8.98587128215615));
#80419=CARTESIAN_POINT('',(53.95,-2.78766447874883,9.08179094418728));
#80420=CARTESIAN_POINT('Origin',(53.95,0.,0.));
#80421=CARTESIAN_POINT('',(30.5,-2.78766447874883,9.08179094418727));
#80422=CARTESIAN_POINT('',(41.725,-2.78766447874883,9.08179094418727));
#80423=CARTESIAN_POINT('',(30.5,0.83853681067963,9.46292005763206));
#80424=CARTESIAN_POINT('Origin',(30.5,0.,0.));
#80425=CARTESIAN_POINT('',(53.95,0.83853681067963,9.46292005763206));
#80426=CARTESIAN_POINT('',(41.725,0.83853681067963,9.46292005763206));
#80427=CARTESIAN_POINT('',(53.95,1.14723893976232,9.43047415642994));
#80428=CARTESIAN_POINT('Origin',(53.95,0.,0.));
#80429=CARTESIAN_POINT('',(30.5,1.14723893976232,9.43047415642994));
#80430=CARTESIAN_POINT('',(41.725,1.14723893976232,9.43047415642994));
#80431=CARTESIAN_POINT('',(30.5,4.61495783239842,8.30374398721351));
#80432=CARTESIAN_POINT('Origin',(30.5,0.,0.));
#80433=CARTESIAN_POINT('',(53.95,4.61495783239842,8.30374398721351));
#80434=CARTESIAN_POINT('',(41.725,4.61495783239842,8.30374398721351));
#80435=CARTESIAN_POINT('',(53.95,4.88377432324998,8.14854271385775));
#80436=CARTESIAN_POINT('Origin',(53.95,0.,0.));
#80437=CARTESIAN_POINT('',(30.5,4.88377432324998,8.14854271385775));
#80438=CARTESIAN_POINT('',(41.725,4.88377432324998,8.14854271385775));
#80439=CARTESIAN_POINT('',(30.5,7.5934107193198,5.70877514425986));
#80440=CARTESIAN_POINT('Origin',(30.5,0.,0.));
#80441=CARTESIAN_POINT('',(53.95,7.5934107193198,5.70877514425986));
#80442=CARTESIAN_POINT('',(41.725,7.5934107193198,5.70877514425986));
#80443=CARTESIAN_POINT('',(53.95,7.77586075855086,5.45765420887297));
#80444=CARTESIAN_POINT('Origin',(53.95,0.,0.));
#80445=CARTESIAN_POINT('',(30.5,7.77586075855086,5.45765420887297));
#80446=CARTESIAN_POINT('',(41.725,7.77586075855086,5.45765420887297));
#80447=CARTESIAN_POINT('',(30.5,9.25889390890006,2.12670721626964));
#80448=CARTESIAN_POINT('Origin',(30.5,0.,0.));
#80449=CARTESIAN_POINT('',(41.725,9.25889390890006,2.12670721626964));
#80450=CARTESIAN_POINT('Origin',(30.5,0.,0.));
#80451=CARTESIAN_POINT('Origin',(41.725,8.95307562210873,2.42561507669434));
#80452=CARTESIAN_POINT('',(30.5,8.6472573353174,2.72452293711905));
#80453=CARTESIAN_POINT('',(30.5,8.60257639973902,2.76819423943269));
#80454=CARTESIAN_POINT('',(41.725,8.6472573353174,2.72452293711904));
#80455=CARTESIAN_POINT('Origin',(30.5,9.22680912219027,4.10804009506558));
#80456=CARTESIAN_POINT('',(30.5,7.81085966673651,4.60310285835948));
#80457=CARTESIAN_POINT('Origin',(30.5,9.22680912219027,4.10804009506558));
#80458=CARTESIAN_POINT('',(54.3836840636427,7.81085966673362,4.60310285835122));
#80459=CARTESIAN_POINT('',(41.725,7.81085966673651,4.60310285835948));
#80460=CARTESIAN_POINT('',(54.75,7.73152634314227,3.98917289739329));
#80461=CARTESIAN_POINT('Ctrl Pts',(54.75,7.73152634314226,3.98917289739329));
#80462=CARTESIAN_POINT('Ctrl Pts',(54.687196533521,7.71865497184144,4.15108754016898));
#80463=CARTESIAN_POINT('Ctrl Pts',(54.5981025051697,7.73384100509704,4.30742787102608));
#80464=CARTESIAN_POINT('Ctrl Pts',(54.4672398095032,7.77674247228157,4.49599757651354));
#80465=CARTESIAN_POINT('Ctrl Pts',(54.4264645321808,7.79236929017938,4.55021776871212));
#80466=CARTESIAN_POINT('Ctrl Pts',(54.3836840636385,7.81085966673255,4.60310285834817));
#80467=CARTESIAN_POINT('Origin',(54.75,9.22680912219027,4.10804009506558));
#80468=CARTESIAN_POINT('Origin',(41.725,7.79336021264368,5.03037853361623));
#80469=CARTESIAN_POINT('Ctrl Pts',(53.95,7.77586075855086,5.45765420887297));
#80470=CARTESIAN_POINT('Ctrl Pts',(54.1865412262364,7.79376897625248,5.02039795094072));
#80471=CARTESIAN_POINT('Ctrl Pts',(54.3836840636427,7.81085966673362,4.60310285835122));
#80472=CARTESIAN_POINT('',(30.5,7.81341638755651,4.54067664728931));
#80473=CARTESIAN_POINT('Origin',(54.35,0.,0.));
#80474=CARTESIAN_POINT('',(54.3836840636427,6.7914993463103,6.00613197382757));
#80475=CARTESIAN_POINT('Ctrl Pts',(54.3836840636427,6.7914993463103,6.00613197382757));
#80476=CARTESIAN_POINT('Ctrl Pts',(54.1865412262364,7.18308924953125,5.86092648599811));
#80477=CARTESIAN_POINT('Ctrl Pts',(53.95,7.5934107193198,5.70877514425986));
#80478=CARTESIAN_POINT('',(54.75,6.18310191118245,6.12039629075862));
#80479=CARTESIAN_POINT('Ctrl Pts',(54.3836840636385,6.79149934630708,6.0061319738275));
#80480=CARTESIAN_POINT('Ctrl Pts',(54.4264645321807,6.73548879660653,6.00488897216444));
#80481=CARTESIAN_POINT('Ctrl Pts',(54.4672398095032,6.67909337720287,6.0067819460014));
#80482=CARTESIAN_POINT('Ctrl Pts',(54.5981025051697,6.48649564757953,6.02425146969684));
#80483=CARTESIAN_POINT('Ctrl Pts',(54.687196533521,6.33311441480502,6.05812051295347));
#80484=CARTESIAN_POINT('Ctrl Pts',(54.75,6.18310191118246,6.12039629075861));
#80485=CARTESIAN_POINT('Origin',(54.75,0.,0.));
#80486=CARTESIAN_POINT('Origin',(41.725,7.19245503281942,5.85745355904381));
#80487=CARTESIAN_POINT('',(30.5,6.79149934631905,6.00613197382777));
#80488=CARTESIAN_POINT('',(30.5,6.7329185616764,6.0278543199391));
#80489=CARTESIAN_POINT('',(41.725,6.79149934631905,6.00613197382777));
#80490=CARTESIAN_POINT('Origin',(30.5,6.75821912422447,7.50576273732168));
#80491=CARTESIAN_POINT('',(30.5,5.26332476448918,7.38210654770054));
#80492=CARTESIAN_POINT('Origin',(30.5,6.75821912422447,7.50576273732168));
#80493=CARTESIAN_POINT('',(54.3836840636427,5.2633247644899,7.38210654769182));
#80494=CARTESIAN_POINT('',(41.725,5.26332476448918,7.38210654770054));
#80495=CARTESIAN_POINT('',(54.75,5.44055797848702,6.78898585082641));
#80496=CARTESIAN_POINT('Ctrl Pts',(54.75,5.44055797848701,6.78898585082641));
#80497=CARTESIAN_POINT('Ctrl Pts',(54.687196533521,5.3629427774341,6.9316669789053));
#80498=CARTESIAN_POINT('Ctrl Pts',(54.5981025051697,5.3132265677842,7.08066769419416));
#80499=CARTESIAN_POINT('Ctrl Pts',(54.4672398095032,5.27572079926106,7.27038429083689));
#80500=CARTESIAN_POINT('Ctrl Pts',(54.4264645321808,5.26794326880725,7.32627290058613));
#80501=CARTESIAN_POINT('Ctrl Pts',(54.3836840636385,5.26332476449017,7.38210654768861));
#80502=CARTESIAN_POINT('Origin',(54.75,6.75821912422447,7.50576273732168));
#80503=CARTESIAN_POINT('Origin',(41.725,5.07354954386958,7.76532463077915));
#80504=CARTESIAN_POINT('Ctrl Pts',(53.95,4.88377432324998,8.14854271385775));
#80505=CARTESIAN_POINT('Ctrl Pts',(54.1865412262364,5.07798243670107,7.75637317394928));
#80506=CARTESIAN_POINT('Ctrl Pts',(54.3836840636427,5.2633247644899,7.38210654769182));
#80507=CARTESIAN_POINT('',(30.5,5.29105147271138,7.32611727818317));
#80508=CARTESIAN_POINT('Origin',(54.35,0.,0.));
#80509=CARTESIAN_POINT('',(54.3836840636427,3.76142942149961,8.24922622826191));
#80510=CARTESIAN_POINT('Ctrl Pts',(54.3836840636427,3.76142942149961,8.24922622826192));
#80511=CARTESIAN_POINT('Ctrl Pts',(54.1865412262364,4.1782249915217,8.27584837712899));
#80512=CARTESIAN_POINT('Ctrl Pts',(53.95,4.61495783239842,8.30374398721351));
#80513=CARTESIAN_POINT('',(54.75,3.15915522350528,8.10615434554508));
#80514=CARTESIAN_POINT('Ctrl Pts',(54.3836840636385,3.76142942149669,8.24922622826054));
#80515=CARTESIAN_POINT('Ctrl Pts',(54.4264645321808,3.71076681256147,8.22530914677537));
#80516=CARTESIAN_POINT('Ctrl Pts',(54.4672398095032,3.65847709150953,8.20410038085247));
#80517=CARTESIAN_POINT('Ctrl Pts',(54.5981025051697,3.47542481503583,8.1417230308606));
#80518=CARTESIAN_POINT('Ctrl Pts',(54.687196533521,3.32152830558866,8.11027817375286));
#80519=CARTESIAN_POINT('Ctrl Pts',(54.75,3.15915522350528,8.10615434554507));
#80520=CARTESIAN_POINT('Origin',(54.75,0.,0.));
#80521=CARTESIAN_POINT('Origin',(41.725,4.18819362695297,8.27648510773958));
#80522=CARTESIAN_POINT('',(30.5,3.76142942150752,8.24922622826565));
#80523=CARTESIAN_POINT('',(30.5,3.69907793765504,8.2452436271907));
#80524=CARTESIAN_POINT('',(41.725,3.76142942150752,8.24922622826565));
#80525=CARTESIAN_POINT('Origin',(30.5,3.12107164318697,9.60567081458105));
#80526=CARTESIAN_POINT('',(30.5,1.8057131946573,8.88467695061159));
#80527=CARTESIAN_POINT('Origin',(30.5,3.12107164318697,9.60567081458105));
#80528=CARTESIAN_POINT('',(54.3836840636427,1.80571319466151,8.88467695060392));
#80529=CARTESIAN_POINT('',(41.725,1.8057131946573,8.88467695061159));
#80530=CARTESIAN_POINT('',(54.75,2.20886771343379,8.41492147465143));
#80531=CARTESIAN_POINT('Ctrl Pts',(54.75,2.20886771343378,8.41492147465143));
#80532=CARTESIAN_POINT('Ctrl Pts',(54.687196533521,2.07992905600282,8.51369822477129));
#80533=CARTESIAN_POINT('Ctrl Pts',(54.5981025051697,1.97390698775344,8.62959574718948));
#80534=CARTESIAN_POINT('Ctrl Pts',(54.4672398095032,1.86247907162951,8.78765551190679));
#80535=CARTESIAN_POINT('Ctrl Pts',(54.4264645321807,1.83264199849617,8.83554889084895));
#80536=CARTESIAN_POINT('Ctrl Pts',(54.3836840636385,1.80571319466305,8.88467695060109));
#80537=CARTESIAN_POINT('Origin',(54.75,3.12107164318697,9.60567081458105));
#80538=CARTESIAN_POINT('Origin',(41.725,1.47647606720981,9.15757555352076));
#80539=CARTESIAN_POINT('Ctrl Pts',(53.95,1.14723893976232,9.43047415642994));
#80540=CARTESIAN_POINT('Ctrl Pts',(54.1865412262364,1.48416660182181,9.15120101074399));
#80541=CARTESIAN_POINT('Ctrl Pts',(54.3836840636427,1.80571319466151,8.88467695060392));
#80542=CARTESIAN_POINT('',(30.5,1.85381569054083,8.8448056759931));
#80543=CARTESIAN_POINT('Origin',(54.35,0.,0.));
#80544=CARTESIAN_POINT('',(54.3836840636427,0.0809741781981114,9.06595432596218));
#80545=CARTESIAN_POINT('Ctrl Pts',(54.3836840636427,0.0809741781981114,
9.06595432596218));
#80546=CARTESIAN_POINT('Ctrl Pts',(54.1865412262363,0.450907674495694,9.25980090013203));
#80547=CARTESIAN_POINT('Ctrl Pts',(53.95,0.83853681067963,9.46292005763206));
#80548=CARTESIAN_POINT('',(54.75,-0.411038102340174,8.69028467188645));
#80549=CARTESIAN_POINT('Ctrl Pts',(54.3836840636385,0.0809741781960095,
9.06595432595974));
#80550=CARTESIAN_POINT('Ctrl Pts',(54.4264645321807,0.0444195353663552,
9.02349864532112));
#80551=CARTESIAN_POINT('Ctrl Pts',(54.4672398095032,0.005276880473219,8.98285532794201));
#80552=CARTESIAN_POINT('Ctrl Pts',(54.5981025051697,-0.136578541270811,
8.85141671475685));
#80553=CARTESIAN_POINT('Ctrl Pts',(54.687196533521,-0.264380222801317,8.76009505874624));
#80554=CARTESIAN_POINT('Ctrl Pts',(54.75,-0.411038102340168,8.69028467188645));
#80555=CARTESIAN_POINT('Origin',(54.75,0.,0.));
#80556=CARTESIAN_POINT('Origin',(41.725,0.459755494441725,9.26443719180043));
#80557=CARTESIAN_POINT('',(30.5,0.0809741782038195,9.06595432596881));
#80558=CARTESIAN_POINT('',(30.5,0.0256331331450422,9.03695540561423));
#80559=CARTESIAN_POINT('',(41.725,0.0809741782038194,9.06595432596881));
#80560=CARTESIAN_POINT('Origin',(30.5,-1.0557374790033,10.0446711432196));
#80561=CARTESIAN_POINT('',(30.5,-1.96412259092021,8.85100599400572));
#80562=CARTESIAN_POINT('Origin',(30.5,-1.0557374790033,10.0446711432196));
#80563=CARTESIAN_POINT('',(54.3836840636427,-1.96412259091325,8.85100599400042));
#80564=CARTESIAN_POINT('',(41.725,-1.96412259092021,8.85100599400572));
#80565=CARTESIAN_POINT('',(54.75,-1.40475584620535,8.58584072834757));
#80566=CARTESIAN_POINT('Ctrl Pts',(54.75,-1.40475584620535,8.58584072834756));
#80567=CARTESIAN_POINT('Ctrl Pts',(54.687196533521,-1.56272329477365,8.6236337030541));
#80568=CARTESIAN_POINT('Ctrl Pts',(54.5981025051697,-1.70671904284191,8.68638829807956));
#80569=CARTESIAN_POINT('Ctrl Pts',(54.4672398095032,-1.87280220757798,8.78546126162393));
#80570=CARTESIAN_POINT('Ctrl Pts',(54.4264645321808,-1.91953972238478,8.81707820944224));
#80571=CARTESIAN_POINT('Ctrl Pts',(54.3836840636385,-1.96412259091068,8.85100599399847));
#80572=CARTESIAN_POINT('Origin',(54.75,-1.0557374790033,10.0446711432196));
#80573=CARTESIAN_POINT('Origin',(41.725,-2.37589353483452,8.9663984690965));
#80574=CARTESIAN_POINT('Ctrl Pts',(53.95,-2.78766447874883,9.08179094418728));
#80575=CARTESIAN_POINT('Ctrl Pts',(54.1865412262364,-2.36627512174276,8.96370305672978));
#80576=CARTESIAN_POINT('Ctrl Pts',(54.3836840636427,-1.96412259091325,8.85100599400042));
#80577=CARTESIAN_POINT('',(30.5,-1.90396166591106,8.83414681988681));
#80578=CARTESIAN_POINT('Origin',(54.35,0.,0.));
#80579=CARTESIAN_POINT('',(54.3836840636427,-3.61348223614116,8.31509655909415));
#80580=CARTESIAN_POINT('Ctrl Pts',(54.3836840636427,-3.61348223614116,8.31509655909415));
#80581=CARTESIAN_POINT('Ctrl Pts',(54.1865412262364,-3.35437567581821,8.64264972485202));
#80582=CARTESIAN_POINT('Ctrl Pts',(53.95,-3.08287484347343,8.98587128215615));
#80583=CARTESIAN_POINT('',(54.75,-3.91015920612708,7.7717858297009));
#80584=CARTESIAN_POINT('Ctrl Pts',(54.3836840636385,-3.61348223614209,8.31509655909106));
#80585=CARTESIAN_POINT('Ctrl Pts',(54.4264645321808,-3.62960828303242,8.26144325217917));
#80586=CARTESIAN_POINT('Ctrl Pts',(54.4672398095032,-3.64883575113587,8.20839298215165));
#80587=CARTESIAN_POINT('Ctrl Pts',(54.5981025051697,-3.72496622701463,8.03062003607524));
#80588=CARTESIAN_POINT('Ctrl Pts',(54.687196533521,-3.80457500885003,7.89521192511718));
#80589=CARTESIAN_POINT('Ctrl Pts',(54.75,-3.91015920612707,7.77178582970089));
#80590=CARTESIAN_POINT('Origin',(54.75,0.,0.));
#80591=CARTESIAN_POINT('Origin',(41.725,-3.34817853980604,8.65048392062934));
#80592=CARTESIAN_POINT('',(30.5,-3.61348223613864,8.31509655910254));
#80593=CARTESIAN_POINT('',(30.5,-3.65224387295544,8.26609549624456));
#80594=CARTESIAN_POINT('',(41.725,-3.61348223613864,8.31509655910254));
#80595=CARTESIAN_POINT('Origin',(30.5,-5.05,8.74685657822283));
#80596=CARTESIAN_POINT('',(30.5,-5.39434373703405,7.28691569217113));
#80597=CARTESIAN_POINT('Origin',(30.5,-5.05,8.74685657822283));
#80598=CARTESIAN_POINT('',(54.3836840636427,-5.39434373702553,7.28691569216912));
#80599=CARTESIAN_POINT('',(41.725,-5.39434373703405,7.28691569217113));
#80600=CARTESIAN_POINT('',(54.75,-4.77548435822936,7.27219012019809));
#80601=CARTESIAN_POINT('Ctrl Pts',(54.75,-4.77548435822936,7.27219012019809));
#80602=CARTESIAN_POINT('Ctrl Pts',(54.687196533521,-4.9351665909883,7.24246457082613));
#80603=CARTESIAN_POINT('Ctrl Pts',(54.5981025051697,-5.09223784587414,7.24122539887136));
#80604=CARTESIAN_POINT('Ctrl Pts',(54.4672398095032,-5.2842589712213,7.26418094579636));
#80605=CARTESIAN_POINT('Ctrl Pts',(54.4264645321807,-5.33981558679448,7.27405460498208));
#80606=CARTESIAN_POINT('Ctrl Pts',(54.3836840636385,-5.3943437370224,7.28691569216838));
#80607=CARTESIAN_POINT('Origin',(54.75,-5.05,8.74685657822283));
#80608=CARTESIAN_POINT('Origin',(41.725,-5.8174495603908,7.22484963219259));
#80609=CARTESIAN_POINT('Ctrl Pts',(53.95,-6.24055538374755,7.16278357221405));
#80610=CARTESIAN_POINT('Ctrl Pts',(54.1865412262364,-5.8075663798233,7.22629941152117));
#80611=CARTESIAN_POINT('Ctrl Pts',(54.3836840636427,-5.39434373702553,7.28691569216912));
#80612=CARTESIAN_POINT('',(30.5,-5.3325267533782,7.29598372291776));
#80613=CARTESIAN_POINT('Origin',(54.35,0.,0.));
#80614=CARTESIAN_POINT('',(54.3836840636427,-6.68313474439608,6.126483056878));
#80615=CARTESIAN_POINT('Ctrl Pts',(54.3836840636427,-6.68313474439608,6.126483056878));
#80616=CARTESIAN_POINT('Ctrl Pts',(54.1865412262364,-6.57965699823688,6.53110589613716));
#80617=CARTESIAN_POINT('Ctrl Pts',(53.95,-6.47122943015123,6.95508372791763));
#80618=CARTESIAN_POINT('',(54.75,-6.73317826049339,5.50947461310234));
#80619=CARTESIAN_POINT('Ctrl Pts',(54.3836840636385,-6.68313474439567,6.1264830568748));
#80620=CARTESIAN_POINT('Ctrl Pts',(54.4264645321807,-6.6760438553388,6.07090926787968));
#80621=CARTESIAN_POINT('Ctrl Pts',(54.4672398095032,-6.67203153274142,6.01462491883807));
#80622=CARTESIAN_POINT('Ctrl Pts',(54.5981025051697,-6.66927341185182,5.82125619726353));
#80623=CARTESIAN_POINT('Ctrl Pts',(54.687196533521,-6.68692421238969,5.66517492388676));
#80624=CARTESIAN_POINT('Ctrl Pts',(54.75,-6.73317826049339,5.50947461310234));
#80625=CARTESIAN_POINT('Origin',(54.75,0.,0.));
#80626=CARTESIAN_POINT('Origin',(41.725,-6.57718208727421,6.54078339240215));
#80627=CARTESIAN_POINT('',(30.5,-6.68313474439718,6.12648305688668));
#80628=CARTESIAN_POINT('',(30.5,-6.69861473382796,6.06595258045413));
#80629=CARTESIAN_POINT('',(41.725,-6.68313474439718,6.12648305688668));
#80630=CARTESIAN_POINT('Origin',(30.5,-8.17107164318697,5.93663104815398));
#80631=CARTESIAN_POINT('',(30.5,-7.89183384494033,4.46285146760933));
#80632=CARTESIAN_POINT('Origin',(30.5,-8.17107164318697,5.93663104815398));
#80633=CARTESIAN_POINT('',(54.3836840636427,-7.89183384493173,4.46285146761096));
#80634=CARTESIAN_POINT('',(41.725,-7.89183384494033,4.46285146760933));
#80635=CARTESIAN_POINT('',(54.75,-7.32048824080211,4.70111177449315));
#80636=CARTESIAN_POINT('Ctrl Pts',(54.75,-7.32048824080211,4.70111177449315));
#80637=CARTESIAN_POINT('Ctrl Pts',(54.687196533521,-7.45427474904012,4.60900751857725));
#80638=CARTESIAN_POINT('Ctrl Pts',(54.5981025051697,-7.59726246382623,4.54398884373077));
#80639=CARTESIAN_POINT('Ctrl Pts',(54.4672398095032,-7.78201935275478,4.48685775142846));
#80640=CARTESIAN_POINT('Ctrl Pts',(54.4264645321807,-7.83678882554574,4.473280876609));
#80641=CARTESIAN_POINT('Ctrl Pts',(54.3836840636385,-7.89183384492856,4.46285146761156));
#80642=CARTESIAN_POINT('Origin',(54.75,-8.17107164318697,5.93663104815398));
#80643=CARTESIAN_POINT('Origin',(41.725,-8.25311570708541,4.23405865818421));
#80644=CARTESIAN_POINT('Ctrl Pts',(53.95,-8.61439756923049,4.00526584875909));
#80645=CARTESIAN_POINT('Ctrl Pts',(54.1865412262364,-8.2446766507482,4.23940294919136));
#80646=CARTESIAN_POINT('Ctrl Pts',(54.3836840636427,-7.89183384493173,4.46285146761096));
#80647=CARTESIAN_POINT('',(30.5,-7.83904952070155,4.49627875832492));
#80648=CARTESIAN_POINT('Origin',(54.35,0.,0.));
#80649=CARTESIAN_POINT('',(54.3836840636427,-8.5972125409718,2.87854497677634));
#80650=CARTESIAN_POINT('Ctrl Pts',(54.3836840636427,-8.5972125409718,2.87854497677635));
#80651=CARTESIAN_POINT('Ctrl Pts',(54.1865412262364,-8.66725585135303,3.29027452474581));
#80652=CARTESIAN_POINT('Ctrl Pts',(53.95,-8.74064965908211,3.72169901217008));
#80653=CARTESIAN_POINT('',(54.75,-8.39196962461624,2.29452518389281));
#80654=CARTESIAN_POINT('Ctrl Pts',(54.3836840636385,-8.59721254097013,2.87854497677359));
#80655=CARTESIAN_POINT('Ctrl Pts',(54.4264645321808,-8.5681307951027,2.83065991868452));
#80656=CARTESIAN_POINT('Ctrl Pts',(54.4672398095032,-8.54157244883238,2.78087356590539));
#80657=CARTESIAN_POINT('Ctrl Pts',(54.5981025051697,-8.46040263533297,2.60534427749265));
#80658=CARTESIAN_POINT('Ctrl Pts',(54.687196533521,-8.41304347080783,2.45557771181784));
#80659=CARTESIAN_POINT('Ctrl Pts',(54.75,-8.39196962461623,2.29452518389282));
#80660=CARTESIAN_POINT('Origin',(54.75,0.,0.));
#80661=CARTESIAN_POINT('Origin',(41.725,-8.66893110002923,3.30012199447695));
#80662=CARTESIAN_POINT('',(30.5,-8.59721254097634,2.87854497678382));
#80663=CARTESIAN_POINT('',(30.5,-8.58673425221723,2.816951356054));
#80664=CARTESIAN_POINT('',(41.725,-8.59721254097634,2.87854497678382));
#80665=CARTESIAN_POINT('Origin',(30.5,-9.87929076741144,2.09990807725937));
#80666=CARTESIAN_POINT('',(30.5,-9.0247541859967,0.867119680565108));
#80667=CARTESIAN_POINT('Origin',(30.5,-9.87929076741144,2.09990807725937));
#80668=CARTESIAN_POINT('',(54.3836840636427,-9.02475418598951,0.867119680570092));
#80669=CARTESIAN_POINT('',(41.725,-9.0247541859967,0.867119680565108));
#80670=CARTESIAN_POINT('',(54.75,-8.59971320199229,1.31716849471867));
#80671=CARTESIAN_POINT('Ctrl Pts',(54.75,-8.59971320199229,1.31716849471866));
#80672=CARTESIAN_POINT('Ctrl Pts',(54.687196533521,-8.68447108302277,1.17861119484757));
#80673=CARTESIAN_POINT('Ctrl Pts',(54.5981025051697,-8.78865138282002,1.06105533666644));
#80674=CARTESIAN_POINT('Ctrl Pts',(54.4672398095032,-8.93419789077059,0.93371609001558));
#80675=CARTESIAN_POINT('Ctrl Pts',(54.4264645321807,-8.97871008136871,0.899036246189251));
#80676=CARTESIAN_POINT('Ctrl Pts',(54.3836840636385,-9.02475418598686,0.867119680571931));
#80677=CARTESIAN_POINT('Origin',(54.75,-9.87929076741144,2.09990807725937));
#80678=CARTESIAN_POINT('Origin',(41.725,-9.26174317082255,0.511160476960435));
#80679=CARTESIAN_POINT('Ctrl Pts',(53.95,-9.49873215564839,0.155201273355763));
#80680=CARTESIAN_POINT('Ctrl Pts',(54.1865412262364,-9.2562074282228,0.519475203179616));
#80681=CARTESIAN_POINT('Ctrl Pts',(54.3836840636427,-9.02475418598951,0.867119680570092));
#80682=CARTESIAN_POINT('',(30.5,-8.99012941036642,0.919126349007539));
#80683=CARTESIAN_POINT('Origin',(54.35,0.,0.));
#80684=CARTESIAN_POINT('',(54.3836840636427,-9.02475418598951,-0.867119680570087));
#80685=CARTESIAN_POINT('Ctrl Pts',(54.3836840636427,-9.02475418598951,-0.867119680570087));
#80686=CARTESIAN_POINT('Ctrl Pts',(54.1865412262364,-9.25620742822278,-0.519475203179662));
#80687=CARTESIAN_POINT('Ctrl Pts',(53.95,-9.49873215564839,-0.155201273355761));
#80688=CARTESIAN_POINT('',(54.75,-8.59971320199229,-1.31716849471866));
#80689=CARTESIAN_POINT('Ctrl Pts',(54.3836840636385,-9.02475418598685,-0.867119680571927));
#80690=CARTESIAN_POINT('Ctrl Pts',(54.4264645321808,-8.97871008136871,-0.899036246189249));
#80691=CARTESIAN_POINT('Ctrl Pts',(54.4672398095032,-8.93419789077059,-0.933716090015573));
#80692=CARTESIAN_POINT('Ctrl Pts',(54.5981025051697,-8.78865138282002,-1.06105533666644));
#80693=CARTESIAN_POINT('Ctrl Pts',(54.687196533521,-8.68447108302277,-1.17861119484756));
#80694=CARTESIAN_POINT('Ctrl Pts',(54.75,-8.59971320199229,-1.31716849471866));
#80695=CARTESIAN_POINT('Origin',(54.75,0.,0.));
#80696=CARTESIAN_POINT('Origin',(41.725,-9.26174317082254,-0.511160476960432));
#80697=CARTESIAN_POINT('',(30.5,-9.0247541859967,-0.867119680565103));
#80698=CARTESIAN_POINT('',(30.5,-8.99012941036642,-0.919126349007532));
#80699=CARTESIAN_POINT('',(41.725,-9.0247541859967,-0.867119680565103));
#80700=CARTESIAN_POINT('Origin',(30.5,-9.87929076741144,-2.09990807725937));
#80701=CARTESIAN_POINT('',(30.5,-8.59721254097635,-2.87854497678382));
#80702=CARTESIAN_POINT('Origin',(30.5,-9.87929076741144,-2.09990807725937));
#80703=CARTESIAN_POINT('',(54.3836840636427,-8.5972125409718,-2.87854497677634));
#80704=CARTESIAN_POINT('',(41.725,-8.59721254097635,-2.87854497678382));
#80705=CARTESIAN_POINT('',(54.75,-8.39196962461624,-2.29452518389281));
#80706=CARTESIAN_POINT('Ctrl Pts',(54.75,-8.39196962461624,-2.29452518389281));
#80707=CARTESIAN_POINT('Ctrl Pts',(54.687196533521,-8.41304347080783,-2.45557771181783));
#80708=CARTESIAN_POINT('Ctrl Pts',(54.5981025051697,-8.46040263533297,-2.60534427749264));
#80709=CARTESIAN_POINT('Ctrl Pts',(54.4672398095032,-8.54157244883238,-2.78087356590538));
#80710=CARTESIAN_POINT('Ctrl Pts',(54.4264645321808,-8.5681307951027,-2.83065991868451));
#80711=CARTESIAN_POINT('Ctrl Pts',(54.3836840636385,-8.59721254097013,-2.87854497677358));
#80712=CARTESIAN_POINT('Origin',(54.75,-9.87929076741144,-2.09990807725937));
#80713=CARTESIAN_POINT('Origin',(41.725,-8.66893110002923,-3.30012199447695));
#80714=CARTESIAN_POINT('Ctrl Pts',(53.95,-8.74064965908211,-3.72169901217008));
#80715=CARTESIAN_POINT('Ctrl Pts',(54.1865412262364,-8.66725585135304,-3.29027452474592));
#80716=CARTESIAN_POINT('Ctrl Pts',(54.3836840636427,-8.5972125409718,-2.87854497677634));
#80717=CARTESIAN_POINT('',(30.5,-8.58673425221724,-2.816951356054));
#80718=CARTESIAN_POINT('Origin',(54.35,0.,0.));
#80719=CARTESIAN_POINT('',(54.3836840636427,-7.89183384493173,-4.46285146761096));
#80720=CARTESIAN_POINT('Ctrl Pts',(54.3836840636427,-7.89183384493173,-4.46285146761096));
#80721=CARTESIAN_POINT('Ctrl Pts',(54.1865412262364,-8.2446766507482,-4.23940294919137));
#80722=CARTESIAN_POINT('Ctrl Pts',(53.95,-8.61439756923049,-4.00526584875909));
#80723=CARTESIAN_POINT('',(54.75,-7.32048824080209,-4.70111177449316));
#80724=CARTESIAN_POINT('Ctrl Pts',(54.3836840636385,-7.89183384492855,-4.46285146761156));
#80725=CARTESIAN_POINT('Ctrl Pts',(54.4264645321808,-7.83678882554573,-4.473280876609));
#80726=CARTESIAN_POINT('Ctrl Pts',(54.4672398095032,-7.78201935275478,-4.48685775142846));
#80727=CARTESIAN_POINT('Ctrl Pts',(54.5981025051697,-7.59726246382623,-4.54398884373077));
#80728=CARTESIAN_POINT('Ctrl Pts',(54.687196533521,-7.45427474904011,-4.60900751857725));
#80729=CARTESIAN_POINT('Ctrl Pts',(54.75,-7.32048824080209,-4.70111177449316));
#80730=CARTESIAN_POINT('Origin',(54.75,0.,0.));
#80731=CARTESIAN_POINT('Origin',(41.725,-8.25311570708541,-4.23405865818421));
#80732=CARTESIAN_POINT('',(30.5,-7.89183384494032,-4.46285146760933));
#80733=CARTESIAN_POINT('',(30.5,-7.83904952070155,-4.49627875832492));
#80734=CARTESIAN_POINT('',(41.725,-7.89183384494032,-4.46285146760933));
#80735=CARTESIAN_POINT('Origin',(30.5,-8.17107164318697,-5.93663104815398));
#80736=CARTESIAN_POINT('',(30.5,-6.68313474439719,-6.12648305688667));
#80737=CARTESIAN_POINT('Origin',(30.5,-8.17107164318697,-5.93663104815398));
#80738=CARTESIAN_POINT('',(54.3836840636427,-6.68313474439608,-6.12648305687799));
#80739=CARTESIAN_POINT('',(41.725,-6.68313474439719,-6.12648305688667));
#80740=CARTESIAN_POINT('',(54.75,-6.73317826049341,-5.50947461310232));
#80741=CARTESIAN_POINT('Ctrl Pts',(54.75,-6.7331782604934,-5.50947461310232));
#80742=CARTESIAN_POINT('Ctrl Pts',(54.687196533521,-6.68692421238969,-5.66517492388675));
#80743=CARTESIAN_POINT('Ctrl Pts',(54.5981025051697,-6.66927341185182,-5.82125619726353));
#80744=CARTESIAN_POINT('Ctrl Pts',(54.4672398095033,-6.67203153274142,-6.01462491883807));
#80745=CARTESIAN_POINT('Ctrl Pts',(54.4264645321808,-6.6760438553388,-6.07090926787966));
#80746=CARTESIAN_POINT('Ctrl Pts',(54.3836840636385,-6.68313474439567,-6.12648305687479));
#80747=CARTESIAN_POINT('Origin',(54.75,-8.17107164318697,-5.93663104815398));
#80748=CARTESIAN_POINT('Origin',(41.725,-6.57718208727421,-6.54078339240215));
#80749=CARTESIAN_POINT('Ctrl Pts',(53.95,-6.47122943015123,-6.95508372791763));
#80750=CARTESIAN_POINT('Ctrl Pts',(54.1865412262364,-6.57965699823685,-6.53110589613718));
#80751=CARTESIAN_POINT('Ctrl Pts',(54.3836840636427,-6.68313474439608,-6.12648305687799));
#80752=CARTESIAN_POINT('',(30.5,-6.69861473382797,-6.06595258045412));
#80753=CARTESIAN_POINT('Origin',(54.35,0.,0.));
#80754=CARTESIAN_POINT('',(54.3836840636427,-5.39434373702554,-7.28691569216912));
#80755=CARTESIAN_POINT('Ctrl Pts',(54.3836840636427,-5.39434373702554,-7.28691569216912));
#80756=CARTESIAN_POINT('Ctrl Pts',(54.1865412262364,-5.80756637982325,-7.22629941152119));
#80757=CARTESIAN_POINT('Ctrl Pts',(53.95,-6.24055538374756,-7.16278357221404));
#80758=CARTESIAN_POINT('',(54.75,-4.77548435822936,-7.27219012019809));
#80759=CARTESIAN_POINT('Ctrl Pts',(54.3836840636385,-5.39434373702239,-7.28691569216838));
#80760=CARTESIAN_POINT('Ctrl Pts',(54.4264645321808,-5.33981558679448,-7.27405460498207));
#80761=CARTESIAN_POINT('Ctrl Pts',(54.4672398095033,-5.2842589712213,-7.26418094579635));
#80762=CARTESIAN_POINT('Ctrl Pts',(54.5981025051697,-5.09223784587415,-7.24122539887136));
#80763=CARTESIAN_POINT('Ctrl Pts',(54.687196533521,-4.93516659098831,-7.24246457082612));
#80764=CARTESIAN_POINT('Ctrl Pts',(54.75,-4.77548435822936,-7.27219012019808));
#80765=CARTESIAN_POINT('Origin',(54.75,0.,0.));
#80766=CARTESIAN_POINT('Origin',(41.725,-5.81744956039081,-7.22484963219258));
#80767=CARTESIAN_POINT('',(30.5,-5.39434373703405,-7.28691569217113));
#80768=CARTESIAN_POINT('',(30.5,-5.33252675337821,-7.29598372291775));
#80769=CARTESIAN_POINT('',(41.725,-5.39434373703405,-7.28691569217113));
#80770=CARTESIAN_POINT('Origin',(30.5,-5.05,-8.74685657822283));
#80771=CARTESIAN_POINT('',(30.5,-3.61348223613864,-8.31509655910253));
#80772=CARTESIAN_POINT('Origin',(30.5,-5.05,-8.74685657822283));
#80773=CARTESIAN_POINT('',(54.3836840636427,-3.61348223614116,-8.31509655909415));
#80774=CARTESIAN_POINT('',(41.725,-3.61348223613864,-8.31509655910253));
#80775=CARTESIAN_POINT('',(54.75,-3.91015920612708,-7.77178582970089));
#80776=CARTESIAN_POINT('Ctrl Pts',(54.75,-3.91015920612708,-7.77178582970089));
#80777=CARTESIAN_POINT('Ctrl Pts',(54.687196533521,-3.80457500885004,-7.89521192511717));
#80778=CARTESIAN_POINT('Ctrl Pts',(54.5981025051697,-3.72496622701464,-8.03062003607523));
#80779=CARTESIAN_POINT('Ctrl Pts',(54.4672398095032,-3.64883575113587,-8.20839298215164));
#80780=CARTESIAN_POINT('Ctrl Pts',(54.4264645321808,-3.62960828303242,-8.26144325217916));
#80781=CARTESIAN_POINT('Ctrl Pts',(54.3836840636385,-3.61348223614209,-8.31509655909106));
#80782=CARTESIAN_POINT('Origin',(54.75,-5.05,-8.74685657822283));
#80783=CARTESIAN_POINT('Origin',(41.725,-3.34817853980604,-8.65048392062934));
#80784=CARTESIAN_POINT('Ctrl Pts',(53.95,-3.08287484347344,-8.98587128215615));
#80785=CARTESIAN_POINT('Ctrl Pts',(54.1865412262364,-3.35437567581825,-8.64264972485195));
#80786=CARTESIAN_POINT('Ctrl Pts',(54.3836840636427,-3.61348223614116,-8.31509655909415));
#80787=CARTESIAN_POINT('',(30.5,-3.65224387295544,-8.26609549624456));
#80788=CARTESIAN_POINT('Origin',(54.35,0.,0.));
#80789=CARTESIAN_POINT('',(54.3836840636427,-1.96412259091325,-8.85100599400042));
#80790=CARTESIAN_POINT('Ctrl Pts',(54.3836840636427,-1.96412259091325,-8.85100599400042));
#80791=CARTESIAN_POINT('Ctrl Pts',(54.1865412262364,-2.36627512174265,-8.96370305672976));
#80792=CARTESIAN_POINT('Ctrl Pts',(53.95,-2.78766447874883,-9.08179094418728));
#80793=CARTESIAN_POINT('',(54.75,-1.40475584620536,-8.58584072834757));
#80794=CARTESIAN_POINT('Ctrl Pts',(54.3836840636385,-1.96412259091069,-8.85100599399847));
#80795=CARTESIAN_POINT('Ctrl Pts',(54.4264645321807,-1.91953972238479,-8.81707820944224));
#80796=CARTESIAN_POINT('Ctrl Pts',(54.4672398095032,-1.87280220757798,-8.78546126162393));
#80797=CARTESIAN_POINT('Ctrl Pts',(54.5981025051697,-1.70671904284191,-8.68638829807956));
#80798=CARTESIAN_POINT('Ctrl Pts',(54.687196533521,-1.56272329477366,-8.6236337030541));
#80799=CARTESIAN_POINT('Ctrl Pts',(54.75,-1.40475584620536,-8.58584072834756));
#80800=CARTESIAN_POINT('Origin',(54.75,0.,0.));
#80801=CARTESIAN_POINT('Origin',(41.725,-2.37589353483453,-8.9663984690965));
#80802=CARTESIAN_POINT('',(30.5,-1.96412259092022,-8.85100599400572));
#80803=CARTESIAN_POINT('',(30.5,-1.90396166591106,-8.83414681988681));
#80804=CARTESIAN_POINT('',(41.725,-1.96412259092022,-8.85100599400572));
#80805=CARTESIAN_POINT('Origin',(30.5,-1.05573747900331,-10.0446711432196));
#80806=CARTESIAN_POINT('',(30.5,0.0809741782038119,-9.06595432596881));
#80807=CARTESIAN_POINT('Origin',(30.5,-1.05573747900331,-10.0446711432196));
#80808=CARTESIAN_POINT('',(54.3836840636427,0.0809741781981025,-9.06595432596218));
#80809=CARTESIAN_POINT('',(41.725,0.0809741782038119,-9.06595432596881));
#80810=CARTESIAN_POINT('',(54.75,-0.411038102340181,-8.69028467188645));
#80811=CARTESIAN_POINT('Ctrl Pts',(54.75,-0.411038102340177,-8.69028467188645));
#80812=CARTESIAN_POINT('Ctrl Pts',(54.687196533521,-0.264380222801327,-8.76009505874624));
#80813=CARTESIAN_POINT('Ctrl Pts',(54.5981025051697,-0.136578541270819,
-8.85141671475685));
#80814=CARTESIAN_POINT('Ctrl Pts',(54.4672398095032,0.00527688047320916,
-8.98285532794201));
#80815=CARTESIAN_POINT('Ctrl Pts',(54.4264645321808,0.0444195353663464,
-9.02349864532112));
#80816=CARTESIAN_POINT('Ctrl Pts',(54.3836840636385,0.0809741781959984,
-9.06595432595973));
#80817=CARTESIAN_POINT('Origin',(54.75,-1.05573747900331,-10.0446711432196));
#80818=CARTESIAN_POINT('Origin',(41.725,0.459755494441719,-9.26443719180044));
#80819=CARTESIAN_POINT('Ctrl Pts',(53.95,0.838536810679625,-9.46292005763206));
#80820=CARTESIAN_POINT('Ctrl Pts',(54.1865412262364,0.450907674495762,-9.25980090013205));
#80821=CARTESIAN_POINT('Ctrl Pts',(54.3836840636427,0.0809741781981025,
-9.06595432596218));
#80822=CARTESIAN_POINT('',(30.5,0.025633133145034,-9.03695540561423));
#80823=CARTESIAN_POINT('Origin',(54.35,0.,0.));
#80824=CARTESIAN_POINT('',(54.3836840636427,1.8057131946615,-8.88467695060392));
#80825=CARTESIAN_POINT('Ctrl Pts',(54.3836840636427,1.8057131946615,-8.88467695060392));
#80826=CARTESIAN_POINT('Ctrl Pts',(54.1865412262364,1.48416660182181,-9.15120101074401));
#80827=CARTESIAN_POINT('Ctrl Pts',(53.95,1.14723893976231,-9.43047415642994));
#80828=CARTESIAN_POINT('',(54.75,2.20886771343379,-8.41492147465143));
#80829=CARTESIAN_POINT('Ctrl Pts',(54.3836840636385,1.80571319466305,-8.88467695060108));
#80830=CARTESIAN_POINT('Ctrl Pts',(54.4264645321808,1.83264199849617,-8.83554889084895));
#80831=CARTESIAN_POINT('Ctrl Pts',(54.4672398095032,1.8624790716295,-8.78765551190679));
#80832=CARTESIAN_POINT('Ctrl Pts',(54.5981025051697,1.97390698775344,-8.62959574718948));
#80833=CARTESIAN_POINT('Ctrl Pts',(54.687196533521,2.07992905600281,-8.5136982247713));
#80834=CARTESIAN_POINT('Ctrl Pts',(54.75,2.20886771343378,-8.41492147465143));
#80835=CARTESIAN_POINT('Origin',(54.75,0.,0.));
#80836=CARTESIAN_POINT('Origin',(41.725,1.4764760672098,-9.15757555352076));
#80837=CARTESIAN_POINT('',(30.5,1.8057131946573,-8.88467695061159));
#80838=CARTESIAN_POINT('',(30.5,1.85381569054083,-8.8448056759931));
#80839=CARTESIAN_POINT('',(41.725,1.8057131946573,-8.88467695061159));
#80840=CARTESIAN_POINT('Origin',(30.5,3.12107164318697,-9.60567081458105));
#80841=CARTESIAN_POINT('',(30.5,3.76142942150752,-8.24922622826565));
#80842=CARTESIAN_POINT('Origin',(30.5,3.12107164318697,-9.60567081458105));
#80843=CARTESIAN_POINT('',(54.3836840636427,3.76142942149961,-8.24922622826191));
#80844=CARTESIAN_POINT('',(41.725,3.76142942150752,-8.24922622826565));
#80845=CARTESIAN_POINT('',(54.75,3.15915522350527,-8.10615434554508));
#80846=CARTESIAN_POINT('Ctrl Pts',(54.75,3.15915522350528,-8.10615434554507));
#80847=CARTESIAN_POINT('Ctrl Pts',(54.687196533521,3.32152830558867,-8.11027817375286));
#80848=CARTESIAN_POINT('Ctrl Pts',(54.5981025051697,3.47542481503583,-8.1417230308606));
#80849=CARTESIAN_POINT('Ctrl Pts',(54.4672398095032,3.65847709150953,-8.20410038085247));
#80850=CARTESIAN_POINT('Ctrl Pts',(54.4264645321807,3.71076681256147,-8.22530914677538));
#80851=CARTESIAN_POINT('Ctrl Pts',(54.3836840636385,3.76142942149669,-8.24922622826054));
#80852=CARTESIAN_POINT('Origin',(54.75,3.12107164318697,-9.60567081458105));
#80853=CARTESIAN_POINT('Origin',(41.725,4.18819362695297,-8.27648510773958));
#80854=CARTESIAN_POINT('Ctrl Pts',(53.95,4.61495783239841,-8.30374398721351));
#80855=CARTESIAN_POINT('Ctrl Pts',(54.1865412262364,4.17822499152176,-8.27584837712898));
#80856=CARTESIAN_POINT('Ctrl Pts',(54.3836840636427,3.76142942149961,-8.24922622826191));
#80857=CARTESIAN_POINT('',(30.5,3.69907793765504,-8.2452436271907));
#80858=CARTESIAN_POINT('Origin',(54.35,0.,0.));
#80859=CARTESIAN_POINT('',(54.3836840636427,5.2633247644899,-7.38210654769183));
#80860=CARTESIAN_POINT('Ctrl Pts',(54.3836840636427,5.2633247644899,-7.38210654769183));
#80861=CARTESIAN_POINT('Ctrl Pts',(54.1865412262364,5.07798243670109,-7.75637317394928));
#80862=CARTESIAN_POINT('Ctrl Pts',(53.95,4.88377432324997,-8.14854271385775));
#80863=CARTESIAN_POINT('',(54.75,5.44055797848702,-6.78898585082642));
#80864=CARTESIAN_POINT('Ctrl Pts',(54.3836840636385,5.26332476449016,-7.38210654768861));
#80865=CARTESIAN_POINT('Ctrl Pts',(54.4264645321808,5.26794326880724,-7.32627290058613));
#80866=CARTESIAN_POINT('Ctrl Pts',(54.4672398095032,5.27572079926106,-7.2703842908369));
#80867=CARTESIAN_POINT('Ctrl Pts',(54.5981025051697,5.31322656778419,-7.08066769419416));
#80868=CARTESIAN_POINT('Ctrl Pts',(54.687196533521,5.3629427774341,-6.9316669789053));
#80869=CARTESIAN_POINT('Ctrl Pts',(54.75,5.44055797848701,-6.78898585082642));
#80870=CARTESIAN_POINT('Origin',(54.75,0.,0.));
#80871=CARTESIAN_POINT('Origin',(41.725,5.07354954386957,-7.76532463077915));
#80872=CARTESIAN_POINT('',(30.5,5.26332476448917,-7.38210654770055));
#80873=CARTESIAN_POINT('',(30.5,5.29105147271138,-7.32611727818317));
#80874=CARTESIAN_POINT('',(41.725,5.26332476448918,-7.38210654770055));
#80875=CARTESIAN_POINT('Origin',(30.5,6.75821912422446,-7.50576273732169));
#80876=CARTESIAN_POINT('',(30.5,6.79149934631904,-6.00613197382777));
#80877=CARTESIAN_POINT('Origin',(30.5,6.75821912422446,-7.50576273732169));
#80878=CARTESIAN_POINT('',(54.3836840636427,6.7914993463103,-6.00613197382758));
#80879=CARTESIAN_POINT('',(41.725,6.79149934631904,-6.00613197382777));
#80880=CARTESIAN_POINT('',(54.75,6.18310191118245,-6.12039629075862));
#80881=CARTESIAN_POINT('Ctrl Pts',(54.75,6.18310191118245,-6.12039629075862));
#80882=CARTESIAN_POINT('Ctrl Pts',(54.687196533521,6.33311441480502,-6.05812051295347));
#80883=CARTESIAN_POINT('Ctrl Pts',(54.5981025051697,6.48649564757952,-6.02425146969684));
#80884=CARTESIAN_POINT('Ctrl Pts',(54.4672398095032,6.67909337720287,-6.00678194600141));
#80885=CARTESIAN_POINT('Ctrl Pts',(54.4264645321807,6.73548879660653,-6.00488897216445));
#80886=CARTESIAN_POINT('Ctrl Pts',(54.3836840636385,6.79149934630707,-6.00613197382751));
#80887=CARTESIAN_POINT('Origin',(54.75,6.75821912422446,-7.50576273732169));
#80888=CARTESIAN_POINT('Origin',(41.725,7.19245503281942,-5.85745355904382));
#80889=CARTESIAN_POINT('Ctrl Pts',(53.95,7.5934107193198,-5.70877514425986));
#80890=CARTESIAN_POINT('Ctrl Pts',(54.1865412262364,7.18308924953126,-5.86092648599809));
#80891=CARTESIAN_POINT('Ctrl Pts',(54.3836840636427,6.7914993463103,-6.00613197382758));
#80892=CARTESIAN_POINT('',(30.5,6.7329185616764,-6.02785431993911));
#80893=CARTESIAN_POINT('Origin',(54.35,0.,0.));
#80894=CARTESIAN_POINT('',(54.3836840636427,7.81085966673361,-4.60310285835123));
#80895=CARTESIAN_POINT('Ctrl Pts',(54.3836840636427,7.81085966673361,-4.60310285835123));
#80896=CARTESIAN_POINT('Ctrl Pts',(54.1865412262364,7.7937689762525,-5.02039795094069));
#80897=CARTESIAN_POINT('Ctrl Pts',(53.95,7.77586075855085,-5.45765420887298));
#80898=CARTESIAN_POINT('',(54.75,7.73152634314226,-3.98917289739329));
#80899=CARTESIAN_POINT('Ctrl Pts',(54.3836840636385,7.81085966673255,-4.60310285834819));
#80900=CARTESIAN_POINT('Ctrl Pts',(54.4264645321807,7.79236929017938,-4.55021776871213));
#80901=CARTESIAN_POINT('Ctrl Pts',(54.4672398095032,7.77674247228156,-4.49599757651355));
#80902=CARTESIAN_POINT('Ctrl Pts',(54.5981025051697,7.73384100509704,-4.30742787102609));
#80903=CARTESIAN_POINT('Ctrl Pts',(54.687196533521,7.71865497184143,-4.15108754016899));
#80904=CARTESIAN_POINT('Ctrl Pts',(54.75,7.73152634314226,-3.98917289739329));
#80905=CARTESIAN_POINT('Origin',(54.75,0.,0.));
#80906=CARTESIAN_POINT('Origin',(41.725,7.79336021264368,-5.03037853361623));
#80907=CARTESIAN_POINT('',(30.5,7.8108596667365,-4.60310285835949));
#80908=CARTESIAN_POINT('',(30.5,7.81341638755651,-4.54067664728932));
#80909=CARTESIAN_POINT('',(41.725,7.8108596667365,-4.60310285835949));
#80910=CARTESIAN_POINT('Origin',(30.5,9.22680912219027,-4.10804009506559));
#80911=CARTESIAN_POINT('',(30.5,8.64725733531739,-2.72452293711905));
#80912=CARTESIAN_POINT('Origin',(30.5,9.22680912219027,-4.10804009506559));
#80913=CARTESIAN_POINT('',(54.3836840636427,8.64725733530932,-2.72452293712243));
#80914=CARTESIAN_POINT('',(41.725,8.64725733531739,-2.72452293711905));
#80915=CARTESIAN_POINT('',(54.75,8.13793410669875,-3.07636611524525));
#80916=CARTESIAN_POINT('Ctrl Pts',(54.75,8.13793410669875,-3.07636611524524));
#80917=CARTESIAN_POINT('Ctrl Pts',(54.687196533521,8.24964750716333,-2.95845877916736));
#80918=CARTESIAN_POINT('Ctrl Pts',(54.5981025051697,8.37599245469372,-2.86513210081603));
#80919=CARTESIAN_POINT('Ctrl Pts',(54.4672398095032,8.54483374031939,-2.77083634278586));
#80920=CARTESIAN_POINT('Ctrl Pts',(54.4264645321807,8.59558357772358,-2.74616894156258));
#80921=CARTESIAN_POINT('Ctrl Pts',(54.3836840636385,8.64725733530634,-2.72452293712368));
#80922=CARTESIAN_POINT('Origin',(54.75,9.22680912219027,-4.10804009506559));
#80923=CARTESIAN_POINT('Origin',(41.725,8.95307562210873,-2.42561507669435));
#80924=CARTESIAN_POINT('Ctrl Pts',(53.95,9.25889390890006,-2.12670721626965));
#80925=CARTESIAN_POINT('Ctrl Pts',(54.1865412262364,8.94593211997956,-2.43259716059258));
#80926=CARTESIAN_POINT('Ctrl Pts',(54.3836840636427,8.64725733530932,-2.72452293712243));
#80927=CARTESIAN_POINT('',(30.5,8.60257639973902,-2.7681942394327));
#80928=CARTESIAN_POINT('Origin',(54.5,-0.5,-1.73205080756888));
#80929=CARTESIAN_POINT('',(54.75,-2.,-1.15470053837925));
#80930=CARTESIAN_POINT('',(54.75,-5.55111512312578E-16,-2.3094010767585));
#80931=CARTESIAN_POINT('',(54.75,-0.625,-1.94855715851499));
#80932=CARTESIAN_POINT('',(54.25,-3.18172571617472E-16,-1.73205080756888));
#80933=CARTESIAN_POINT('',(54.75,-5.55111512312578E-16,-2.3094010767585));
#80934=CARTESIAN_POINT('',(54.25,-1.5,-0.866025403784439));
#80935=CARTESIAN_POINT('',(54.25,-0.375,-1.51554445662277));
#80936=CARTESIAN_POINT('',(54.75,-2.,-1.15470053837925));
#80937=CARTESIAN_POINT('Origin',(54.5,1.25,-1.29903810567666));
#80938=CARTESIAN_POINT('',(54.75,2.,-1.15470053837925));
#80939=CARTESIAN_POINT('',(54.75,1.375,-1.51554445662277));
#80940=CARTESIAN_POINT('',(54.25,1.5,-0.866025403784439));
#80941=CARTESIAN_POINT('',(54.75,2.,-1.15470053837925));
#80942=CARTESIAN_POINT('',(54.25,1.125,-1.08253175473055));
#80943=CARTESIAN_POINT('Origin',(54.5,0.5,1.73205080756888));
#80944=CARTESIAN_POINT('',(54.75,2.,1.15470053837925));
#80945=CARTESIAN_POINT('',(54.75,2.77555756156289E-16,2.3094010767585));
#80946=CARTESIAN_POINT('',(54.75,0.625,1.94855715851499));
#80947=CARTESIAN_POINT('',(54.25,1.06057523872491E-16,1.73205080756888));
#80948=CARTESIAN_POINT('',(54.75,0.,2.3094010767585));
#80949=CARTESIAN_POINT('',(54.25,1.5,0.866025403784439));
#80950=CARTESIAN_POINT('',(54.25,0.375,1.51554445662277));
#80951=CARTESIAN_POINT('',(54.25,1.5,0.866025403784439));
#80952=CARTESIAN_POINT('Origin',(54.5,-1.25,1.29903810567666));
#80953=CARTESIAN_POINT('',(54.25,-1.5,0.866025403784439));
#80954=CARTESIAN_POINT('',(54.25,-1.125,1.08253175473055));
#80955=CARTESIAN_POINT('',(54.75,-2.,1.15470053837925));
#80956=CARTESIAN_POINT('',(54.75,-1.375,1.51554445662277));
#80957=CARTESIAN_POINT('',(54.75,-2.,1.15470053837925));
#80958=CARTESIAN_POINT('Origin',(54.5,1.75,0.433012701892219));
#80959=CARTESIAN_POINT('',(54.75,2.,0.433012701892219));
#80960=CARTESIAN_POINT('',(54.25,1.5,0.433012701892219));
#80961=CARTESIAN_POINT('Origin',(54.5,-1.75,-0.43301270189222));
#80962=CARTESIAN_POINT('',(54.25,-1.5,-0.43301270189222));
#80963=CARTESIAN_POINT('',(54.75,-2.,-0.43301270189222));
#80964=CARTESIAN_POINT('Origin',(54.75,1.5,-0.866025403784439));
#80965=CARTESIAN_POINT('',(50.75,1.5,-0.866025403784439));
#80966=CARTESIAN_POINT('',(54.75,1.5,-0.866025403784439));
#80967=CARTESIAN_POINT('',(50.75,-2.77555756156289E-16,-1.73205080756888));
#80968=CARTESIAN_POINT('',(50.75,-3.18172571617472E-16,-1.73205080756888));
#80969=CARTESIAN_POINT('',(54.75,-3.18172571617472E-16,-1.73205080756888));
#80970=CARTESIAN_POINT('Origin',(54.75,1.5,0.866025403784439));
#80971=CARTESIAN_POINT('',(50.75,1.5,0.866025403784439));
#80972=CARTESIAN_POINT('',(54.75,1.5,0.866025403784439));
#80973=CARTESIAN_POINT('',(50.75,1.5,-0.866025403784439));
#80974=CARTESIAN_POINT('Origin',(54.75,0.,1.73205080756888));
#80975=CARTESIAN_POINT('',(50.75,0.,1.73205080756888));
#80976=CARTESIAN_POINT('',(54.75,1.06057523872491E-16,1.73205080756888));
#80977=CARTESIAN_POINT('',(50.75,1.5,0.866025403784439));
#80978=CARTESIAN_POINT('Origin',(54.75,0.,0.));
#80979=CARTESIAN_POINT('Origin',(54.75,0.,0.));
#80980=CARTESIAN_POINT('Origin',(54.75,-1.5,0.866025403784439));
#80981=CARTESIAN_POINT('',(50.75,-1.5,0.866025403784439));
#80982=CARTESIAN_POINT('',(54.75,-1.5,0.866025403784439));
#80983=CARTESIAN_POINT('',(50.75,1.06057523872491E-16,1.73205080756888));
#80984=CARTESIAN_POINT('Origin',(54.75,-1.5,-0.866025403784439));
#80985=CARTESIAN_POINT('',(50.75,-1.5,-0.866025403784439));
#80986=CARTESIAN_POINT('',(54.75,-1.5,-0.866025403784439));
#80987=CARTESIAN_POINT('',(50.75,-1.5,0.866025403784439));
#80988=CARTESIAN_POINT('Origin',(54.75,-2.77555756156289E-16,-1.73205080756888));
#80989=CARTESIAN_POINT('',(50.75,-1.5,-0.866025403784439));
#80990=CARTESIAN_POINT('Origin',(50.75,0.,0.));
#80991=CARTESIAN_POINT('Origin',(30.5,9.22680912219027,-4.10804009506559));
#80992=CARTESIAN_POINT('Origin',(30.5,6.75821912422446,-7.50576273732169));
#80993=CARTESIAN_POINT('Origin',(30.5,3.12107164318697,-9.60567081458105));
#80994=CARTESIAN_POINT('Origin',(30.5,-1.05573747900331,-10.0446711432196));
#80995=CARTESIAN_POINT('Origin',(30.5,-5.05,-8.74685657822283));
#80996=CARTESIAN_POINT('Origin',(30.5,-8.17107164318697,-5.93663104815398));
#80997=CARTESIAN_POINT('Origin',(30.5,-9.87929076741144,-2.09990807725937));
#80998=CARTESIAN_POINT('Origin',(30.5,-9.87929076741144,2.09990807725937));
#80999=CARTESIAN_POINT('Origin',(30.5,-8.17107164318697,5.93663104815398));
#81000=CARTESIAN_POINT('Origin',(30.5,-5.05,8.74685657822283));
#81001=CARTESIAN_POINT('Origin',(30.5,-1.0557374790033,10.0446711432196));
#81002=CARTESIAN_POINT('Origin',(30.5,3.12107164318697,9.60567081458105));
#81003=CARTESIAN_POINT('Origin',(30.5,6.75821912422447,7.50576273732168));
#81004=CARTESIAN_POINT('Origin',(30.5,9.22680912219027,4.10804009506558));
#81005=CARTESIAN_POINT('Origin',(30.5,10.1,0.));
#81006=CARTESIAN_POINT('Origin',(54.35,0.,0.));
#81007=CARTESIAN_POINT('Origin',(27.2,0.,0.));
#81008=CARTESIAN_POINT('',(27.4,-8.,-9.79717439317883E-16));
#81009=CARTESIAN_POINT('Origin',(27.4,0.,0.));
#81010=CARTESIAN_POINT('',(27.2,-7.8,-9.55224503334935E-16));
#81011=CARTESIAN_POINT('Origin',(28.2,0.,0.));
#81012=CARTESIAN_POINT('',(29.,-8.,-9.79717439317883E-16));
#81013=CARTESIAN_POINT('Origin',(29.,0.,0.));
#81014=CARTESIAN_POINT('',(28.2,-8.,-9.79717439317883E-16));
#81015=CARTESIAN_POINT('Origin',(29.,9.,0.));
#81016=CARTESIAN_POINT('',(29.,-9.,-1.10218211923262E-15));
#81017=CARTESIAN_POINT('Origin',(29.,0.,0.));
#81018=CARTESIAN_POINT('Origin',(29.25,0.,0.));
#81019=CARTESIAN_POINT('',(29.25,-9.25,-1.1327982892113E-15));
#81020=CARTESIAN_POINT('Origin',(49.,5.05,0.));
#81021=CARTESIAN_POINT('',(0.,0.,0.));
#81022=CARTESIAN_POINT('Origin',(2.075,0.,0.));
#81023=CARTESIAN_POINT('',(0.574155045842906,-1.46519261812194,0.000976835818179873));
#81024=CARTESIAN_POINT('',(0.502844954157094,-1.46475946759348,0.00161057725761545));
#81025=CARTESIAN_POINT('',(2.075,-1.4635,-1.79227059055215E-16));
#81026=CARTESIAN_POINT('',(0.4135,0.634777254283071,1.31995703642142));
#81027=CARTESIAN_POINT('Ctrl Pts',(0.574155045842906,-1.46519261812194,
0.000976835818179873));
#81028=CARTESIAN_POINT('Ctrl Pts',(0.57130704891923,-1.46556281925314,0.0531772786997573));
#81029=CARTESIAN_POINT('Ctrl Pts',(0.568459051995553,-1.46301484057674,
0.105338898321017));
#81030=CARTESIAN_POINT('Ctrl Pts',(0.565611055071877,-1.45742890091883,
0.157170235506765));
#81031=CARTESIAN_POINT('Ctrl Pts',(0.539186980530809,-1.4056018484823,0.638067916952109));
#81032=CARTESIAN_POINT('Ctrl Pts',(0.512762905989741,-1.09225610638139,
1.09053368953482));
#81033=CARTESIAN_POINT('Ctrl Pts',(0.486338831448674,-0.660330380719405,
1.30858720339481));
#81034=CARTESIAN_POINT('Ctrl Pts',(0.462059220965782,-0.263457886270657,
1.50894443341694));
#81035=CARTESIAN_POINT('Ctrl Pts',(0.437779610482891,0.233528707448358,
1.51139328602859));
#81036=CARTESIAN_POINT('Ctrl Pts',(0.4135,0.63554741399093,1.32087379520599));
#81037=CARTESIAN_POINT('',(0.4135,-0.634007094575215,1.31904027763685));
#81038=CARTESIAN_POINT('Origin',(0.4135,0.,0.));
#81039=CARTESIAN_POINT('Ctrl Pts',(0.4135,-0.634007094575211,1.31904027763685));
#81040=CARTESIAN_POINT('Ctrl Pts',(0.439924074541068,-1.07200063648892,
1.10851523328497));
#81041=CARTESIAN_POINT('Ctrl Pts',(0.466348149082135,-1.393162466651,0.66456818150847));
#81042=CARTESIAN_POINT('Ctrl Pts',(0.492772223623203,-1.4539947208087,0.185460774447188));
#81043=CARTESIAN_POINT('Ctrl Pts',(0.496129800467833,-1.46172437535721,
0.124582958895325));
#81044=CARTESIAN_POINT('Ctrl Pts',(0.499487377312464,-1.4652508704938,0.0631374607139664));
#81045=CARTESIAN_POINT('Ctrl Pts',(0.502844954157094,-1.46475946759348,
0.00161057725761545));
#81046=CARTESIAN_POINT('Origin',(2.075,0.,0.));
#81047=CARTESIAN_POINT('',(1.07415504584291,-1.46139381528846,0.000649084939641151));
#81048=CARTESIAN_POINT('',(1.00284495415709,-1.46127859184819,0.000519472235833149));
#81049=CARTESIAN_POINT('',(2.075,-1.4635,-1.79227059055215E-16));
#81050=CARTESIAN_POINT('Ctrl Pts',(1.07415504584291,-1.46139381528846,0.000649084939641151));
#81051=CARTESIAN_POINT('Ctrl Pts',(1.06318482949897,-1.46220383399087,0.203077133365655));
#81052=CARTESIAN_POINT('Ctrl Pts',(1.05221461315503,-1.4230119511318,0.405204867450792));
#81053=CARTESIAN_POINT('Ctrl Pts',(1.0412443968111,-1.34229994073582,0.589109347613649));
#81054=CARTESIAN_POINT('Ctrl Pts',(1.01482032227003,-1.14788807936524,1.03208198734153));
#81055=CARTESIAN_POINT('Ctrl Pts',(0.988396247728961,-0.71258117373777,
1.36932538632444));
#81056=CARTESIAN_POINT('Ctrl Pts',(0.961972173187893,-0.235083460125689,
1.44690837412835));
#81057=CARTESIAN_POINT('Ctrl Pts',(0.935548098646825,0.242414253486394,
1.52449136193227));
#81058=CARTESIAN_POINT('Ctrl Pts',(0.909124024105757,0.762102775083091,
1.34241393855718));
#81059=CARTESIAN_POINT('Ctrl Pts',(0.882699949564689,1.08675402559799,0.983767539938644));
#81060=CARTESIAN_POINT('Ctrl Pts',(0.856275875023622,1.4114052761129,0.625121141320107));
#81061=CARTESIAN_POINT('Ctrl Pts',(0.829851800482554,1.54101925554601,0.0899057674581173));
#81062=CARTESIAN_POINT('Ctrl Pts',(0.803427725941486,1.41643784418256,-0.377524557756998));
#81063=CARTESIAN_POINT('Ctrl Pts',(0.777003651400418,1.29185643281911,-0.844954882972116));
#81064=CARTESIAN_POINT('Ctrl Pts',(0.750579576859351,0.913079630659097,
-1.24460015954036));
#81065=CARTESIAN_POINT('Ctrl Pts',(0.724155502318283,0.452995311679302,
-1.39411299623214));
#81066=CARTESIAN_POINT('Ctrl Pts',(0.697731427777215,-0.00708900730049256,
-1.54362583292391));
#81067=CARTESIAN_POINT('Ctrl Pts',(0.671307353236147,-0.548480843100068,
-1.44300622973923));
#81068=CARTESIAN_POINT('Ctrl Pts',(0.64488327869508,-0.924022579613784,
-1.13803163299289));
#81069=CARTESIAN_POINT('Ctrl Pts',(0.621307201077688,-1.25908828323405,
-0.865927315657216));
#81070=CARTESIAN_POINT('Ctrl Pts',(0.597731123460297,-1.46212804648194,
-0.431145011929348));
#81071=CARTESIAN_POINT('Ctrl Pts',(0.574155045842906,-1.46519261812194,
0.000976835818179873));
#81072=CARTESIAN_POINT('Ctrl Pts',(0.502844954157094,-1.46475946759348,
0.00161057725761545));
#81073=CARTESIAN_POINT('Ctrl Pts',(0.525911451853531,-1.46138353775099,
-0.421078100079624));
#81074=CARTESIAN_POINT('Ctrl Pts',(0.548977949549969,-1.2683761840885,-0.847607891709197));
#81075=CARTESIAN_POINT('Ctrl Pts',(0.572044447246407,-0.945806624145029,
-1.12030156148761));
#81076=CARTESIAN_POINT('Ctrl Pts',(0.598468521787474,-0.576283595170322,
-1.43268872801506));
#81077=CARTESIAN_POINT('Ctrl Pts',(0.624892596328542,-0.0367348590675789,
-1.5431952987239));
#81078=CARTESIAN_POINT('Ctrl Pts',(0.651316670869609,0.426181990272789,
-1.40242879098034));
#81079=CARTESIAN_POINT('Ctrl Pts',(0.677740745410677,0.889098839613157,
-1.26166228323678));
#81080=CARTESIAN_POINT('Ctrl Pts',(0.704164819951745,1.27538380219115,-0.869622697040829));
#81081=CARTESIAN_POINT('Ctrl Pts',(0.730588894492813,1.40889782546728,-0.404732685395172));
#81082=CARTESIAN_POINT('Ctrl Pts',(0.757012969033881,1.54241184874341,0.0601573262504863));
#81083=CARTESIAN_POINT('Ctrl Pts',(0.783437043574948,1.42315493271767,0.597897763345852));
#81084=CARTESIAN_POINT('Ctrl Pts',(0.809861118116016,1.1054653199822,0.962746225793369));
#81085=CARTESIAN_POINT('Ctrl Pts',(0.836285192657083,0.787775707246719,
1.32759468824088));
#81086=CARTESIAN_POINT('Ctrl Pts',(0.862709267198151,0.271653397801502,
1.51955117604055));
#81087=CARTESIAN_POINT('Ctrl Pts',(0.889133341739219,-0.207253044667741,
1.45113831243121));
#81088=CARTESIAN_POINT('Ctrl Pts',(0.915557416280287,-0.686159487136987,
1.38272544882186));
#81089=CARTESIAN_POINT('Ctrl Pts',(0.941981490821354,-1.12785006263026,
1.0539432338035));
#81090=CARTESIAN_POINT('Ctrl Pts',(0.968405565362422,-1.33073196102483,
0.614795628754564));
#81091=CARTESIAN_POINT('Ctrl Pts',(0.979885361627313,-1.41887290445823,
0.4240103269518));
#81092=CARTESIAN_POINT('Ctrl Pts',(0.991365157892203,-1.46194059597963,
0.212394429344695));
#81093=CARTESIAN_POINT('Ctrl Pts',(1.00284495415709,-1.46127859184819,0.000519472235833149));
#81094=CARTESIAN_POINT('Origin',(2.075,0.,0.));
#81095=CARTESIAN_POINT('',(1.57415504584291,-1.46286099658906,-0.00129511982714603));
#81096=CARTESIAN_POINT('',(1.50284495415709,-1.46313245043143,-0.00132110950983211));
#81097=CARTESIAN_POINT('',(2.075,-1.4635,-1.79227059055215E-16));
#81098=CARTESIAN_POINT('Ctrl Pts',(1.57415504584291,-1.46286099658906,-0.00129511982714603));
#81099=CARTESIAN_POINT('Ctrl Pts',(1.55506261007871,-1.45984286410086,0.350117793684843));
#81100=CARTESIAN_POINT('Ctrl Pts',(1.53597017431451,-1.33270149288247,0.703490485179472));
#81101=CARTESIAN_POINT('Ctrl Pts',(1.51687773855032,-1.10228477898897,0.966326030701892));
#81102=CARTESIAN_POINT('Ctrl Pts',(1.49045366400925,-0.783386315816066,
1.3300924004152));
#81103=CARTESIAN_POINT('Ctrl Pts',(1.46402958946818,-0.266666330116682,
1.52043696781344));
#81104=CARTESIAN_POINT('Ctrl Pts',(1.43760551492711,0.212006026409088,1.45047264850784));
#81105=CARTESIAN_POINT('Ctrl Pts',(1.41118144038604,0.690678382934858,1.38050832920223));
#81106=CARTESIAN_POINT('Ctrl Pts',(1.38475736584498,1.13130311028701,1.05023512319278));
#81107=CARTESIAN_POINT('Ctrl Pts',(1.35833329130391,1.33274643432974,0.610413666753209));
#81108=CARTESIAN_POINT('Ctrl Pts',(1.33190921676284,1.53418975837247,0.170592210313635));
#81109=CARTESIAN_POINT('Ctrl Pts',(1.30548514222177,1.49645167910578,-0.378777496556064));
#81110=CARTESIAN_POINT('Ctrl Pts',(1.2790610676807,1.23675879853513,-0.786921626060999));
#81111=CARTESIAN_POINT('Ctrl Pts',(1.25263699313964,0.977065917964476,-1.19506575556593));
#81112=CARTESIAN_POINT('Ctrl Pts',(1.22621291859857,0.495418236089865,-1.46198430770611));
#81113=CARTESIAN_POINT('Ctrl Pts',(1.1997888440575,0.0116750633943819,-1.46583761597847));
#81114=CARTESIAN_POINT('Ctrl Pts',(1.17336476951643,-0.472068109301102,
-1.46969092425084));
#81115=CARTESIAN_POINT('Ctrl Pts',(1.14694069497537,-0.957906772817458,
-1.2104789886554));
#81116=CARTESIAN_POINT('Ctrl Pts',(1.1205166204343,-1.22406769601878,-0.806522080621249));
#81117=CARTESIAN_POINT('Ctrl Pts',(1.10506276223717,-1.37972927494667,-0.570271885186438));
#81118=CARTESIAN_POINT('Ctrl Pts',(1.08960890404004,-1.46025273349283,-0.284513418462271));
#81119=CARTESIAN_POINT('Ctrl Pts',(1.07415504584291,-1.46139381528846,0.000649084939641151));
#81120=CARTESIAN_POINT('Ctrl Pts',(1.00284495415709,-1.46127859184819,0.000519472235833149));
#81121=CARTESIAN_POINT('Ctrl Pts',(1.01778923243327,-1.46041680181882,-0.275297122913305));
#81122=CARTESIAN_POINT('Ctrl Pts',(1.03273351070945,-1.38544822458409,-0.551552734778286));
#81123=CARTESIAN_POINT('Ctrl Pts',(1.04767778898562,-1.23933685982455,-0.782864800020116));
#81124=CARTESIAN_POINT('Ctrl Pts',(1.07410186352669,-0.980986638933794,
-1.19186462866637));
#81125=CARTESIAN_POINT('Ctrl Pts',(1.10052593806776,-0.500212975856397,
-1.4603512908794));
#81126=CARTESIAN_POINT('Ctrl Pts',(1.12695001260883,-0.0164840723619047,
-1.46578875316014));
#81127=CARTESIAN_POINT('Ctrl Pts',(1.1533740871499,0.467244831132591,-1.47122621544088));
#81128=CARTESIAN_POINT('Ctrl Pts',(1.17979816169096,0.953928975044182,-1.21361447778934));
#81129=CARTESIAN_POINT('Ctrl Pts',(1.20622223623203,1.2214137186877,-0.810535480622874));
#81130=CARTESIAN_POINT('Ctrl Pts',(1.2326463107731,1.48889846233122,-0.407456483456409));
#81131=CARTESIAN_POINT('Ctrl Pts',(1.25907038531417,1.53718380570666,0.141089773224978));
#81132=CARTESIAN_POINT('Ctrl Pts',(1.28549445985523,1.34422666083829,0.584700402760684));
#81133=CARTESIAN_POINT('Ctrl Pts',(1.3119185343963,1.15126951596991,1.02831103229639));
#81134=CARTESIAN_POINT('Ctrl Pts',(1.33834260893737,0.717069882857724,1.36698603468642));
#81135=CARTESIAN_POINT('Ctrl Pts',(1.36476668347844,0.239829664321294,1.44613216920364));
#81136=CARTESIAN_POINT('Ctrl Pts',(1.3911907580195,-0.237410554215136,1.52527830372087));
#81137=CARTESIAN_POINT('Ctrl Pts',(1.41761483256057,-0.757691358175806,
1.3448955703653));
#81138=CARTESIAN_POINT('Ctrl Pts',(1.44403890710164,-1.08351870931689,0.987322372169865));
#81139=CARTESIAN_POINT('Ctrl Pts',(1.46364092278679,-1.32522529539969,0.722065951222254));
#81140=CARTESIAN_POINT('Ctrl Pts',(1.48324293847194,-1.45992355989755,0.359301083042489));
#81141=CARTESIAN_POINT('Ctrl Pts',(1.50284495415709,-1.46313245043143,-0.00132110950983211));
#81142=CARTESIAN_POINT('Origin',(2.075,0.,0.));
#81143=CARTESIAN_POINT('',(2.07415504584291,-1.46582439386645,0.000266631823466895));
#81144=CARTESIAN_POINT('',(2.00284495415709,-1.46572742945109,0.000432510777846343));
#81145=CARTESIAN_POINT('',(2.075,-1.4635,-1.79227059055215E-16));
#81146=CARTESIAN_POINT('Ctrl Pts',(2.07415504584291,-1.46582439386645,0.000266631823466895));
#81147=CARTESIAN_POINT('Ctrl Pts',(2.07336446519952,-1.4658608176029,0.0147417778359328));
#81148=CARTESIAN_POINT('Ctrl Pts',(2.07257388455613,-1.46566489447349,0.0292159135494899));
#81149=CARTESIAN_POINT('Ctrl Pts',(2.07178330391274,-1.46523358600562,0.0436830317182805));
#81150=CARTESIAN_POINT('Ctrl Pts',(2.04535922937167,-1.45081769156067,0.527226629810276));
#81151=CARTESIAN_POINT('Ctrl Pts',(2.0189351548306,-1.17344365284929,1.00293065488095));
#81152=CARTESIAN_POINT('Ctrl Pts',(1.99251108028953,-0.759725478262044,
1.25364862470184));
#81153=CARTESIAN_POINT('Ctrl Pts',(1.96608700574846,-0.346007303674802,
1.50436659452273));
#81154=CARTESIAN_POINT('Ctrl Pts',(1.9396629312074,0.2040550067883,1.53009850909383));
#81155=CARTESIAN_POINT('Ctrl Pts',(1.91323885666633,0.639372355957431,1.31909842667499));
#81156=CARTESIAN_POINT('Ctrl Pts',(1.88681478212526,1.07468970512656,1.10809834425614));
#81157=CARTESIAN_POINT('Ctrl Pts',(1.86039070758419,1.39526209300172,0.660366264847353));
#81158=CARTESIAN_POINT('Ctrl Pts',(1.83396663304313,1.45475658686102,0.180280192601334));
#81159=CARTESIAN_POINT('Ctrl Pts',(1.80754255850206,1.51425108072031,-0.299805879644685));
#81160=CARTESIAN_POINT('Ctrl Pts',(1.78111848396099,1.31266768056373,-0.812245944727934));
#81161=CARTESIAN_POINT('Ctrl Pts',(1.75469440941992,0.942023952429685,-1.12312446186072));
#81162=CARTESIAN_POINT('Ctrl Pts',(1.72827033487886,0.571380224295636,-1.4340029789935));
#81163=CARTESIAN_POINT('Ctrl Pts',(1.70184626033779,0.0316761681841161,
-1.54331994817583));
#81164=CARTESIAN_POINT('Ctrl Pts',(1.67542218579672,-0.430727399126193,
-1.40117506038533));
#81165=CARTESIAN_POINT('Ctrl Pts',(1.64899811125565,-0.893130966436502,
-1.25903017259483));
#81166=CARTESIAN_POINT('Ctrl Pts',(1.62257403671458,-1.2782340449456,-0.865423427831514));
#81167=CARTESIAN_POINT('Ctrl Pts',(1.59614996217352,-1.41024711387694,-0.400025969435661));
#81168=CARTESIAN_POINT('Ctrl Pts',(1.58881832339665,-1.44687553519503,-0.270896525476177));
#81169=CARTESIAN_POINT('Ctrl Pts',(1.58148668461978,-1.46401998214006,-0.136240318816841));
#81170=CARTESIAN_POINT('Ctrl Pts',(1.57415504584291,-1.46286099658906,-0.00129511982714603));
#81171=CARTESIAN_POINT('Ctrl Pts',(1.50284495415709,-1.46313245043143,-0.00132110950983211));
#81172=CARTESIAN_POINT('Ctrl Pts',(1.50966701301301,-1.46424923558434,-0.126827887070737));
#81173=CARTESIAN_POINT('Ctrl Pts',(1.51648907186893,-1.4494395291456,-0.252075135634468));
#81174=CARTESIAN_POINT('Ctrl Pts',(1.52331113072484,-1.41767134400802,-0.372862109562419));
#81175=CARTESIAN_POINT('Ctrl Pts',(1.54973520526591,-1.29462272923655,-0.840709730063979));
#81176=CARTESIAN_POINT('Ctrl Pts',(1.57615927980698,-0.917151601372094,
-1.24164130803181));
#81177=CARTESIAN_POINT('Ctrl Pts',(1.60258335434805,-0.457563842382232,
-1.39264248123405));
#81178=CARTESIAN_POINT('Ctrl Pts',(1.62900742888911,0.00202391660763093,
-1.5436436544363));
#81179=CARTESIAN_POINT('Ctrl Pts',(1.65543150343018,0.5437283067229,-1.44471442287297));
#81180=CARTESIAN_POINT('Ctrl Pts',(1.68185557797125,0.920275488657587,-1.14101316666404));
#81181=CARTESIAN_POINT('Ctrl Pts',(1.70827965251232,1.29682267059227,-0.837311910455112));
#81182=CARTESIAN_POINT('Ctrl Pts',(1.73470372705338,1.50821264434637,-0.328838629600589));
#81183=CARTESIAN_POINT('Ctrl Pts',(1.76112780159445,1.45795135754826,0.152301764924768));
#81184=CARTESIAN_POINT('Ctrl Pts',(1.78755187613552,1.40769007075015,0.633442159450128));
#81185=CARTESIAN_POINT('Ctrl Pts',(1.81397595067659,1.09577752339981,1.08724966764632));
#81186=CARTESIAN_POINT('Ctrl Pts',(1.84040002521766,0.664593679489687,1.30657306483852));
#81187=CARTESIAN_POINT('Ctrl Pts',(1.86682409975872,0.233409835579564,1.52589646203071));
#81188=CARTESIAN_POINT('Ctrl Pts',(1.89324817429979,-0.31704530489035,1.51073574821891));
#81189=CARTESIAN_POINT('Ctrl Pts',(1.91967224884086,-0.73550334159657,1.26801135974902));
#81190=CARTESIAN_POINT('Ctrl Pts',(1.94609632338193,-1.15396137830279,1.02528697127912));
#81191=CARTESIAN_POINT('Ctrl Pts',(1.972520397923,-1.44042231124532,0.554998908151132));
#81192=CARTESIAN_POINT('Ctrl Pts',(1.99894447246406,-1.4641241916468,0.0718214210643886));
#81193=CARTESIAN_POINT('Ctrl Pts',(2.00024463302841,-1.46529041035962,0.0480473315191685));
#81194=CARTESIAN_POINT('Ctrl Pts',(2.00154479359275,-1.46582048996688,0.0242420367060462));
#81195=CARTESIAN_POINT('Ctrl Pts',(2.00284495415709,-1.46572742945109,0.000432510777846343));
#81196=CARTESIAN_POINT('Origin',(2.075,0.,0.));
#81197=CARTESIAN_POINT('',(2.57415504584291,-1.4621001751952,0.00110317554495899));
#81198=CARTESIAN_POINT('',(2.50284495415709,-1.46189080583895,0.00100911082079524));
#81199=CARTESIAN_POINT('',(2.075,-1.4635,-1.79227059055215E-16));
#81200=CARTESIAN_POINT('Ctrl Pts',(2.57415504584291,-1.4621001751952,0.00110317554495899));
#81201=CARTESIAN_POINT('Ctrl Pts',(2.56524224577926,-1.46325600427614,0.165366982867302));
#81202=CARTESIAN_POINT('Ctrl Pts',(2.55632944571561,-1.43771198705001,0.329281846754665));
#81203=CARTESIAN_POINT('Ctrl Pts',(2.54741664565196,-1.38391158804006,0.48332822780337));
#81204=CARTESIAN_POINT('Ctrl Pts',(2.52099257111089,-1.22440775718717,0.940034653005688));
#81205=CARTESIAN_POINT('Ctrl Pts',(2.49456849656982,-0.816540414072506,
1.31000063573895));
#81206=CARTESIAN_POINT('Ctrl Pts',(2.46814442202875,-0.34649012402834,1.42434628007155));
#81207=CARTESIAN_POINT('Ctrl Pts',(2.44172034748768,0.123560166015825,1.53869192440415));
#81208=CARTESIAN_POINT('Ctrl Pts',(2.41529627294662,0.655793402989496,1.39741723033608));
#81209=CARTESIAN_POINT('Ctrl Pts',(2.38887219840555,1.00725887392402,1.06501045033488));
#81210=CARTESIAN_POINT('Ctrl Pts',(2.36244812386448,1.35872434485854,0.732603670333682));
#81211=CARTESIAN_POINT('Ctrl Pts',(2.33602404932341,1.5294220497539,0.209064804399345));
#81212=CARTESIAN_POINT('Ctrl Pts',(2.30959997478235,1.44143300464197,-0.266624333721933));
#81213=CARTESIAN_POINT('Ctrl Pts',(2.28317590024128,1.35344395953004,-0.742313471843213));
#81214=CARTESIAN_POINT('Ctrl Pts',(2.25675182570021,1.0067681644108,-1.17015288215143));
#81215=CARTESIAN_POINT('Ctrl Pts',(2.23032775115914,0.559654041834648,-1.35484502332898));
#81216=CARTESIAN_POINT('Ctrl Pts',(2.20390367661807,0.112539919258502,-1.53953716450654));
#81217=CARTESIAN_POINT('Ctrl Pts',(2.17747960207701,-0.435012530774549,
-1.48108203655343));
#81218=CARTESIAN_POINT('Ctrl Pts',(2.15105552753594,-0.833059880701816,
-1.20616288702022));
#81219=CARTESIAN_POINT('Ctrl Pts',(2.12542203363826,-1.21919807068798,-0.939469030591619));
#81220=CARTESIAN_POINT('Ctrl Pts',(2.09978853974058,-1.46464340412969,-0.469070139929011));
#81221=CARTESIAN_POINT('Ctrl Pts',(2.07415504584291,-1.46582439386645,0.000266631823466895));
#81222=CARTESIAN_POINT('Ctrl Pts',(2.00284495415709,-1.46572742945109,0.000432510777846343));
#81223=CARTESIAN_POINT('Ctrl Pts',(2.02796886813382,-1.46392915587056,-0.459655648832342));
#81224=CARTESIAN_POINT('Ctrl Pts',(2.05309278211054,-1.22944698309651,-0.921323729743966));
#81225=CARTESIAN_POINT('Ctrl Pts',(2.07821669608726,-0.856076040177704,
-1.18993771791139));
#81226=CARTESIAN_POINT('Ctrl Pts',(2.10464077062833,-0.46338318044671,-1.47245245875494));
#81227=CARTESIAN_POINT('Ctrl Pts',(2.1310648451694,0.082945366875701,-1.54141502939652));
#81228=CARTESIAN_POINT('Ctrl Pts',(2.15748891971047,0.533524871153222,-1.36534580916677));
#81229=CARTESIAN_POINT('Ctrl Pts',(2.18391299425154,0.984104375430741,-1.18927658893702));
#81230=CARTESIAN_POINT('Ctrl Pts',(2.2103370687926,1.33893483666337,-0.768175577835949));
#81231=CARTESIAN_POINT('Ctrl Pts',(2.23676114333367,1.43604540933339,-0.294264407305756));
#81232=CARTESIAN_POINT('Ctrl Pts',(2.26318521787474,1.53315598200341,0.179646763224435));
#81233=CARTESIAN_POINT('Ctrl Pts',(2.28960929241581,1.37254666611082,0.706368093183742));
#81234=CARTESIAN_POINT('Ctrl Pts',(2.31603336695688,1.02753141629579,1.04546504179445));
#81235=CARTESIAN_POINT('Ctrl Pts',(2.34245744149794,0.682516166480747,1.38456199040515));
#81236=CARTESIAN_POINT('Ctrl Pts',(2.36888151603901,0.153094982743255,1.53603455766725));
#81237=CARTESIAN_POINT('Ctrl Pts',(2.39530559058008,-0.319065158892983,
1.43073945857828));
#81238=CARTESIAN_POINT('Ctrl Pts',(2.42172966512114,-0.791225300529222,
1.32544435948931));
#81239=CARTESIAN_POINT('Ctrl Pts',(2.44815373966221,-1.20612440006421,0.963381594049256));
#81240=CARTESIAN_POINT('Ctrl Pts',(2.47457781420328,-1.37437187360323,0.509823386701214));
#81241=CARTESIAN_POINT('Ctrl Pts',(2.48400019418789,-1.43436608928222,0.348092168144163));
#81242=CARTESIAN_POINT('Ctrl Pts',(2.49342257417249,-1.4629981685089,0.174727162368823));
#81243=CARTESIAN_POINT('Ctrl Pts',(2.50284495415709,-1.46189080583895,0.00100911082079524));
#81244=CARTESIAN_POINT('Origin',(2.075,0.,0.));
#81245=CARTESIAN_POINT('',(3.07415504584291,-1.46191041475934,-0.00101355436836398));
#81246=CARTESIAN_POINT('',(3.00284495415709,-1.46211555199137,-0.00110832896150793));
#81247=CARTESIAN_POINT('',(2.075,-1.4635,-1.79227059055215E-16));
#81248=CARTESIAN_POINT('Ctrl Pts',(3.07415504584291,-1.46191041475934,-0.00101355436836398));
#81249=CARTESIAN_POINT('Ctrl Pts',(3.057120026359,-1.45989180311158,0.313048991404907));
#81250=CARTESIAN_POINT('Ctrl Pts',(3.04008500687508,-1.36064269050357,0.628272692059618));
#81251=CARTESIAN_POINT('Ctrl Pts',(3.02304998739117,-1.17384327638965,0.878009133678142));
#81252=CARTESIAN_POINT('Ctrl Pts',(2.99662591285011,-0.884087127449746,
1.26539080677699));
#81253=CARTESIAN_POINT('Ctrl Pts',(2.97020183830904,-0.383675892838044,
1.49520335760678));
#81254=CARTESIAN_POINT('Ctrl Pts',(2.94377776376797,0.0989770050351939,
1.46253974538111));
#81255=CARTESIAN_POINT('Ctrl Pts',(2.9173536892269,0.581629902908439,1.42987613315544));
#81256=CARTESIAN_POINT('Ctrl Pts',(2.89092961468584,1.04652446404322,1.1347363578743));
#81257=CARTESIAN_POINT('Ctrl Pts',(2.86450554014477,1.28144253601592,0.71184592283405));
#81258=CARTESIAN_POINT('Ctrl Pts',(2.8380814656037,1.51636060798861,0.288955487793809));
#81259=CARTESIAN_POINT('Ctrl Pts',(2.81165739106263,1.52130219079924,-0.261685607005537));
#81260=CARTESIAN_POINT('Ctrl Pts',(2.78523331652156,1.29401468788972,-0.688725062015598));
#81261=CARTESIAN_POINT('Ctrl Pts',(2.7588092419805,1.0667271849802,-1.11576451702566));
#81262=CARTESIAN_POINT('Ctrl Pts',(2.73238516743943,0.607210596350554,-1.41920233224644));
#81263=CARTESIAN_POINT('Ctrl Pts',(2.70596109289836,0.125220624736377,-1.46052653740258));
#81264=CARTESIAN_POINT('Ctrl Pts',(2.6795370183573,-0.356769346877805,-1.50185074255872));
#81265=CARTESIAN_POINT('Ctrl Pts',(2.65311294381622,-0.861232701476513,
-1.28106133765021));
#81266=CARTESIAN_POINT('Ctrl Pts',(2.62668886927516,-1.1578942194803,-0.89894320136026));
#81267=CARTESIAN_POINT('Ctrl Pts',(2.60917759479774,-1.35449225967194,-0.645712929966165));
#81268=CARTESIAN_POINT('Ctrl Pts',(2.59166632032032,-1.45982927938907,-0.321631385556492));
#81269=CARTESIAN_POINT('Ctrl Pts',(2.57415504584291,-1.4621001751952,0.00110317554495899));
#81270=CARTESIAN_POINT('Ctrl Pts',(2.50284495415709,-1.46189080583895,0.00100911082079524));
#81271=CARTESIAN_POINT('Ctrl Pts',(2.51984664871356,-1.45989268626529,-0.312446858497935));
#81272=CARTESIAN_POINT('Ctrl Pts',(2.53684834327002,-1.36106767188624,-0.627052288724924));
#81273=CARTESIAN_POINT('Ctrl Pts',(2.55385003782648,-1.17494880597854,-0.876534820703437));
#81274=CARTESIAN_POINT('Ctrl Pts',(2.58027411236755,-0.88568241727176,-1.264281171504));
#81275=CARTESIAN_POINT('Ctrl Pts',(2.60669818690862,-0.385553792315123,
-1.4947202238491));
#81276=CARTESIAN_POINT('Ctrl Pts',(2.63312226144969,0.0971412829342949,
-1.46266250128816));
#81277=CARTESIAN_POINT('Ctrl Pts',(2.65954633599075,0.579836358183716,-1.43060477872723));
#81278=CARTESIAN_POINT('Ctrl Pts',(2.68597041053182,1.04509788372592,-1.13605028126026));
#81279=CARTESIAN_POINT('Ctrl Pts',(2.71239448507289,1.28054632987947,-0.713455567940678));
#81280=CARTESIAN_POINT('Ctrl Pts',(2.73881855961396,1.51599477603302,-0.290860854621103));
#81281=CARTESIAN_POINT('Ctrl Pts',(2.76524263415503,1.52163014279793,0.25977407455108));
#81282=CARTESIAN_POINT('Ctrl Pts',(2.79166670869609,1.29487961420695,0.687098957268968));
#81283=CARTESIAN_POINT('Ctrl Pts',(2.81809078323716,1.06812908561596,1.11442383998686));
#81284=CARTESIAN_POINT('Ctrl Pts',(2.84451485777823,0.60899266166908,1.41843867625045));
#81285=CARTESIAN_POINT('Ctrl Pts',(2.8709389323193,0.127054938312572,1.46036820791103));
#81286=CARTESIAN_POINT('Ctrl Pts',(2.89736300686036,-0.354882785043935,
1.50229773957161));
#81287=CARTESIAN_POINT('Ctrl Pts',(2.92378708140143,-0.859621807810064,
1.28214196662917));
#81288=CARTESIAN_POINT('Ctrl Pts',(2.9502111559425,-1.15676344772793,0.900397048359602));
#81289=CARTESIAN_POINT('Ctrl Pts',(2.96775575534737,-1.35405440793777,0.646932668539104));
#81290=CARTESIAN_POINT('Ctrl Pts',(2.98530035475223,-1.45982680029096,0.322232288733347));
#81291=CARTESIAN_POINT('Ctrl Pts',(3.00284495415709,-1.46211555199137,-0.00110832896150793));
#81292=CARTESIAN_POINT('Origin',(2.075,0.,0.));
#81293=CARTESIAN_POINT('',(3.57415504584291,-1.46604124392818,-0.000321941105464977));
#81294=CARTESIAN_POINT('',(3.50284495415709,-1.4658722466537,-0.00023313482661453));
#81295=CARTESIAN_POINT('',(2.075,-1.4635,-1.79227059055215E-16));
#81296=CARTESIAN_POINT('Ctrl Pts',(3.57415504584291,-1.46605134156425,-0.000323220338867419));
#81297=CARTESIAN_POINT('Ctrl Pts',(3.54899780693873,-1.46449204195007,0.460439060568385));
#81298=CARTESIAN_POINT('Ctrl Pts',(3.52384056803456,-1.22876388509762,0.922506535519241));
#81299=CARTESIAN_POINT('Ctrl Pts',(3.49868332913039,-0.854425848690436,
1.19096311852186));
#81300=CARTESIAN_POINT('Ctrl Pts',(3.47225925458933,-0.461237382529298,
1.47293829025366));
#81301=CARTESIAN_POINT('Ctrl Pts',(3.44583518004826,0.0848723231897744,
1.54131239917703));
#81302=CARTESIAN_POINT('Ctrl Pts',(3.41941110550719,0.535157675223674,1.36470060702409));
#81303=CARTESIAN_POINT('Ctrl Pts',(3.39298703096612,0.985443027257573,1.18808881487115));
#81304=CARTESIAN_POINT('Ctrl Pts',(3.36656295642505,1.3399040256063,0.766491121641905));
#81305=CARTESIAN_POINT('Ctrl Pts',(3.34013888188399,1.43645708514186,0.292446179449027));
#81306=CARTESIAN_POINT('Ctrl Pts',(3.31371480734292,1.53301014467742,-0.181598762743851));
#81307=CARTESIAN_POINT('Ctrl Pts',(3.28729073280185,1.37165526539981,-0.708090953900364));
#81308=CARTESIAN_POINT('Ctrl Pts',(3.26086665826079,1.026194375012,-1.04674777447125));
#81309=CARTESIAN_POINT('Ctrl Pts',(3.23444258371972,0.68073348462418,-1.38540459504213));
#81310=CARTESIAN_POINT('Ctrl Pts',(3.20801850917865,0.151166583126158,-1.53622604502739));
#81311=CARTESIAN_POINT('Ctrl Pts',(3.18159443463758,-0.320850406538498,
-1.43034120921067));
#81312=CARTESIAN_POINT('Ctrl Pts',(3.15517036009651,-0.792867396203154,
-1.32445637339395));
#81313=CARTESIAN_POINT('Ctrl Pts',(3.12874628555544,-1.20733447403444,-0.961865251775244));
#81314=CARTESIAN_POINT('Ctrl Pts',(3.10232221101438,-1.37501748131604,-0.508094293281935));
#81315=CARTESIAN_POINT('Ctrl Pts',(3.09293315595722,-1.43459894310271,-0.346859488028452));
#81316=CARTESIAN_POINT('Ctrl Pts',(3.08354410090006,-1.46302299675068,-0.174112888739021));
#81317=CARTESIAN_POINT('Ctrl Pts',(3.07415504584291,-1.46191041475934,-0.00101355436836398));
#81318=CARTESIAN_POINT('Ctrl Pts',(3.00284495415709,-1.46211555199137,-0.00110832896150793));
#81319=CARTESIAN_POINT('Ctrl Pts',(3.0117244292933,-1.46327390923554,-0.164753842266872));
#81320=CARTESIAN_POINT('Ctrl Pts',(3.0206039044295,-1.43792533976859,-0.328051057866522));
#81321=CARTESIAN_POINT('Ctrl Pts',(3.0294833795657,-1.38451871835904,-0.481588823801387));
#81322=CARTESIAN_POINT('Ctrl Pts',(3.05590745410677,-1.22558809200266,-0.938495714096107));
#81323=CARTESIAN_POINT('Ctrl Pts',(3.08233152864784,-0.818182582220306,
-1.30897543108885));
#81324=CARTESIAN_POINT('Ctrl Pts',(3.10875560318891,-0.34827766430965,-1.42391077883767));
#81325=CARTESIAN_POINT('Ctrl Pts',(3.13517967772997,0.121627253601006,-1.53884612658648));
#81326=CARTESIAN_POINT('Ctrl Pts',(3.16160375227104,0.65403157963996,-1.39823710509136));
#81327=CARTESIAN_POINT('Ctrl Pts',(3.18802782681211,1.00591707366984,-1.06627352702385));
#81328=CARTESIAN_POINT('Ctrl Pts',(3.21445190135318,1.35780256769973,-0.73430994895634));
#81329=CARTESIAN_POINT('Ctrl Pts',(3.24087597589425,1.52916922972054,-0.210991814316436));
#81330=CARTESIAN_POINT('Ctrl Pts',(3.26730005043531,1.44177276521797,0.264810197511405));
#81331=CARTESIAN_POINT('Ctrl Pts',(3.29372412497638,1.3543763007154,0.740612209339246));
#81332=CARTESIAN_POINT('Ctrl Pts',(3.32014819951745,1.00821670968944,1.16889809835502));
#81333=CARTESIAN_POINT('Ctrl Pts',(3.34657227405851,0.561344663652188,1.35414673718099));
#81334=CARTESIAN_POINT('Ctrl Pts',(3.37299634859958,0.114472617614934,1.53939537600697));
#81335=CARTESIAN_POINT('Ctrl Pts',(3.39942042314065,-0.43311188343362,1.48160676464313));
#81336=CARTESIAN_POINT('Ctrl Pts',(3.42584449768172,-0.831522847359714,
1.20719757316213));
#81337=CARTESIAN_POINT('Ctrl Pts',(3.45151131650685,-1.2185162314853,0.940652344085303));
#81338=CARTESIAN_POINT('Ctrl Pts',(3.47717813533197,-1.46476353619869,0.469724367507778));
#81339=CARTESIAN_POINT('Ctrl Pts',(3.50284495415709,-1.4658722466537,-0.00023313482661453));
#81340=CARTESIAN_POINT('Origin',(-0.510867114736157,0.,0.));
#81341=CARTESIAN_POINT('',(3.23913288526384,-1.17647078304258,-0.000815656752585949));
#81342=CARTESIAN_POINT('',(3.33786711473616,-1.17965906286054,-0.000187614992894769));
#81343=CARTESIAN_POINT('',(-0.510867114736157,-1.17775,-2.64996692395027E-14));
#81344=CARTESIAN_POINT('',(3.7365,-1.1771054344427,0.038959706177682));
#81345=CARTESIAN_POINT('Ctrl Pts',(3.23913288526384,-1.17647078304258,-0.000815656752586099));
#81346=CARTESIAN_POINT('Ctrl Pts',(3.248521940321,-1.17736613216475,-0.140117153886184));
#81347=CARTESIAN_POINT('Ctrl Pts',(3.28433506991922,-1.09011586029682,-0.670378880060937));
#81348=CARTESIAN_POINT('Ctrl Pts',(3.34657227405852,-0.30451723605224,-1.35764959839504));
#81349=CARTESIAN_POINT('Ctrl Pts',(3.42584449768172,0.973987891872518,-0.993529415162783));
#81350=CARTESIAN_POINT('Ctrl Pts',(3.50511672130493,1.36353837168639,0.277552603562025));
#81351=CARTESIAN_POINT('Ctrl Pts',(3.58438894492812,0.507782087152296,1.29539343007532));
#81352=CARTESIAN_POINT('Ctrl Pts',(3.66151670449316,-0.774995051475287,
1.13478697521395));
#81353=CARTESIAN_POINT('Ctrl Pts',(3.71222038951711,-1.16517681126,0.396292593442729));
#81354=CARTESIAN_POINT('Ctrl Pts',(3.7365,-1.17898709763096,0.0385437240067104));
#81355=CARTESIAN_POINT('',(3.7365,-0.344648939580369,1.12619366493784));
#81356=CARTESIAN_POINT('Origin',(3.7365,0.,0.));
#81357=CARTESIAN_POINT('Ctrl Pts',(3.33786711473616,-1.17965906286054,-0.000187614992895038));
#81358=CARTESIAN_POINT('Ctrl Pts',(3.3386243704521,-1.17968538668852,-0.0113456954406013));
#81359=CARTESIAN_POINT('Ctrl Pts',(3.36580570070911,-1.17446657122554,-0.411835233187));
#81360=CARTESIAN_POINT('Ctrl Pts',(3.41941110550719,-0.722370214448171,
-1.18914586543665));
#81361=CARTESIAN_POINT('Ctrl Pts',(3.49868332913039,0.60485244622559,-1.25257895798247));
#81362=CARTESIAN_POINT('Ctrl Pts',(3.57795555275359,1.38146769635508,-0.173309657930487));
#81363=CARTESIAN_POINT('Ctrl Pts',(3.6572277763768,0.893721090248042,1.06587168358242));
#81364=CARTESIAN_POINT('Ctrl Pts',(3.71007592545893,0.029308975541542,1.24063596994012));
#81365=CARTESIAN_POINT('Ctrl Pts',(3.7365,-0.344648939580369,1.12619366493784));
#81366=CARTESIAN_POINT('Origin',(-0.510867114736157,0.,0.));
#81367=CARTESIAN_POINT('',(2.73913288526384,-1.17662349254263,0.000887779294870973));
#81368=CARTESIAN_POINT('',(2.83786711473616,-1.17663586700228,-0.000891926501168649));
#81369=CARTESIAN_POINT('',(-0.510867114736157,-1.17775,-2.64996692395027E-14));
#81370=CARTESIAN_POINT('Ctrl Pts',(2.73913288526384,-1.17662349254263,0.000887779294870931));
#81371=CARTESIAN_POINT('Ctrl Pts',(2.75664415974126,-1.17479599166414,-0.258832500402587));
#81372=CARTESIAN_POINT('Ctrl Pts',(2.80057950875975,-0.96211056230301,-0.913183863350559));
#81373=CARTESIAN_POINT('Ctrl Pts',(2.87093893231929,0.118856588721082,-1.38629274593749));
#81374=CARTESIAN_POINT('Ctrl Pts',(2.9502111559425,1.22824298214487,-0.653719011308979));
#81375=CARTESIAN_POINT('Ctrl Pts',(3.0294833795657,1.21631278230501,0.675664417594188));
#81376=CARTESIAN_POINT('Ctrl Pts',(3.10875560318891,0.0939426366750465,
1.38820463693965));
#81377=CARTESIAN_POINT('Ctrl Pts',(3.17863877175495,-0.971083435973477,
0.899094198311085));
#81378=CARTESIAN_POINT('Ctrl Pts',(3.22209786577993,-1.17484630756042,0.251925828238525));
#81379=CARTESIAN_POINT('Ctrl Pts',(3.23913288526384,-1.17647078304258,-0.000815656752586099));
#81380=CARTESIAN_POINT('Ctrl Pts',(2.83786711473616,-1.17663586700228,-0.000891926501168892));
#81381=CARTESIAN_POINT('Ctrl Pts',(2.84674658987236,-1.17756805370834,-0.132585471629546));
#81382=CARTESIAN_POINT('Ctrl Pts',(2.88205013954964,-1.09646355944131,-0.655066162450786));
#81383=CARTESIAN_POINT('Ctrl Pts',(2.94377776376796,-0.330572392937332,
-1.35153966563246));
#81384=CARTESIAN_POINT('Ctrl Pts',(3.02304998739118,0.954782977733753,-1.01207480386435));
#81385=CARTESIAN_POINT('Ctrl Pts',(3.10232221101437,1.3685043706856,0.251344259488195));
#81386=CARTESIAN_POINT('Ctrl Pts',(3.18159443463759,0.532789731128058,1.28533204040039));
#81387=CARTESIAN_POINT('Ctrl Pts',(3.26010940254484,-0.776585752658408,
1.14714881787129));
#81388=CARTESIAN_POINT('Ctrl Pts',(3.31220029591104,-1.17876682935294,0.378010163192515));
#81389=CARTESIAN_POINT('Ctrl Pts',(3.33786711473616,-1.17965906286054,-0.000187614992895038));
#81390=CARTESIAN_POINT('Origin',(-0.510867114736157,0.,0.));
#81391=CARTESIAN_POINT('',(2.23913288526384,-1.17962055338313,0.000214571663858193));
#81392=CARTESIAN_POINT('',(2.33786711473616,-1.17645500278567,0.000812080812545024));
#81393=CARTESIAN_POINT('',(-0.510867114736157,-1.17775,-2.64996692395027E-14));
#81394=CARTESIAN_POINT('Ctrl Pts',(2.23913288526384,-1.17962055338313,0.000214571663858217));
#81395=CARTESIAN_POINT('Ctrl Pts',(2.26476637916152,-1.17867015320378,-0.377483674274969));
#81396=CARTESIAN_POINT('Ctrl Pts',(2.31682394760027,-0.77753452327143,-1.14626486346891));
#81397=CARTESIAN_POINT('Ctrl Pts',(2.39530559058008,0.53120860125257,-1.28598252302312));
#81398=CARTESIAN_POINT('Ctrl Pts',(2.47457781420328,1.36816948482281,-0.25307265184342));
#81399=CARTESIAN_POINT('Ctrl Pts',(2.55385003782648,0.956063119382725,1.01087931130145));
#81400=CARTESIAN_POINT('Ctrl Pts',(2.63312226144969,-0.328879200082413,
1.35195127086139));
#81401=CARTESIAN_POINT('Ctrl Pts',(2.69488321059547,-1.09605252871168,0.65606806460703));
#81402=CARTESIAN_POINT('Ctrl Pts',(2.73022008520019,-1.17755364471214,0.133078895846903));
#81403=CARTESIAN_POINT('Ctrl Pts',(2.73913288526384,-1.17662349254263,0.000887779294870931));
#81404=CARTESIAN_POINT('Ctrl Pts',(2.33786711473616,-1.17645500278567,0.00081208081254492));
#81405=CARTESIAN_POINT('Ctrl Pts',(2.35486880929262,-1.17484701827737,-0.251441262450268));
#81406=CARTESIAN_POINT('Ctrl Pts',(2.39829457839015,-0.971713036485233,
-0.898110065252741));
#81407=CARTESIAN_POINT('Ctrl Pts',(2.46814442202875,0.0922039693498821,
-1.3883200119834));
#81408=CARTESIAN_POINT('Ctrl Pts',(2.54741664565196,1.21546005757808,-0.677192797651213));
#81409=CARTESIAN_POINT('Ctrl Pts',(2.62668886927516,1.22906522301855,0.65217574590713));
#81410=CARTESIAN_POINT('Ctrl Pts',(2.70596109289836,0.120596640913772,1.38614255166615));
#81411=CARTESIAN_POINT('Ctrl Pts',(2.77635384138536,-0.96147348091212,0.914167980049009));
#81412=CARTESIAN_POINT('Ctrl Pts',(2.82032251533129,-1.1747939966127,0.259316076566906));
#81413=CARTESIAN_POINT('Ctrl Pts',(2.83786711473616,-1.17663586700228,-0.000891926501168892));
#81414=CARTESIAN_POINT('Origin',(-0.510867114736157,0.,0.));
#81415=CARTESIAN_POINT('',(1.73913288526384,-1.17723576271456,-0.00104224624287887));
#81416=CARTESIAN_POINT('',(1.83786711473616,-1.17954252137753,0.000348062568210376));
#81417=CARTESIAN_POINT('',(-0.510867114736157,-1.17775,-2.64996692395027E-14));
#81418=CARTESIAN_POINT('Ctrl Pts',(1.73913288526384,-1.17723576271456,-0.00104224624287901));
#81419=CARTESIAN_POINT('Ctrl Pts',(1.74646452404071,-1.17816845504985,-0.109639245293173));
#81420=CARTESIAN_POINT('Ctrl Pts',(1.78022023735865,-1.11464558726191,-0.608561633391758));
#81421=CARTESIAN_POINT('Ctrl Pts',(1.84040002521766,-0.408834878719842,
-1.32995772423544));
#81422=CARTESIAN_POINT('Ctrl Pts',(1.91967224884086,0.894143840963125,-1.06603959552792));
#81423=CARTESIAN_POINT('Ctrl Pts',(1.99894447246406,1.3808158933056,0.17111712463292));
#81424=CARTESIAN_POINT('Ctrl Pts',(2.07821669608726,0.606875073722467,1.2520528059251));
#81425=CARTESIAN_POINT('Ctrl Pts',(2.15748891971047,-0.721111027024888,
1.18992961688625));
#81426=CARTESIAN_POINT('Ctrl Pts',(2.21112764943599,-1.17422232882441,0.41283140296388));
#81427=CARTESIAN_POINT('Ctrl Pts',(2.23834230462045,-1.17964986534459,0.0118634293448927));
#81428=CARTESIAN_POINT('Ctrl Pts',(2.23913288526384,-1.17962055338313,0.000214571663858217));
#81429=CARTESIAN_POINT('Ctrl Pts',(1.83786711473616,-1.17954252137753,0.000348062568210372));
#81430=CARTESIAN_POINT('Ctrl Pts',(1.86299102871288,-1.17809536271031,-0.369907373018322));
#81431=CARTESIAN_POINT('Ctrl Pts',(1.91453901723068,-0.790931654118442,
-1.13218761048638));
#81432=CARTESIAN_POINT('Ctrl Pts',(1.99251108028953,0.506407483735447,-1.29594958554484));
#81433=CARTESIAN_POINT('Ctrl Pts',(2.07178330391274,1.3630557428063,-0.279307872204986));
#81434=CARTESIAN_POINT('Ctrl Pts',(2.15105552753594,0.975305236911186,0.992327344111197));
#81435=CARTESIAN_POINT('Ctrl Pts',(2.23032775115914,-0.302848092395607,
1.35801948506016));
#81436=CARTESIAN_POINT('Ctrl Pts',(2.29259828022588,-1.08968667651,0.671382772571054));
#81437=CARTESIAN_POINT('Ctrl Pts',(2.32844473475155,-1.17734615166475,0.140611489907658));
#81438=CARTESIAN_POINT('Ctrl Pts',(2.33786711473616,-1.17645500278567,0.00081208081254492));
#81439=CARTESIAN_POINT('Origin',(-0.510867114736157,0.,0.));
#81440=CARTESIAN_POINT('',(1.23913288526384,-1.17605505019199,0.000522350384450236));
#81441=CARTESIAN_POINT('',(1.33786711473616,-1.1774542148928,-0.00106316141115878));
#81442=CARTESIAN_POINT('',(-0.510867114736157,-1.17775,-2.64996692395027E-14));
#81443=CARTESIAN_POINT('Ctrl Pts',(1.23913288526384,-1.17605505019199,0.000522350384450018));
#81444=CARTESIAN_POINT('Ctrl Pts',(1.25458674346097,-1.17513676588396,-0.22896185759751));
#81445=CARTESIAN_POINT('Ctrl Pts',(1.29646467619917,-0.999534094584203,
-0.852133676211331));
#81446=CARTESIAN_POINT('Ctrl Pts',(1.36476668347844,0.0110818382145732,
-1.39133265677073));
#81447=CARTESIAN_POINT('Ctrl Pts',(1.44403890710164,1.1738981497851,-0.746925431386865));
#81448=CARTESIAN_POINT('Ctrl Pts',(1.52331113072484,1.26500718194706,0.579388553442205));
#81449=CARTESIAN_POINT('Ctrl Pts',(1.60258335434805,0.201230401682631,1.37674954089208));
#81450=CARTESIAN_POINT('Ctrl Pts',(1.67452393919438,-0.930882719706594,
0.959712096433582));
#81451=CARTESIAN_POINT('Ctrl Pts',(1.72004044949964,-1.17480692394588,0.281756905713905));
#81452=CARTESIAN_POINT('Ctrl Pts',(1.73913288526384,-1.17723576271456,-0.00104224624287901));
#81453=CARTESIAN_POINT('Ctrl Pts',(1.33786711473616,-1.1774542148928,-0.00106316141115873));
#81454=CARTESIAN_POINT('Ctrl Pts',(1.34468917359208,-1.17835294650458,-0.102064601296605));
#81455=CARTESIAN_POINT('Ctrl Pts',(1.37793530698906,-1.12027215618224,-0.593259967820105));
#81456=CARTESIAN_POINT('Ctrl Pts',(1.43760551492711,-0.434307261820031,
-1.32185870617429));
#81457=CARTESIAN_POINT('Ctrl Pts',(1.51687773855032,0.873500757568272,-1.08301913841129));
#81458=CARTESIAN_POINT('Ctrl Pts',(1.59614996217352,1.38384829755233,0.144560786138938));
#81459=CARTESIAN_POINT('Ctrl Pts',(1.67542218579672,0.630814469109849,1.24016405114351));
#81460=CARTESIAN_POINT('Ctrl Pts',(1.75469440941992,-0.698120020172913,
1.20356234832455));
#81461=CARTESIAN_POINT('Ctrl Pts',(1.8088427190664,-1.17052112656004,0.428012959930639));
#81462=CARTESIAN_POINT('Ctrl Pts',(1.83656695417181,-1.17961741172428,0.0195087521219825));
#81463=CARTESIAN_POINT('Ctrl Pts',(1.83786711473616,-1.17954252137753,0.000348062568210372));
#81464=CARTESIAN_POINT('Origin',(-0.510867114736157,0.,0.));
#81465=CARTESIAN_POINT('',(0.739132885263843,-1.17911213255423,0.000786107540026912));
#81466=CARTESIAN_POINT('',(0.837867114736159,-1.17596232425638,0.000418044704970089));
#81467=CARTESIAN_POINT('',(-0.510867114736157,-1.17775,-2.64996692395027E-14));
#81468=CARTESIAN_POINT('Ctrl Pts',(0.739132885263843,-1.17911213255423,
0.000786107540026912));
#81469=CARTESIAN_POINT('Ctrl Pts',(0.762708962881233,-1.17664592192968,
-0.346963469627478));
#81470=CARTESIAN_POINT('Ctrl Pts',(0.812709115039692,-0.830115587406687,
-1.08901150369434));
#81471=CARTESIAN_POINT('Ctrl Pts',(0.889133341739219,0.429979607970486,
-1.32320468901736));
#81472=CARTESIAN_POINT('Ctrl Pts',(0.968405565362423,1.34444024085867,-0.358362411303147));
#81473=CARTESIAN_POINT('Ctrl Pts',(1.04767778898562,1.03152012276366,0.933779522210948));
#81474=CARTESIAN_POINT('Ctrl Pts',(1.12695001260883,-0.223136159389758,
1.3733593350842));
#81475=CARTESIAN_POINT('Ctrl Pts',(1.1907683780349,-1.06919746578618,0.717893990913368));
#81476=CARTESIAN_POINT('Ctrl Pts',(1.2281626689199,-1.17670691184336,0.16342609758892));
#81477=CARTESIAN_POINT('Ctrl Pts',(1.23913288526384,-1.17605505019199,0.000522350384450018));
#81478=CARTESIAN_POINT('Ctrl Pts',(0.837867114736159,-1.17596232425638,
0.000418044704970002));
#81479=CARTESIAN_POINT('Ctrl Pts',(0.852811393012336,-1.17526879968713,
-0.221545053987815));
#81480=CARTESIAN_POINT('Ctrl Pts',(0.89417974582958,-1.00826246762855,-0.836955378552283));
#81481=CARTESIAN_POINT('Ctrl Pts',(0.961972173187893,-0.0156437653744218,
-1.39128042313263));
#81482=CARTESIAN_POINT('Ctrl Pts',(1.0412443968111,1.15933180789216,-0.769342143626431));
#81483=CARTESIAN_POINT('Ctrl Pts',(1.1205166204343,1.27590453729514,0.554983829328479));
#81484=CARTESIAN_POINT('Ctrl Pts',(1.1997888440575,0.227639519397196,1.3726288257033));
#81485=CARTESIAN_POINT('Ctrl Pts',(1.27223900882479,-0.920349622811229,
0.974617948196986));
#81486=CARTESIAN_POINT('Ctrl Pts',(1.31826509905101,-1.17487186379867,0.289147147627791));
#81487=CARTESIAN_POINT('Ctrl Pts',(1.33786711473616,-1.1774542148928,-0.00106316141115873));
#81488=CARTESIAN_POINT('Origin',(3.7365,3.28582941601228E-17,0.));
#81489=CARTESIAN_POINT('',(3.7365,0.66187319412785,-1.30528009442227));
#81490=CARTESIAN_POINT('Ctrl Pts',(3.7365,-1.17898709763096,0.0385437240067023));
#81491=CARTESIAN_POINT('Ctrl Pts',(3.7365,-1.18395318976076,0.0068885070196644));
#81492=CARTESIAN_POINT('Ctrl Pts',(3.7365,-1.18753666953077,-0.0249123100679694));
#81493=CARTESIAN_POINT('Ctrl Pts',(3.7365,-1.1896998725534,-0.0567807570343834));
#81494=CARTESIAN_POINT('Ctrl Pts',(3.7365,-1.19296909471786,-0.104943149597595));
#81495=CARTESIAN_POINT('Ctrl Pts',(3.7365,-1.19299730966002,-0.153259572705676));
#81496=CARTESIAN_POINT('Ctrl Pts',(3.7365,-1.18997678969837,-0.201492670338683));
#81497=CARTESIAN_POINT('Ctrl Pts',(3.7365,-1.18852496860528,-0.224676039234535));
#81498=CARTESIAN_POINT('Ctrl Pts',(3.7365,-1.18636806011878,-0.247840396141398));
#81499=CARTESIAN_POINT('Ctrl Pts',(3.7365,-1.18352338482475,-0.270960259527509));
#81500=CARTESIAN_POINT('Ctrl Pts',(3.7365,-1.18229282775955,-0.28096151038943));
#81501=CARTESIAN_POINT('Ctrl Pts',(3.7365,-1.18093363039742,-0.290953014018376));
#81502=CARTESIAN_POINT('Ctrl Pts',(3.7365,-1.17944884835669,-0.300923054854913));
#81503=CARTESIAN_POINT('Ctrl Pts',(3.7365,-1.17199727383116,-0.350959019917949));
#81504=CARTESIAN_POINT('Ctrl Pts',(3.7365,-1.16137910126565,-0.400519951283811));
#81505=CARTESIAN_POINT('Ctrl Pts',(3.7365,-1.14780434654206,-0.449345351076564));
#81506=CARTESIAN_POINT('Ctrl Pts',(3.7365,-1.1381603195141,-0.484032789990987));
#81507=CARTESIAN_POINT('Ctrl Pts',(3.7365,-1.12702287204522,-0.518349414699403));
#81508=CARTESIAN_POINT('Ctrl Pts',(3.7365,-1.11445155766447,-0.552203463055681));
#81509=CARTESIAN_POINT('Ctrl Pts',(3.7365,-1.10956752286223,-0.565355974031146));
#81510=CARTESIAN_POINT('Ctrl Pts',(3.7365,-1.10446693006086,-0.578438661643457));
#81511=CARTESIAN_POINT('Ctrl Pts',(3.7365,-1.09915277069566,-0.591446096472848));
#81512=CARTESIAN_POINT('Ctrl Pts',(3.7365,-1.09531873084628,-0.600830651968257));
#81513=CARTESIAN_POINT('Ctrl Pts',(3.7365,-1.09137504997109,-0.610172118209165));
#81514=CARTESIAN_POINT('Ctrl Pts',(3.7365,-1.087326496467,-0.619461079847843));
#81515=CARTESIAN_POINT('Ctrl Pts',(3.7365,-1.06633587924426,-0.667621747097829));
#81516=CARTESIAN_POINT('Ctrl Pts',(3.7365,-1.04250587869293,-0.714431076751343));
#81517=CARTESIAN_POINT('Ctrl Pts',(3.7365,-1.01604654267101,-0.75962191442263));
#81518=CARTESIAN_POINT('Ctrl Pts',(3.7365,-0.989101302874277,-0.805642644370617));
#81519=CARTESIAN_POINT('Ctrl Pts',(3.7365,-0.959429029561841,-0.849986048299225));
#81520=CARTESIAN_POINT('Ctrl Pts',(3.7365,-0.927198803465423,-0.892364654491487));
#81521=CARTESIAN_POINT('Ctrl Pts',(3.7365,-0.908698673052218,-0.916689948981861));
#81522=CARTESIAN_POINT('Ctrl Pts',(3.7365,-0.889354812189278,-0.940367701839285));
#81523=CARTESIAN_POINT('Ctrl Pts',(3.7365,-0.869192074342517,-0.963340448953061));
#81524=CARTESIAN_POINT('Ctrl Pts',(3.7365,-0.857848710493305,-0.976264697192959));
#81525=CARTESIAN_POINT('Ctrl Pts',(3.7365,-0.846246075599409,-0.988965753946543));
#81526=CARTESIAN_POINT('Ctrl Pts',(3.7365,-0.834387932224055,-1.00143289879475));
#81527=CARTESIAN_POINT('Ctrl Pts',(3.7365,-0.827553225622948,-1.00861861703864));
#81528=CARTESIAN_POINT('Ctrl Pts',(3.7365,-0.820633298378763,-1.01572679588455));
#81529=CARTESIAN_POINT('Ctrl Pts',(3.7365,-0.813639868172984,-1.02274468687781));
#81530=CARTESIAN_POINT('Ctrl Pts',(3.7365,-0.774949026471088,-1.06157085679896));
#81531=CARTESIAN_POINT('Ctrl Pts',(3.7365,-0.733934919892263,-1.09771763061715));
#81532=CARTESIAN_POINT('Ctrl Pts',(3.7365,-0.69079018012452,-1.13089396681559));
#81533=CARTESIAN_POINT('Ctrl Pts',(3.7365,-0.683113793755067,-1.13679675766224));
#81534=CARTESIAN_POINT('Ctrl Pts',(3.7365,-0.675369835460676,-1.14260546817357));
#81535=CARTESIAN_POINT('Ctrl Pts',(3.7365,-0.667559232793028,-1.14831838686635));
#81536=CARTESIAN_POINT('Ctrl Pts',(3.7365,-0.625187949984191,-1.17931006624061));
#81537=CARTESIAN_POINT('Ctrl Pts',(3.7365,-0.580858497988276,-1.20748566736297));
#81538=CARTESIAN_POINT('Ctrl Pts',(3.7365,-0.534866759029188,-1.23287345299529));
#81539=CARTESIAN_POINT('Ctrl Pts',(3.7365,-0.511266715166499,-1.24590085461261));
#81540=CARTESIAN_POINT('Ctrl Pts',(3.7365,-0.48722834897051,-1.25819361049471));
#81541=CARTESIAN_POINT('Ctrl Pts',(3.7365,-0.462788279793142,-1.26975163493864));
#81542=CARTESIAN_POINT('Ctrl Pts',(3.7365,-0.447910497377259,-1.27678753044231));
#81543=CARTESIAN_POINT('Ctrl Pts',(3.7365,-0.432883815548152,-1.28355110292038));
#81544=CARTESIAN_POINT('Ctrl Pts',(3.7365,-0.41771617777022,-1.29004182329204));
#81545=CARTESIAN_POINT('Ctrl Pts',(3.7365,-0.407705569003771,-1.29432568497205));
#81546=CARTESIAN_POINT('Ctrl Pts',(3.7365,-0.397632108665662,-1.2984911384465));
#81547=CARTESIAN_POINT('Ctrl Pts',(3.7365,-0.38751563048501,-1.30253128217036));
#81548=CARTESIAN_POINT('Ctrl Pts',(3.7365,-0.336601391291811,-1.32286452860831));
#81549=CARTESIAN_POINT('Ctrl Pts',(3.7365,-0.284504357316613,-1.34006945525572));
#81550=CARTESIAN_POINT('Ctrl Pts',(3.7365,-0.231557314522765,-1.35419331042861));
#81551=CARTESIAN_POINT('Ctrl Pts',(3.7365,-0.177455970281344,-1.36862508055975));
#81552=CARTESIAN_POINT('Ctrl Pts',(3.7365,-0.12246626002564,-1.37984038062529));
#81553=CARTESIAN_POINT('Ctrl Pts',(3.7365,-0.066909525356045,-1.38784621613597));
#81554=CARTESIAN_POINT('Ctrl Pts',(3.7365,-0.0356886580014238,-1.39234520496295));
#81555=CARTESIAN_POINT('Ctrl Pts',(3.7365,-0.00428819436563625,-1.39582982383752));
#81556=CARTESIAN_POINT('Ctrl Pts',(3.7365,0.0272376679168194,-1.39829475873246));
#81557=CARTESIAN_POINT('Ctrl Pts',(3.7365,0.047886366616149,-1.39990923314407));
#81558=CARTESIAN_POINT('Ctrl Pts',(3.7365,0.0685888961784583,-1.40108617121842));
#81559=CARTESIAN_POINT('Ctrl Pts',(3.7365,0.0893302635243502,-1.40182292113385));
#81560=CARTESIAN_POINT('Ctrl Pts',(3.7365,0.0997890716871271,-1.40219442634375));
#81561=CARTESIAN_POINT('Ctrl Pts',(3.7365,0.11026029244007,-1.40245402241009));
#81562=CARTESIAN_POINT('Ctrl Pts',(3.7365,0.120733734333452,-1.40260117612064));
#81563=CARTESIAN_POINT('Ctrl Pts',(3.7365,0.178939128318525,-1.40341897219821));
#81564=CARTESIAN_POINT('Ctrl Pts',(3.7365,0.237032745754499,-1.40076707020305));
#81565=CARTESIAN_POINT('Ctrl Pts',(3.7365,0.294671049963821,-1.39466962302802));
#81566=CARTESIAN_POINT('Ctrl Pts',(3.7365,0.35245700073739,-1.38855655660224));
#81567=CARTESIAN_POINT('Ctrl Pts',(3.7365,0.409786446730489,-1.37898053666939));
#81568=CARTESIAN_POINT('Ctrl Pts',(3.7365,0.466329084911745,-1.36591626968488));
#81569=CARTESIAN_POINT('Ctrl Pts',(3.7365,0.521568448510678,-1.35315312637705));
#81570=CARTESIAN_POINT('Ctrl Pts',(3.7365,0.576057945793192,-1.33706073718071));
#81571=CARTESIAN_POINT('Ctrl Pts',(3.7365,0.629488202861402,-1.31756621599704));
#81572=CARTESIAN_POINT('Ctrl Pts',(3.7365,0.640327714531275,-1.31361132037302));
#81573=CARTESIAN_POINT('Ctrl Pts',(3.7365,0.651123595619572,-1.30951623562727));
#81574=CARTESIAN_POINT('Ctrl Pts',(3.7365,0.661873194127841,-1.30528009442227));
#81575=CARTESIAN_POINT('',(3.7365,-1.4635,-1.79227059055215E-16));
#81576=CARTESIAN_POINT('Origin',(3.7365,0.,0.));
#81577=CARTESIAN_POINT('',(3.7365,1.43393351041226,-0.298434655783759));
#81578=CARTESIAN_POINT('Origin',(3.7365,0.,0.));
#81579=CARTESIAN_POINT('Ctrl Pts',(3.7365,1.43512958320548,-0.29838030867993));
#81580=CARTESIAN_POINT('Ctrl Pts',(3.7365,1.43970072126023,-0.259303035834852));
#81581=CARTESIAN_POINT('Ctrl Pts',(3.7365,1.44258412773515,-0.22010113429756));
#81582=CARTESIAN_POINT('Ctrl Pts',(3.7365,1.44371345760419,-0.180852703561548));
#81583=CARTESIAN_POINT('Ctrl Pts',(3.7365,1.44536844720772,-0.123335633834173));
#81584=CARTESIAN_POINT('Ctrl Pts',(3.7365,1.44325833111679,-0.0657175785747762));
#81585=CARTESIAN_POINT('Ctrl Pts',(3.7365,1.43753775138039,-0.00830635976255858));
#81586=CARTESIAN_POINT('Ctrl Pts',(3.7365,1.43561812626606,0.0109588235850785));
#81587=CARTESIAN_POINT('Ctrl Pts',(3.7365,1.43329155082908,0.0302005775953646));
#81588=CARTESIAN_POINT('Ctrl Pts',(3.7365,1.43056272371359,0.0494067470887997));
#81589=CARTESIAN_POINT('Ctrl Pts',(3.7365,1.42888893925048,0.0611872618423588));
#81590=CARTESIAN_POINT('Ctrl Pts',(3.7365,1.42706380724748,0.0729543826609247));
#81591=CARTESIAN_POINT('Ctrl Pts',(3.7365,1.42508831579175,0.0847052377538888));
#81592=CARTESIAN_POINT('Ctrl Pts',(3.7365,1.42299842767926,0.0971365607541427));
#81593=CARTESIAN_POINT('Ctrl Pts',(3.7365,1.4207417497427,0.109540674919579));
#81594=CARTESIAN_POINT('Ctrl Pts',(3.7365,1.41832075091978,0.121911261685987));
#81595=CARTESIAN_POINT('Ctrl Pts',(3.7365,1.40726488370833,0.178403467845804));
#81596=CARTESIAN_POINT('Ctrl Pts',(3.7365,1.39278238314873,0.234219775072268));
#81597=CARTESIAN_POINT('Ctrl Pts',(3.7365,1.3750275593212,0.289049165597431));
#81598=CARTESIAN_POINT('Ctrl Pts',(3.7365,1.36331774565455,0.325210715424246));
#81599=CARTESIAN_POINT('Ctrl Pts',(3.7365,1.35018350192035,0.360942623635693));
#81600=CARTESIAN_POINT('Ctrl Pts',(3.7365,1.33565892575706,0.396148542417578));
#81601=CARTESIAN_POINT('Ctrl Pts',(3.7365,1.33049266787634,0.408670963265526));
#81602=CARTESIAN_POINT('Ctrl Pts',(3.7365,1.32515044411142,0.421126773855556));
#81603=CARTESIAN_POINT('Ctrl Pts',(3.7365,1.31963357868943,0.433511409073657));
#81604=CARTESIAN_POINT('Ctrl Pts',(3.7365,1.31439779966332,0.445265042407288));
#81605=CARTESIAN_POINT('Ctrl Pts',(3.7365,1.3090038207151,0.456956118390431));
#81606=CARTESIAN_POINT('Ctrl Pts',(3.7365,1.30346243158798,0.468561223712885));
#81607=CARTESIAN_POINT('Ctrl Pts',(3.7365,1.27922239399636,0.519326146157052));
#81608=CARTESIAN_POINT('Ctrl Pts',(3.7365,1.2521280954727,0.568534300549584));
#81609=CARTESIAN_POINT('Ctrl Pts',(3.7365,1.22232167814254,0.615895849808824));
#81610=CARTESIAN_POINT('Ctrl Pts',(3.7365,1.19326257719367,0.662069934596494));
#81611=CARTESIAN_POINT('Ctrl Pts',(3.7365,1.16162489851506,0.706489580149001));
#81612=CARTESIAN_POINT('Ctrl Pts',(3.7365,1.12750665010922,0.74885119383388));
#81613=CARTESIAN_POINT('Ctrl Pts',(3.7365,1.10741856610523,0.773792792362729));
#81614=CARTESIAN_POINT('Ctrl Pts',(3.7365,1.08646998561998,0.798020235695572));
#81615=CARTESIAN_POINT('Ctrl Pts',(3.7365,1.06467675390854,0.821464153697248));
#81616=CARTESIAN_POINT('Ctrl Pts',(3.7365,1.04901069950777,0.838316803164048));
#81617=CARTESIAN_POINT('Ctrl Pts',(3.7365,1.03290811296377,0.854764454447756));
#81618=CARTESIAN_POINT('Ctrl Pts',(3.7365,1.01637411063827,0.870779272925361));
#81619=CARTESIAN_POINT('Ctrl Pts',(3.7365,1.00938013201465,0.877553633778137));
#81620=CARTESIAN_POINT('Ctrl Pts',(3.7365,1.00230930693102,0.884250039088091));
#81621=CARTESIAN_POINT('Ctrl Pts',(3.7365,0.995171997621989,0.890857486243074));
#81622=CARTESIAN_POINT('Ctrl Pts',(3.7365,0.956476284193968,0.926680493279688));
#81623=CARTESIAN_POINT('Ctrl Pts',(3.7365,0.915755145653486,0.959964172630004));
#81624=CARTESIAN_POINT('Ctrl Pts',(3.7365,0.873106335678439,0.990433823056644));
#81625=CARTESIAN_POINT('Ctrl Pts',(3.7365,0.864608521552303,0.996504928580231));
#81626=CARTESIAN_POINT('Ctrl Pts',(3.7365,0.856034094162739,1.00246417157846));
#81627=CARTESIAN_POINT('Ctrl Pts',(3.7365,0.847383710313845,1.00830915591921));
#81628=CARTESIAN_POINT('Ctrl Pts',(3.7365,0.800817662288227,1.0397734037809));
#81629=CARTESIAN_POINT('Ctrl Pts',(3.7365,0.752051536069289,1.06793166378029));
#81630=CARTESIAN_POINT('Ctrl Pts',(3.7365,0.701457004762612,1.09273173067751));
#81631=CARTESIAN_POINT('Ctrl Pts',(3.7365,0.679744688332938,1.10337451925649));
#81632=CARTESIAN_POINT('Ctrl Pts',(3.7365,0.657695506324503,1.1133980690338));
#81633=CARTESIAN_POINT('Ctrl Pts',(3.7365,0.63533868558444,1.12279473411649));
#81634=CARTESIAN_POINT('Ctrl Pts',(3.7365,0.619306521374032,1.12953311965831));
#81635=CARTESIAN_POINT('Ctrl Pts',(3.7365,0.603116157757065,1.13594909322168));
#81636=CARTESIAN_POINT('Ctrl Pts',(3.7365,0.586778487209965,1.14203916526268));
#81637=CARTESIAN_POINT('Ctrl Pts',(3.7365,0.577296942343772,1.14557353028299));
#81638=CARTESIAN_POINT('Ctrl Pts',(3.7365,0.567774044499413,1.14899500605876));
#81639=CARTESIAN_POINT('Ctrl Pts',(3.7365,0.558216209668818,1.15230211828721));
#81640=CARTESIAN_POINT('Ctrl Pts',(3.7365,0.508587976552736,1.16947401333705));
#81641=CARTESIAN_POINT('Ctrl Pts',(3.7365,0.457982493420678,1.1835801791689));
#81642=CARTESIAN_POINT('Ctrl Pts',(3.7365,0.406709608338887,1.1946002349887));
#81643=CARTESIAN_POINT('Ctrl Pts',(3.7365,0.355691719174312,1.2055654846622));
#81644=CARTESIAN_POINT('Ctrl Pts',(3.7365,0.304011857242369,1.21347515766827));
#81645=CARTESIAN_POINT('Ctrl Pts',(3.7365,0.251977513100709,1.21825818903545));
#81646=CARTESIAN_POINT('Ctrl Pts',(3.7365,0.225944148236759,1.2206511931713));
#81647=CARTESIAN_POINT('Ctrl Pts',(3.7365,0.199822199175476,1.2222607723633));
#81648=CARTESIAN_POINT('Ctrl Pts',(3.7365,0.173651787414364,1.2230732991355));
#81649=CARTESIAN_POINT('Ctrl Pts',(3.7365,0.154357834140816,1.2236723288229));
#81650=CARTESIAN_POINT('Ctrl Pts',(3.7365,0.135037563201662,1.2238380736161));
#81651=CARTESIAN_POINT('Ctrl Pts',(3.7365,0.1157076553361,1.22356398342678));
#81652=CARTESIAN_POINT('Ctrl Pts',(3.7365,0.106361568937003,1.22343145974336));
#81653=CARTESIAN_POINT('Ctrl Pts',(3.7365,0.0970142683297624,1.22319601976542));
#81654=CARTESIAN_POINT('Ctrl Pts',(3.7365,0.0876804416350563,1.22285765921622));
#81655=CARTESIAN_POINT('Ctrl Pts',(3.7365,0.0372834290399511,1.2210307171251));
#81656=CARTESIAN_POINT('Ctrl Pts',(3.7365,-0.0128221292937848,1.2162064058474));
#81657=CARTESIAN_POINT('Ctrl Pts',(3.7365,-0.0623571086805372,1.20833476103376));
#81658=CARTESIAN_POINT('Ctrl Pts',(3.7365,-0.110880903841195,1.20062380434732));
#81659=CARTESIAN_POINT('Ctrl Pts',(3.7365,-0.15885808999604,1.18998841684919));
#81660=CARTESIAN_POINT('Ctrl Pts',(3.7365,-0.206006127539271,1.17633630959573));
#81661=CARTESIAN_POINT('Ctrl Pts',(3.7365,-0.253154165082502,1.16268420234226));
#81662=CARTESIAN_POINT('Ctrl Pts',(3.7365,-0.299473974845737,1.14601529259411));
#81663=CARTESIAN_POINT('Ctrl Pts',(3.7365,-0.344648939580368,1.12619366493784));
#81664=CARTESIAN_POINT('Ctrl Pts',(0.248522160579065,-0.510216505388422,
1.06149619882938));
#81665=CARTESIAN_POINT('Ctrl Pts',(0.274946235120132,-0.862691321916517,
0.892076403144088));
#81666=CARTESIAN_POINT('Ctrl Pts',(0.327794384202268,-1.37960057435709,
0.177544609184711));
#81667=CARTESIAN_POINT('Ctrl Pts',(0.407066607825471,-0.89796482962545,
-1.06402462300472));
#81668=CARTESIAN_POINT('Ctrl Pts',(0.486338831448674,0.404638909243713,
-1.33081474323498));
#81669=CARTESIAN_POINT('Ctrl Pts',(0.565611055071876,1.33722609341091,-0.384334478167097));
#81670=CARTESIAN_POINT('Ctrl Pts',(0.644883278695081,1.0493104811472,0.913903580847046));
#81671=CARTESIAN_POINT('Ctrl Pts',(0.724155502318283,-0.196736085198769,
1.37733389209964));
#81672=CARTESIAN_POINT('Ctrl Pts',(0.803427725941487,-1.26308608578749,
0.583572524683419));
#81673=CARTESIAN_POINT('Ctrl Pts',(0.882699949564689,-1.17634997997517,
-0.743087393228864));
#81674=CARTESIAN_POINT('Ctrl Pts',(0.961972173187893,-0.0156437653744218,
-1.39128042313263));
#81675=CARTESIAN_POINT('Ctrl Pts',(1.0412443968111,1.15933180789216,-0.769342143626431));
#81676=CARTESIAN_POINT('Ctrl Pts',(1.1205166204343,1.27590453729514,0.554983829328479));
#81677=CARTESIAN_POINT('Ctrl Pts',(1.1997888440575,0.227639519397196,1.3726288257033));
#81678=CARTESIAN_POINT('Ctrl Pts',(1.2790610676807,-1.02844667848052,0.937140412564534));
#81679=CARTESIAN_POINT('Ctrl Pts',(1.35833329130391,-1.34561567488944,-0.353910979590878));
#81680=CARTESIAN_POINT('Ctrl Pts',(1.43760551492711,-0.434307261820031,
-1.32185870617429));
#81681=CARTESIAN_POINT('Ctrl Pts',(1.51687773855032,0.873500757568272,-1.08301913841129));
#81682=CARTESIAN_POINT('Ctrl Pts',(1.59614996217352,1.38384829755233,0.144560786138938));
#81683=CARTESIAN_POINT('Ctrl Pts',(1.67542218579672,0.630814469109849,1.24016405114351));
#81684=CARTESIAN_POINT('Ctrl Pts',(1.75469440941992,-0.698120020172913,
1.20356234832455));
#81685=CARTESIAN_POINT('Ctrl Pts',(1.83396663304313,-1.38970737331209,0.0681709584735189));
#81686=CARTESIAN_POINT('Ctrl Pts',(1.91323885666633,-0.812564391786863,
-1.12945692909156));
#81687=CARTESIAN_POINT('Ctrl Pts',(1.99251108028953,0.506407483735447,-1.29594958554484));
#81688=CARTESIAN_POINT('Ctrl Pts',(2.07178330391274,1.3630557428063,-0.279307872204986));
#81689=CARTESIAN_POINT('Ctrl Pts',(2.15105552753594,0.975305236911186,0.992327344111197));
#81690=CARTESIAN_POINT('Ctrl Pts',(2.23032775115914,-0.302848092395607,
1.35801948506016));
#81691=CARTESIAN_POINT('Ctrl Pts',(2.30959997478234,-1.30451686139594,0.48391065964775));
#81692=CARTESIAN_POINT('Ctrl Pts',(2.38887219840555,-1.11522989749538,-0.831983297464578));
#81693=CARTESIAN_POINT('Ctrl Pts',(2.46814442202875,0.0922039693498821,
-1.3883200119834));
#81694=CARTESIAN_POINT('Ctrl Pts',(2.54741664565196,1.21546005757808,-0.677192797651213));
#81695=CARTESIAN_POINT('Ctrl Pts',(2.62668886927516,1.22906522301855,0.65217574590713));
#81696=CARTESIAN_POINT('Ctrl Pts',(2.70596109289836,0.120596640913772,1.38614255166615));
#81697=CARTESIAN_POINT('Ctrl Pts',(2.78523331652156,-1.09796786348556,0.854632210191007));
#81698=CARTESIAN_POINT('Ctrl Pts',(2.86450554014477,-1.31414978783895,-0.457110242971296));
#81699=CARTESIAN_POINT('Ctrl Pts',(2.94377776376796,-0.330572392937332,
-1.35153966563246));
#81700=CARTESIAN_POINT('Ctrl Pts',(3.02304998739118,0.954782977733753,-1.01207480386435));
#81701=CARTESIAN_POINT('Ctrl Pts',(3.10232221101437,1.3685043706856,0.251344259488195));
#81702=CARTESIAN_POINT('Ctrl Pts',(3.18159443463759,0.532789731128058,1.28533204040039));
#81703=CARTESIAN_POINT('Ctrl Pts',(3.26086665826078,-0.789214326493944,
1.14581607791232));
#81704=CARTESIAN_POINT('Ctrl Pts',(3.34013888188399,-1.39093495393087,-0.0396509125210518));
#81705=CARTESIAN_POINT('Ctrl Pts',(3.41941110550719,-0.722370214448171,
-1.18914586543665));
#81706=CARTESIAN_POINT('Ctrl Pts',(3.49868332913039,0.60485244622559,-1.25257895798247));
#81707=CARTESIAN_POINT('Ctrl Pts',(3.57795555275359,1.38146769635508,-0.173309657930487));
#81708=CARTESIAN_POINT('Ctrl Pts',(3.6572277763768,0.893721090248042,1.06587168358242));
#81709=CARTESIAN_POINT('Ctrl Pts',(3.71007592545893,0.029308975541542,1.24063596994012));
#81710=CARTESIAN_POINT('Ctrl Pts',(3.7365,-0.344648939580369,1.12619366493784));
#81711=CARTESIAN_POINT('Ctrl Pts',(0.303514773719376,-0.55148003511735,
1.14734422509854));
#81712=CARTESIAN_POINT('Ctrl Pts',(0.329938848260444,-0.932461093440649,
0.964222679857717));
#81713=CARTESIAN_POINT('Ctrl Pts',(0.38278699734258,-1.49117514850909,0.191903449367132));
#81714=CARTESIAN_POINT('Ctrl Pts',(0.462059220965783,-0.970587330174655,
-1.15007713443856));
#81715=CARTESIAN_POINT('Ctrl Pts',(0.541331444588985,0.437363898507531,
-1.4384437853009));
#81716=CARTESIAN_POINT('Ctrl Pts',(0.620603668212189,1.44537365053032,-0.415417355726357));
#81717=CARTESIAN_POINT('Ctrl Pts',(0.699875891835392,1.13417299299545,0.98781512071177));
#81718=CARTESIAN_POINT('Ctrl Pts',(0.779148115458594,-0.212647027347087,
1.4887251493465));
#81719=CARTESIAN_POINT('Ctrl Pts',(0.8584203390818,-1.36523760323283,0.630768689383992));
#81720=CARTESIAN_POINT('Ctrl Pts',(0.937692562705,-1.27148675398718,-0.803184250970361));
#81721=CARTESIAN_POINT('Ctrl Pts',(1.01696478632821,-0.016908947842616,
-1.50379959978589));
#81722=CARTESIAN_POINT('Ctrl Pts',(1.09623700995141,1.25309224491337,-0.831562342463553));
#81723=CARTESIAN_POINT('Ctrl Pts',(1.17550923357461,1.37909274122413,0.599867896187775));
#81724=CARTESIAN_POINT('Ctrl Pts',(1.25478145719781,0.246049762846643,1.48363956282768));
#81725=CARTESIAN_POINT('Ctrl Pts',(1.33405368082102,-1.11162183969917,1.01293122071293));
#81726=CARTESIAN_POINT('Ctrl Pts',(1.41332590444422,-1.45444173562663,-0.382533370425969));
#81727=CARTESIAN_POINT('Ctrl Pts',(1.49259812806742,-0.4694316657159,-1.42876343278274));
#81728=CARTESIAN_POINT('Ctrl Pts',(1.57187035169063,0.944144737324904,-1.17060782271074));
#81729=CARTESIAN_POINT('Ctrl Pts',(1.65114257531383,1.49576640440171,0.156252074510604));
#81730=CARTESIAN_POINT('Ctrl Pts',(1.73041479893703,0.681831304756392,1.34046175937651));
#81731=CARTESIAN_POINT('Ctrl Pts',(1.80968702256024,-0.75458016190203,1.30089991035207));
#81732=CARTESIAN_POINT('Ctrl Pts',(1.88895924618344,-1.50209933027067,0.0736842539900608));
#81733=CARTESIAN_POINT('Ctrl Pts',(1.96823146980664,-0.878280170447616,
-1.22080124876549));
#81734=CARTESIAN_POINT('Ctrl Pts',(2.04750369342985,0.547362960556334,-1.40075892370926));
#81735=CARTESIAN_POINT('Ctrl Pts',(2.12677591705305,1.47329226116953,-0.301896770381618));
#81736=CARTESIAN_POINT('Ctrl Pts',(2.20604814067625,1.05418260801354,1.07258137045515));
#81737=CARTESIAN_POINT('Ctrl Pts',(2.28532036429946,-0.327340795261818,
1.46784869834989));
#81738=CARTESIAN_POINT('Ctrl Pts',(2.36459258792266,-1.41001907413036,0.523046715968235));
#81739=CARTESIAN_POINT('Ctrl Pts',(2.44386481154586,-1.20542361240639,-0.899269571362686));
#81740=CARTESIAN_POINT('Ctrl Pts',(2.52313703516907,0.099660923780427,-1.50059976672033));
#81741=CARTESIAN_POINT('Ctrl Pts',(2.60240925879226,1.31375984147476,-0.731960459698575));
#81742=CARTESIAN_POINT('Ctrl Pts',(2.68168148241547,1.32846531853331,0.704920165179175));
#81743=CARTESIAN_POINT('Ctrl Pts',(2.76095370603867,0.130349839849914,1.49824620528212));
#81744=CARTESIAN_POINT('Ctrl Pts',(2.84022592966187,-1.18676551918244,0.92375020468958));
#81745=CARTESIAN_POINT('Ctrl Pts',(2.91949815328508,-1.42043105915431,-0.494078827681982));
#81746=CARTESIAN_POINT('Ctrl Pts',(2.99877037690828,-0.357307286104204,
-1.46084482644884));
#81747=CARTESIAN_POINT('Ctrl Pts',(3.07804260053149,1.03200062038214,-1.09392589710831));
#81748=CARTESIAN_POINT('Ctrl Pts',(3.15731482415468,1.47918154437085,0.271671613099952));
#81749=CARTESIAN_POINT('Ctrl Pts',(3.23658704777789,0.575878860306533,1.38928268939053));
#81750=CARTESIAN_POINT('Ctrl Pts',(3.31585927140109,-0.853041679156686,
1.23848343636798));
#81751=CARTESIAN_POINT('Ctrl Pts',(3.3951314950243,-1.50342619091827,-0.0428576621857739));
#81752=CARTESIAN_POINT('Ctrl Pts',(3.47440371864751,-0.78079157970072,-1.28531750091348));
#81753=CARTESIAN_POINT('Ctrl Pts',(3.5536759422707,0.653769614982104,-1.35388071620606));
#81754=CARTESIAN_POINT('Ctrl Pts',(3.63294816589391,1.49319327315646,-0.187325998340491));
#81755=CARTESIAN_POINT('Ctrl Pts',(3.71222038951711,0.966000380289331,1.15207357520732));
#81756=CARTESIAN_POINT('Ctrl Pts',(3.76506853859925,0.0316793257180091,
1.34097184439293));
#81757=CARTESIAN_POINT('Ctrl Pts',(3.79149261314031,-0.372522267107456,
1.21727406959531));
#81758=CARTESIAN_POINT('Ctrl Pts',(0.358507386859688,-0.592743564846278,
1.2331922513677));
#81759=CARTESIAN_POINT('Ctrl Pts',(0.384931461400756,-1.00223086496478,
1.03636895657134));
#81760=CARTESIAN_POINT('Ctrl Pts',(0.437779610482891,-1.60274972266108,
0.206262289549554));
#81761=CARTESIAN_POINT('Ctrl Pts',(0.517051834106095,-1.04320983072386,
-1.23612964587239));
#81762=CARTESIAN_POINT('Ctrl Pts',(0.596324057729297,0.470088887771348,
-1.54607282736681));
#81763=CARTESIAN_POINT('Ctrl Pts',(0.675596281352501,1.55352120764973,-0.446500233285617));
#81764=CARTESIAN_POINT('Ctrl Pts',(0.754868504975704,1.21903550484369,1.06172666057649));
#81765=CARTESIAN_POINT('Ctrl Pts',(0.834140728598906,-0.228557969495404,
1.60011640659336));
#81766=CARTESIAN_POINT('Ctrl Pts',(0.913412952222111,-1.46738912067818,
0.677964854084563));
#81767=CARTESIAN_POINT('Ctrl Pts',(0.992685175845312,-1.36662352799918,
-0.863281108711857));
#81768=CARTESIAN_POINT('Ctrl Pts',(1.07195739946852,-0.0181741303108103,
-1.61631877643916));
#81769=CARTESIAN_POINT('Ctrl Pts',(1.15122962309172,1.34685268193457,-0.893782541300675));
#81770=CARTESIAN_POINT('Ctrl Pts',(1.23050184671492,1.48228094515312,0.64475196304707));
#81771=CARTESIAN_POINT('Ctrl Pts',(1.30977407033813,0.264460006296089,1.59465029995206));
#81772=CARTESIAN_POINT('Ctrl Pts',(1.38904629396133,-1.19479700091782,1.08872202886133));
#81773=CARTESIAN_POINT('Ctrl Pts',(1.46831851758453,-1.56326779636382,-0.411155761261059));
#81774=CARTESIAN_POINT('Ctrl Pts',(1.54759074120773,-0.504556069611769,
-1.53566815939119));
#81775=CARTESIAN_POINT('Ctrl Pts',(1.62686296483094,1.01478871708154,-1.25819650701018));
#81776=CARTESIAN_POINT('Ctrl Pts',(1.70613518845414,1.6076845112511,0.16794336288227));
#81777=CARTESIAN_POINT('Ctrl Pts',(1.78540741207735,0.732848140402935,1.44075946760951));
#81778=CARTESIAN_POINT('Ctrl Pts',(1.86467963570055,-0.811040303631148,
1.39823747237959));
#81779=CARTESIAN_POINT('Ctrl Pts',(1.94395185932375,-1.61449128722926,0.0791975495066015));
#81780=CARTESIAN_POINT('Ctrl Pts',(2.02322408294695,-0.943995949108369,
-1.31214556843942));
#81781=CARTESIAN_POINT('Ctrl Pts',(2.10249630657016,0.58831843737722,-1.50556826187368));
#81782=CARTESIAN_POINT('Ctrl Pts',(2.18176853019336,1.58352877953276,-0.32448566855825));
#81783=CARTESIAN_POINT('Ctrl Pts',(2.26104075381656,1.13305997911589,1.1528353967991));
#81784=CARTESIAN_POINT('Ctrl Pts',(2.34031297743977,-0.351833498128028,
1.57767791163962));
#81785=CARTESIAN_POINT('Ctrl Pts',(2.41958520106297,-1.51552128686477,0.56218277228872));
#81786=CARTESIAN_POINT('Ctrl Pts',(2.49885742468617,-1.2956173273174,-0.966555845260797));
#81787=CARTESIAN_POINT('Ctrl Pts',(2.57812964830937,0.107117878210971,-1.61287952145726));
#81788=CARTESIAN_POINT('Ctrl Pts',(2.65740187193258,1.41205962537143,-0.786728121745937));
#81789=CARTESIAN_POINT('Ctrl Pts',(2.73667409555578,1.42786541404808,0.75766458445122));
#81790=CARTESIAN_POINT('Ctrl Pts',(2.81594631917899,0.140103038786054,1.61034985889808));
#81791=CARTESIAN_POINT('Ctrl Pts',(2.89521854280218,-1.27556317487932,0.992868199188152));
#81792=CARTESIAN_POINT('Ctrl Pts',(2.9744907664254,-1.52671233046967,-0.531047412392669));
#81793=CARTESIAN_POINT('Ctrl Pts',(3.05376299004859,-0.384042179271076,
-1.57014998726522));
#81794=CARTESIAN_POINT('Ctrl Pts',(3.1330352136718,1.10921826303053,-1.17577699035228));
#81795=CARTESIAN_POINT('Ctrl Pts',(3.212307437295,1.58985871805611,0.291998966711711));
#81796=CARTESIAN_POINT('Ctrl Pts',(3.2915796609182,0.61896798948501,1.49323333838066));
#81797=CARTESIAN_POINT('Ctrl Pts',(3.37085188454141,-0.91686903181943,1.33115079482364));
#81798=CARTESIAN_POINT('Ctrl Pts',(3.45012410816461,-1.61591742790568,-0.0460644118504966));
#81799=CARTESIAN_POINT('Ctrl Pts',(3.52939633178781,-0.83921294495327,-1.38148913639031));
#81800=CARTESIAN_POINT('Ctrl Pts',(3.60866855541102,0.702686783738618,-1.45518247442965));
#81801=CARTESIAN_POINT('Ctrl Pts',(3.68794077903422,1.60491884995784,-0.201342338750495));
#81802=CARTESIAN_POINT('Ctrl Pts',(3.76721300265742,1.03827967033062,1.23827546683221));
#81803=CARTESIAN_POINT('Ctrl Pts',(3.82006115173956,0.0340496758944771,
1.44130771884574));
#81804=CARTESIAN_POINT('Ctrl Pts',(3.84648522628063,-0.400395594634544,
1.30835447425277));
#81805=CARTESIAN_POINT('Ctrl Pts',(0.4135,-0.634007094575206,1.31904027763685));
#81806=CARTESIAN_POINT('Ctrl Pts',(0.439924074541068,-1.07200063648891,
1.10851523328497));
#81807=CARTESIAN_POINT('Ctrl Pts',(0.492772223623203,-1.71432429681307,
0.220621129731974));
#81808=CARTESIAN_POINT('Ctrl Pts',(0.572044447246407,-1.11583233127307,
-1.32218215730623));
#81809=CARTESIAN_POINT('Ctrl Pts',(0.651316670869609,0.502813877035165,
-1.65370186943273));
#81810=CARTESIAN_POINT('Ctrl Pts',(0.730588894492813,1.66166876476914,-0.477583110844877));
#81811=CARTESIAN_POINT('Ctrl Pts',(0.809861118116016,1.30389801669194,1.13563820044122));
#81812=CARTESIAN_POINT('Ctrl Pts',(0.889133341739219,-0.244468911643721,
1.71150766384022));
#81813=CARTESIAN_POINT('Ctrl Pts',(0.968405565362422,-1.56954063812352,
0.725161018785134));
#81814=CARTESIAN_POINT('Ctrl Pts',(1.04767778898562,-1.46176030201119,-0.923377966453352));
#81815=CARTESIAN_POINT('Ctrl Pts',(1.12695001260883,-0.0194393127790041,
-1.72883795309242));
#81816=CARTESIAN_POINT('Ctrl Pts',(1.20622223623203,1.44061311895578,-0.956002740137796));
#81817=CARTESIAN_POINT('Ctrl Pts',(1.28549445985524,1.5854691490821,0.689636029906365));
#81818=CARTESIAN_POINT('Ctrl Pts',(1.36476668347844,0.282870249745534,1.70566103707644));
#81819=CARTESIAN_POINT('Ctrl Pts',(1.44403890710164,-1.27797216213648,1.16451283700972));
#81820=CARTESIAN_POINT('Ctrl Pts',(1.52331113072484,-1.672093857101,-0.439778152096151));
#81821=CARTESIAN_POINT('Ctrl Pts',(1.60258335434805,-0.53968047350764,-1.64257288599964));
#81822=CARTESIAN_POINT('Ctrl Pts',(1.68185557797125,1.08543269683817,-1.34578519130964));
#81823=CARTESIAN_POINT('Ctrl Pts',(1.76112780159445,1.71960261810048,0.179634651253938));
#81824=CARTESIAN_POINT('Ctrl Pts',(1.84040002521766,0.783864976049478,1.54105717584251));
#81825=CARTESIAN_POINT('Ctrl Pts',(1.91967224884086,-0.867500445360263,
1.49557503440711));
#81826=CARTESIAN_POINT('Ctrl Pts',(1.99894447246407,-1.72688324418785,0.0847108450231425));
#81827=CARTESIAN_POINT('Ctrl Pts',(2.07821669608726,-1.00971172776912,-1.40348988811335));
#81828=CARTESIAN_POINT('Ctrl Pts',(2.15748891971047,0.629273914198106,-1.6103776000381));
#81829=CARTESIAN_POINT('Ctrl Pts',(2.23676114333367,1.693765297896,-0.347074566734881));
#81830=CARTESIAN_POINT('Ctrl Pts',(2.31603336695688,1.21193735021824,1.23308942314305));
#81831=CARTESIAN_POINT('Ctrl Pts',(2.39530559058007,-0.376326200994238,
1.68750712492935));
#81832=CARTESIAN_POINT('Ctrl Pts',(2.47457781420328,-1.62102349959919,0.601318828609204));
#81833=CARTESIAN_POINT('Ctrl Pts',(2.55385003782648,-1.3858110422284,-1.03384211915891));
#81834=CARTESIAN_POINT('Ctrl Pts',(2.63312226144969,0.114574832641515,-1.72515927619419));
#81835=CARTESIAN_POINT('Ctrl Pts',(2.71239448507289,1.51035940926811,-0.8414957837933));
#81836=CARTESIAN_POINT('Ctrl Pts',(2.79166670869609,1.52726550956285,0.810409003723266));
#81837=CARTESIAN_POINT('Ctrl Pts',(2.8709389323193,0.149856237722195,1.72245351251404));
#81838=CARTESIAN_POINT('Ctrl Pts',(2.9502111559425,-1.3643608305762,1.06198619368673));
#81839=CARTESIAN_POINT('Ctrl Pts',(3.0294833795657,-1.63299360178502,-0.568015997103359));
#81840=CARTESIAN_POINT('Ctrl Pts',(3.10875560318891,-0.410777072437948,
-1.6794551480816));
#81841=CARTESIAN_POINT('Ctrl Pts',(3.1880278268121,1.18643590567891,-1.25762808359624));
#81842=CARTESIAN_POINT('Ctrl Pts',(3.26730005043532,1.70053589174136,0.312326320323468));
#81843=CARTESIAN_POINT('Ctrl Pts',(3.34657227405851,0.662057118663487,1.5971839873708));
#81844=CARTESIAN_POINT('Ctrl Pts',(3.42584449768172,-0.980696384482174,
1.42381815327929));
#81845=CARTESIAN_POINT('Ctrl Pts',(3.50511672130492,-1.72840866489308,-0.0492711615152196));
#81846=CARTESIAN_POINT('Ctrl Pts',(3.58438894492813,-0.89763431020582,-1.47766077186714));
#81847=CARTESIAN_POINT('Ctrl Pts',(3.66366116855132,0.751603952495131,-1.55648423265323));
#81848=CARTESIAN_POINT('Ctrl Pts',(3.74293339217453,1.71664442675922,-0.215358679160498));
#81849=CARTESIAN_POINT('Ctrl Pts',(3.82220561579773,1.11055896037191,1.32447735845711));
#81850=CARTESIAN_POINT('Ctrl Pts',(3.87505376487987,0.0364200260709443,
1.54164359329855));
#81851=CARTESIAN_POINT('Ctrl Pts',(3.90147783942094,-0.428268922161632,
1.39943487891024));
#81852=CARTESIAN_POINT('Ctrl Pts',(3.50284495415709,-1.4658722466537,-0.00023313482661453));
#81853=CARTESIAN_POINT('Ctrl Pts',(3.50360220987304,-1.46590495726483,-0.0140984294436677));
#81854=CARTESIAN_POINT('Ctrl Pts',(3.50435946558898,-1.46572428836199,-0.0279628793168609));
#81855=CARTESIAN_POINT('Ctrl Pts',(3.50511672130492,-1.46532755904339,-0.0418212107747877));
#81856=CARTESIAN_POINT('Ctrl Pts',(3.53154079584599,-1.45148387999733,-0.525401031632525));
#81857=CARTESIAN_POINT('Ctrl Pts',(3.55796487038706,-1.17455909510157,-1.00153090174984));
#81858=CARTESIAN_POINT('Ctrl Pts',(3.58438894492813,-0.761223658870205,
-1.25273308027284));
#81859=CARTESIAN_POINT('Ctrl Pts',(3.61081301946919,-0.347888222638836,
-1.50393525879584));
#81860=CARTESIAN_POINT('Ctrl Pts',(3.63723709401026,0.201857864928146,-1.53020974572454));
#81861=CARTESIAN_POINT('Ctrl Pts',(3.66366116855133,0.637570987755653,-1.31982606360676));
#81862=CARTESIAN_POINT('Ctrl Pts',(3.68794077903422,1.0379235105316,-1.12651621482333));
#81863=CARTESIAN_POINT('Ctrl Pts',(3.71222038951711,1.3420008677259,-0.73340182300052));
#81864=CARTESIAN_POINT('Ctrl Pts',(3.7365,1.43512958320548,-0.29838030867994));
#81865=CARTESIAN_POINT('',(0.4135,-0.684664424539457,-0.958295198918399));
#81866=CARTESIAN_POINT('Ctrl Pts',(0.4135,-0.686138785896735,-0.95953609754738));
#81867=CARTESIAN_POINT('Ctrl Pts',(0.4135,-0.714291760736759,-0.944234963869998));
#81868=CARTESIAN_POINT('Ctrl Pts',(0.4135,-0.741719807224122,-0.927747538280581));
#81869=CARTESIAN_POINT('Ctrl Pts',(0.4135,-0.768338120235236,-0.910091316634728));
#81870=CARTESIAN_POINT('Ctrl Pts',(0.4135,-0.808566078090619,-0.883407666924919));
#81871=CARTESIAN_POINT('Ctrl Pts',(0.4135,-0.846946021796831,-0.854057054820037));
#81872=CARTESIAN_POINT('Ctrl Pts',(0.4135,-0.883406381928383,-0.822336436728148));
#81873=CARTESIAN_POINT('Ctrl Pts',(0.4135,-0.900931220434468,-0.807089776866099));
#81874=CARTESIAN_POINT('Ctrl Pts',(0.4135,-0.918012314882335,-0.791294839075063));
#81875=CARTESIAN_POINT('Ctrl Pts',(0.4135,-0.934639962853447,-0.774980866858151));
#81876=CARTESIAN_POINT('Ctrl Pts',(0.4135,-0.941832779854533,-0.767923740262681));
#81877=CARTESIAN_POINT('Ctrl Pts',(0.4135,-0.948939652538661,-0.760770400163592));
#81878=CARTESIAN_POINT('Ctrl Pts',(0.4135,-0.955953136700092,-0.75353039471608));
#81879=CARTESIAN_POINT('Ctrl Pts',(0.4135,-0.991151160285013,-0.717195546496428));
#81880=CARTESIAN_POINT('Ctrl Pts',(0.4135,-1.02404693575632,-0.67863524199184));
#81881=CARTESIAN_POINT('Ctrl Pts',(0.4135,-1.05456130615998,-0.638174593980841));
#81882=CARTESIAN_POINT('Ctrl Pts',(0.4135,-1.07623986056963,-0.609429830521755));
#81883=CARTESIAN_POINT('Ctrl Pts',(0.4135,-1.09671609730046,-0.57972473829133));
#81884=CARTESIAN_POINT('Ctrl Pts',(0.4135,-1.11595336287888,-0.549162386019891));
#81885=CARTESIAN_POINT('Ctrl Pts',(0.4135,-1.12342713252684,-0.537288766048001));
#81886=CARTESIAN_POINT('Ctrl Pts',(0.4135,-1.13071381256276,-0.525285650206696));
#81887=CARTESIAN_POINT('Ctrl Pts',(0.4135,-1.13781091071671,-0.51315871424196));
#81888=CARTESIAN_POINT('Ctrl Pts',(0.4135,-1.14293138389033,-0.504409272013786));
#81889=CARTESIAN_POINT('Ctrl Pts',(0.4135,-1.14795098786502,-0.495598970025009));
#81890=CARTESIAN_POINT('Ctrl Pts',(0.4135,-1.15286514594592,-0.486737318018312));
#81891=CARTESIAN_POINT('Ctrl Pts',(0.4135,-1.17834338405788,-0.440792666630386));
#81892=CARTESIAN_POINT('Ctrl Pts',(0.4135,-1.20102252315539,-0.393415091402672));
#81893=CARTESIAN_POINT('Ctrl Pts',(0.4135,-1.22081814050263,-0.344933777036805));
#81894=CARTESIAN_POINT('Ctrl Pts',(0.4135,-1.24097727802828,-0.295562167827453));
#81895=CARTESIAN_POINT('Ctrl Pts',(0.4135,-1.25814678940821,-0.245045016208608));
#81896=CARTESIAN_POINT('Ctrl Pts',(0.4135,-1.27220121508717,-0.193691330378271));
#81897=CARTESIAN_POINT('Ctrl Pts',(0.4135,-1.28026843106556,-0.164214403725913));
#81898=CARTESIAN_POINT('Ctrl Pts',(0.4135,-1.28730858055556,-0.134461223038789));
#81899=CARTESIAN_POINT('Ctrl Pts',(0.4135,-1.29329114713789,-0.104486455012093));
#81900=CARTESIAN_POINT('Ctrl Pts',(0.4135,-1.29665686867299,-0.0876230033699474));
#81901=CARTESIAN_POINT('Ctrl Pts',(0.4135,-1.29968776382401,-0.0706893780411438));
#81902=CARTESIAN_POINT('Ctrl Pts',(0.4135,-1.30237760820265,-0.0536950834617746));
#81903=CARTESIAN_POINT('Ctrl Pts',(0.4135,-1.30392796078445,-0.0439000378129977));
#81904=CARTESIAN_POINT('Ctrl Pts',(0.4135,-1.30536494097996,-0.0340844664323464));
#81905=CARTESIAN_POINT('Ctrl Pts',(0.4135,-1.30668555024684,-0.0242654228606041));
#81906=CARTESIAN_POINT('Ctrl Pts',(0.4135,-1.31399180339102,0.0300583046551521));
#81907=CARTESIAN_POINT('Ctrl Pts',(0.4135,-1.3177582625026,0.0845978055922513));
#81908=CARTESIAN_POINT('Ctrl Pts',(0.4135,-1.31787095116813,0.139023202239183));
#81909=CARTESIAN_POINT('Ctrl Pts',(0.4135,-1.31789100087815,0.148706637709421));
#81910=CARTESIAN_POINT('Ctrl Pts',(0.4135,-1.317795273435,0.158386530765053));
#81911=CARTESIAN_POINT('Ctrl Pts',(0.4135,-1.31758297383669,0.16806110450681));
#81912=CARTESIAN_POINT('Ctrl Pts',(0.4135,-1.31643127886986,0.220544283812512));
#81913=CARTESIAN_POINT('Ctrl Pts',(0.4135,-1.31185321745701,0.272870263476887));
#81914=CARTESIAN_POINT('Ctrl Pts',(0.4135,-1.30405110481389,0.324821294688041));
#81915=CARTESIAN_POINT('Ctrl Pts',(0.4135,-1.30004755732558,0.351479256452338));
#81916=CARTESIAN_POINT('Ctrl Pts',(0.4135,-1.29519424013352,0.378038631051489));
#81917=CARTESIAN_POINT('Ctrl Pts',(0.4135,-1.28951334705064,0.404470290630908));
#81918=CARTESIAN_POINT('Ctrl Pts',(0.4135,-1.28605512944955,0.420560442135318));
#81919=CARTESIAN_POINT('Ctrl Pts',(0.4135,-1.28229017007228,0.436603265746692));
#81920=CARTESIAN_POINT('Ctrl Pts',(0.4135,-1.27822287787089,0.452592132714455));
#81921=CARTESIAN_POINT('Ctrl Pts',(0.4135,-1.27553847269057,0.463144754751541));
#81922=CARTESIAN_POINT('Ctrl Pts',(0.4135,-1.27272184329057,0.473675296709342));
#81923=CARTESIAN_POINT('Ctrl Pts',(0.4135,-1.26977956742198,0.48416381510515));
#81924=CARTESIAN_POINT('Ctrl Pts',(0.4135,-1.25497166843981,0.536950476796429));
#81925=CARTESIAN_POINT('Ctrl Pts',(0.4135,-1.23696085773443,0.588774472230241));
#81926=CARTESIAN_POINT('Ctrl Pts',(0.4135,-1.21598695973147,0.639400292991206));
#81927=CARTESIAN_POINT('Ctrl Pts',(0.4135,-1.19455580907984,0.691129808956144));
#81928=CARTESIAN_POINT('Ctrl Pts',(0.4135,-1.17003074758714,0.741609292791885));
#81929=CARTESIAN_POINT('Ctrl Pts',(0.4135,-1.1426126898322,0.790587857943637));
#81930=CARTESIAN_POINT('Ctrl Pts',(0.4135,-1.12720475153753,0.818112007041462));
#81931=CARTESIAN_POINT('Ctrl Pts',(0.4135,-1.11088223265367,0.845162088565469));
#81932=CARTESIAN_POINT('Ctrl Pts',(0.4135,-1.09367386201465,0.871691839113621));
#81933=CARTESIAN_POINT('Ctrl Pts',(0.4135,-1.08240277099321,0.889068221775127));
#81934=CARTESIAN_POINT('Ctrl Pts',(0.4135,-1.07075155454919,0.90622135373255));
#81935=CARTESIAN_POINT('Ctrl Pts',(0.4135,-1.05872722186107,0.923137718332686));
#81936=CARTESIAN_POINT('Ctrl Pts',(0.4135,-1.05266396799753,0.931667772821302));
#81937=CARTESIAN_POINT('Ctrl Pts',(0.4135,-1.04650431325987,0.940139649745939));
#81938=CARTESIAN_POINT('Ctrl Pts',(0.4135,-1.04025403002402,0.948544932930425));
#81939=CARTESIAN_POINT('Ctrl Pts',(0.4135,-1.00551853942241,0.995256677669289));
#81940=CARTESIAN_POINT('Ctrl Pts',(0.4135,-0.968096092333637,1.03977033457125));
#81941=CARTESIAN_POINT('Ctrl Pts',(0.4135,-0.928214711176929,1.08182781872808));
#81942=CARTESIAN_POINT('Ctrl Pts',(0.4135,-0.888231183206945,1.12399302327614));
#81943=CARTESIAN_POINT('Ctrl Pts',(0.4135,-0.845775625163952,1.16369052758893));
#81944=CARTESIAN_POINT('Ctrl Pts',(0.4135,-0.801028754132348,1.20064269443073));
#81945=CARTESIAN_POINT('Ctrl Pts',(0.4135,-0.757313300281664,1.23674311233737));
#81946=CARTESIAN_POINT('Ctrl Pts',(0.4135,-0.711410323916766,1.27022418935027));
#81947=CARTESIAN_POINT('Ctrl Pts',(0.4135,-0.663450030477264,1.30079597351158));
#81948=CARTESIAN_POINT('Ctrl Pts',(0.4135,-0.653720195627844,1.30699815430759));
#81949=CARTESIAN_POINT('Ctrl Pts',(0.4135,-0.64390557580449,1.3130804666773));
#81950=CARTESIAN_POINT('Ctrl Pts',(0.4135,-0.634007094575209,1.31904027763685));
#81951=CARTESIAN_POINT('Ctrl Pts',(0.4135,-0.68613878589674,-0.959536097547376));
#81952=CARTESIAN_POINT('Ctrl Pts',(0.437779610482891,-0.393693948037641,
-1.16605720471058));
#81953=CARTESIAN_POINT('Ctrl Pts',(0.488483295506851,0.429867162043437,
-1.3052106562365));
#81954=CARTESIAN_POINT('Ctrl Pts',(0.565611055071876,1.33722609341091,-0.384334478167097));
#81955=CARTESIAN_POINT('Ctrl Pts',(0.644883278695081,1.0493104811472,0.913903580847046));
#81956=CARTESIAN_POINT('Ctrl Pts',(0.724155502318283,-0.196736085198769,
1.37733389209964));
#81957=CARTESIAN_POINT('Ctrl Pts',(0.78848344766531,-1.06205941565968,0.733211202865703));
#81958=CARTESIAN_POINT('Ctrl Pts',(0.826387318471269,-1.1764950713461,0.170924181182572));
#81959=CARTESIAN_POINT('Ctrl Pts',(0.837867114736159,-1.17596232425638,
0.000418044704970002));
#81960=CARTESIAN_POINT('Origin',(0.4135,-3.28582941601228E-17,0.));
#81961=CARTESIAN_POINT('',(0.4135,-1.4635,-1.79227059055215E-16));
#81962=CARTESIAN_POINT('Origin',(0.4135,0.,0.));
#81963=CARTESIAN_POINT('Origin',(0.4135,0.,0.));
#81964=CARTESIAN_POINT('',(0.4135,0.684664424539459,-0.958295198918398));
#81965=CARTESIAN_POINT('Ctrl Pts',(0.4135,0.635547413990925,1.32087379520599));
#81966=CARTESIAN_POINT('Ctrl Pts',(0.4135,0.669353330290829,1.30074697282028));
#81967=CARTESIAN_POINT('Ctrl Pts',(0.4135,0.702232179962959,1.27920433805169));
#81968=CARTESIAN_POINT('Ctrl Pts',(0.4135,0.734081619959607,1.2562406920021));
#81969=CARTESIAN_POINT('Ctrl Pts',(0.4135,0.780755752573622,1.22258834957055));
#81970=CARTESIAN_POINT('Ctrl Pts',(0.4135,0.825221151134185,1.18588514692087));
#81971=CARTESIAN_POINT('Ctrl Pts',(0.4135,0.8673274179155,1.14644100535051));
#81972=CARTESIAN_POINT('Ctrl Pts',(0.4135,0.881456789981801,1.13320494823394));
#81973=CARTESIAN_POINT('Ctrl Pts',(0.4135,0.895320162781675,1.11966001938105));
#81974=CARTESIAN_POINT('Ctrl Pts',(0.4135,0.908910741618978,1.10581733905333));
#81975=CARTESIAN_POINT('Ctrl Pts',(0.4135,0.917246814053772,1.09732663477318));
#81976=CARTESIAN_POINT('Ctrl Pts',(0.4135,0.925480243365935,1.08872390441625));
#81977=CARTESIAN_POINT('Ctrl Pts',(0.4135,0.933609350058259,1.08001167838196));
#81978=CARTESIAN_POINT('Ctrl Pts',(0.4135,0.942209207594102,1.07079493347373));
#81979=CARTESIAN_POINT('Ctrl Pts',(0.4135,0.950686065026906,1.06146229962268));
#81980=CARTESIAN_POINT('Ctrl Pts',(0.4135,0.95903640633612,1.05201957849277));
#81981=CARTESIAN_POINT('Ctrl Pts',(0.4135,0.997169509051934,1.00889795730031));
#81982=CARTESIAN_POINT('Ctrl Pts',(0.4135,1.03268280360029,0.963466516297889));
#81983=CARTESIAN_POINT('Ctrl Pts',(0.4135,1.06542315300417,0.916036856053426));
#81984=CARTESIAN_POINT('Ctrl Pts',(0.4135,1.08701635006398,0.884755638266009));
#81985=CARTESIAN_POINT('Ctrl Pts',(0.4135,1.10740246223309,0.852604627640892));
#81986=CARTESIAN_POINT('Ctrl Pts',(0.4135,1.12652571878095,0.819669470930706));
#81987=CARTESIAN_POINT('Ctrl Pts',(0.4135,1.13332764876214,0.807954801449515));
#81988=CARTESIAN_POINT('Ctrl Pts',(0.4135,1.13996971756187,0.796140912143825));
#81989=CARTESIAN_POINT('Ctrl Pts',(0.4135,1.14644910558472,0.78423162968392));
#81990=CARTESIAN_POINT('Ctrl Pts',(0.4135,1.15259842154092,0.772929028203779));
#81991=CARTESIAN_POINT('Ctrl Pts',(0.4135,1.15860189203148,0.761538847236137));
#81992=CARTESIAN_POINT('Ctrl Pts',(0.4135,1.16444748634856,0.750083887702724));
#81993=CARTESIAN_POINT('Ctrl Pts',(0.4135,1.19001813114109,0.699975945643586));
#81994=CARTESIAN_POINT('Ctrl Pts',(0.4135,1.21261752532289,0.648548155053135));
#81995=CARTESIAN_POINT('Ctrl Pts',(0.4135,1.2321019520388,0.596089578702456));
#81996=CARTESIAN_POINT('Ctrl Pts',(0.4135,1.25109784966556,0.544946285623718));
#81997=CARTESIAN_POINT('Ctrl Pts',(0.4135,1.26713314523672,0.492822207443129));
#81998=CARTESIAN_POINT('Ctrl Pts',(0.4135,1.28002636999895,0.439979726788032));
#81999=CARTESIAN_POINT('Ctrl Pts',(0.4135,1.28761762878201,0.408867188785392));
#82000=CARTESIAN_POINT('Ctrl Pts',(0.4135,1.29411873111552,0.37750558303088));
#82001=CARTESIAN_POINT('Ctrl Pts',(0.4135,1.2994842302109,0.345949663324928));
#82002=CARTESIAN_POINT('Ctrl Pts',(0.4135,1.3033411938025,0.323265840023198));
#82003=CARTESIAN_POINT('Ctrl Pts',(0.4135,1.30661121725092,0.300481627400674));
#82004=CARTESIAN_POINT('Ctrl Pts',(0.4135,1.30927531071834,0.277618009171112));
#82005=CARTESIAN_POINT('Ctrl Pts',(0.4135,1.31040225052168,0.267946456071913));
#82006=CARTESIAN_POINT('Ctrl Pts',(0.4135,1.31142057568754,0.258261278874394));
#82007=CARTESIAN_POINT('Ctrl Pts',(0.4135,1.31232784965945,0.248577394511979));
#82008=CARTESIAN_POINT('Ctrl Pts',(0.4135,1.31724670409264,0.19607548329048));
#82009=CARTESIAN_POINT('Ctrl Pts',(0.4135,1.31891803803387,0.143509146220101));
#82010=CARTESIAN_POINT('Ctrl Pts',(0.4135,1.3171831677328,0.0911229999231752));
#82011=CARTESIAN_POINT('Ctrl Pts',(0.4135,1.31683748835986,0.0806848650426602));
#82012=CARTESIAN_POINT('Ctrl Pts',(0.4135,1.31635641176535,0.0702539051829255));
#82013=CARTESIAN_POINT('Ctrl Pts',(0.4135,1.31573843466204,0.059832098621419));
#82014=CARTESIAN_POINT('Ctrl Pts',(0.4135,1.31241181507788,0.00373069029382706));
#82015=CARTESIAN_POINT('Ctrl Pts',(0.4135,1.3051227222334,-0.0521077326158235));
#82016=CARTESIAN_POINT('Ctrl Pts',(0.4135,1.29405566219162,-0.107356325259506));
#82017=CARTESIAN_POINT('Ctrl Pts',(0.4135,1.28930638402934,-0.1310655066996));
#82018=CARTESIAN_POINT('Ctrl Pts',(0.4135,1.28386065917644,-0.154665702263389));
#82019=CARTESIAN_POINT('Ctrl Pts',(0.4135,1.27773018452238,-0.178129059070878));
#82020=CARTESIAN_POINT('Ctrl Pts',(0.4135,1.27333395871588,-0.194954871185749));
#82021=CARTESIAN_POINT('Ctrl Pts',(0.413500000000001,1.26858556750922,-0.21171028751553));
#82022=CARTESIAN_POINT('Ctrl Pts',(0.413500000000001,1.26348886213856,-0.228384538292229));
#82023=CARTESIAN_POINT('Ctrl Pts',(0.413500000000001,1.26053100374918,-0.238061392055544));
#82024=CARTESIAN_POINT('Ctrl Pts',(0.4135,1.25745837360604,-0.247702450741358));
#82025=CARTESIAN_POINT('Ctrl Pts',(0.4135,1.25427370148489,-0.257301724258028));
#82026=CARTESIAN_POINT('Ctrl Pts',(0.4135,1.23773749554111,-0.30714533695771));
#82027=CARTESIAN_POINT('Ctrl Pts',(0.413500000000001,1.21817302763353,-0.35590112182507));
#82028=CARTESIAN_POINT('Ctrl Pts',(0.413500000000001,1.19575248320236,-0.403310675257065));
#82029=CARTESIAN_POINT('Ctrl Pts',(0.413500000000001,1.17344343049265,-0.45048447291861));
#82030=CARTESIAN_POINT('Ctrl Pts',(0.4135,1.14830584182414,-0.496326289088077));
#82031=CARTESIAN_POINT('Ctrl Pts',(0.4135,1.12047022689924,-0.540548779036441));
#82032=CARTESIAN_POINT('Ctrl Pts',(0.4135,1.1065437748044,-0.562673757753156));
#82033=CARTESIAN_POINT('Ctrl Pts',(0.413500000000001,1.09194143893574,-0.584392804363012));
#82034=CARTESIAN_POINT('Ctrl Pts',(0.413500000000001,1.07667679045606,-0.605665778680436));
#82035=CARTESIAN_POINT('Ctrl Pts',(0.413500000000001,1.06542302105988,-0.621349149814594));
#82036=CARTESIAN_POINT('Ctrl Pts',(0.413500000000001,1.05380922812795,-0.636790009908271));
#82037=CARTESIAN_POINT('Ctrl Pts',(0.413500000000001,1.04184035177154,-0.651971132742421));
#82038=CARTESIAN_POINT('Ctrl Pts',(0.413500000000001,1.03605335611918,-0.659311261357929));
#82039=CARTESIAN_POINT('Ctrl Pts',(0.4135,1.03018390785768,-0.666589788171434));
#82040=CARTESIAN_POINT('Ctrl Pts',(0.4135,1.02424093292914,-0.673795048425256));
#82041=CARTESIAN_POINT('Ctrl Pts',(0.4135,0.992152443281526,-0.712699119507982));
#82042=CARTESIAN_POINT('Ctrl Pts',(0.4135,0.957861254279335,-0.749549587746932));
#82043=CARTESIAN_POINT('Ctrl Pts',(0.4135,0.921497384787766,-0.78409445806545));
#82044=CARTESIAN_POINT('Ctrl Pts',(0.4135,0.885875868446326,-0.817934109339342));
#82045=CARTESIAN_POINT('Ctrl Pts',(0.4135,0.848264687334309,-0.849561915469862));
#82046=CARTESIAN_POINT('Ctrl Pts',(0.4135,0.808762330645478,-0.87869744037182));
#82047=CARTESIAN_POINT('Ctrl Pts',(0.4135,0.769259973956647,-0.907832965273778));
#82048=CARTESIAN_POINT('Ctrl Pts',(0.4135,0.727865816193214,-0.934476889771254));
#82049=CARTESIAN_POINT('Ctrl Pts',(0.4135,0.684664424539464,-0.958295198918394));
#82050=CARTESIAN_POINT('Origin',(0.4135,0.,0.));
#82051=CARTESIAN_POINT('Origin',(-0.510867114736157,0.,0.));
#82052=CARTESIAN_POINT('Ctrl Pts',(0.4135,0.68466442453946,-0.958295198918397));
#82053=CARTESIAN_POINT('Ctrl Pts',(0.439924074541068,1.00287086257571,-0.730949149362124));
#82054=CARTESIAN_POINT('Ctrl Pts',(0.492772223623204,1.38961280228995,0.0616289067023483));
#82055=CARTESIAN_POINT('Ctrl Pts',(0.572044447246405,0.702229323936485,
1.20223305857378));
#82056=CARTESIAN_POINT('Ctrl Pts',(0.65131667086961,-0.626827250790123,
1.2417271038667));
#82057=CARTESIAN_POINT('Ctrl Pts',(0.707012816875422,-1.15833492858927,
0.474239310809062));
#82058=CARTESIAN_POINT('Ctrl Pts',(0.736284888340166,-1.17941005150351,
0.0427943559881212));
#82059=CARTESIAN_POINT('Ctrl Pts',(0.739132885263843,-1.17911213255423,
0.000786107540026912));
#82060=CARTESIAN_POINT('Ctrl Pts',(0.248522160579064,0.850780204044571,
-1.1908002747757));
#82061=CARTESIAN_POINT('Ctrl Pts',(0.274946235120132,1.24619104850736,-0.90829469759412));
#82062=CARTESIAN_POINT('Ctrl Pts',(0.327794384202267,1.72676572799944,0.0765815367937832));
#82063=CARTESIAN_POINT('Ctrl Pts',(0.407066607825471,0.872606763388711,
1.49392322752938));
#82064=CARTESIAN_POINT('Ctrl Pts',(0.486338831448673,-0.778910364280483,
1.54299946211752));
#82065=CARTESIAN_POINT('Ctrl Pts',(0.565611055071877,-1.71894759058321,
0.185602144369403));
#82066=CARTESIAN_POINT('Ctrl Pts',(0.64488327869508,-1.08987267889964,-1.34238662655454));
#82067=CARTESIAN_POINT('Ctrl Pts',(0.724155502318283,0.534302828499086,
-1.6442454361086));
#82068=CARTESIAN_POINT('Ctrl Pts',(0.803427725941486,1.67063323497912,-0.445309606403874));
#82069=CARTESIAN_POINT('Ctrl Pts',(0.882699949564689,1.28179129667979,1.1603365151821));
#82070=CARTESIAN_POINT('Ctrl Pts',(0.961972173187892,-0.277274268110296,
1.70656878530735));
#82071=CARTESIAN_POINT('Ctrl Pts',(1.0412443968111,-1.58319498499271,0.694838588358626));
#82072=CARTESIAN_POINT('Ctrl Pts',(1.1205166204343,-1.44374543633381,-0.95126705305996));
#82073=CARTESIAN_POINT('Ctrl Pts',(1.1997888440575,0.0137705542152546,-1.72890285984628));
#82074=CARTESIAN_POINT('Ctrl Pts',(1.2790610676807,1.45871359983909,-0.928147203425756));
#82075=CARTESIAN_POINT('Ctrl Pts',(1.35833329130391,1.57192783763916,0.719961917183323));
#82076=CARTESIAN_POINT('Ctrl Pts',(1.43760551492711,0.250053655582714,1.71078153521168));
#82077=CARTESIAN_POINT('Ctrl Pts',(1.51687773855032,-1.30010630151546,1.13974783301697));
#82078=CARTESIAN_POINT('Ctrl Pts',(1.59614996217352,-1.6633371234547,-0.471816683068196));
#82079=CARTESIAN_POINT('Ctrl Pts',(1.67542218579672,-0.508027887927404,
-1.65263691735815));
#82080=CARTESIAN_POINT('Ctrl Pts',(1.75469440941992,1.11108428040716,-1.32468600981118));
#82081=CARTESIAN_POINT('Ctrl Pts',(1.83396663304312,1.71583448087688,0.212634185438564));
#82082=CARTESIAN_POINT('Ctrl Pts',(1.91323885666633,0.754117317251402,1.55583042366493));
#82083=CARTESIAN_POINT('Ctrl Pts',(1.99251108028953,-0.896069614137905,
1.47863467995162));
#82084=CARTESIAN_POINT('Ctrl Pts',(2.07178330391274,-1.72819173027205,0.0515226047396124));
#82085=CARTESIAN_POINT('Ctrl Pts',(2.15105552753594,-0.9825649808076,-1.42262690860033));
#82086=CARTESIAN_POINT('Ctrl Pts',(2.23032775115914,0.660092369291553,-1.59799229245964));
#82087=CARTESIAN_POINT('Ctrl Pts',(2.30959997478234,1.70011975464927,-0.314474061535004));
#82088=CARTESIAN_POINT('Ctrl Pts',(2.38887219840555,1.18802663996317,1.25614253626802));
#82089=CARTESIAN_POINT('Ctrl Pts',(2.46814442202875,-0.408673070957845,
1.67996661847221));
#82090=CARTESIAN_POINT('Ctrl Pts',(2.54741664565196,-1.63227510030183,0.570068670272428));
#82091=CARTESIAN_POINT('Ctrl Pts',(2.62668886927516,-1.36569605607521,-1.0602719327417));
#82092=CARTESIAN_POINT('Ctrl Pts',(2.70596109289836,0.147694007720903,-1.72264014746723));
#82093=CARTESIAN_POINT('Ctrl Pts',(2.78523331652156,1.52624377360986,-0.812326701804879));
#82094=CARTESIAN_POINT('Ctrl Pts',(2.86450554014477,1.51141902517799,0.839596582593152));
#82095=CARTESIAN_POINT('Ctrl Pts',(2.94377776376797,0.116735341773671,1.72501590843657));
#82096=CARTESIAN_POINT('Ctrl Pts',(3.02304998739117,-1.38449836206145,1.03557825594721));
#82097=CARTESIAN_POINT('Ctrl Pts',(3.10232221101438,-1.62180155186573,-0.599274130156542));
#82098=CARTESIAN_POINT('Ctrl Pts',(3.18159443463758,-0.378400318371864,
-1.68704749501265));
#82099=CARTESIAN_POINT('Ctrl Pts',(3.26086665826079,1.2103003861222,-1.23458314505688));
#82100=CARTESIAN_POINT('Ctrl Pts',(3.34013888188398,1.69436502395503,0.344893428412662));
#82101=CARTESIAN_POINT('Ctrl Pts',(3.41941110550719,0.630982028908847,1.60968650810039));
#82102=CARTESIAN_POINT('Ctrl Pts',(3.49868332913039,-1.00734708824837,1.4045641813303));
#82103=CARTESIAN_POINT('Ctrl Pts',(3.5779555527536,-1.72814876805798,-0.0821645222904032));
#82104=CARTESIAN_POINT('Ctrl Pts',(3.6572277763768,-0.867017569131943,-1.49528095887952));
#82105=CARTESIAN_POINT('Ctrl Pts',(3.71007592545893,0.228448785913636,-1.5250582084865));
#82106=CARTESIAN_POINT('Ctrl Pts',(3.7365,0.66187319412785,-1.30528009442227));
#82107=CARTESIAN_POINT('Ctrl Pts',(0.303514773719376,0.795408277542867,
-1.11329858282326));
#82108=CARTESIAN_POINT('Ctrl Pts',(0.329938848260444,1.16508431986348,-0.849179514850122));
#82109=CARTESIAN_POINT('Ctrl Pts',(0.382786997342579,1.61438141942961,0.0715973267633055));
#82110=CARTESIAN_POINT('Ctrl Pts',(0.462059220965783,0.815814283571302,
1.39669317121085));
#82111=CARTESIAN_POINT('Ctrl Pts',(0.541331444588985,-0.72821599311703,
1.44257534270058));
#82112=CARTESIAN_POINT('Ctrl Pts',(0.620603668212189,-1.60707211535051,
0.173522469445461));
#82113=CARTESIAN_POINT('Ctrl Pts',(0.699875891835391,-1.01893972866719,
-1.25501913343577));
#82114=CARTESIAN_POINT('Ctrl Pts',(0.779148115458596,0.49952842165622,-1.53723185374485));
#82115=CARTESIAN_POINT('Ctrl Pts',(0.858420339081797,1.56190223693897,-0.416327208036965));
#82116=CARTESIAN_POINT('Ctrl Pts',(0.937692562705002,1.19836757204108,1.08481751752505));
#82117=CARTESIAN_POINT('Ctrl Pts',(1.0169647863282,-0.259228231870117,1.5954989685663));
#82118=CARTESIAN_POINT('Ctrl Pts',(1.09623700995141,-1.48015479208491,0.649615919727836));
#82119=CARTESIAN_POINT('Ctrl Pts',(1.17550923357461,-1.34978113649726,-0.88935507027625));
#82120=CARTESIAN_POINT('Ctrl Pts',(1.25478145719781,0.0128743155483621,
-1.6163794588211));
#82121=CARTESIAN_POINT('Ctrl Pts',(1.33405368082102,1.36377511648776,-0.867739946079459));
#82122=CARTESIAN_POINT('Ctrl Pts',(1.41332590444422,1.46962095240846,0.673104129269616));
#82123=CARTESIAN_POINT('Ctrl Pts',(1.49259812806742,0.233779237616018,1.59943753710515));
#82124=CARTESIAN_POINT('Ctrl Pts',(1.57187035169063,-1.21549056853332,1.06556882304439));
#82125=CARTESIAN_POINT('Ctrl Pts',(1.65114257531383,-1.55508098337335,-0.441109105984328));
#82126=CARTESIAN_POINT('Ctrl Pts',(1.73041479893703,-0.474963551524882,
-1.54507718631724));
#82127=CARTESIAN_POINT('Ctrl Pts',(1.80968702256023,1.03877080059248,-1.23847053838343));
#82128=CARTESIAN_POINT('Ctrl Pts',(1.88895924618344,1.60416161835313,0.198795165170016));
#82129=CARTESIAN_POINT('Ctrl Pts',(1.96823146980664,0.705036569408422,1.45457121775165));
#82130=CARTESIAN_POINT('Ctrl Pts',(2.04750369342984,-0.837750085100231,
1.38239965892983));
#82131=CARTESIAN_POINT('Ctrl Pts',(2.12677591705305,-1.61571461219319,0.0481693228117334));
#82132=CARTESIAN_POINT('Ctrl Pts',(2.20604814067625,-0.918616012975739,
-1.3300370807601));
#82133=CARTESIAN_POINT('Ctrl Pts',(2.28532036429946,0.617131113278558,-1.4939890359808));
#82134=CARTESIAN_POINT('Ctrl Pts',(2.36459258792266,1.58946966470712,-0.294006924971143));
#82135=CARTESIAN_POINT('Ctrl Pts',(2.44386481154586,1.11070546643635,1.17438812794583));
#82136=CARTESIAN_POINT('Ctrl Pts',(2.52313703516906,-0.382075113999367,
1.5706281692686));
#82137=CARTESIAN_POINT('Ctrl Pts',(2.60240925879227,-1.52604059172393,0.53296648998992));
#82138=CARTESIAN_POINT('Ctrl Pts',(2.68168148241547,-1.27681149895791,-0.991265508694116));
#82139=CARTESIAN_POINT('Ctrl Pts',(2.76095370603867,0.138081534720963,-1.61052434695731));
#82140=CARTESIAN_POINT('Ctrl Pts',(2.84022592966188,1.42691017645486,-0.75945747163958));
#82141=CARTESIAN_POINT('Ctrl Pts',(2.91949815328508,1.41305027755367,0.784952527593498));
#82142=CARTESIAN_POINT('Ctrl Pts',(2.99877037690829,0.109137773407462,1.61274548460426));
#82143=CARTESIAN_POINT('Ctrl Pts',(3.07804260053148,-1.29439008123716,0.968178987837214));
#82144=CARTESIAN_POINT('Ctrl Pts',(3.15731482415469,-1.51624870060833,-0.5602711503838));
#82145=CARTESIAN_POINT('Ctrl Pts',(3.23658704777789,-0.353772624265322,
-1.57724819614011));
#82146=CARTESIAN_POINT('Ctrl Pts',(3.3158592714011,1.13152955470564,-1.15423190175885));
#82147=CARTESIAN_POINT('Ctrl Pts',(3.3951314950243,1.58408947319882,0.322446486795784));
#82148=CARTESIAN_POINT('Ctrl Pts',(3.4744037186475,0.589915381656662,1.5049221487587));
#82149=CARTESIAN_POINT('Ctrl Pts',(3.55367594227071,-0.941785209084957,
1.31314994267521));
#82150=CARTESIAN_POINT('Ctrl Pts',(3.6329481658939,-1.61567444611912,-0.0768169508874945));
#82151=CARTESIAN_POINT('Ctrl Pts',(3.71222038951711,-0.810588854776071,
-1.39796253637643));
#82152=CARTESIAN_POINT('Ctrl Pts',(3.76506853859925,0.213580492877578,-1.42580177230041));
#82153=CARTESIAN_POINT('Ctrl Pts',(3.79149261314031,0.618796035439312,-1.22032763183687));
#82154=CARTESIAN_POINT('Ctrl Pts',(0.358507386859688,0.740036351041164,
-1.03579689087083));
#82155=CARTESIAN_POINT('Ctrl Pts',(0.384931461400756,1.08397759121959,-0.790064332106122));
#82156=CARTESIAN_POINT('Ctrl Pts',(0.437779610482892,1.50199711085978,0.0666131167328262));
#82157=CARTESIAN_POINT('Ctrl Pts',(0.517051834106093,0.759021803753894,
1.29946311489232));
#82158=CARTESIAN_POINT('Ctrl Pts',(0.596324057729298,-0.677521621953577,
1.34215122328364));
#82159=CARTESIAN_POINT('Ctrl Pts',(0.675596281352501,-1.49519664011782,
0.16144279452152));
#82160=CARTESIAN_POINT('Ctrl Pts',(0.754868504975703,-0.94800677843474,
-1.167651640317));
#82161=CARTESIAN_POINT('Ctrl Pts',(0.834140728598908,0.464754014813354,
-1.4302182713811));
#82162=CARTESIAN_POINT('Ctrl Pts',(0.913412952222109,1.45317123889882,-0.387344809670057));
#82163=CARTESIAN_POINT('Ctrl Pts',(0.992685175845314,1.11494384740237,1.009298519868));
#82164=CARTESIAN_POINT('Ctrl Pts',(1.07195739946851,-0.241182195629937,
1.48442915182525));
#82165=CARTESIAN_POINT('Ctrl Pts',(1.15122962309172,-1.37711459917712,0.604393251097046));
#82166=CARTESIAN_POINT('Ctrl Pts',(1.23050184671492,-1.25581683666071,-0.827443087492541));
#82167=CARTESIAN_POINT('Ctrl Pts',(1.30977407033813,0.0119780768814665,
-1.50385605779591));
#82168=CARTESIAN_POINT('Ctrl Pts',(1.38904629396133,1.26883663313643,-0.807332688733162));
#82169=CARTESIAN_POINT('Ctrl Pts',(1.46831851758453,1.36731406717776,0.62624634135591));
#82170=CARTESIAN_POINT('Ctrl Pts',(1.54759074120774,0.217504819649325,1.48809353899862));
#82171=CARTESIAN_POINT('Ctrl Pts',(1.62686296483094,-1.1308748355512,0.991389813071809));
#82172=CARTESIAN_POINT('Ctrl Pts',(1.70613518845414,-1.44682484329199,-0.410401528900456));
#82173=CARTESIAN_POINT('Ctrl Pts',(1.78540741207734,-0.441899215122363,
-1.43751745527634));
#82174=CARTESIAN_POINT('Ctrl Pts',(1.86467963570055,0.966457320777803,-1.15225506695567));
#82175=CARTESIAN_POINT('Ctrl Pts',(1.94395185932375,1.49248875582936,0.184956144901466));
#82176=CARTESIAN_POINT('Ctrl Pts',(2.02322408294696,0.655955821565445,1.35331201183838));
#82177=CARTESIAN_POINT('Ctrl Pts',(2.10249630657015,-0.77943055606256,1.28616463790804));
#82178=CARTESIAN_POINT('Ctrl Pts',(2.18176853019336,-1.50323749411433,0.044816040883855));
#82179=CARTESIAN_POINT('Ctrl Pts',(2.26104075381656,-0.854667045143881,
-1.23744725291987));
#82180=CARTESIAN_POINT('Ctrl Pts',(2.34031297743977,0.574169857265563,-1.38998577950196));
#82181=CARTESIAN_POINT('Ctrl Pts',(2.41958520106297,1.47881957476497,-0.273539788407282));
#82182=CARTESIAN_POINT('Ctrl Pts',(2.49885742468617,1.03338429290954,1.09263371962364));
#82183=CARTESIAN_POINT('Ctrl Pts',(2.57812964830938,-0.35547715704089,1.46128972006499));
#82184=CARTESIAN_POINT('Ctrl Pts',(2.65740187193258,-1.41980608314604,0.495864309707411));
#82185=CARTESIAN_POINT('Ctrl Pts',(2.73667409555578,-1.18792694184062,-0.922259084646528));
#82186=CARTESIAN_POINT('Ctrl Pts',(2.81594631917899,0.128469061721023,-1.4984085464474));
#82187=CARTESIAN_POINT('Ctrl Pts',(2.89521854280219,1.32757657929986,-0.706588241474279));
#82188=CARTESIAN_POINT('Ctrl Pts',(2.97449076642539,1.31468152992934,0.730308472593842));
#82189=CARTESIAN_POINT('Ctrl Pts',(3.05376299004859,0.101540205041254,1.50047506077196));
#82190=CARTESIAN_POINT('Ctrl Pts',(3.1330352136718,-1.20428180041287,0.900779719727221));
#82191=CARTESIAN_POINT('Ctrl Pts',(3.212307437295,-1.41069584935093,-0.521268170611058));
#82192=CARTESIAN_POINT('Ctrl Pts',(3.2915796609182,-0.32914493015878,-1.46744889726758));
#82193=CARTESIAN_POINT('Ctrl Pts',(3.37085188454141,1.05275872328908,-1.07388065846081));
#82194=CARTESIAN_POINT('Ctrl Pts',(3.45012410816461,1.4738139224426,0.299999545178905));
#82195=CARTESIAN_POINT('Ctrl Pts',(3.52939633178781,0.548848734404479,1.40015778941701));
#82196=CARTESIAN_POINT('Ctrl Pts',(3.60866855541102,-0.876223329921544,
1.22173570402013));
#82197=CARTESIAN_POINT('Ctrl Pts',(3.68794077903421,-1.50320012418026,-0.0714693794845846));
#82198=CARTESIAN_POINT('Ctrl Pts',(3.76721300265743,-0.754160140420199,
-1.30064411387334));
#82199=CARTESIAN_POINT('Ctrl Pts',(3.82006115173956,0.198712199841519,-1.32654533611433));
#82200=CARTESIAN_POINT('Ctrl Pts',(3.84648522628063,0.575718876750774,-1.13537516925148));
#82201=CARTESIAN_POINT('Ctrl Pts',(0.4135,0.68466442453946,-0.958295198918397));
#82202=CARTESIAN_POINT('Ctrl Pts',(0.439924074541068,1.00287086257571,-0.730949149362124));
#82203=CARTESIAN_POINT('Ctrl Pts',(0.492772223623204,1.38961280228995,0.0616289067023483));
#82204=CARTESIAN_POINT('Ctrl Pts',(0.572044447246405,0.702229323936485,
1.20223305857378));
#82205=CARTESIAN_POINT('Ctrl Pts',(0.65131667086961,-0.626827250790123,
1.2417271038667));
#82206=CARTESIAN_POINT('Ctrl Pts',(0.730588894492812,-1.38332116488512,
0.149363119597578));
#82207=CARTESIAN_POINT('Ctrl Pts',(0.809861118116015,-0.877073828202288,
-1.08028414719823));
#82208=CARTESIAN_POINT('Ctrl Pts',(0.889133341739219,0.429979607970486,
-1.32320468901736));
#82209=CARTESIAN_POINT('Ctrl Pts',(0.968405565362423,1.34444024085867,-0.358362411303147));
#82210=CARTESIAN_POINT('Ctrl Pts',(1.04767778898562,1.03152012276366,0.933779522210948));
#82211=CARTESIAN_POINT('Ctrl Pts',(1.12695001260883,-0.223136159389758,
1.3733593350842));
#82212=CARTESIAN_POINT('Ctrl Pts',(1.20622223623203,-1.27407440626933,0.559170582466256));
#82213=CARTESIAN_POINT('Ctrl Pts',(1.28549445985523,-1.16185253682415,-0.765531104708832));
#82214=CARTESIAN_POINT('Ctrl Pts',(1.36476668347844,0.0110818382145732,
-1.39133265677073));
#82215=CARTESIAN_POINT('Ctrl Pts',(1.44403890710164,1.1738981497851,-0.746925431386865));
#82216=CARTESIAN_POINT('Ctrl Pts',(1.52331113072484,1.26500718194706,0.579388553442205));
#82217=CARTESIAN_POINT('Ctrl Pts',(1.60258335434805,0.201230401682631,1.37674954089208));
#82218=CARTESIAN_POINT('Ctrl Pts',(1.68185557797125,-1.04625910256907,0.917210803099231));
#82219=CARTESIAN_POINT('Ctrl Pts',(1.76112780159445,-1.33856870321064,-0.379693951816588));
#82220=CARTESIAN_POINT('Ctrl Pts',(1.84040002521766,-0.408834878719842,
-1.32995772423544));
#82221=CARTESIAN_POINT('Ctrl Pts',(1.91967224884086,0.894143840963125,-1.06603959552792));
#82222=CARTESIAN_POINT('Ctrl Pts',(1.99894447246406,1.3808158933056,0.17111712463292));
#82223=CARTESIAN_POINT('Ctrl Pts',(2.07821669608726,0.606875073722467,1.2520528059251));
#82224=CARTESIAN_POINT('Ctrl Pts',(2.15748891971047,-0.721111027024888,
1.18992961688625));
#82225=CARTESIAN_POINT('Ctrl Pts',(2.23676114333367,-1.39076037603547,0.0414627589559757));
#82226=CARTESIAN_POINT('Ctrl Pts',(2.31603336695688,-0.790718077312022,
-1.14485742507963));
#82227=CARTESIAN_POINT('Ctrl Pts',(2.39530559058008,0.53120860125257,-1.28598252302312));
#82228=CARTESIAN_POINT('Ctrl Pts',(2.47457781420328,1.36816948482281,-0.25307265184342));
#82229=CARTESIAN_POINT('Ctrl Pts',(2.55385003782648,0.956063119382725,1.01087931130145));
#82230=CARTESIAN_POINT('Ctrl Pts',(2.63312226144969,-0.328879200082413,
1.35195127086139));
#82231=CARTESIAN_POINT('Ctrl Pts',(2.71239448507289,-1.31357157456815,0.458762129424903));
#82232=CARTESIAN_POINT('Ctrl Pts',(2.7916667086961,-1.09904238472332,-0.853252660598941));
#82233=CARTESIAN_POINT('Ctrl Pts',(2.87093893231929,0.118856588721082,-1.38629274593749));
#82234=CARTESIAN_POINT('Ctrl Pts',(2.9502111559425,1.22824298214487,-0.653719011308979));
#82235=CARTESIAN_POINT('Ctrl Pts',(3.0294833795657,1.21631278230501,0.675664417594188));
#82236=CARTESIAN_POINT('Ctrl Pts',(3.10875560318891,0.0939426366750465,
1.38820463693965));
#82237=CARTESIAN_POINT('Ctrl Pts',(3.18802782681211,-1.11417351958857,0.833380451617229));
#82238=CARTESIAN_POINT('Ctrl Pts',(3.26730005043531,-1.30514299809352,-0.482265190838316));
#82239=CARTESIAN_POINT('Ctrl Pts',(3.34657227405852,-0.30451723605224,-1.35764959839504));
#82240=CARTESIAN_POINT('Ctrl Pts',(3.42584449768172,0.973987891872518,-0.993529415162783));
#82241=CARTESIAN_POINT('Ctrl Pts',(3.50511672130493,1.36353837168639,0.277552603562025));
#82242=CARTESIAN_POINT('Ctrl Pts',(3.58438894492812,0.507782087152296,1.29539343007532));
#82243=CARTESIAN_POINT('Ctrl Pts',(3.66366116855133,-0.810661450758132,
1.13032146536505));
#82244=CARTESIAN_POINT('Ctrl Pts',(3.74293339217452,-1.3907258022414,-0.0661218080816751));
#82245=CARTESIAN_POINT('Ctrl Pts',(3.82220561579774,-0.697731426064326,
-1.20332569137025));
#82246=CARTESIAN_POINT('Ctrl Pts',(3.87505376487987,0.183843906805461,-1.22728889992824));
#82247=CARTESIAN_POINT('Ctrl Pts',(3.90147783942094,0.532641718062236,-1.05042270666609));
#82248=CARTESIAN_POINT('Ctrl Pts',(3.7365,0.66187319412785,-1.30528009442227));
#82249=CARTESIAN_POINT('Ctrl Pts',(3.71007592545893,0.228448785913637,-1.5250582084865));
#82250=CARTESIAN_POINT('Ctrl Pts',(3.68365185091787,-0.319284391609157,
-1.51016958368301));
#82251=CARTESIAN_POINT('Ctrl Pts',(3.6572277763768,-0.736672846858221,-1.26720586518308));
#82252=CARTESIAN_POINT('Ctrl Pts',(3.63080370183573,-1.15406130210729,-1.02424214668315));
#82253=CARTESIAN_POINT('Ctrl Pts',(3.60437962729466,-1.44110503508263,-0.553203334486778));
#82254=CARTESIAN_POINT('Ctrl Pts',(3.5779555527536,-1.46449328826871,-0.0698958111184731));
#82255=CARTESIAN_POINT('Ctrl Pts',(3.5766887171167,-1.46561457910426,-0.0467248503632885));
#82256=CARTESIAN_POINT('Ctrl Pts',(3.5754218814798,-1.46612986275361,-0.0235256902050746));
#82257=CARTESIAN_POINT('Ctrl Pts',(3.57415504584291,-1.46605134156425,-0.000323220338867419));
#82258=CARTESIAN_POINT('Origin',(4.,0.,0.866025403784439));
#82259=CARTESIAN_POINT('',(4.,5.30287619362453E-17,0.866025403784439));
#82260=CARTESIAN_POINT('',(4.,0.75,0.433012701892219));
#82261=CARTESIAN_POINT('',(4.,0.1875,0.757772228311384));
#82262=CARTESIAN_POINT('',(2.,0.,0.866025403784439));
#82263=CARTESIAN_POINT('',(4.,5.30287619362453E-17,0.866025403784439));
#82264=CARTESIAN_POINT('',(2.,0.75,0.433012701892219));
#82265=CARTESIAN_POINT('',(2.,0.75,0.433012701892219));
#82266=CARTESIAN_POINT('',(4.,0.75,0.433012701892219));
#82267=CARTESIAN_POINT('Origin',(4.,-0.75,0.433012701892219));
#82268=CARTESIAN_POINT('',(4.,-0.75,0.433012701892219));
#82269=CARTESIAN_POINT('',(4.,-0.5625,0.541265877365274));
#82270=CARTESIAN_POINT('',(2.,-0.75,0.433012701892219));
#82271=CARTESIAN_POINT('',(4.,-0.75,0.433012701892219));
#82272=CARTESIAN_POINT('',(2.,5.30287619362453E-17,0.866025403784439));
#82273=CARTESIAN_POINT('Origin',(4.,-0.75,-0.433012701892219));
#82274=CARTESIAN_POINT('',(4.,-0.75,-0.433012701892219));
#82275=CARTESIAN_POINT('',(4.,-0.75,-0.21650635094611));
#82276=CARTESIAN_POINT('',(2.,-0.75,-0.433012701892219));
#82277=CARTESIAN_POINT('',(4.,-0.75,-0.433012701892219));
#82278=CARTESIAN_POINT('',(2.,-0.75,0.433012701892219));
#82279=CARTESIAN_POINT('Origin',(4.,-1.38777878078145E-16,-0.866025403784439));
#82280=CARTESIAN_POINT('',(4.,-1.59086285808736E-16,-0.866025403784439));
#82281=CARTESIAN_POINT('',(4.,-0.1875,-0.757772228311384));
#82282=CARTESIAN_POINT('',(2.,-1.38777878078145E-16,-0.866025403784439));
#82283=CARTESIAN_POINT('',(4.,-1.59086285808736E-16,-0.866025403784439));
#82284=CARTESIAN_POINT('',(2.,-0.75,-0.433012701892219));
#82285=CARTESIAN_POINT('Origin',(4.,0.75,-0.43301270189222));
#82286=CARTESIAN_POINT('',(4.,0.75,-0.43301270189222));
#82287=CARTESIAN_POINT('',(4.,0.5625,-0.541265877365275));
#82288=CARTESIAN_POINT('',(2.,0.75,-0.43301270189222));
#82289=CARTESIAN_POINT('',(4.,0.75,-0.43301270189222));
#82290=CARTESIAN_POINT('',(2.,-1.59086285808736E-16,-0.866025403784439));
#82291=CARTESIAN_POINT('Origin',(4.,0.75,0.433012701892219));
#82292=CARTESIAN_POINT('',(4.,0.75,0.21650635094611));
#82293=CARTESIAN_POINT('',(2.,0.75,-0.43301270189222));
#82294=CARTESIAN_POINT('Origin',(2.,0.,0.));
#82295=CARTESIAN_POINT('Origin',(0.,1.05,0.));
#82296=CARTESIAN_POINT('',(0.,-1.05,-1.28587913910472E-16));
#82297=CARTESIAN_POINT('Origin',(0.,0.,0.));
#82298=CARTESIAN_POINT('Origin',(0.225,0.,0.));
#82299=CARTESIAN_POINT('',(0.225,-1.275,-1.56142466891288E-16));
#82300=CARTESIAN_POINT('Origin',(2.075,0.,0.));
#82301=CARTESIAN_POINT('Origin',(3.7365,0.,0.));
#82302=CARTESIAN_POINT('Origin',(3.85,0.,0.));
#82303=CARTESIAN_POINT('',(4.,-1.2,-1.46957615897682E-16));
#82304=CARTESIAN_POINT('Origin',(4.,0.,0.));
#82305=CARTESIAN_POINT('',(3.85,-1.35,-1.65327317884893E-16));
#82306=CARTESIAN_POINT('Origin',(4.,0.,0.));
#82307=CARTESIAN_POINT('',(0.,0.,0.));
#82308=CARTESIAN_POINT('',(0.,0.,0.));
#82309=CARTESIAN_POINT('',(0.,0.,0.));
#82310=CARTESIAN_POINT('',(0.,0.,0.));
#82311=CARTESIAN_POINT('',(0.,0.,0.));
#82312=CARTESIAN_POINT('',(0.,0.,29.35));
#82313=CARTESIAN_POINT('',(0.,0.,19.05));
#82314=CARTESIAN_POINT('',(-52.4250000000002,52.4250000000002,36.0375));
#82315=CARTESIAN_POINT('',(-52.4250000000002,-52.4250000000002,29.325));
#82316=CARTESIAN_POINT('',(52.4250000000002,52.4250000000002,29.325));
#82317=CARTESIAN_POINT('',(-54.0000000000001,-65.9999999999998,20.));
#82318=CARTESIAN_POINT('',(-18.75,56.25,46.));
#82319=CARTESIAN_POINT('',(-18.75,56.2500000000001,51.7));
#82320=CARTESIAN_POINT('',(-18.75,56.2500000000001,52.5));
#82321=CARTESIAN_POINT('',(-56.25,18.75,46.));
#82322=CARTESIAN_POINT('',(-56.2500000000002,18.75,51.7));
#82323=CARTESIAN_POINT('',(-56.2500000000002,18.75,52.5));
#82324=CARTESIAN_POINT('',(-60.,-79.,11.325));
#82325=CARTESIAN_POINT('',(-38.6,-79.,14.));
#82326=CARTESIAN_POINT('',(-33.475,-73.225,3.75));
#82327=CARTESIAN_POINT('',(-33.475,-73.225,10.75));
#82328=CARTESIAN_POINT('',(-52.4250000000001,-52.4250000000001,57.0000000000002));
#82329=CARTESIAN_POINT('',(-52.4250000000001,-52.4250000000001,57.0000000000002));
#82330=CARTESIAN_POINT('',(-52.4250000000001,-52.425,57.0000000000002));
#82331=CARTESIAN_POINT('',(-52.4250000000001,-52.425,57.0000000000002));
#82332=CARTESIAN_POINT('',(-56.0312445840513,-56.0312445840512,67.5));
#82333=CARTESIAN_POINT('',(52.4250000000001,52.4250000000001,57.0000000000002));
#82334=CARTESIAN_POINT('',(52.4250000000001,52.4250000000001,57.0000000000002));
#82335=CARTESIAN_POINT('',(52.425,52.4250000000001,57.0000000000002));
#82336=CARTESIAN_POINT('',(52.425,52.4250000000001,57.0000000000002));
#82337=CARTESIAN_POINT('',(56.0312445840512,56.0312445840513,67.5));
#82338=CARTESIAN_POINT('',(-26.325,-66.,20.));
#82339=CARTESIAN_POINT('',(-26.325,-66.,20.));
#82340=CARTESIAN_POINT('',(-26.325,-66.,20.));
#82341=CARTESIAN_POINT('',(-26.325,-66.,20.));
#82342=CARTESIAN_POINT('',(-15.825,-66.,25.1));
#82343=UNCERTAINTY_MEASURE_WITH_UNIT(LENGTH_MEASURE(0.01),#82385,
'DISTANCE_ACCURACY_VALUE',
'Maximum model space distance between geometric entities at asserted c
onnectivities');
#82344=UNCERTAINTY_MEASURE_WITH_UNIT(LENGTH_MEASURE(0.01),#82385,
'DISTANCE_ACCURACY_VALUE',
'Maximum model space distance between geometric entities at asserted c
onnectivities');
#82345=UNCERTAINTY_MEASURE_WITH_UNIT(LENGTH_MEASURE(0.01),#82385,
'DISTANCE_ACCURACY_VALUE',
'Maximum model space distance between geometric entities at asserted c
onnectivities');
#82346=UNCERTAINTY_MEASURE_WITH_UNIT(LENGTH_MEASURE(0.01),#82385,
'DISTANCE_ACCURACY_VALUE',
'Maximum model space distance between geometric entities at asserted c
onnectivities');
#82347=UNCERTAINTY_MEASURE_WITH_UNIT(LENGTH_MEASURE(0.01),#82385,
'DISTANCE_ACCURACY_VALUE',
'Maximum model space distance between geometric entities at asserted c
onnectivities');
#82348=UNCERTAINTY_MEASURE_WITH_UNIT(LENGTH_MEASURE(0.01),#82385,
'DISTANCE_ACCURACY_VALUE',
'Maximum model space distance between geometric entities at asserted c
onnectivities');
#82349=UNCERTAINTY_MEASURE_WITH_UNIT(LENGTH_MEASURE(0.01),#82385,
'DISTANCE_ACCURACY_VALUE',
'Maximum model space distance between geometric entities at asserted c
onnectivities');
#82350=UNCERTAINTY_MEASURE_WITH_UNIT(LENGTH_MEASURE(0.01),#82385,
'DISTANCE_ACCURACY_VALUE',
'Maximum model space distance between geometric entities at asserted c
onnectivities');
#82351=UNCERTAINTY_MEASURE_WITH_UNIT(LENGTH_MEASURE(0.01),#82385,
'DISTANCE_ACCURACY_VALUE',
'Maximum model space distance between geometric entities at asserted c
onnectivities');
#82352=UNCERTAINTY_MEASURE_WITH_UNIT(LENGTH_MEASURE(0.01),#82385,
'DISTANCE_ACCURACY_VALUE',
'Maximum model space distance between geometric entities at asserted c
onnectivities');
#82353=UNCERTAINTY_MEASURE_WITH_UNIT(LENGTH_MEASURE(0.01),#82385,
'DISTANCE_ACCURACY_VALUE',
'Maximum model space distance between geometric entities at asserted c
onnectivities');
#82354=UNCERTAINTY_MEASURE_WITH_UNIT(LENGTH_MEASURE(0.01),#82385,
'DISTANCE_ACCURACY_VALUE',
'Maximum model space distance between geometric entities at asserted c
onnectivities');
#82355=UNCERTAINTY_MEASURE_WITH_UNIT(LENGTH_MEASURE(0.01),#82385,
'DISTANCE_ACCURACY_VALUE',
'Maximum model space distance between geometric entities at asserted c
onnectivities');
#82356=UNCERTAINTY_MEASURE_WITH_UNIT(LENGTH_MEASURE(0.01),#82385,
'DISTANCE_ACCURACY_VALUE',
'Maximum model space distance between geometric entities at asserted c
onnectivities');
#82357=UNCERTAINTY_MEASURE_WITH_UNIT(LENGTH_MEASURE(0.01),#82385,
'DISTANCE_ACCURACY_VALUE',
'Maximum model space distance between geometric entities at asserted c
onnectivities');
#82358=UNCERTAINTY_MEASURE_WITH_UNIT(LENGTH_MEASURE(0.01),#82385,
'DISTANCE_ACCURACY_VALUE',
'Maximum model space distance between geometric entities at asserted c
onnectivities');
#82359=UNCERTAINTY_MEASURE_WITH_UNIT(LENGTH_MEASURE(0.01),#82385,
'DISTANCE_ACCURACY_VALUE',
'Maximum model space distance between geometric entities at asserted c
onnectivities');
#82360=UNCERTAINTY_MEASURE_WITH_UNIT(LENGTH_MEASURE(0.01),#82385,
'DISTANCE_ACCURACY_VALUE',
'Maximum model space distance between geometric entities at asserted c
onnectivities');
#82361=UNCERTAINTY_MEASURE_WITH_UNIT(LENGTH_MEASURE(0.01),#82385,
'DISTANCE_ACCURACY_VALUE',
'Maximum model space distance between geometric entities at asserted c
onnectivities');
#82362=UNCERTAINTY_MEASURE_WITH_UNIT(LENGTH_MEASURE(0.01),#82385,
'DISTANCE_ACCURACY_VALUE',
'Maximum model space distance between geometric entities at asserted c
onnectivities');
#82363=UNCERTAINTY_MEASURE_WITH_UNIT(LENGTH_MEASURE(0.01),#82385,
'DISTANCE_ACCURACY_VALUE',
'Maximum model space distance between geometric entities at asserted c
onnectivities');
#82364=(
GEOMETRIC_REPRESENTATION_CONTEXT(3)
GLOBAL_UNCERTAINTY_ASSIGNED_CONTEXT((#82343))
GLOBAL_UNIT_ASSIGNED_CONTEXT((#82385,#82387,#82388))
REPRESENTATION_CONTEXT('','3D')
);
#82365=(
GEOMETRIC_REPRESENTATION_CONTEXT(3)
GLOBAL_UNCERTAINTY_ASSIGNED_CONTEXT((#82344))
GLOBAL_UNIT_ASSIGNED_CONTEXT((#82385,#82387,#82388))
REPRESENTATION_CONTEXT('','3D')
);
#82366=(
GEOMETRIC_REPRESENTATION_CONTEXT(3)
GLOBAL_UNCERTAINTY_ASSIGNED_CONTEXT((#82345))
GLOBAL_UNIT_ASSIGNED_CONTEXT((#82385,#82387,#82388))
REPRESENTATION_CONTEXT('','3D')
);
#82367=(
GEOMETRIC_REPRESENTATION_CONTEXT(3)
GLOBAL_UNCERTAINTY_ASSIGNED_CONTEXT((#82346))
GLOBAL_UNIT_ASSIGNED_CONTEXT((#82385,#82387,#82388))
REPRESENTATION_CONTEXT('','3D')
);
#82368=(
GEOMETRIC_REPRESENTATION_CONTEXT(3)
GLOBAL_UNCERTAINTY_ASSIGNED_CONTEXT((#82347))
GLOBAL_UNIT_ASSIGNED_CONTEXT((#82385,#82387,#82388))
REPRESENTATION_CONTEXT('','3D')
);
#82369=(
GEOMETRIC_REPRESENTATION_CONTEXT(3)
GLOBAL_UNCERTAINTY_ASSIGNED_CONTEXT((#82348))
GLOBAL_UNIT_ASSIGNED_CONTEXT((#82385,#82387,#82388))
REPRESENTATION_CONTEXT('','3D')
);
#82370=(
GEOMETRIC_REPRESENTATION_CONTEXT(3)
GLOBAL_UNCERTAINTY_ASSIGNED_CONTEXT((#82349))
GLOBAL_UNIT_ASSIGNED_CONTEXT((#82385,#82387,#82388))
REPRESENTATION_CONTEXT('','3D')
);
#82371=(
GEOMETRIC_REPRESENTATION_CONTEXT(3)
GLOBAL_UNCERTAINTY_ASSIGNED_CONTEXT((#82350))
GLOBAL_UNIT_ASSIGNED_CONTEXT((#82385,#82387,#82388))
REPRESENTATION_CONTEXT('','3D')
);
#82372=(
GEOMETRIC_REPRESENTATION_CONTEXT(3)
GLOBAL_UNCERTAINTY_ASSIGNED_CONTEXT((#82351))
GLOBAL_UNIT_ASSIGNED_CONTEXT((#82385,#82387,#82388))
REPRESENTATION_CONTEXT('','3D')
);
#82373=(
GEOMETRIC_REPRESENTATION_CONTEXT(3)
GLOBAL_UNCERTAINTY_ASSIGNED_CONTEXT((#82352))
GLOBAL_UNIT_ASSIGNED_CONTEXT((#82385,#82387,#82388))
REPRESENTATION_CONTEXT('','3D')
);
#82374=(
GEOMETRIC_REPRESENTATION_CONTEXT(3)
GLOBAL_UNCERTAINTY_ASSIGNED_CONTEXT((#82353))
GLOBAL_UNIT_ASSIGNED_CONTEXT((#82385,#82387,#82388))
REPRESENTATION_CONTEXT('','3D')
);
#82375=(
GEOMETRIC_REPRESENTATION_CONTEXT(3)
GLOBAL_UNCERTAINTY_ASSIGNED_CONTEXT((#82354))
GLOBAL_UNIT_ASSIGNED_CONTEXT((#82385,#82387,#82388))
REPRESENTATION_CONTEXT('','3D')
);
#82376=(
GEOMETRIC_REPRESENTATION_CONTEXT(3)
GLOBAL_UNCERTAINTY_ASSIGNED_CONTEXT((#82355))
GLOBAL_UNIT_ASSIGNED_CONTEXT((#82385,#82387,#82388))
REPRESENTATION_CONTEXT('','3D')
);
#82377=(
GEOMETRIC_REPRESENTATION_CONTEXT(3)
GLOBAL_UNCERTAINTY_ASSIGNED_CONTEXT((#82356))
GLOBAL_UNIT_ASSIGNED_CONTEXT((#82385,#82387,#82388))
REPRESENTATION_CONTEXT('','3D')
);
#82378=(
GEOMETRIC_REPRESENTATION_CONTEXT(3)
GLOBAL_UNCERTAINTY_ASSIGNED_CONTEXT((#82357))
GLOBAL_UNIT_ASSIGNED_CONTEXT((#82385,#82387,#82388))
REPRESENTATION_CONTEXT('','3D')
);
#82379=(
GEOMETRIC_REPRESENTATION_CONTEXT(3)
GLOBAL_UNCERTAINTY_ASSIGNED_CONTEXT((#82358))
GLOBAL_UNIT_ASSIGNED_CONTEXT((#82385,#82387,#82388))
REPRESENTATION_CONTEXT('','3D')
);
#82380=(
GEOMETRIC_REPRESENTATION_CONTEXT(3)
GLOBAL_UNCERTAINTY_ASSIGNED_CONTEXT((#82359))
GLOBAL_UNIT_ASSIGNED_CONTEXT((#82385,#82387,#82388))
REPRESENTATION_CONTEXT('','3D')
);
#82381=(
GEOMETRIC_REPRESENTATION_CONTEXT(3)
GLOBAL_UNCERTAINTY_ASSIGNED_CONTEXT((#82360))
GLOBAL_UNIT_ASSIGNED_CONTEXT((#82385,#82387,#82388))
REPRESENTATION_CONTEXT('','3D')
);
#82382=(
GEOMETRIC_REPRESENTATION_CONTEXT(3)
GLOBAL_UNCERTAINTY_ASSIGNED_CONTEXT((#82361))
GLOBAL_UNIT_ASSIGNED_CONTEXT((#82385,#82387,#82388))
REPRESENTATION_CONTEXT('','3D')
);
#82383=(
GEOMETRIC_REPRESENTATION_CONTEXT(3)
GLOBAL_UNCERTAINTY_ASSIGNED_CONTEXT((#82362))
GLOBAL_UNIT_ASSIGNED_CONTEXT((#82385,#82387,#82388))
REPRESENTATION_CONTEXT('','3D')
);
#82384=(
GEOMETRIC_REPRESENTATION_CONTEXT(3)
GLOBAL_UNCERTAINTY_ASSIGNED_CONTEXT((#82363))
GLOBAL_UNIT_ASSIGNED_CONTEXT((#82385,#82387,#82388))
REPRESENTATION_CONTEXT('','3D')
);
#82385=(
LENGTH_UNIT()
NAMED_UNIT(*)
SI_UNIT(.MILLI.,.METRE.)
);
#82386=(
LENGTH_UNIT()
NAMED_UNIT(*)
SI_UNIT($,.METRE.)
);
#82387=(
NAMED_UNIT(*)
PLANE_ANGLE_UNIT()
SI_UNIT($,.RADIAN.)
);
#82388=(
NAMED_UNIT(*)
SI_UNIT($,.STERADIAN.)
SOLID_ANGLE_UNIT()
);
#82389=SHAPE_DEFINITION_REPRESENTATION(#82409,#82465);
#82390=SHAPE_DEFINITION_REPRESENTATION(#82410,#82466);
#82391=SHAPE_DEFINITION_REPRESENTATION(#82411,#82467);
#82392=SHAPE_DEFINITION_REPRESENTATION(#82412,#82468);
#82393=SHAPE_DEFINITION_REPRESENTATION(#82413,#82469);
#82394=SHAPE_DEFINITION_REPRESENTATION(#82414,#82470);
#82395=SHAPE_DEFINITION_REPRESENTATION(#82415,#82471);
#82396=SHAPE_DEFINITION_REPRESENTATION(#82416,#82472);
#82397=SHAPE_DEFINITION_REPRESENTATION(#82417,#82473);
#82398=SHAPE_DEFINITION_REPRESENTATION(#82418,#82474);
#82399=SHAPE_DEFINITION_REPRESENTATION(#82419,#82475);
#82400=SHAPE_DEFINITION_REPRESENTATION(#82420,#82476);
#82401=SHAPE_DEFINITION_REPRESENTATION(#82421,#82477);
#82402=SHAPE_DEFINITION_REPRESENTATION(#82422,#82478);
#82403=SHAPE_DEFINITION_REPRESENTATION(#82423,#82479);
#82404=SHAPE_DEFINITION_REPRESENTATION(#82424,#82480);
#82405=SHAPE_DEFINITION_REPRESENTATION(#82425,#82481);
#82406=SHAPE_DEFINITION_REPRESENTATION(#82426,#82482);
#82407=SHAPE_DEFINITION_REPRESENTATION(#82427,#82483);
#82408=SHAPE_DEFINITION_REPRESENTATION(#82428,#82484);
#82409=PRODUCT_DEFINITION_SHAPE('',$,#82486);
#82410=PRODUCT_DEFINITION_SHAPE('',$,#82487);
#82411=PRODUCT_DEFINITION_SHAPE('',$,#82488);
#82412=PRODUCT_DEFINITION_SHAPE('',$,#82489);
#82413=PRODUCT_DEFINITION_SHAPE('',$,#82490);
#82414=PRODUCT_DEFINITION_SHAPE('',$,#82491);
#82415=PRODUCT_DEFINITION_SHAPE('',$,#82492);
#82416=PRODUCT_DEFINITION_SHAPE('',$,#82493);
#82417=PRODUCT_DEFINITION_SHAPE('',$,#82494);
#82418=PRODUCT_DEFINITION_SHAPE('',$,#82495);
#82419=PRODUCT_DEFINITION_SHAPE('',$,#82496);
#82420=PRODUCT_DEFINITION_SHAPE('',$,#82497);
#82421=PRODUCT_DEFINITION_SHAPE('',$,#82498);
#82422=PRODUCT_DEFINITION_SHAPE('',$,#82499);
#82423=PRODUCT_DEFINITION_SHAPE('',$,#82500);
#82424=PRODUCT_DEFINITION_SHAPE('',$,#82501);
#82425=PRODUCT_DEFINITION_SHAPE('',$,#82502);
#82426=PRODUCT_DEFINITION_SHAPE('',$,#82503);
#82427=PRODUCT_DEFINITION_SHAPE('',$,#82504);
#82428=PRODUCT_DEFINITION_SHAPE('',$,#82505);
#82429=PRODUCT_DEFINITION_SHAPE($,$,#119);
#82430=PRODUCT_DEFINITION_SHAPE($,$,#120);
#82431=PRODUCT_DEFINITION_SHAPE($,$,#121);
#82432=PRODUCT_DEFINITION_SHAPE($,$,#122);
#82433=PRODUCT_DEFINITION_SHAPE($,$,#123);
#82434=PRODUCT_DEFINITION_SHAPE($,$,#124);
#82435=PRODUCT_DEFINITION_SHAPE($,$,#125);
#82436=PRODUCT_DEFINITION_SHAPE($,$,#126);
#82437=PRODUCT_DEFINITION_SHAPE($,$,#127);
#82438=PRODUCT_DEFINITION_SHAPE($,$,#128);
#82439=PRODUCT_DEFINITION_SHAPE($,$,#129);
#82440=PRODUCT_DEFINITION_SHAPE($,$,#130);
#82441=PRODUCT_DEFINITION_SHAPE($,$,#131);
#82442=PRODUCT_DEFINITION_SHAPE($,$,#132);
#82443=PRODUCT_DEFINITION_SHAPE($,$,#133);
#82444=PRODUCT_DEFINITION_SHAPE($,$,#134);
#82445=PRODUCT_DEFINITION_SHAPE($,$,#135);
#82446=PRODUCT_DEFINITION_SHAPE($,$,#136);
#82447=PRODUCT_DEFINITION_SHAPE($,$,#137);
#82448=PRODUCT_DEFINITION_SHAPE($,$,#138);
#82449=PRODUCT_DEFINITION_SHAPE($,$,#139);
#82450=PRODUCT_DEFINITION_SHAPE($,$,#140);
#82451=PRODUCT_DEFINITION_SHAPE($,$,#141);
#82452=PRODUCT_DEFINITION_SHAPE($,$,#142);
#82453=PRODUCT_DEFINITION_SHAPE($,$,#143);
#82454=PRODUCT_DEFINITION_SHAPE($,$,#144);
#82455=PRODUCT_DEFINITION_SHAPE($,$,#145);
#82456=PRODUCT_DEFINITION_SHAPE($,$,#146);
#82457=PRODUCT_DEFINITION_SHAPE($,$,#147);
#82458=PRODUCT_DEFINITION_SHAPE($,$,#148);
#82459=PRODUCT_DEFINITION_SHAPE($,$,#149);
#82460=PRODUCT_DEFINITION_SHAPE($,$,#150);
#82461=PRODUCT_DEFINITION_SHAPE($,$,#151);
#82462=PRODUCT_DEFINITION_SHAPE($,$,#152);
#82463=PRODUCT_DEFINITION_SHAPE($,$,#153);
#82464=PRODUCT_DEFINITION_SHAPE($,$,#154);
#82465=SHAPE_REPRESENTATION('',(#30890,#33377,#33378,#33379,#33380,#33381,
#33382,#33383,#33384,#33385,#33386,#33387,#33388,#33389,#33390,#33391,#33392,
#33393,#33394,#33395,#33396,#33397,#33398,#33399,#33400,#33401,#33402,#33403,
#33404,#33405,#33406,#33407,#33408,#33409,#33410,#33411,#33412),#82364);
#82466=SHAPE_REPRESENTATION('',(#30891),#82365);
#82467=SHAPE_REPRESENTATION('',(#31122),#82366);
#82468=SHAPE_REPRESENTATION('',(#31321),#82367);
#82469=SHAPE_REPRESENTATION('',(#31710),#82368);
#82470=SHAPE_REPRESENTATION('',(#31766),#82369);
#82471=SHAPE_REPRESENTATION('',(#31784),#82370);
#82472=SHAPE_REPRESENTATION('',(#32066),#82371);
#82473=SHAPE_REPRESENTATION('',(#32075),#82372);
#82474=SHAPE_REPRESENTATION('',(#32078),#82373);
#82475=SHAPE_REPRESENTATION('',(#32088),#82374);
#82476=SHAPE_REPRESENTATION('',(#32093),#82375);
#82477=SHAPE_REPRESENTATION('',(#32107),#82376);
#82478=SHAPE_REPRESENTATION('',(#32444),#82377);
#82479=SHAPE_REPRESENTATION('',(#32454),#82378);
#82480=SHAPE_REPRESENTATION('',(#32845),#82379);
#82481=SHAPE_REPRESENTATION('',(#32907),#82380);
#82482=SHAPE_REPRESENTATION('',(#32982),#82381);
#82483=SHAPE_REPRESENTATION('',(#33154),#82382);
#82484=SHAPE_REPRESENTATION('',(#33338),#82383);
#82485=PRODUCT_DEFINITION_CONTEXT('part definition',#82547,'design');
#82486=PRODUCT_DEFINITION('2026-10-20-12-38-02-863','MAS-285',#82506,#82485);
#82487=PRODUCT_DEFINITION('2026-10-20-12-38-04-055','01_Base_Plate',#82507,
#82485);
#82488=PRODUCT_DEFINITION('2026-10-20-12-38-05-983',
'02_Rotation_Carrier_Plate',#82508,#82485);
#82489=PRODUCT_DEFINITION('2026-10-20-12-38-07-933',
'03_Top_Tilt_Platform',#82509,#82485);
#82490=PRODUCT_DEFINITION('2026-10-20-12-38-12-594',
'04_Rotation_Adjuster_Block',#82510,#82485);
#82491=PRODUCT_DEFINITION('2026-10-20-12-38-29-156',
'16_Rotation_Return_Extension_Spring',#82511,#82485);
#82492=PRODUCT_DEFINITION('2026-10-20-12-38-20-714',
'11_ISO_7379_Shoulder_Screw_10x12_M8',#82512,#82485);
#82493=PRODUCT_DEFINITION('2026-10-20-12-38-23-638',
'12_PTFE_Thrust_Washer_30x10.5x0.75',#82513,#82485);
#82494=PRODUCT_DEFINITION('2026-10-20-12-38-19-717',
'09_Pivot_Ball_15.875_Hardened',#82514,#82485);
#82495=PRODUCT_DEFINITION('2026-10-20-12-38-20-133',
'10_Hardened_Seat_Pad_D10x5',#82515,#82485);
#82496=PRODUCT_DEFINITION('2026-10-20-12-38-24-156',
'13_Preload_Compression_Spring_D9x5.7',#82516,#82485);
#82497=PRODUCT_DEFINITION('2026-10-20-12-38-28-563',
'15_ISO_7089_Washer_M4',#82517,#82485);
#82498=PRODUCT_DEFINITION('2026-10-20-12-38-25-351','14_ISO_4762_M4x30',
#82518,#82485);
#82499=PRODUCT_DEFINITION('2026-10-20-12-38-37-321',
'17_ISO_8734_Dowel_Pin_3x18',#82519,#82485);
#82500=PRODUCT_DEFINITION('2026-10-20-12-38-38-109','18_DIN_912_M3x35',
#82520,#82485);
#82501=PRODUCT_DEFINITION('2026-10-20-12-38-18-701',
'08_Bushing_Jam_Ring_M14x1.25',#82521,#82485);
#82502=PRODUCT_DEFINITION('2026-10-20-12-38-17-430',
'07_AJS_Bushing_M14x1.25_Brass',#82522,#82485);
#82503=PRODUCT_DEFINITION('2026-10-20-12-38-14-832',
'05_AJS100_Adjustment_Screw_M10x0.75',#82523,#82485);
#82504=PRODUCT_DEFINITION('2026-10-20-12-38-15-744',
'06_AJS_Fluted_Knob',#82524,#82485);
#82505=PRODUCT_DEFINITION('2026-10-20-12-38-42-004',
'19_ISO_4026_Set_Screw_M3x4',#82525,#82485);
#82506=PRODUCT_DEFINITION_FORMATION('',$,#82549);
#82507=PRODUCT_DEFINITION_FORMATION('',$,#82550);
#82508=PRODUCT_DEFINITION_FORMATION('',$,#82551);
#82509=PRODUCT_DEFINITION_FORMATION('',$,#82552);
#82510=PRODUCT_DEFINITION_FORMATION('',$,#82553);
#82511=PRODUCT_DEFINITION_FORMATION('',$,#82554);
#82512=PRODUCT_DEFINITION_FORMATION('',$,#82555);
#82513=PRODUCT_DEFINITION_FORMATION('',$,#82556);
#82514=PRODUCT_DEFINITION_FORMATION('',$,#82557);
#82515=PRODUCT_DEFINITION_FORMATION('',$,#82558);
#82516=PRODUCT_DEFINITION_FORMATION('',$,#82559);
#82517=PRODUCT_DEFINITION_FORMATION('',$,#82560);
#82518=PRODUCT_DEFINITION_FORMATION('',$,#82561);
#82519=PRODUCT_DEFINITION_FORMATION('',$,#82562);
#82520=PRODUCT_DEFINITION_FORMATION('',$,#82563);
#82521=PRODUCT_DEFINITION_FORMATION('',$,#82564);
#82522=PRODUCT_DEFINITION_FORMATION('',$,#82565);
#82523=PRODUCT_DEFINITION_FORMATION('',$,#82566);
#82524=PRODUCT_DEFINITION_FORMATION('',$,#82567);
#82525=PRODUCT_DEFINITION_FORMATION('',$,#82568);
#82526=PRODUCT_RELATED_PRODUCT_CATEGORY('MAS-285','MAS-285',(#82549));
#82527=PRODUCT_RELATED_PRODUCT_CATEGORY('01_Base_Plate','01_Base_Plate',
(#82550));
#82528=PRODUCT_RELATED_PRODUCT_CATEGORY('02_Rotation_Carrier_Plate',
'02_Rotation_Carrier_Plate',(#82551));
#82529=PRODUCT_RELATED_PRODUCT_CATEGORY('03_Top_Tilt_Platform',
'03_Top_Tilt_Platform',(#82552));
#82530=PRODUCT_RELATED_PRODUCT_CATEGORY('04_Rotation_Adjuster_Block',
'04_Rotation_Adjuster_Block',(#82553));
#82531=PRODUCT_RELATED_PRODUCT_CATEGORY(
'16_Rotation_Return_Extension_Spring',
'16_Rotation_Return_Extension_Spring',(#82554));
#82532=PRODUCT_RELATED_PRODUCT_CATEGORY(
'11_ISO_7379_Shoulder_Screw_10x12_M8',
'11_ISO_7379_Shoulder_Screw_10x12_M8',(#82555));
#82533=PRODUCT_RELATED_PRODUCT_CATEGORY(
'12_PTFE_Thrust_Washer_30x10.5x0.75',
'12_PTFE_Thrust_Washer_30x10.5x0.75',(#82556));
#82534=PRODUCT_RELATED_PRODUCT_CATEGORY('09_Pivot_Ball_15.875_Hardened',
'09_Pivot_Ball_15.875_Hardened',(#82557));
#82535=PRODUCT_RELATED_PRODUCT_CATEGORY('10_Hardened_Seat_Pad_D10x5',
'10_Hardened_Seat_Pad_D10x5',(#82558));
#82536=PRODUCT_RELATED_PRODUCT_CATEGORY(
'13_Preload_Compression_Spring_D9x5.7',
'13_Preload_Compression_Spring_D9x5.7',(#82559));
#82537=PRODUCT_RELATED_PRODUCT_CATEGORY('15_ISO_7089_Washer_M4',
'15_ISO_7089_Washer_M4',(#82560));
#82538=PRODUCT_RELATED_PRODUCT_CATEGORY('14_ISO_4762_M4x30',
'14_ISO_4762_M4x30',(#82561));
#82539=PRODUCT_RELATED_PRODUCT_CATEGORY('17_ISO_8734_Dowel_Pin_3x18',
'17_ISO_8734_Dowel_Pin_3x18',(#82562));
#82540=PRODUCT_RELATED_PRODUCT_CATEGORY('18_DIN_912_M3x35',
'18_DIN_912_M3x35',(#82563));
#82541=PRODUCT_RELATED_PRODUCT_CATEGORY('08_Bushing_Jam_Ring_M14x1.25',
'08_Bushing_Jam_Ring_M14x1.25',(#82564));
#82542=PRODUCT_RELATED_PRODUCT_CATEGORY('07_AJS_Bushing_M14x1.25_Brass',
'07_AJS_Bushing_M14x1.25_Brass',(#82565));
#82543=PRODUCT_RELATED_PRODUCT_CATEGORY(
'05_AJS100_Adjustment_Screw_M10x0.75',
'05_AJS100_Adjustment_Screw_M10x0.75',(#82566));
#82544=PRODUCT_RELATED_PRODUCT_CATEGORY('06_AJS_Fluted_Knob',
'06_AJS_Fluted_Knob',(#82567));
#82545=PRODUCT_RELATED_PRODUCT_CATEGORY('19_ISO_4026_Set_Screw_M3x4',
'19_ISO_4026_Set_Screw_M3x4',(#82568));
#82546=APPLICATION_PROTOCOL_DEFINITION('international standard',
'automotive_design',2009,#82547);
#82547=APPLICATION_CONTEXT(
'Core Data for Automotive Mechanical Design Process');
#82548=PRODUCT_CONTEXT('part definition',#82547,'mechanical');
#82549=PRODUCT('2026-10-20-12-38-02-863','MAS-285',$,(#82548));
#82550=PRODUCT('2026-10-20-12-38-04-055','01_Base_Plate',$,(#82548));
#82551=PRODUCT('2026-10-20-12-38-05-983','02_Rotation_Carrier_Plate',$,
(#82548));
#82552=PRODUCT('2026-10-20-12-38-07-933','03_Top_Tilt_Platform',$,(#82548));
#82553=PRODUCT('2026-10-20-12-38-12-594','04_Rotation_Adjuster_Block',$,
(#82548));
#82554=PRODUCT('2026-10-20-12-38-29-156',
'16_Rotation_Return_Extension_Spring',$,(#82548));
#82555=PRODUCT('2026-10-20-12-38-20-714',
'11_ISO_7379_Shoulder_Screw_10x12_M8',$,(#82548));
#82556=PRODUCT('2026-10-20-12-38-23-638',
'12_PTFE_Thrust_Washer_30x10.5x0.75',$,(#82548));
#82557=PRODUCT('2026-10-20-12-38-19-717',
'09_Pivot_Ball_15.875_Hardened',$,(#82548));
#82558=PRODUCT('2026-10-20-12-38-20-133','10_Hardened_Seat_Pad_D10x5',$,
(#82548));
#82559=PRODUCT('2026-10-20-12-38-24-156',
'13_Preload_Compression_Spring_D9x5.7',$,(#82548));
#82560=PRODUCT('2026-10-20-12-38-28-563','15_ISO_7089_Washer_M4',$,(#82548));
#82561=PRODUCT('2026-10-20-12-38-25-351','14_ISO_4762_M4x30',$,(#82548));
#82562=PRODUCT('2026-10-20-12-38-37-321','17_ISO_8734_Dowel_Pin_3x18',$,
(#82548));
#82563=PRODUCT('2026-10-20-12-38-38-109','18_DIN_912_M3x35',$,(#82548));
#82564=PRODUCT('2026-10-20-12-38-18-701','08_Bushing_Jam_Ring_M14x1.25',
$,(#82548));
#82565=PRODUCT('2026-10-20-12-38-17-430',
'07_AJS_Bushing_M14x1.25_Brass',$,(#82548));
#82566=PRODUCT('2026-10-20-12-38-14-832',
'05_AJS100_Adjustment_Screw_M10x0.75',$,(#82548));
#82567=PRODUCT('2026-10-20-12-38-15-744','06_AJS_Fluted_Knob',$,(#82548));
#82568=PRODUCT('2026-10-20-12-38-42-004','19_ISO_4026_Set_Screw_M3x4',$,
(#82548));
#82569=PRESENTATION_STYLE_ASSIGNMENT((#82574));
#82570=PRESENTATION_STYLE_ASSIGNMENT((#82575));
#82571=PRESENTATION_STYLE_ASSIGNMENT((#82576));
#82572=PRESENTATION_STYLE_ASSIGNMENT((#82577));
#82573=PRESENTATION_STYLE_ASSIGNMENT((#82578));
#82574=SURFACE_STYLE_USAGE(.BOTH.,#82579);
#82575=SURFACE_STYLE_USAGE(.BOTH.,#82580);
#82576=SURFACE_STYLE_USAGE(.BOTH.,#82581);
#82577=SURFACE_STYLE_USAGE(.BOTH.,#82582);
#82578=SURFACE_STYLE_USAGE(.BOTH.,#82583);
#82579=SURFACE_SIDE_STYLE('',(#82584));
#82580=SURFACE_SIDE_STYLE('',(#82585));
#82581=SURFACE_SIDE_STYLE('',(#82586));
#82582=SURFACE_SIDE_STYLE('',(#82587));
#82583=SURFACE_SIDE_STYLE('',(#82588));
#82584=SURFACE_STYLE_FILL_AREA(#82589);
#82585=SURFACE_STYLE_FILL_AREA(#82590);
#82586=SURFACE_STYLE_FILL_AREA(#82591);
#82587=SURFACE_STYLE_FILL_AREA(#82592);
#82588=SURFACE_STYLE_FILL_AREA(#82593);
#82589=FILL_AREA_STYLE('Steel - Satin',(#82594));
#82590=FILL_AREA_STYLE('MAS285_gun',(#82595));
#82591=FILL_AREA_STYLE('MAS285_ss',(#82596));
#82592=FILL_AREA_STYLE('MAS285_al',(#82597));
#82593=FILL_AREA_STYLE('MAS285_ti',(#82598));
#82594=FILL_AREA_STYLE_COLOUR('Steel - Satin',#82599);
#82595=FILL_AREA_STYLE_COLOUR('MAS285_gun',#82600);
#82596=FILL_AREA_STYLE_COLOUR('MAS285_ss',#82601);
#82597=FILL_AREA_STYLE_COLOUR('MAS285_al',#82602);
#82598=FILL_AREA_STYLE_COLOUR('MAS285_ti',#82603);
#82599=COLOUR_RGB('Steel - Satin',0.627450980392157,0.627450980392157,0.627450980392157);
#82600=COLOUR_RGB('MAS285_gun',0.313725490196078,0.337254901960784,0.364705882352941);
#82601=COLOUR_RGB('MAS285_ss',0.83921568627451,0.850980392156863,0.862745098039216);
#82602=COLOUR_RGB('MAS285_al',0.67843137254902,0.705882352941177,0.729411764705882);
#82603=COLOUR_RGB('MAS285_ti',0.549019607843137,0.572549019607843,0.596078431372549);
#82604=COLOUR_RGB('Dark Blue',0.08,0.2,0.34);
#82605=FILL_AREA_STYLE_COLOUR('',#82604);
#82606=FILL_AREA_STYLE('',(#82605));
#82607=SURFACE_STYLE_FILL_AREA(#82606);
#82608=SURFACE_SIDE_STYLE('',(#82607));
#82609=SURFACE_STYLE_USAGE(.BOTH.,#82608);
#82610=PRESENTATION_STYLE_ASSIGNMENT((#82609));
#82611=COLOUR_RGB('Light Blue',0.38,0.62,0.78);
#82612=FILL_AREA_STYLE_COLOUR('',#82611);
#82613=FILL_AREA_STYLE('',(#82612));
#82614=SURFACE_STYLE_FILL_AREA(#82613);
#82615=SURFACE_SIDE_STYLE('',(#82614));
#82616=SURFACE_STYLE_USAGE(.BOTH.,#82615);
#82617=PRESENTATION_STYLE_ASSIGNMENT((#82616));
#82618=COLOUR_RGB('Sky Blue',0.24,0.69,0.87);
#82619=FILL_AREA_STYLE_COLOUR('',#82618);
#82620=FILL_AREA_STYLE('',(#82619));
#82621=SURFACE_STYLE_FILL_AREA(#82620);
#82622=SURFACE_SIDE_STYLE('',(#82621));
#82623=SURFACE_STYLE_USAGE(.BOTH.,#82622);
#82624=PRESENTATION_STYLE_ASSIGNMENT((#82623));
#82625=COLOUR_RGB('Grey',0.48,0.52,0.57);
#82626=FILL_AREA_STYLE_COLOUR('',#82625);
#82627=FILL_AREA_STYLE('',(#82626));
#82628=SURFACE_STYLE_FILL_AREA(#82627);
#82629=SURFACE_SIDE_STYLE('',(#82628));
#82630=SURFACE_STYLE_USAGE(.BOTH.,#82629);
#82631=PRESENTATION_STYLE_ASSIGNMENT((#82630));
#82632=COLOUR_RGB('Black',0.12,0.14,0.17);
#82633=FILL_AREA_STYLE_COLOUR('',#82632);
#82634=FILL_AREA_STYLE('',(#82633));
#82635=SURFACE_STYLE_FILL_AREA(#82634);
#82636=SURFACE_SIDE_STYLE('',(#82635));
#82637=SURFACE_STYLE_USAGE(.BOTH.,#82636);
#82638=PRESENTATION_STYLE_ASSIGNMENT((#82637));
#82639=COLOUR_RGB('Off White',0.89,0.88,0.83);
#82640=FILL_AREA_STYLE_COLOUR('',#82639);
#82641=FILL_AREA_STYLE('',(#82640));
#82642=SURFACE_STYLE_FILL_AREA(#82641);
#82643=SURFACE_SIDE_STYLE('',(#82642));
#82644=SURFACE_STYLE_USAGE(.BOTH.,#82643);
#82645=PRESENTATION_STYLE_ASSIGNMENT((#82644));
ENDSEC;
END-ISO-10303-21;
